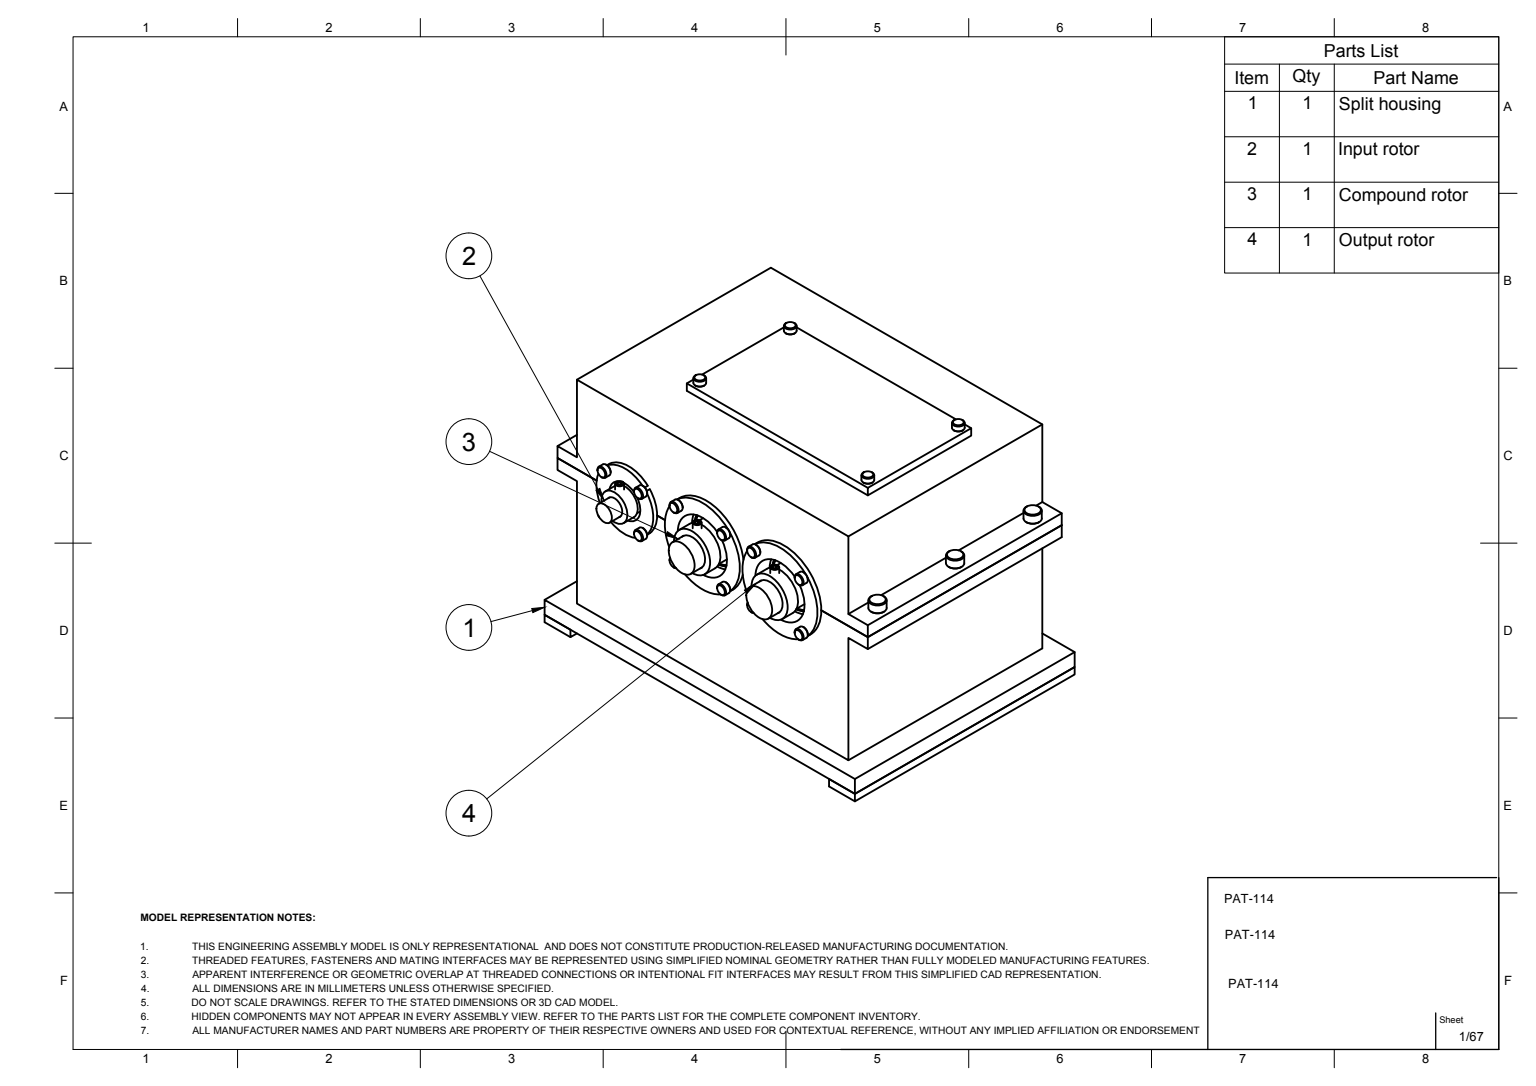
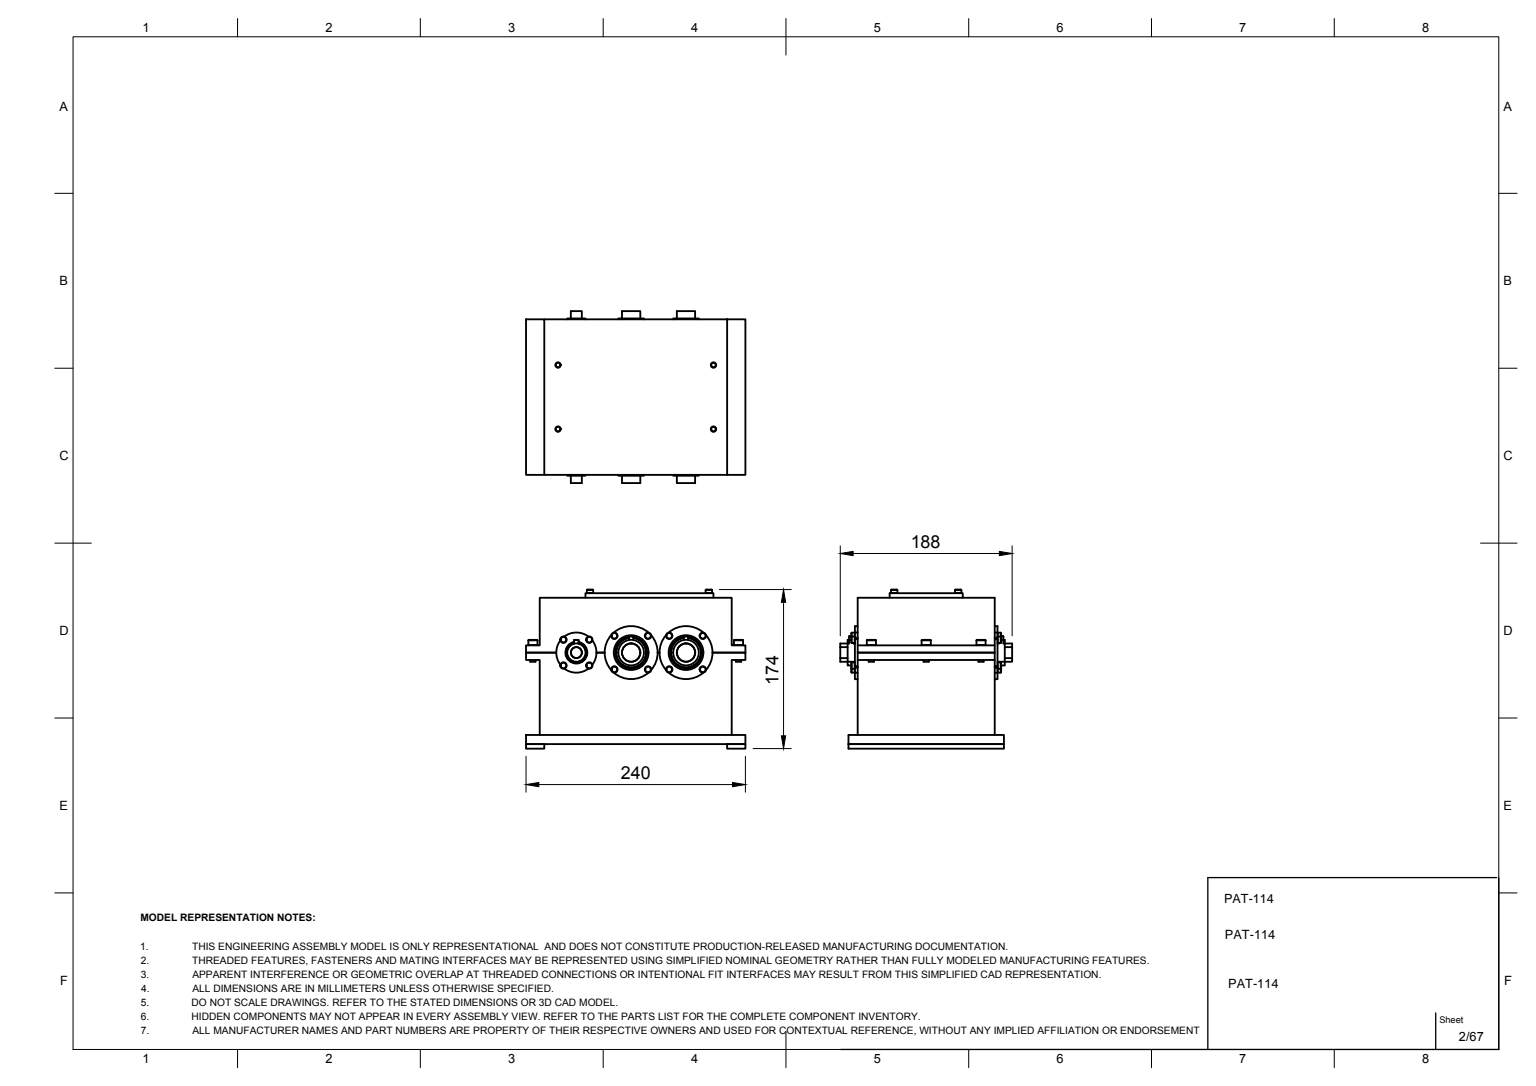
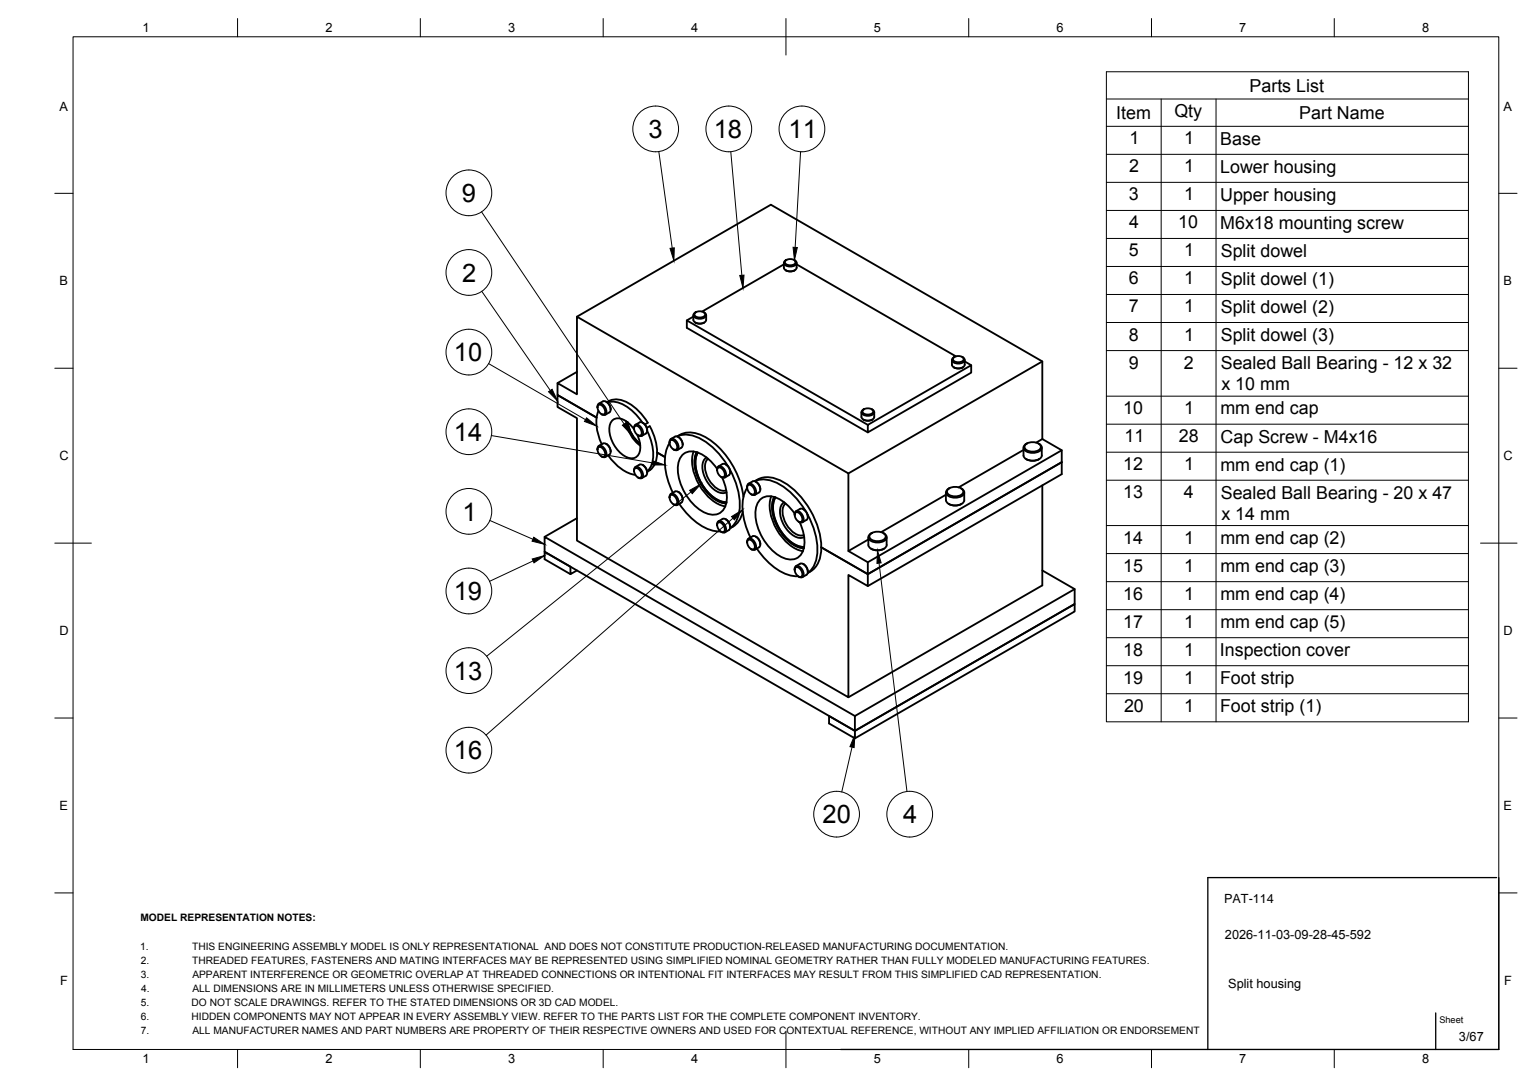
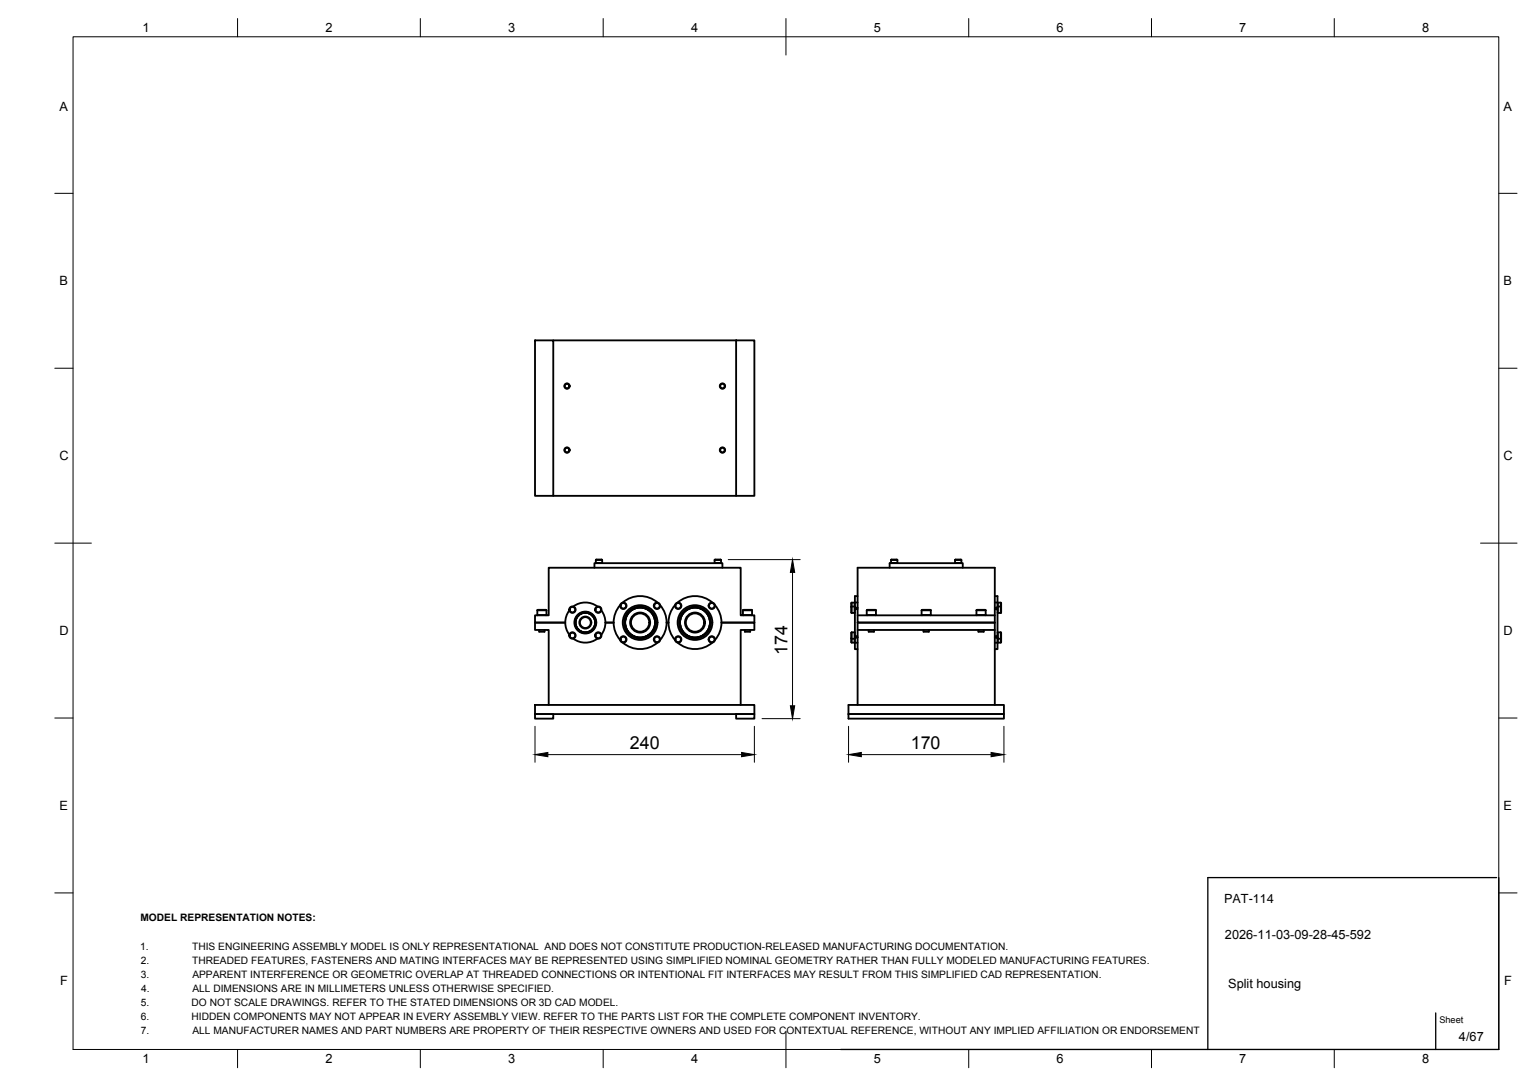
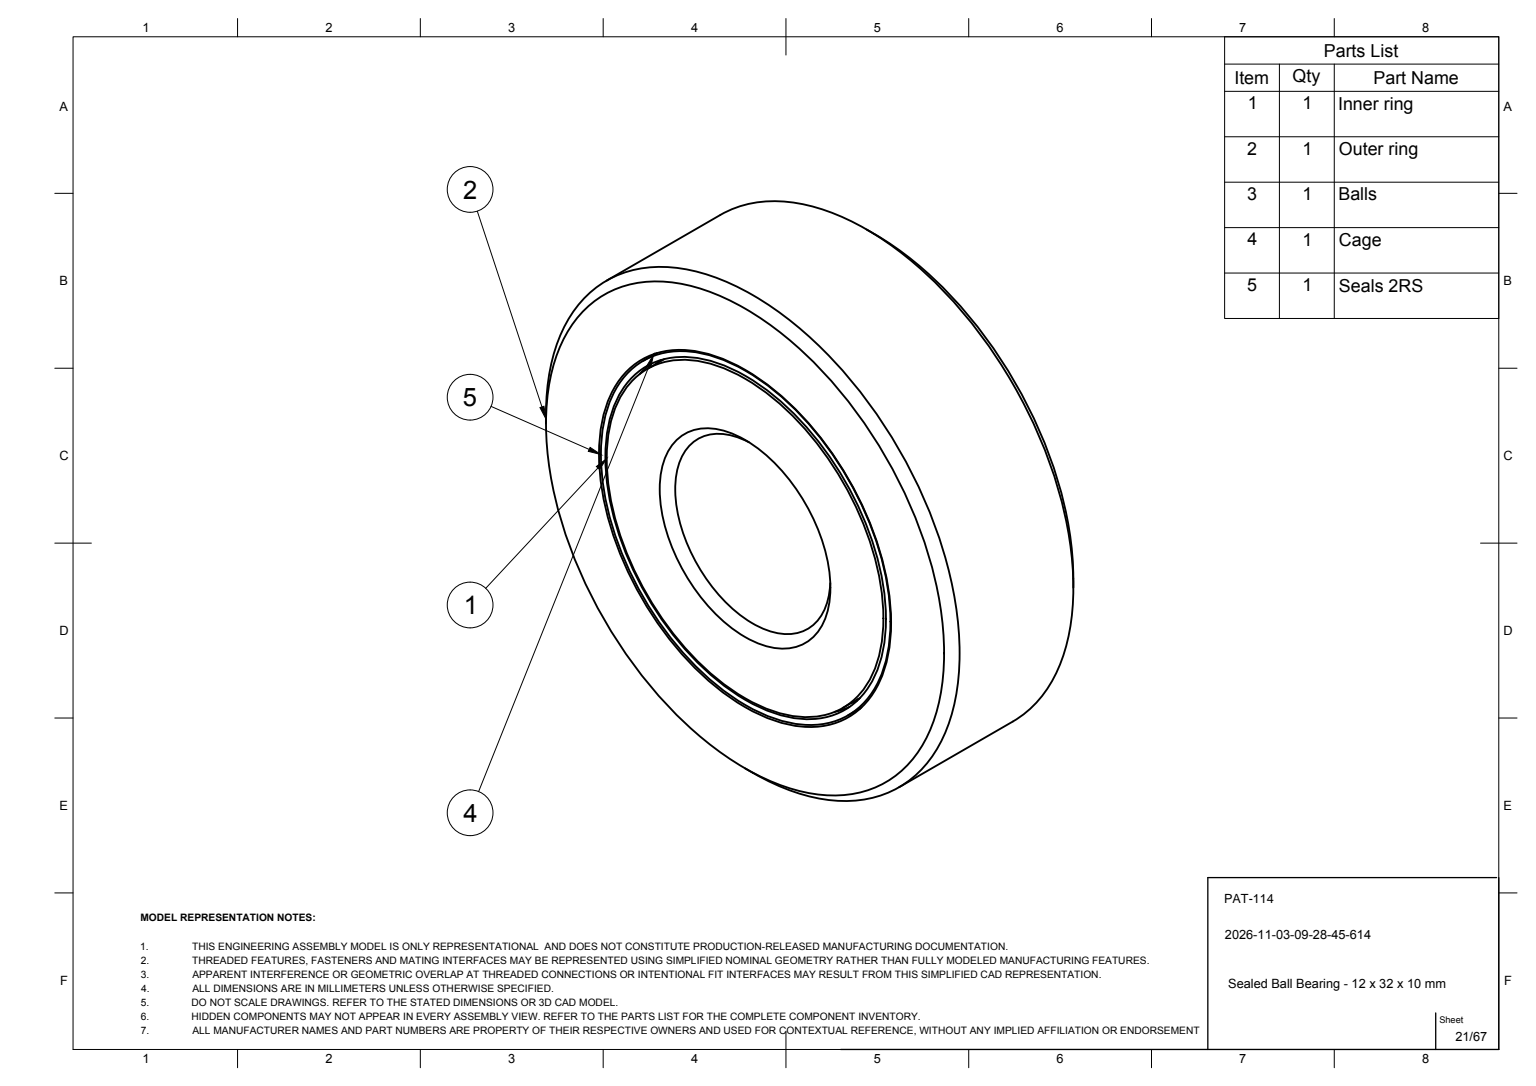
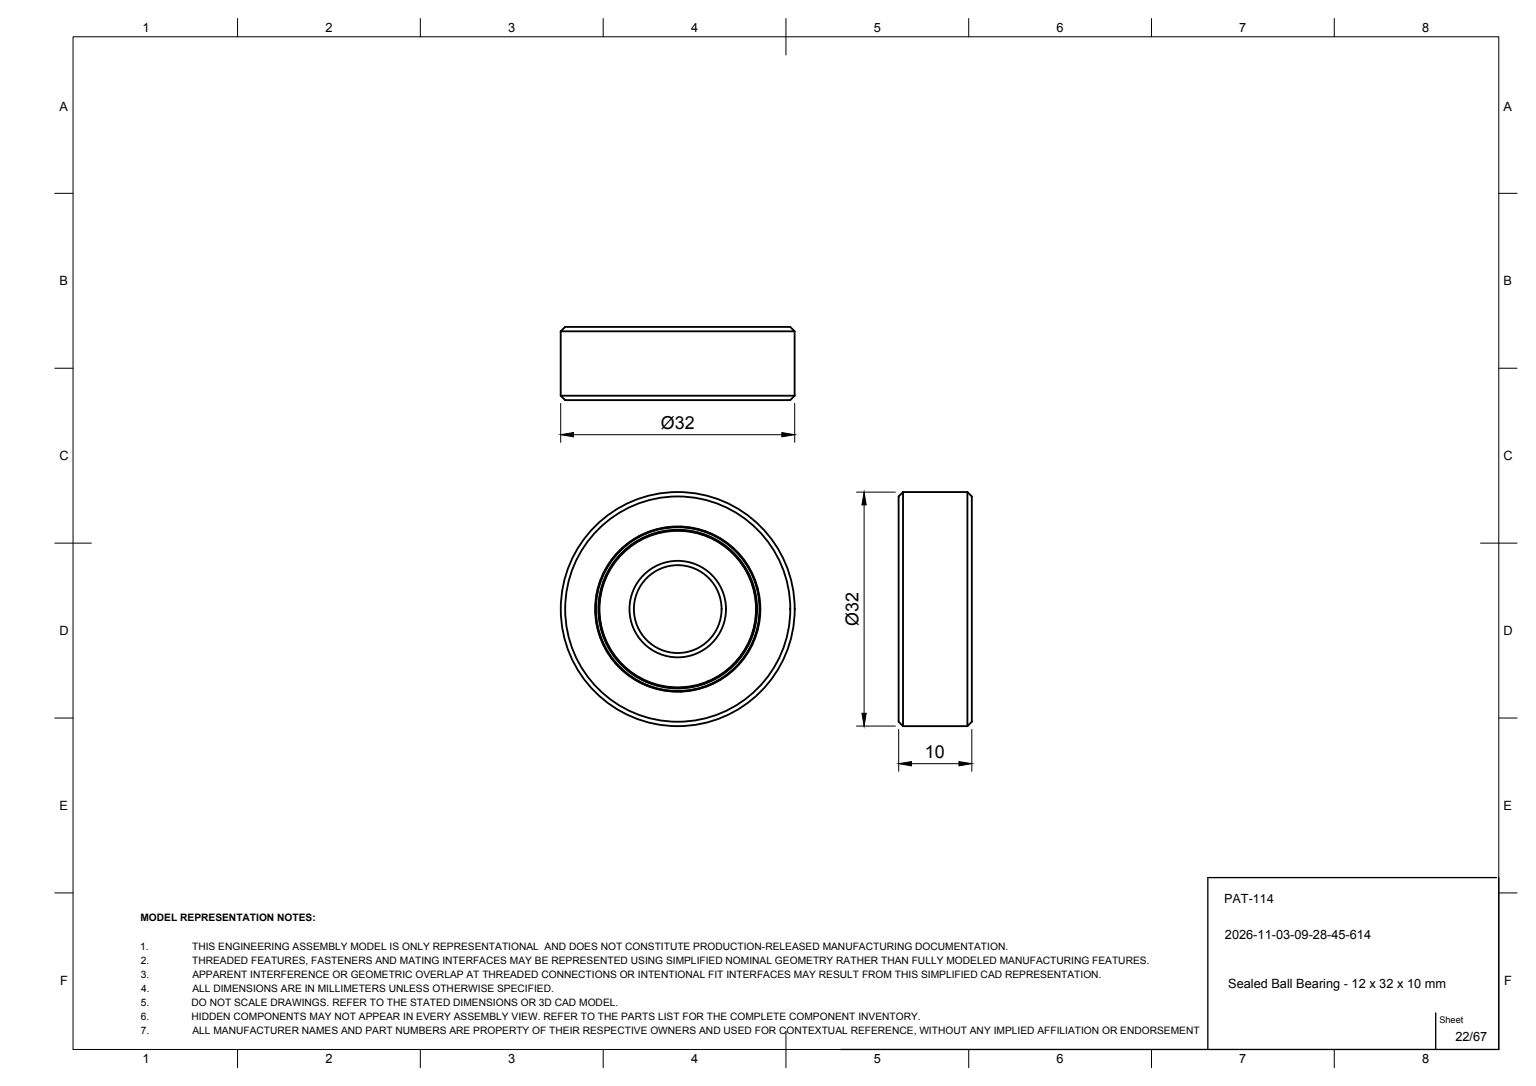
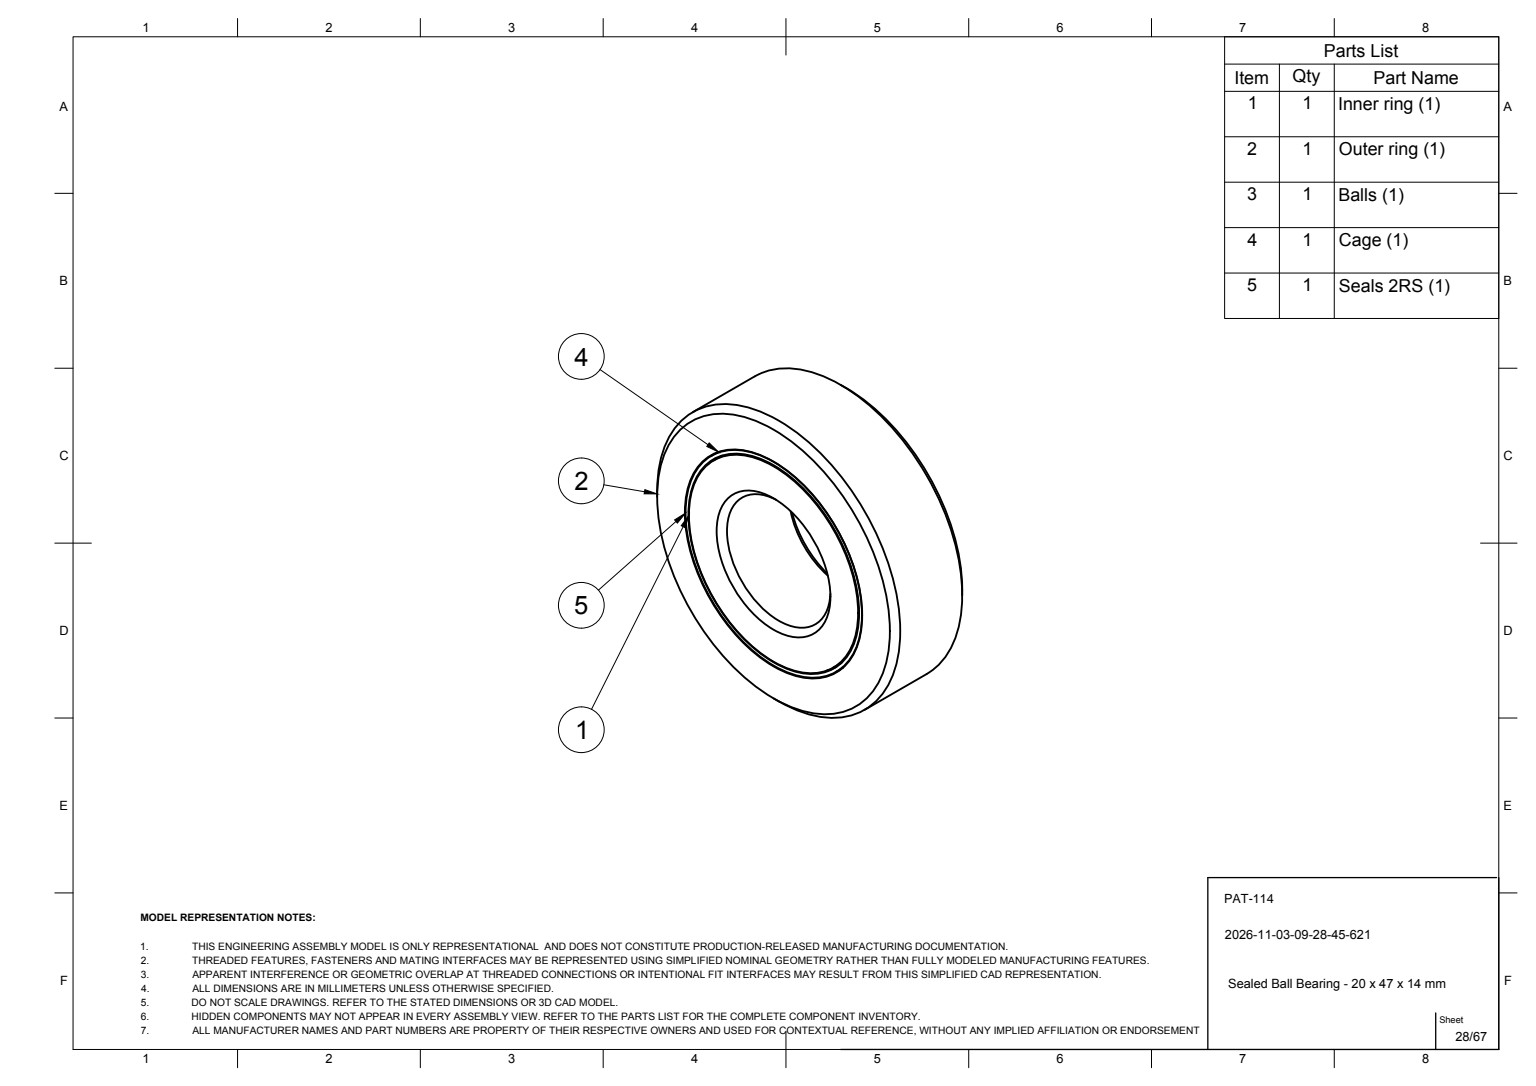
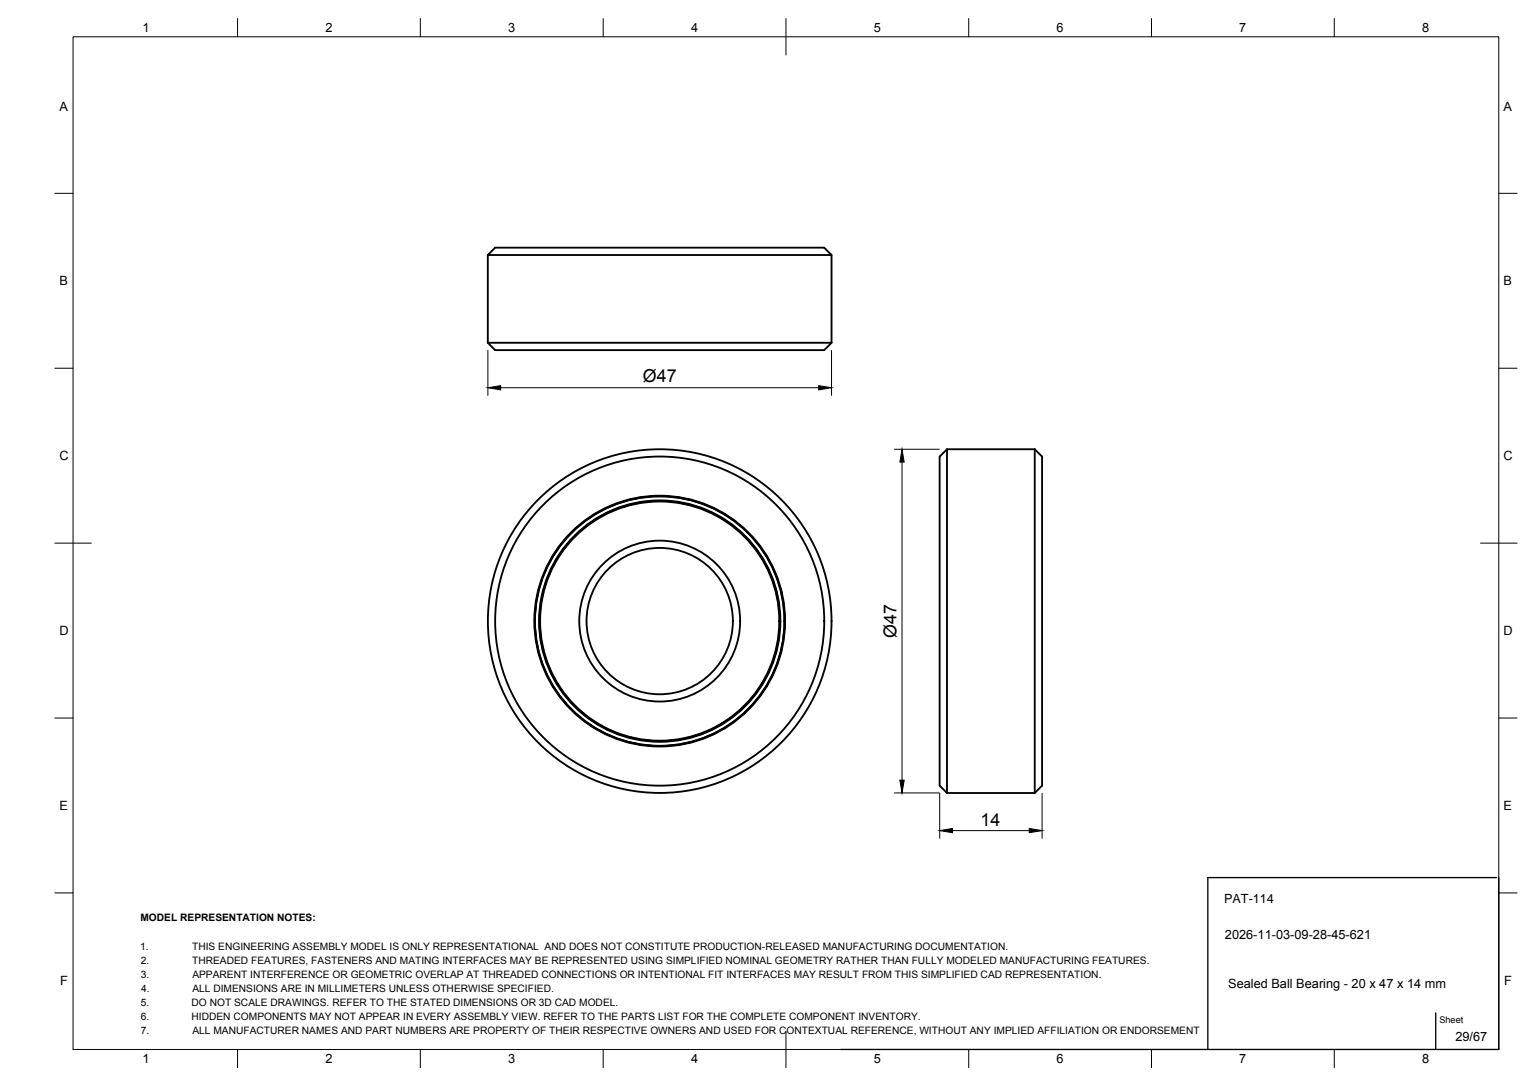
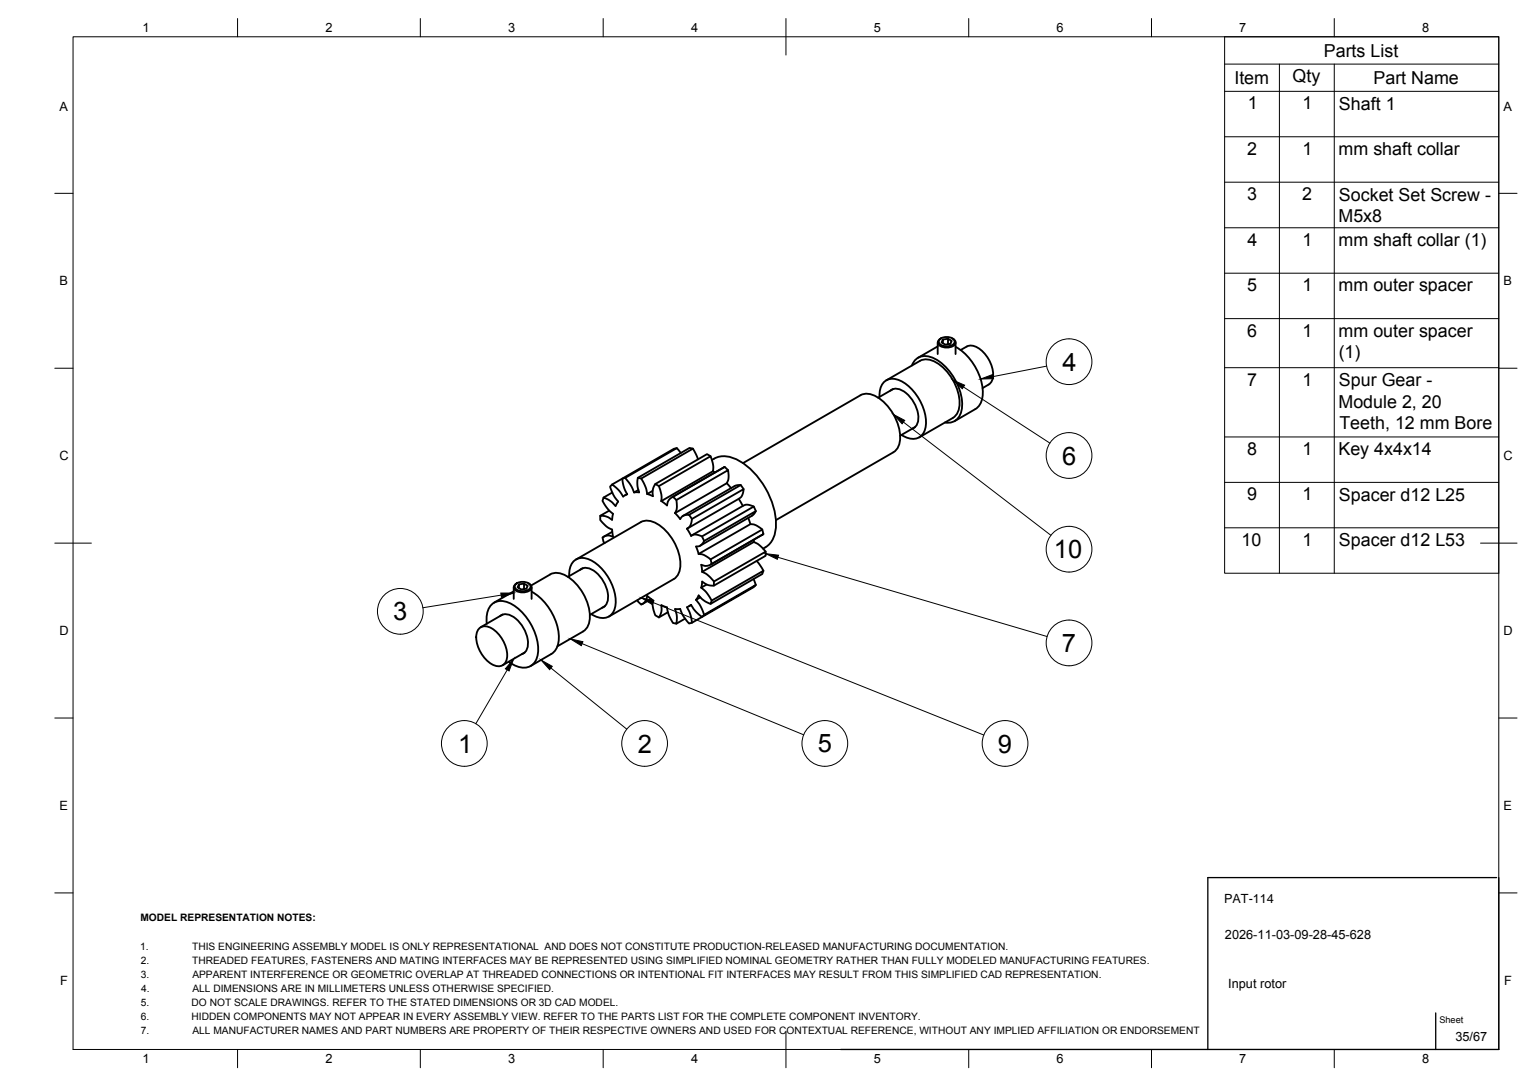
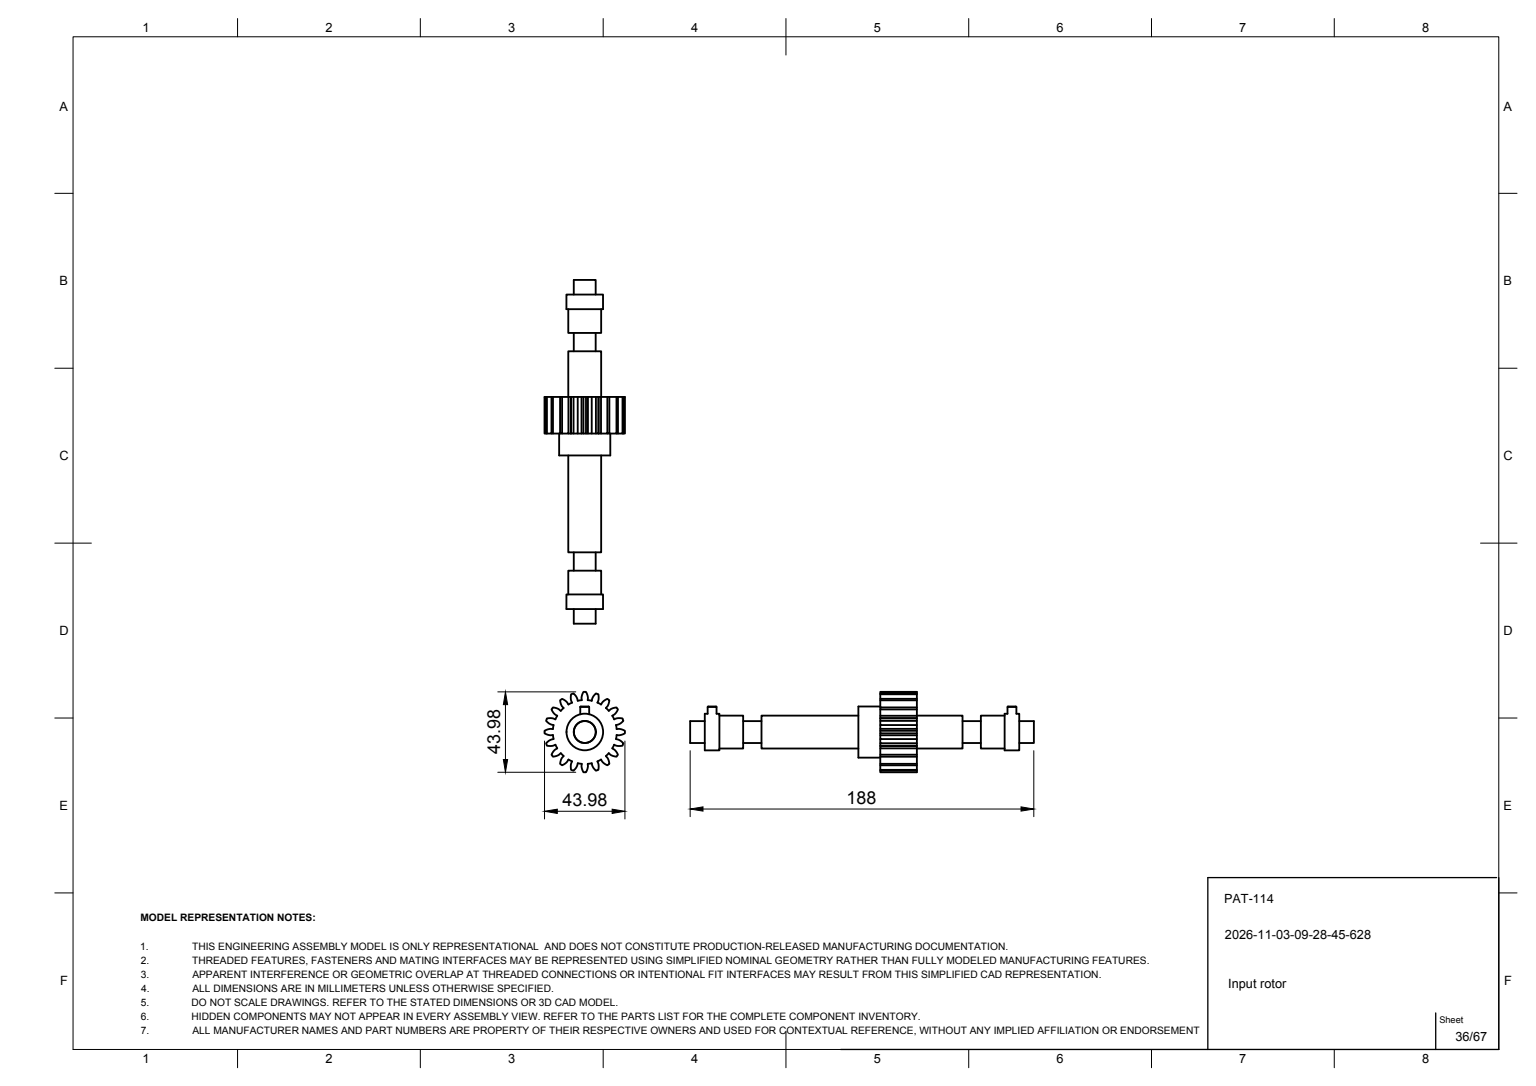
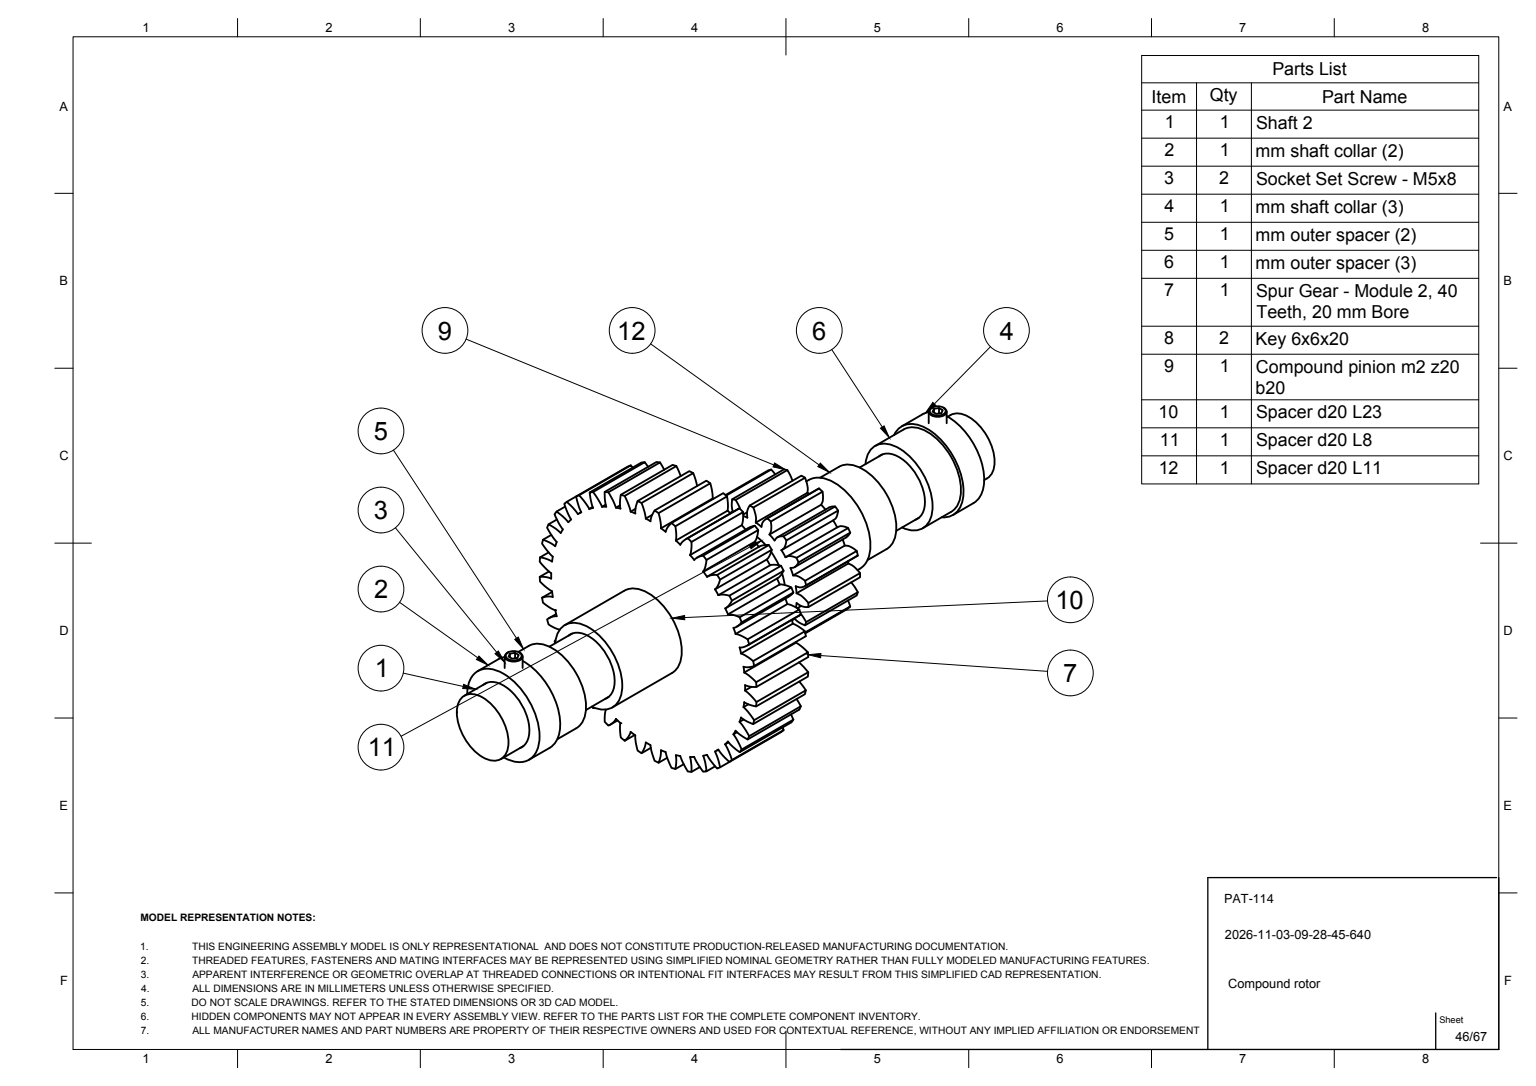
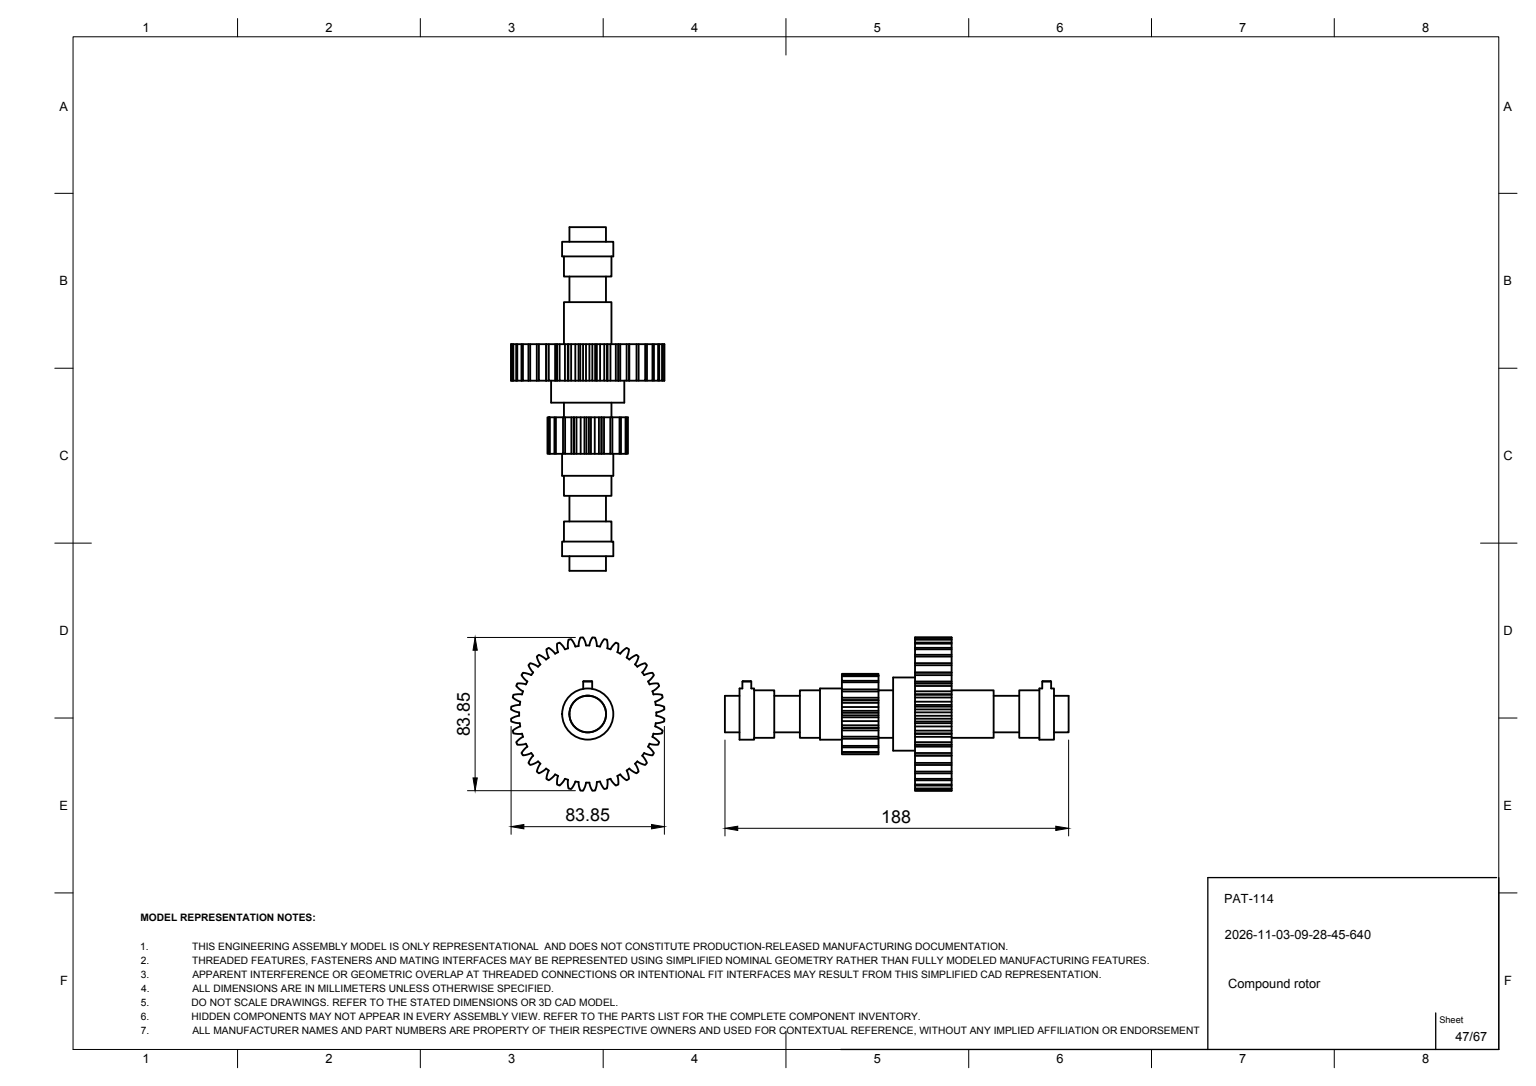
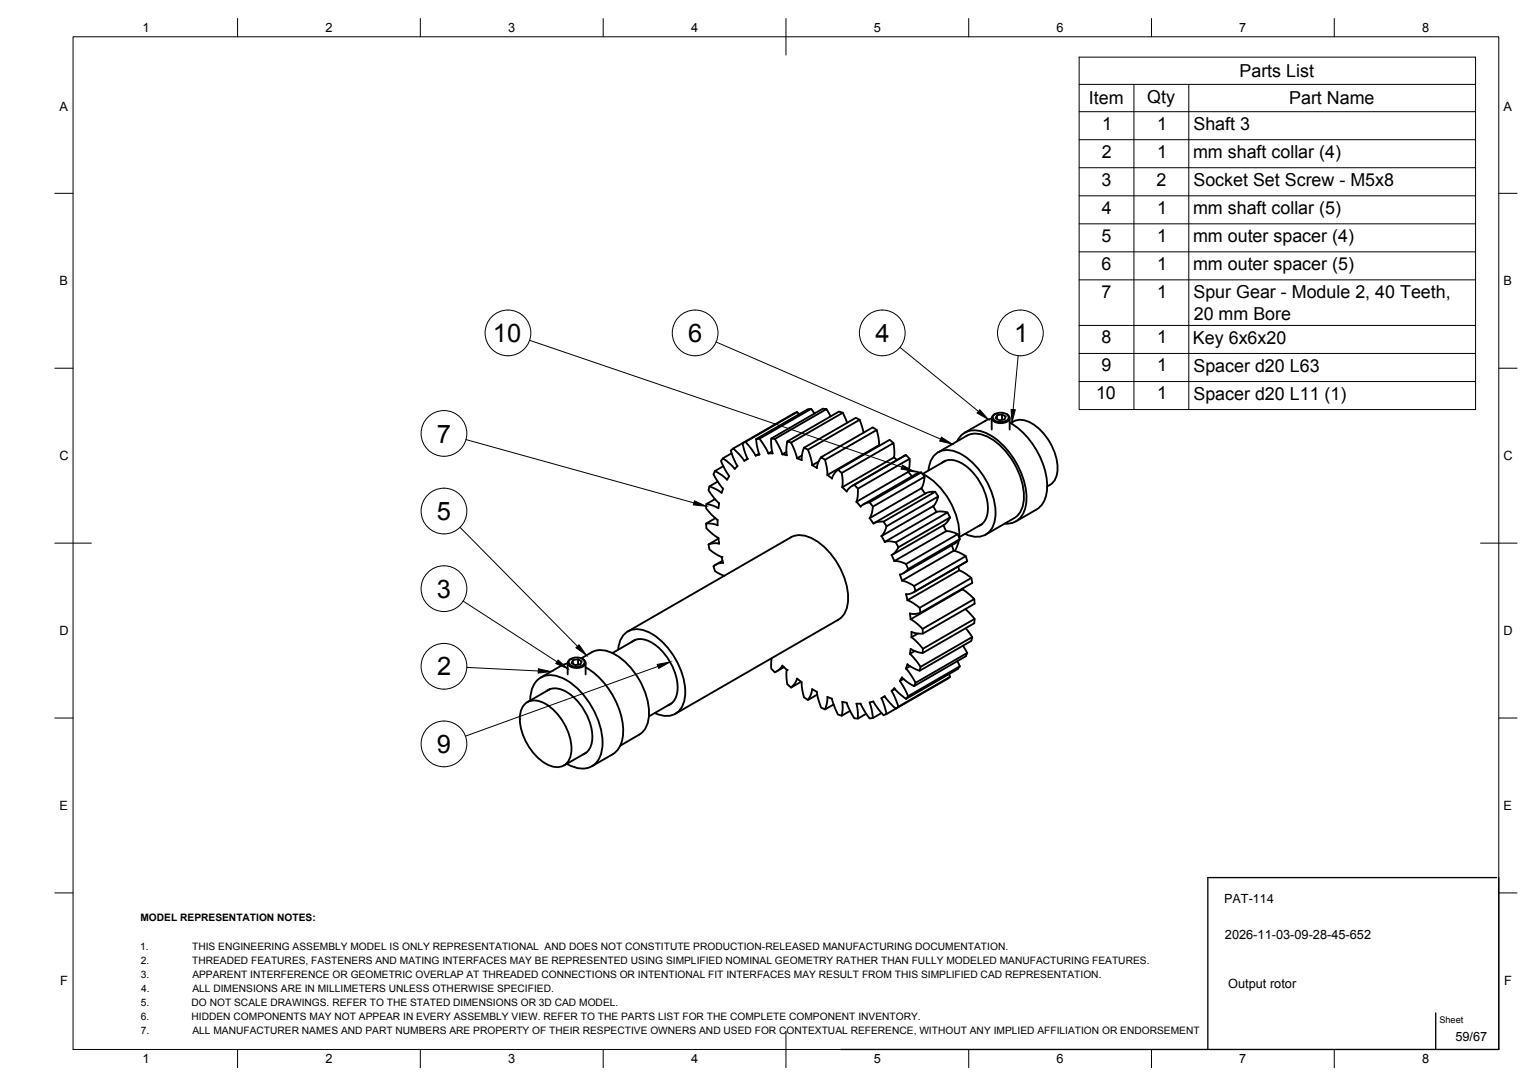
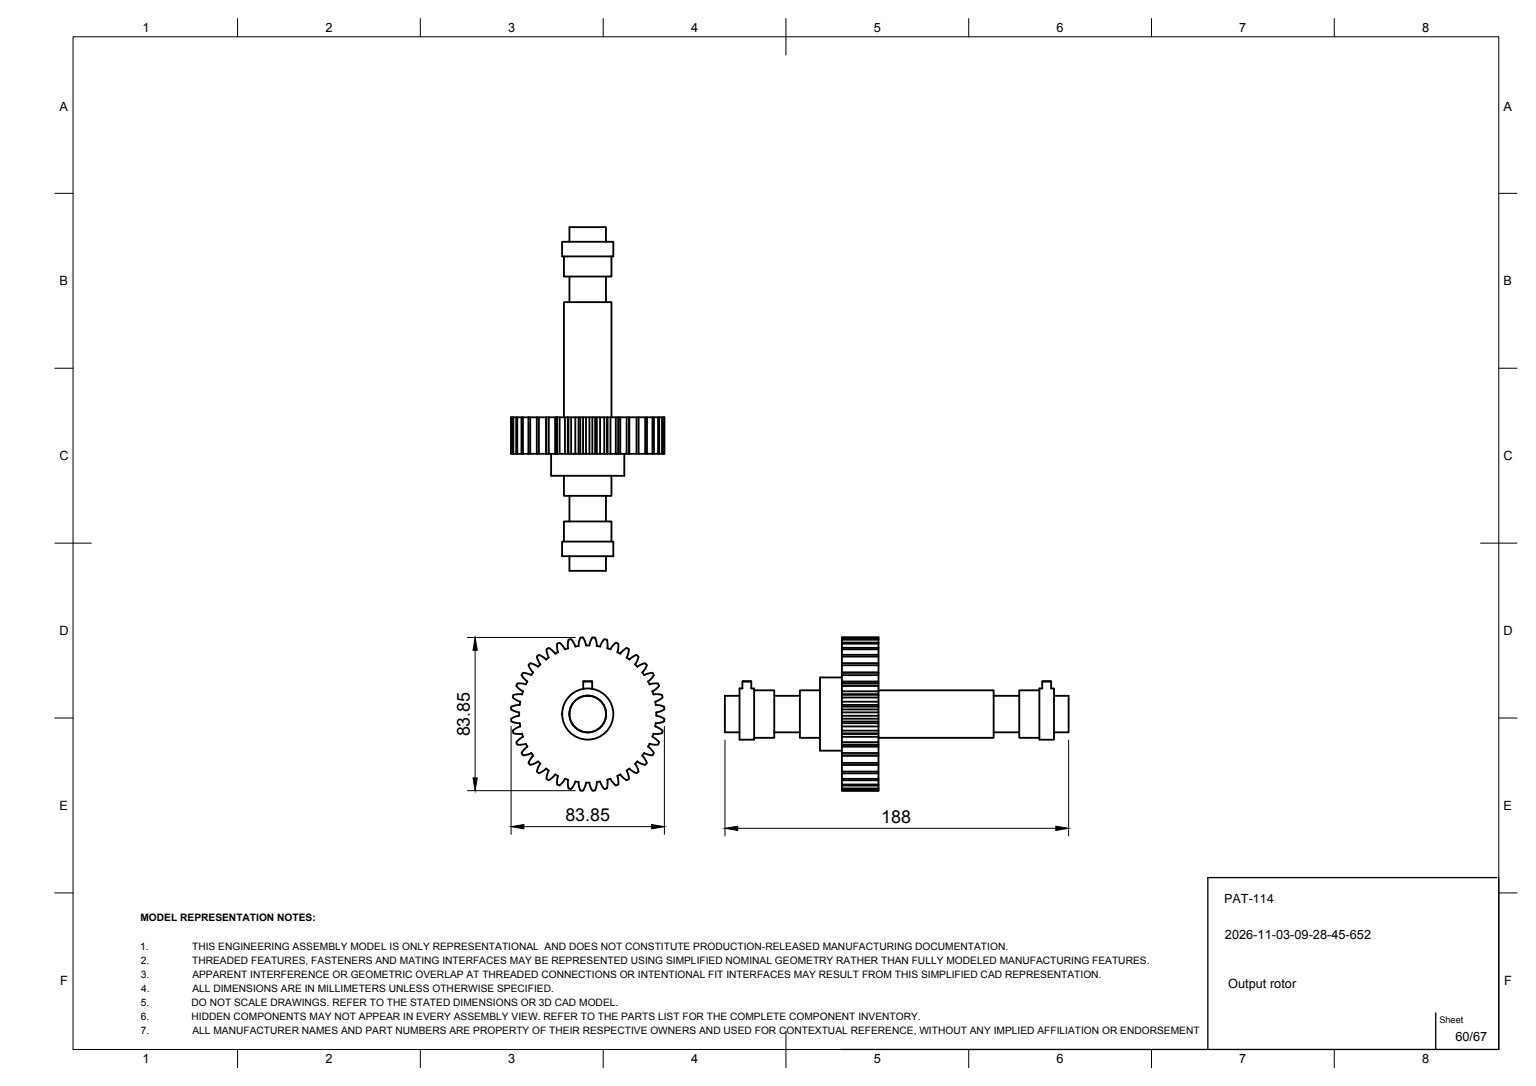
ISO-10303-21;
HEADER;
/* Generated by software containing ST-Developer
 * from STEP Tools, Inc. (www.steptools.com) 
 */

FILE_DESCRIPTION(
/* description */ ('Two-stage gear reducer in split housing'),
/* implementation_level */ '2;1');

FILE_NAME(
/* name */ 'PAT-114',
/* time_stamp */ '2026-10-28T03:22:31-07:00',
/* author */ (''),
/* organization */ (''),
/* preprocessor_version */ 'ST-DEVELOPER v20.2',
/* originating_system */ 'Autodesk Translation Framework v15.17.0.0',
/* authorisation */ '');

FILE_SCHEMA (('AUTOMOTIVE_DESIGN { 1 0 10303 214 3 1 1 }'));
ENDSEC;

DATA;
#10=MECHANICAL_DESIGN_GEOMETRIC_PRESENTATION_REPRESENTATION('',(#1234,#1235,
#1236,#1237,#1238,#1239,#1240,#1241,#1242,#1243,#1244,#1245,#1246,#1247,
#1248,#1249,#1250,#1251,#1252,#1253,#1254,#1255,#1256,#1257,#1258,#1259,
#1260,#1261,#1262,#1263,#1264,#1265,#1266,#1267,#1268,#1269,#1270,#1271,
#1272,#1273,#1274,#1275,#1276,#1277,#1278,#1279,#1280,#1281,#1282,#1283,
#1284,#1285,#1286,#1287,#1288,#1289,#1290,#1291,#1292,#1293,#1294,#1295,
#1296,#1297,#1298,#1299,#1300,#1301,#1302,#1303,#1304),#73366);
#11=(
BOUNDED_SURFACE()
B_SPLINE_SURFACE(5,1,((#28644,#28645),(#28646,#28647),(#28648,#28649),(#28650,
#28651),(#28652,#28653),(#28654,#28655),(#28656,#28657),(#28658,#28659),
(#28660,#28661),(#28662,#28663),(#28664,#28665),(#28666,#28667),(#28668,
#28669),(#28670,#28671),(#28672,#28673),(#28674,#28675),(#28676,#28677),
(#28678,#28679),(#28680,#28681),(#28682,#28683),(#28684,#28685),(#28686,
#28687),(#28688,#28689),(#28690,#28691),(#28692,#28693),(#28694,#28695),
(#28696,#28697),(#28698,#28699),(#28700,#28701),(#28702,#28703),(#28704,
#28705),(#28706,#28707),(#28708,#28709),(#28710,#28711),(#28712,#28713),
(#28714,#28715),(#28716,#28717),(#28718,#28719),(#28720,#28721),(#28722,
#28723),(#28724,#28725),(#28726,#28727),(#28728,#28729),(#28730,#28731),
(#28732,#28733),(#28734,#28735),(#28736,#28737),(#28738,#28739),(#28740,
#28741),(#28742,#28743),(#28744,#28745),(#28746,#28747),(#28748,#28749),
(#28750,#28751),(#28752,#28753),(#28754,#28755),(#28756,#28757),(#28758,
#28759),(#28760,#28761),(#28762,#28763),(#28764,#28765),(#28766,#28767),
(#28768,#28769),(#28770,#28771),(#28772,#28773),(#28774,#28775),(#28776,
#28777),(#28778,#28779),(#28780,#28781),(#28782,#28783)),.UNSPECIFIED.,
 .F.,.F.,.F.)
B_SPLINE_SURFACE_WITH_KNOTS((6,1,1,1,1,1,1,1,1,1,1,1,1,1,1,1,1,1,1,1,1,
1,1,1,1,1,1,1,1,1,1,1,1,1,1,1,1,1,1,1,1,1,1,1,1,1,1,1,1,1,1,1,1,1,1,1,1,
1,1,1,1,1,1,1,1,6),(2,2),(-1.,-0.984615384615383,-0.969230769230768,-0.953846153846152,
-0.938461538461537,-0.923076923076922,-0.907692307692306,-0.892307692307691,
-0.876923076923076,-0.86153846153846,-0.846153846153845,-0.83076923076923,
-0.815384615384614,-0.799999999999999,-0.784615384615384,-0.769230769230768,
-0.753846153846153,-0.738461538461538,-0.723076923076922,-0.707692307692307,
-0.692307692307692,-0.676923076923076,-0.661538461538461,-0.646153846153846,
-0.63076923076923,-0.615384615384615,-0.6,-0.584615384615384,-0.569230769230769,
-0.553846153846154,-0.538461538461538,-0.523076923076923,-0.507692307692308,
-0.492307692307692,-0.476923076923077,-0.461538461538462,-0.446153846153846,
-0.430769230769231,-0.415384615384615,-0.4,-0.384615384615385,-0.369230769230769,
-0.353846153846154,-0.338461538461538,-0.323076923076923,-0.307692307692308,
-0.292307692307692,-0.276923076923077,-0.261538461538462,-0.246153846153846,
-0.230769230769231,-0.215384615384615,-0.2,-0.184615384615385,-0.169230769230769,
-0.153846153846154,-0.138461538461538,-0.123076923076923,-0.107692307692308,
-0.0923076923076923,-0.0769230769230769,-0.0615384615384615,-0.0461538461538462,
-0.0307692307692308,-0.0153846153846154,0.),(-1.,1.),.UNSPECIFIED.)
GEOMETRIC_REPRESENTATION_ITEM()
RATIONAL_B_SPLINE_SURFACE(((1.,1.),(1.,1.),(1.,1.),(1.,1.),(1.,1.),(1.,
1.),(1.,1.),(1.,1.),(1.,1.),(1.,1.),(1.,1.),(1.,1.),(1.,1.),(1.,1.),(1.,
1.),(1.,1.),(1.,1.),(1.,1.),(1.,1.),(1.,1.),(1.,1.),(1.,1.),(1.,1.),(1.,
1.),(1.,1.),(1.,1.),(1.,1.),(1.,1.),(1.,1.),(1.,1.),(1.,1.),(1.,1.),(1.,
1.),(1.,1.),(1.,1.),(1.,1.),(1.,1.),(1.,1.),(1.,1.),(1.,1.),(1.,1.),(1.,
1.),(1.,1.),(1.,1.),(1.,1.),(1.,1.),(1.,1.),(1.,1.),(1.,1.),(1.,1.),(1.,
1.),(1.,1.),(1.,1.),(1.,1.),(1.,1.),(1.,1.),(1.,1.),(1.,1.),(1.,1.),(1.,
1.),(1.,1.),(1.,1.),(1.,1.),(1.,1.),(1.,1.),(1.,1.),(1.,1.),(1.,1.),(1.,
1.),(1.,1.)))
REPRESENTATION_ITEM('')
SURFACE()
);
#12=(
BOUNDED_SURFACE()
B_SPLINE_SURFACE(5,1,((#28862,#28863),(#28864,#28865),(#28866,#28867),(#28868,
#28869),(#28870,#28871),(#28872,#28873),(#28874,#28875),(#28876,#28877),
(#28878,#28879),(#28880,#28881),(#28882,#28883),(#28884,#28885),(#28886,
#28887),(#28888,#28889),(#28890,#28891),(#28892,#28893),(#28894,#28895),
(#28896,#28897),(#28898,#28899),(#28900,#28901),(#28902,#28903),(#28904,
#28905),(#28906,#28907),(#28908,#28909),(#28910,#28911),(#28912,#28913),
(#28914,#28915),(#28916,#28917),(#28918,#28919),(#28920,#28921),(#28922,
#28923),(#28924,#28925),(#28926,#28927),(#28928,#28929),(#28930,#28931),
(#28932,#28933),(#28934,#28935),(#28936,#28937),(#28938,#28939),(#28940,
#28941),(#28942,#28943),(#28944,#28945),(#28946,#28947),(#28948,#28949),
(#28950,#28951),(#28952,#28953),(#28954,#28955),(#28956,#28957),(#28958,
#28959),(#28960,#28961),(#28962,#28963),(#28964,#28965),(#28966,#28967),
(#28968,#28969),(#28970,#28971),(#28972,#28973),(#28974,#28975),(#28976,
#28977),(#28978,#28979),(#28980,#28981),(#28982,#28983),(#28984,#28985),
(#28986,#28987),(#28988,#28989),(#28990,#28991),(#28992,#28993),(#28994,
#28995),(#28996,#28997),(#28998,#28999),(#29000,#29001)),.UNSPECIFIED.,
 .F.,.F.,.F.)
B_SPLINE_SURFACE_WITH_KNOTS((6,1,1,1,1,1,1,1,1,1,1,1,1,1,1,1,1,1,1,1,1,
1,1,1,1,1,1,1,1,1,1,1,1,1,1,1,1,1,1,1,1,1,1,1,1,1,1,1,1,1,1,1,1,1,1,1,1,
1,1,1,1,1,1,1,1,6),(2,2),(-1.,-0.984615384615383,-0.969230769230768,-0.953846153846152,
-0.938461538461537,-0.923076923076922,-0.907692307692306,-0.892307692307691,
-0.876923076923076,-0.86153846153846,-0.846153846153845,-0.83076923076923,
-0.815384615384614,-0.799999999999999,-0.784615384615384,-0.769230769230768,
-0.753846153846153,-0.738461538461538,-0.723076923076922,-0.707692307692307,
-0.692307692307692,-0.676923076923076,-0.661538461538461,-0.646153846153846,
-0.63076923076923,-0.615384615384615,-0.6,-0.584615384615384,-0.569230769230769,
-0.553846153846154,-0.538461538461538,-0.523076923076923,-0.507692307692308,
-0.492307692307692,-0.476923076923077,-0.461538461538462,-0.446153846153846,
-0.430769230769231,-0.415384615384615,-0.4,-0.384615384615385,-0.369230769230769,
-0.353846153846154,-0.338461538461538,-0.323076923076923,-0.307692307692308,
-0.292307692307692,-0.276923076923077,-0.261538461538462,-0.246153846153846,
-0.230769230769231,-0.215384615384615,-0.2,-0.184615384615385,-0.169230769230769,
-0.153846153846154,-0.138461538461538,-0.123076923076923,-0.107692307692308,
-0.0923076923076923,-0.0769230769230769,-0.0615384615384615,-0.0461538461538462,
-0.0307692307692308,-0.0153846153846154,0.),(-1.,1.),.UNSPECIFIED.)
GEOMETRIC_REPRESENTATION_ITEM()
RATIONAL_B_SPLINE_SURFACE(((1.,1.),(1.,1.),(1.,1.),(1.,1.),(1.,1.),(1.,
1.),(1.,1.),(1.,1.),(1.,1.),(1.,1.),(1.,1.),(1.,1.),(1.,1.),(1.,1.),(1.,
1.),(1.,1.),(1.,1.),(1.,1.),(1.,1.),(1.,1.),(1.,1.),(1.,1.),(1.,1.),(1.,
1.),(1.,1.),(1.,1.),(1.,1.),(1.,1.),(1.,1.),(1.,1.),(1.,1.),(1.,1.),(1.,
1.),(1.,1.),(1.,1.),(1.,1.),(1.,1.),(1.,1.),(1.,1.),(1.,1.),(1.,1.),(1.,
1.),(1.,1.),(1.,1.),(1.,1.),(1.,1.),(1.,1.),(1.,1.),(1.,1.),(1.,1.),(1.,
1.),(1.,1.),(1.,1.),(1.,1.),(1.,1.),(1.,1.),(1.,1.),(1.,1.),(1.,1.),(1.,
1.),(1.,1.),(1.,1.),(1.,1.),(1.,1.),(1.,1.),(1.,1.),(1.,1.),(1.,1.),(1.,
1.),(1.,1.)))
REPRESENTATION_ITEM('')
SURFACE()
);
#13=(
BOUNDED_SURFACE()
B_SPLINE_SURFACE(5,1,((#29078,#29079),(#29080,#29081),(#29082,#29083),(#29084,
#29085),(#29086,#29087),(#29088,#29089),(#29090,#29091),(#29092,#29093),
(#29094,#29095),(#29096,#29097),(#29098,#29099),(#29100,#29101),(#29102,
#29103),(#29104,#29105),(#29106,#29107),(#29108,#29109),(#29110,#29111),
(#29112,#29113),(#29114,#29115),(#29116,#29117),(#29118,#29119),(#29120,
#29121),(#29122,#29123),(#29124,#29125),(#29126,#29127),(#29128,#29129),
(#29130,#29131),(#29132,#29133),(#29134,#29135),(#29136,#29137),(#29138,
#29139),(#29140,#29141),(#29142,#29143),(#29144,#29145),(#29146,#29147),
(#29148,#29149),(#29150,#29151),(#29152,#29153),(#29154,#29155),(#29156,
#29157),(#29158,#29159),(#29160,#29161),(#29162,#29163),(#29164,#29165),
(#29166,#29167),(#29168,#29169),(#29170,#29171),(#29172,#29173),(#29174,
#29175),(#29176,#29177),(#29178,#29179),(#29180,#29181),(#29182,#29183),
(#29184,#29185),(#29186,#29187),(#29188,#29189),(#29190,#29191),(#29192,
#29193),(#29194,#29195),(#29196,#29197),(#29198,#29199),(#29200,#29201),
(#29202,#29203),(#29204,#29205),(#29206,#29207),(#29208,#29209),(#29210,
#29211),(#29212,#29213),(#29214,#29215),(#29216,#29217)),.UNSPECIFIED.,
 .F.,.F.,.F.)
B_SPLINE_SURFACE_WITH_KNOTS((6,1,1,1,1,1,1,1,1,1,1,1,1,1,1,1,1,1,1,1,1,
1,1,1,1,1,1,1,1,1,1,1,1,1,1,1,1,1,1,1,1,1,1,1,1,1,1,1,1,1,1,1,1,1,1,1,1,
1,1,1,1,1,1,1,1,6),(2,2),(-1.,-0.984615384615383,-0.969230769230768,-0.953846153846152,
-0.938461538461537,-0.923076923076922,-0.907692307692306,-0.892307692307691,
-0.876923076923076,-0.86153846153846,-0.846153846153845,-0.83076923076923,
-0.815384615384614,-0.799999999999999,-0.784615384615384,-0.769230769230768,
-0.753846153846153,-0.738461538461538,-0.723076923076922,-0.707692307692307,
-0.692307692307692,-0.676923076923076,-0.661538461538461,-0.646153846153846,
-0.63076923076923,-0.615384615384615,-0.6,-0.584615384615384,-0.569230769230769,
-0.553846153846154,-0.538461538461538,-0.523076923076923,-0.507692307692308,
-0.492307692307692,-0.476923076923077,-0.461538461538462,-0.446153846153846,
-0.430769230769231,-0.415384615384615,-0.4,-0.384615384615385,-0.369230769230769,
-0.353846153846154,-0.338461538461538,-0.323076923076923,-0.307692307692308,
-0.292307692307692,-0.276923076923077,-0.261538461538462,-0.246153846153846,
-0.230769230769231,-0.215384615384615,-0.2,-0.184615384615385,-0.169230769230769,
-0.153846153846154,-0.138461538461538,-0.123076923076923,-0.107692307692308,
-0.0923076923076923,-0.0769230769230769,-0.0615384615384615,-0.0461538461538462,
-0.0307692307692308,-0.0153846153846154,0.),(-1.,1.),.UNSPECIFIED.)
GEOMETRIC_REPRESENTATION_ITEM()
RATIONAL_B_SPLINE_SURFACE(((1.,1.),(1.,1.),(1.,1.),(1.,1.),(1.,1.),(1.,
1.),(1.,1.),(1.,1.),(1.,1.),(1.,1.),(1.,1.),(1.,1.),(1.,1.),(1.,1.),(1.,
1.),(1.,1.),(1.,1.),(1.,1.),(1.,1.),(1.,1.),(1.,1.),(1.,1.),(1.,1.),(1.,
1.),(1.,1.),(1.,1.),(1.,1.),(1.,1.),(1.,1.),(1.,1.),(1.,1.),(1.,1.),(1.,
1.),(1.,1.),(1.,1.),(1.,1.),(1.,1.),(1.,1.),(1.,1.),(1.,1.),(1.,1.),(1.,
1.),(1.,1.),(1.,1.),(1.,1.),(1.,1.),(1.,1.),(1.,1.),(1.,1.),(1.,1.),(1.,
1.),(1.,1.),(1.,1.),(1.,1.),(1.,1.),(1.,1.),(1.,1.),(1.,1.),(1.,1.),(1.,
1.),(1.,1.),(1.,1.),(1.,1.),(1.,1.),(1.,1.),(1.,1.),(1.,1.),(1.,1.),(1.,
1.),(1.,1.)))
REPRESENTATION_ITEM('')
SURFACE()
);
#14=(
BOUNDED_SURFACE()
B_SPLINE_SURFACE(5,1,((#29294,#29295),(#29296,#29297),(#29298,#29299),(#29300,
#29301),(#29302,#29303),(#29304,#29305),(#29306,#29307),(#29308,#29309),
(#29310,#29311),(#29312,#29313),(#29314,#29315),(#29316,#29317),(#29318,
#29319),(#29320,#29321),(#29322,#29323),(#29324,#29325),(#29326,#29327),
(#29328,#29329),(#29330,#29331),(#29332,#29333),(#29334,#29335),(#29336,
#29337),(#29338,#29339),(#29340,#29341),(#29342,#29343),(#29344,#29345),
(#29346,#29347),(#29348,#29349),(#29350,#29351),(#29352,#29353),(#29354,
#29355),(#29356,#29357),(#29358,#29359),(#29360,#29361),(#29362,#29363),
(#29364,#29365),(#29366,#29367),(#29368,#29369),(#29370,#29371),(#29372,
#29373),(#29374,#29375),(#29376,#29377),(#29378,#29379),(#29380,#29381),
(#29382,#29383),(#29384,#29385),(#29386,#29387),(#29388,#29389),(#29390,
#29391),(#29392,#29393),(#29394,#29395),(#29396,#29397),(#29398,#29399),
(#29400,#29401),(#29402,#29403),(#29404,#29405),(#29406,#29407),(#29408,
#29409),(#29410,#29411),(#29412,#29413),(#29414,#29415),(#29416,#29417),
(#29418,#29419),(#29420,#29421),(#29422,#29423),(#29424,#29425),(#29426,
#29427),(#29428,#29429),(#29430,#29431),(#29432,#29433)),.UNSPECIFIED.,
 .F.,.F.,.F.)
B_SPLINE_SURFACE_WITH_KNOTS((6,1,1,1,1,1,1,1,1,1,1,1,1,1,1,1,1,1,1,1,1,
1,1,1,1,1,1,1,1,1,1,1,1,1,1,1,1,1,1,1,1,1,1,1,1,1,1,1,1,1,1,1,1,1,1,1,1,
1,1,1,1,1,1,1,1,6),(2,2),(-1.,-0.984615384615383,-0.969230769230768,-0.953846153846152,
-0.938461538461537,-0.923076923076922,-0.907692307692306,-0.892307692307691,
-0.876923076923076,-0.86153846153846,-0.846153846153845,-0.83076923076923,
-0.815384615384614,-0.799999999999999,-0.784615384615384,-0.769230769230768,
-0.753846153846153,-0.738461538461538,-0.723076923076922,-0.707692307692307,
-0.692307692307692,-0.676923076923076,-0.661538461538461,-0.646153846153846,
-0.63076923076923,-0.615384615384615,-0.6,-0.584615384615384,-0.569230769230769,
-0.553846153846154,-0.538461538461538,-0.523076923076923,-0.507692307692308,
-0.492307692307692,-0.476923076923077,-0.461538461538462,-0.446153846153846,
-0.430769230769231,-0.415384615384615,-0.4,-0.384615384615385,-0.369230769230769,
-0.353846153846154,-0.338461538461538,-0.323076923076923,-0.307692307692308,
-0.292307692307692,-0.276923076923077,-0.261538461538462,-0.246153846153846,
-0.230769230769231,-0.215384615384615,-0.2,-0.184615384615385,-0.169230769230769,
-0.153846153846154,-0.138461538461538,-0.123076923076923,-0.107692307692308,
-0.0923076923076923,-0.0769230769230769,-0.0615384615384615,-0.0461538461538462,
-0.0307692307692308,-0.0153846153846154,0.),(-1.,1.),.UNSPECIFIED.)
GEOMETRIC_REPRESENTATION_ITEM()
RATIONAL_B_SPLINE_SURFACE(((1.,1.),(1.,1.),(1.,1.),(1.,1.),(1.,1.),(1.,
1.),(1.,1.),(1.,1.),(1.,1.),(1.,1.),(1.,1.),(1.,1.),(1.,1.),(1.,1.),(1.,
1.),(1.,1.),(1.,1.),(1.,1.),(1.,1.),(1.,1.),(1.,1.),(1.,1.),(1.,1.),(1.,
1.),(1.,1.),(1.,1.),(1.,1.),(1.,1.),(1.,1.),(1.,1.),(1.,1.),(1.,1.),(1.,
1.),(1.,1.),(1.,1.),(1.,1.),(1.,1.),(1.,1.),(1.,1.),(1.,1.),(1.,1.),(1.,
1.),(1.,1.),(1.,1.),(1.,1.),(1.,1.),(1.,1.),(1.,1.),(1.,1.),(1.,1.),(1.,
1.),(1.,1.),(1.,1.),(1.,1.),(1.,1.),(1.,1.),(1.,1.),(1.,1.),(1.,1.),(1.,
1.),(1.,1.),(1.,1.),(1.,1.),(1.,1.),(1.,1.),(1.,1.),(1.,1.),(1.,1.),(1.,
1.),(1.,1.)))
REPRESENTATION_ITEM('')
SURFACE()
);
#15=(
BOUNDED_SURFACE()
B_SPLINE_SURFACE(5,1,((#29510,#29511),(#29512,#29513),(#29514,#29515),(#29516,
#29517),(#29518,#29519),(#29520,#29521),(#29522,#29523),(#29524,#29525),
(#29526,#29527),(#29528,#29529),(#29530,#29531),(#29532,#29533),(#29534,
#29535),(#29536,#29537),(#29538,#29539),(#29540,#29541),(#29542,#29543),
(#29544,#29545),(#29546,#29547),(#29548,#29549),(#29550,#29551),(#29552,
#29553),(#29554,#29555),(#29556,#29557),(#29558,#29559),(#29560,#29561),
(#29562,#29563),(#29564,#29565),(#29566,#29567),(#29568,#29569),(#29570,
#29571),(#29572,#29573),(#29574,#29575),(#29576,#29577),(#29578,#29579),
(#29580,#29581),(#29582,#29583),(#29584,#29585),(#29586,#29587),(#29588,
#29589),(#29590,#29591),(#29592,#29593),(#29594,#29595),(#29596,#29597),
(#29598,#29599),(#29600,#29601),(#29602,#29603),(#29604,#29605),(#29606,
#29607),(#29608,#29609),(#29610,#29611),(#29612,#29613),(#29614,#29615),
(#29616,#29617),(#29618,#29619),(#29620,#29621),(#29622,#29623),(#29624,
#29625),(#29626,#29627),(#29628,#29629),(#29630,#29631),(#29632,#29633),
(#29634,#29635),(#29636,#29637),(#29638,#29639),(#29640,#29641),(#29642,
#29643),(#29644,#29645),(#29646,#29647),(#29648,#29649)),.UNSPECIFIED.,
 .F.,.F.,.F.)
B_SPLINE_SURFACE_WITH_KNOTS((6,1,1,1,1,1,1,1,1,1,1,1,1,1,1,1,1,1,1,1,1,
1,1,1,1,1,1,1,1,1,1,1,1,1,1,1,1,1,1,1,1,1,1,1,1,1,1,1,1,1,1,1,1,1,1,1,1,
1,1,1,1,1,1,1,1,6),(2,2),(-1.,-0.984615384615383,-0.969230769230768,-0.953846153846152,
-0.938461538461537,-0.923076923076922,-0.907692307692306,-0.892307692307691,
-0.876923076923076,-0.86153846153846,-0.846153846153845,-0.83076923076923,
-0.815384615384614,-0.799999999999999,-0.784615384615384,-0.769230769230768,
-0.753846153846153,-0.738461538461538,-0.723076923076922,-0.707692307692307,
-0.692307692307692,-0.676923076923076,-0.661538461538461,-0.646153846153846,
-0.63076923076923,-0.615384615384615,-0.6,-0.584615384615384,-0.569230769230769,
-0.553846153846154,-0.538461538461538,-0.523076923076923,-0.507692307692308,
-0.492307692307692,-0.476923076923077,-0.461538461538462,-0.446153846153846,
-0.430769230769231,-0.415384615384615,-0.4,-0.384615384615385,-0.369230769230769,
-0.353846153846154,-0.338461538461538,-0.323076923076923,-0.307692307692308,
-0.292307692307692,-0.276923076923077,-0.261538461538462,-0.246153846153846,
-0.230769230769231,-0.215384615384615,-0.2,-0.184615384615385,-0.169230769230769,
-0.153846153846154,-0.138461538461538,-0.123076923076923,-0.107692307692308,
-0.0923076923076923,-0.0769230769230769,-0.0615384615384615,-0.0461538461538462,
-0.0307692307692308,-0.0153846153846154,0.),(-1.,1.),.UNSPECIFIED.)
GEOMETRIC_REPRESENTATION_ITEM()
RATIONAL_B_SPLINE_SURFACE(((1.,1.),(1.,1.),(1.,1.),(1.,1.),(1.,1.),(1.,
1.),(1.,1.),(1.,1.),(1.,1.),(1.,1.),(1.,1.),(1.,1.),(1.,1.),(1.,1.),(1.,
1.),(1.,1.),(1.,1.),(1.,1.),(1.,1.),(1.,1.),(1.,1.),(1.,1.),(1.,1.),(1.,
1.),(1.,1.),(1.,1.),(1.,1.),(1.,1.),(1.,1.),(1.,1.),(1.,1.),(1.,1.),(1.,
1.),(1.,1.),(1.,1.),(1.,1.),(1.,1.),(1.,1.),(1.,1.),(1.,1.),(1.,1.),(1.,
1.),(1.,1.),(1.,1.),(1.,1.),(1.,1.),(1.,1.),(1.,1.),(1.,1.),(1.,1.),(1.,
1.),(1.,1.),(1.,1.),(1.,1.),(1.,1.),(1.,1.),(1.,1.),(1.,1.),(1.,1.),(1.,
1.),(1.,1.),(1.,1.),(1.,1.),(1.,1.),(1.,1.),(1.,1.),(1.,1.),(1.,1.),(1.,
1.),(1.,1.)))
REPRESENTATION_ITEM('')
SURFACE()
);
#16=(
BOUNDED_SURFACE()
B_SPLINE_SURFACE(5,1,((#29726,#29727),(#29728,#29729),(#29730,#29731),(#29732,
#29733),(#29734,#29735),(#29736,#29737),(#29738,#29739),(#29740,#29741),
(#29742,#29743),(#29744,#29745),(#29746,#29747),(#29748,#29749),(#29750,
#29751),(#29752,#29753),(#29754,#29755),(#29756,#29757),(#29758,#29759),
(#29760,#29761),(#29762,#29763),(#29764,#29765),(#29766,#29767),(#29768,
#29769),(#29770,#29771),(#29772,#29773),(#29774,#29775),(#29776,#29777),
(#29778,#29779),(#29780,#29781),(#29782,#29783),(#29784,#29785),(#29786,
#29787),(#29788,#29789),(#29790,#29791),(#29792,#29793),(#29794,#29795),
(#29796,#29797),(#29798,#29799),(#29800,#29801),(#29802,#29803),(#29804,
#29805),(#29806,#29807),(#29808,#29809),(#29810,#29811),(#29812,#29813),
(#29814,#29815),(#29816,#29817),(#29818,#29819),(#29820,#29821),(#29822,
#29823),(#29824,#29825),(#29826,#29827),(#29828,#29829),(#29830,#29831),
(#29832,#29833),(#29834,#29835),(#29836,#29837),(#29838,#29839),(#29840,
#29841),(#29842,#29843),(#29844,#29845),(#29846,#29847),(#29848,#29849),
(#29850,#29851),(#29852,#29853),(#29854,#29855),(#29856,#29857),(#29858,
#29859),(#29860,#29861),(#29862,#29863),(#29864,#29865)),.UNSPECIFIED.,
 .F.,.F.,.F.)
B_SPLINE_SURFACE_WITH_KNOTS((6,1,1,1,1,1,1,1,1,1,1,1,1,1,1,1,1,1,1,1,1,
1,1,1,1,1,1,1,1,1,1,1,1,1,1,1,1,1,1,1,1,1,1,1,1,1,1,1,1,1,1,1,1,1,1,1,1,
1,1,1,1,1,1,1,1,6),(2,2),(-1.,-0.984615384615383,-0.969230769230768,-0.953846153846152,
-0.938461538461537,-0.923076923076922,-0.907692307692306,-0.892307692307691,
-0.876923076923076,-0.86153846153846,-0.846153846153845,-0.83076923076923,
-0.815384615384614,-0.799999999999999,-0.784615384615384,-0.769230769230768,
-0.753846153846153,-0.738461538461538,-0.723076923076922,-0.707692307692307,
-0.692307692307692,-0.676923076923076,-0.661538461538461,-0.646153846153846,
-0.63076923076923,-0.615384615384615,-0.6,-0.584615384615384,-0.569230769230769,
-0.553846153846154,-0.538461538461538,-0.523076923076923,-0.507692307692308,
-0.492307692307692,-0.476923076923077,-0.461538461538462,-0.446153846153846,
-0.430769230769231,-0.415384615384615,-0.4,-0.384615384615385,-0.369230769230769,
-0.353846153846154,-0.338461538461538,-0.323076923076923,-0.307692307692308,
-0.292307692307692,-0.276923076923077,-0.261538461538462,-0.246153846153846,
-0.230769230769231,-0.215384615384615,-0.2,-0.184615384615385,-0.169230769230769,
-0.153846153846154,-0.138461538461538,-0.123076923076923,-0.107692307692308,
-0.0923076923076923,-0.0769230769230769,-0.0615384615384615,-0.0461538461538462,
-0.0307692307692308,-0.0153846153846154,0.),(-1.,1.),.UNSPECIFIED.)
GEOMETRIC_REPRESENTATION_ITEM()
RATIONAL_B_SPLINE_SURFACE(((1.,1.),(1.,1.),(1.,1.),(1.,1.),(1.,1.),(1.,
1.),(1.,1.),(1.,1.),(1.,1.),(1.,1.),(1.,1.),(1.,1.),(1.,1.),(1.,1.),(1.,
1.),(1.,1.),(1.,1.),(1.,1.),(1.,1.),(1.,1.),(1.,1.),(1.,1.),(1.,1.),(1.,
1.),(1.,1.),(1.,1.),(1.,1.),(1.,1.),(1.,1.),(1.,1.),(1.,1.),(1.,1.),(1.,
1.),(1.,1.),(1.,1.),(1.,1.),(1.,1.),(1.,1.),(1.,1.),(1.,1.),(1.,1.),(1.,
1.),(1.,1.),(1.,1.),(1.,1.),(1.,1.),(1.,1.),(1.,1.),(1.,1.),(1.,1.),(1.,
1.),(1.,1.),(1.,1.),(1.,1.),(1.,1.),(1.,1.),(1.,1.),(1.,1.),(1.,1.),(1.,
1.),(1.,1.),(1.,1.),(1.,1.),(1.,1.),(1.,1.),(1.,1.),(1.,1.),(1.,1.),(1.,
1.),(1.,1.)))
REPRESENTATION_ITEM('')
SURFACE()
);
#17=(
BOUNDED_SURFACE()
B_SPLINE_SURFACE(5,1,((#29942,#29943),(#29944,#29945),(#29946,#29947),(#29948,
#29949),(#29950,#29951),(#29952,#29953),(#29954,#29955),(#29956,#29957),
(#29958,#29959),(#29960,#29961),(#29962,#29963),(#29964,#29965),(#29966,
#29967),(#29968,#29969),(#29970,#29971),(#29972,#29973),(#29974,#29975),
(#29976,#29977),(#29978,#29979),(#29980,#29981),(#29982,#29983),(#29984,
#29985),(#29986,#29987),(#29988,#29989),(#29990,#29991),(#29992,#29993),
(#29994,#29995),(#29996,#29997),(#29998,#29999),(#30000,#30001),(#30002,
#30003),(#30004,#30005),(#30006,#30007),(#30008,#30009),(#30010,#30011),
(#30012,#30013),(#30014,#30015),(#30016,#30017),(#30018,#30019),(#30020,
#30021),(#30022,#30023),(#30024,#30025),(#30026,#30027),(#30028,#30029),
(#30030,#30031),(#30032,#30033),(#30034,#30035),(#30036,#30037),(#30038,
#30039),(#30040,#30041),(#30042,#30043),(#30044,#30045),(#30046,#30047),
(#30048,#30049),(#30050,#30051),(#30052,#30053),(#30054,#30055),(#30056,
#30057),(#30058,#30059),(#30060,#30061),(#30062,#30063),(#30064,#30065),
(#30066,#30067),(#30068,#30069),(#30070,#30071),(#30072,#30073),(#30074,
#30075),(#30076,#30077),(#30078,#30079),(#30080,#30081)),.UNSPECIFIED.,
 .F.,.F.,.F.)
B_SPLINE_SURFACE_WITH_KNOTS((6,1,1,1,1,1,1,1,1,1,1,1,1,1,1,1,1,1,1,1,1,
1,1,1,1,1,1,1,1,1,1,1,1,1,1,1,1,1,1,1,1,1,1,1,1,1,1,1,1,1,1,1,1,1,1,1,1,
1,1,1,1,1,1,1,1,6),(2,2),(-1.,-0.984615384615383,-0.969230769230768,-0.953846153846152,
-0.938461538461537,-0.923076923076922,-0.907692307692306,-0.892307692307691,
-0.876923076923076,-0.86153846153846,-0.846153846153845,-0.83076923076923,
-0.815384615384614,-0.799999999999999,-0.784615384615384,-0.769230769230768,
-0.753846153846153,-0.738461538461538,-0.723076923076922,-0.707692307692307,
-0.692307692307692,-0.676923076923076,-0.661538461538461,-0.646153846153846,
-0.63076923076923,-0.615384615384615,-0.6,-0.584615384615384,-0.569230769230769,
-0.553846153846154,-0.538461538461538,-0.523076923076923,-0.507692307692308,
-0.492307692307692,-0.476923076923077,-0.461538461538462,-0.446153846153846,
-0.430769230769231,-0.415384615384615,-0.4,-0.384615384615385,-0.369230769230769,
-0.353846153846154,-0.338461538461538,-0.323076923076923,-0.307692307692308,
-0.292307692307692,-0.276923076923077,-0.261538461538462,-0.246153846153846,
-0.230769230769231,-0.215384615384615,-0.2,-0.184615384615385,-0.169230769230769,
-0.153846153846154,-0.138461538461538,-0.123076923076923,-0.107692307692308,
-0.0923076923076923,-0.0769230769230769,-0.0615384615384615,-0.0461538461538462,
-0.0307692307692308,-0.0153846153846154,0.),(-1.,1.),.UNSPECIFIED.)
GEOMETRIC_REPRESENTATION_ITEM()
RATIONAL_B_SPLINE_SURFACE(((1.,1.),(1.,1.),(1.,1.),(1.,1.),(1.,1.),(1.,
1.),(1.,1.),(1.,1.),(1.,1.),(1.,1.),(1.,1.),(1.,1.),(1.,1.),(1.,1.),(1.,
1.),(1.,1.),(1.,1.),(1.,1.),(1.,1.),(1.,1.),(1.,1.),(1.,1.),(1.,1.),(1.,
1.),(1.,1.),(1.,1.),(1.,1.),(1.,1.),(1.,1.),(1.,1.),(1.,1.),(1.,1.),(1.,
1.),(1.,1.),(1.,1.),(1.,1.),(1.,1.),(1.,1.),(1.,1.),(1.,1.),(1.,1.),(1.,
1.),(1.,1.),(1.,1.),(1.,1.),(1.,1.),(1.,1.),(1.,1.),(1.,1.),(1.,1.),(1.,
1.),(1.,1.),(1.,1.),(1.,1.),(1.,1.),(1.,1.),(1.,1.),(1.,1.),(1.,1.),(1.,
1.),(1.,1.),(1.,1.),(1.,1.),(1.,1.),(1.,1.),(1.,1.),(1.,1.),(1.,1.),(1.,
1.),(1.,1.)))
REPRESENTATION_ITEM('')
SURFACE()
);
#18=(
BOUNDED_SURFACE()
B_SPLINE_SURFACE(5,1,((#30158,#30159),(#30160,#30161),(#30162,#30163),(#30164,
#30165),(#30166,#30167),(#30168,#30169),(#30170,#30171),(#30172,#30173),
(#30174,#30175),(#30176,#30177),(#30178,#30179),(#30180,#30181),(#30182,
#30183),(#30184,#30185),(#30186,#30187),(#30188,#30189),(#30190,#30191),
(#30192,#30193),(#30194,#30195),(#30196,#30197),(#30198,#30199),(#30200,
#30201),(#30202,#30203),(#30204,#30205),(#30206,#30207),(#30208,#30209),
(#30210,#30211),(#30212,#30213),(#30214,#30215),(#30216,#30217),(#30218,
#30219),(#30220,#30221),(#30222,#30223),(#30224,#30225),(#30226,#30227),
(#30228,#30229),(#30230,#30231),(#30232,#30233),(#30234,#30235),(#30236,
#30237),(#30238,#30239),(#30240,#30241),(#30242,#30243),(#30244,#30245),
(#30246,#30247),(#30248,#30249),(#30250,#30251),(#30252,#30253),(#30254,
#30255),(#30256,#30257),(#30258,#30259),(#30260,#30261),(#30262,#30263),
(#30264,#30265),(#30266,#30267),(#30268,#30269),(#30270,#30271),(#30272,
#30273),(#30274,#30275),(#30276,#30277),(#30278,#30279),(#30280,#30281),
(#30282,#30283),(#30284,#30285),(#30286,#30287),(#30288,#30289),(#30290,
#30291),(#30292,#30293),(#30294,#30295),(#30296,#30297)),.UNSPECIFIED.,
 .F.,.F.,.F.)
B_SPLINE_SURFACE_WITH_KNOTS((6,1,1,1,1,1,1,1,1,1,1,1,1,1,1,1,1,1,1,1,1,
1,1,1,1,1,1,1,1,1,1,1,1,1,1,1,1,1,1,1,1,1,1,1,1,1,1,1,1,1,1,1,1,1,1,1,1,
1,1,1,1,1,1,1,1,6),(2,2),(-1.,-0.984615384615383,-0.969230769230768,-0.953846153846152,
-0.938461538461537,-0.923076923076922,-0.907692307692306,-0.892307692307691,
-0.876923076923076,-0.86153846153846,-0.846153846153845,-0.83076923076923,
-0.815384615384614,-0.799999999999999,-0.784615384615384,-0.769230769230768,
-0.753846153846153,-0.738461538461538,-0.723076923076922,-0.707692307692307,
-0.692307692307692,-0.676923076923076,-0.661538461538461,-0.646153846153846,
-0.63076923076923,-0.615384615384615,-0.6,-0.584615384615384,-0.569230769230769,
-0.553846153846154,-0.538461538461538,-0.523076923076923,-0.507692307692308,
-0.492307692307692,-0.476923076923077,-0.461538461538462,-0.446153846153846,
-0.430769230769231,-0.415384615384615,-0.4,-0.384615384615385,-0.369230769230769,
-0.353846153846154,-0.338461538461538,-0.323076923076923,-0.307692307692308,
-0.292307692307692,-0.276923076923077,-0.261538461538462,-0.246153846153846,
-0.230769230769231,-0.215384615384615,-0.2,-0.184615384615385,-0.169230769230769,
-0.153846153846154,-0.138461538461538,-0.123076923076923,-0.107692307692308,
-0.0923076923076923,-0.0769230769230769,-0.0615384615384615,-0.0461538461538462,
-0.0307692307692308,-0.0153846153846154,0.),(-1.,1.),.UNSPECIFIED.)
GEOMETRIC_REPRESENTATION_ITEM()
RATIONAL_B_SPLINE_SURFACE(((1.,1.),(1.,1.),(1.,1.),(1.,1.),(1.,1.),(1.,
1.),(1.,1.),(1.,1.),(1.,1.),(1.,1.),(1.,1.),(1.,1.),(1.,1.),(1.,1.),(1.,
1.),(1.,1.),(1.,1.),(1.,1.),(1.,1.),(1.,1.),(1.,1.),(1.,1.),(1.,1.),(1.,
1.),(1.,1.),(1.,1.),(1.,1.),(1.,1.),(1.,1.),(1.,1.),(1.,1.),(1.,1.),(1.,
1.),(1.,1.),(1.,1.),(1.,1.),(1.,1.),(1.,1.),(1.,1.),(1.,1.),(1.,1.),(1.,
1.),(1.,1.),(1.,1.),(1.,1.),(1.,1.),(1.,1.),(1.,1.),(1.,1.),(1.,1.),(1.,
1.),(1.,1.),(1.,1.),(1.,1.),(1.,1.),(1.,1.),(1.,1.),(1.,1.),(1.,1.),(1.,
1.),(1.,1.),(1.,1.),(1.,1.),(1.,1.),(1.,1.),(1.,1.),(1.,1.),(1.,1.),(1.,
1.),(1.,1.)))
REPRESENTATION_ITEM('')
SURFACE()
);
#19=(
BOUNDED_SURFACE()
B_SPLINE_SURFACE(5,1,((#30374,#30375),(#30376,#30377),(#30378,#30379),(#30380,
#30381),(#30382,#30383),(#30384,#30385),(#30386,#30387),(#30388,#30389),
(#30390,#30391),(#30392,#30393),(#30394,#30395),(#30396,#30397),(#30398,
#30399),(#30400,#30401),(#30402,#30403),(#30404,#30405),(#30406,#30407),
(#30408,#30409),(#30410,#30411),(#30412,#30413),(#30414,#30415),(#30416,
#30417),(#30418,#30419),(#30420,#30421),(#30422,#30423),(#30424,#30425),
(#30426,#30427),(#30428,#30429),(#30430,#30431),(#30432,#30433),(#30434,
#30435),(#30436,#30437),(#30438,#30439),(#30440,#30441),(#30442,#30443),
(#30444,#30445),(#30446,#30447),(#30448,#30449),(#30450,#30451),(#30452,
#30453),(#30454,#30455),(#30456,#30457),(#30458,#30459),(#30460,#30461),
(#30462,#30463),(#30464,#30465),(#30466,#30467),(#30468,#30469),(#30470,
#30471),(#30472,#30473),(#30474,#30475),(#30476,#30477),(#30478,#30479),
(#30480,#30481),(#30482,#30483),(#30484,#30485),(#30486,#30487),(#30488,
#30489),(#30490,#30491),(#30492,#30493),(#30494,#30495),(#30496,#30497),
(#30498,#30499),(#30500,#30501),(#30502,#30503),(#30504,#30505),(#30506,
#30507),(#30508,#30509),(#30510,#30511),(#30512,#30513)),.UNSPECIFIED.,
 .F.,.F.,.F.)
B_SPLINE_SURFACE_WITH_KNOTS((6,1,1,1,1,1,1,1,1,1,1,1,1,1,1,1,1,1,1,1,1,
1,1,1,1,1,1,1,1,1,1,1,1,1,1,1,1,1,1,1,1,1,1,1,1,1,1,1,1,1,1,1,1,1,1,1,1,
1,1,1,1,1,1,1,1,6),(2,2),(-1.,-0.984615384615383,-0.969230769230768,-0.953846153846152,
-0.938461538461537,-0.923076923076922,-0.907692307692306,-0.892307692307691,
-0.876923076923076,-0.86153846153846,-0.846153846153845,-0.83076923076923,
-0.815384615384614,-0.799999999999999,-0.784615384615384,-0.769230769230768,
-0.753846153846153,-0.738461538461538,-0.723076923076922,-0.707692307692307,
-0.692307692307692,-0.676923076923076,-0.661538461538461,-0.646153846153846,
-0.63076923076923,-0.615384615384615,-0.6,-0.584615384615384,-0.569230769230769,
-0.553846153846154,-0.538461538461538,-0.523076923076923,-0.507692307692308,
-0.492307692307692,-0.476923076923077,-0.461538461538462,-0.446153846153846,
-0.430769230769231,-0.415384615384615,-0.4,-0.384615384615385,-0.369230769230769,
-0.353846153846154,-0.338461538461538,-0.323076923076923,-0.307692307692308,
-0.292307692307692,-0.276923076923077,-0.261538461538462,-0.246153846153846,
-0.230769230769231,-0.215384615384615,-0.2,-0.184615384615385,-0.169230769230769,
-0.153846153846154,-0.138461538461538,-0.123076923076923,-0.107692307692308,
-0.0923076923076923,-0.0769230769230769,-0.0615384615384615,-0.0461538461538462,
-0.0307692307692308,-0.0153846153846154,0.),(-1.,1.),.UNSPECIFIED.)
GEOMETRIC_REPRESENTATION_ITEM()
RATIONAL_B_SPLINE_SURFACE(((1.,1.),(1.,1.),(1.,1.),(1.,1.),(1.,1.),(1.,
1.),(1.,1.),(1.,1.),(1.,1.),(1.,1.),(1.,1.),(1.,1.),(1.,1.),(1.,1.),(1.,
1.),(1.,1.),(1.,1.),(1.,1.),(1.,1.),(1.,1.),(1.,1.),(1.,1.),(1.,1.),(1.,
1.),(1.,1.),(1.,1.),(1.,1.),(1.,1.),(1.,1.),(1.,1.),(1.,1.),(1.,1.),(1.,
1.),(1.,1.),(1.,1.),(1.,1.),(1.,1.),(1.,1.),(1.,1.),(1.,1.),(1.,1.),(1.,
1.),(1.,1.),(1.,1.),(1.,1.),(1.,1.),(1.,1.),(1.,1.),(1.,1.),(1.,1.),(1.,
1.),(1.,1.),(1.,1.),(1.,1.),(1.,1.),(1.,1.),(1.,1.),(1.,1.),(1.,1.),(1.,
1.),(1.,1.),(1.,1.),(1.,1.),(1.,1.),(1.,1.),(1.,1.),(1.,1.),(1.,1.),(1.,
1.),(1.,1.)))
REPRESENTATION_ITEM('')
SURFACE()
);
#20=(
BOUNDED_SURFACE()
B_SPLINE_SURFACE(5,1,((#30590,#30591),(#30592,#30593),(#30594,#30595),(#30596,
#30597),(#30598,#30599),(#30600,#30601),(#30602,#30603),(#30604,#30605),
(#30606,#30607),(#30608,#30609),(#30610,#30611),(#30612,#30613),(#30614,
#30615),(#30616,#30617),(#30618,#30619),(#30620,#30621),(#30622,#30623),
(#30624,#30625),(#30626,#30627),(#30628,#30629),(#30630,#30631),(#30632,
#30633),(#30634,#30635),(#30636,#30637),(#30638,#30639),(#30640,#30641),
(#30642,#30643),(#30644,#30645),(#30646,#30647),(#30648,#30649),(#30650,
#30651),(#30652,#30653),(#30654,#30655),(#30656,#30657),(#30658,#30659),
(#30660,#30661),(#30662,#30663),(#30664,#30665),(#30666,#30667),(#30668,
#30669),(#30670,#30671),(#30672,#30673),(#30674,#30675),(#30676,#30677),
(#30678,#30679),(#30680,#30681),(#30682,#30683),(#30684,#30685),(#30686,
#30687),(#30688,#30689),(#30690,#30691),(#30692,#30693),(#30694,#30695),
(#30696,#30697),(#30698,#30699),(#30700,#30701),(#30702,#30703),(#30704,
#30705),(#30706,#30707),(#30708,#30709),(#30710,#30711),(#30712,#30713),
(#30714,#30715),(#30716,#30717),(#30718,#30719),(#30720,#30721),(#30722,
#30723),(#30724,#30725),(#30726,#30727),(#30728,#30729)),.UNSPECIFIED.,
 .F.,.F.,.F.)
B_SPLINE_SURFACE_WITH_KNOTS((6,1,1,1,1,1,1,1,1,1,1,1,1,1,1,1,1,1,1,1,1,
1,1,1,1,1,1,1,1,1,1,1,1,1,1,1,1,1,1,1,1,1,1,1,1,1,1,1,1,1,1,1,1,1,1,1,1,
1,1,1,1,1,1,1,1,6),(2,2),(-1.,-0.984615384615383,-0.969230769230768,-0.953846153846152,
-0.938461538461537,-0.923076923076922,-0.907692307692306,-0.892307692307691,
-0.876923076923076,-0.86153846153846,-0.846153846153845,-0.83076923076923,
-0.815384615384614,-0.799999999999999,-0.784615384615384,-0.769230769230768,
-0.753846153846153,-0.738461538461538,-0.723076923076922,-0.707692307692307,
-0.692307692307692,-0.676923076923076,-0.661538461538461,-0.646153846153846,
-0.63076923076923,-0.615384615384615,-0.6,-0.584615384615384,-0.569230769230769,
-0.553846153846154,-0.538461538461538,-0.523076923076923,-0.507692307692308,
-0.492307692307692,-0.476923076923077,-0.461538461538462,-0.446153846153846,
-0.430769230769231,-0.415384615384615,-0.4,-0.384615384615385,-0.369230769230769,
-0.353846153846154,-0.338461538461538,-0.323076923076923,-0.307692307692308,
-0.292307692307692,-0.276923076923077,-0.261538461538462,-0.246153846153846,
-0.230769230769231,-0.215384615384615,-0.2,-0.184615384615385,-0.169230769230769,
-0.153846153846154,-0.138461538461538,-0.123076923076923,-0.107692307692308,
-0.0923076923076923,-0.0769230769230769,-0.0615384615384615,-0.0461538461538462,
-0.0307692307692308,-0.0153846153846154,0.),(-1.,1.),.UNSPECIFIED.)
GEOMETRIC_REPRESENTATION_ITEM()
RATIONAL_B_SPLINE_SURFACE(((1.,1.),(1.,1.),(1.,1.),(1.,1.),(1.,1.),(1.,
1.),(1.,1.),(1.,1.),(1.,1.),(1.,1.),(1.,1.),(1.,1.),(1.,1.),(1.,1.),(1.,
1.),(1.,1.),(1.,1.),(1.,1.),(1.,1.),(1.,1.),(1.,1.),(1.,1.),(1.,1.),(1.,
1.),(1.,1.),(1.,1.),(1.,1.),(1.,1.),(1.,1.),(1.,1.),(1.,1.),(1.,1.),(1.,
1.),(1.,1.),(1.,1.),(1.,1.),(1.,1.),(1.,1.),(1.,1.),(1.,1.),(1.,1.),(1.,
1.),(1.,1.),(1.,1.),(1.,1.),(1.,1.),(1.,1.),(1.,1.),(1.,1.),(1.,1.),(1.,
1.),(1.,1.),(1.,1.),(1.,1.),(1.,1.),(1.,1.),(1.,1.),(1.,1.),(1.,1.),(1.,
1.),(1.,1.),(1.,1.),(1.,1.),(1.,1.),(1.,1.),(1.,1.),(1.,1.),(1.,1.),(1.,
1.),(1.,1.)))
REPRESENTATION_ITEM('')
SURFACE()
);
#21=(
BOUNDED_SURFACE()
B_SPLINE_SURFACE(5,1,((#30806,#30807),(#30808,#30809),(#30810,#30811),(#30812,
#30813),(#30814,#30815),(#30816,#30817),(#30818,#30819),(#30820,#30821),
(#30822,#30823),(#30824,#30825),(#30826,#30827),(#30828,#30829),(#30830,
#30831),(#30832,#30833),(#30834,#30835),(#30836,#30837),(#30838,#30839),
(#30840,#30841),(#30842,#30843),(#30844,#30845),(#30846,#30847),(#30848,
#30849),(#30850,#30851),(#30852,#30853),(#30854,#30855),(#30856,#30857),
(#30858,#30859),(#30860,#30861),(#30862,#30863),(#30864,#30865),(#30866,
#30867),(#30868,#30869),(#30870,#30871),(#30872,#30873),(#30874,#30875),
(#30876,#30877),(#30878,#30879),(#30880,#30881),(#30882,#30883),(#30884,
#30885),(#30886,#30887),(#30888,#30889),(#30890,#30891),(#30892,#30893),
(#30894,#30895),(#30896,#30897),(#30898,#30899),(#30900,#30901),(#30902,
#30903),(#30904,#30905),(#30906,#30907),(#30908,#30909),(#30910,#30911),
(#30912,#30913),(#30914,#30915),(#30916,#30917),(#30918,#30919),(#30920,
#30921),(#30922,#30923),(#30924,#30925),(#30926,#30927),(#30928,#30929),
(#30930,#30931),(#30932,#30933),(#30934,#30935),(#30936,#30937),(#30938,
#30939),(#30940,#30941),(#30942,#30943),(#30944,#30945)),.UNSPECIFIED.,
 .F.,.F.,.F.)
B_SPLINE_SURFACE_WITH_KNOTS((6,1,1,1,1,1,1,1,1,1,1,1,1,1,1,1,1,1,1,1,1,
1,1,1,1,1,1,1,1,1,1,1,1,1,1,1,1,1,1,1,1,1,1,1,1,1,1,1,1,1,1,1,1,1,1,1,1,
1,1,1,1,1,1,1,1,6),(2,2),(-1.,-0.984615384615383,-0.969230769230768,-0.953846153846152,
-0.938461538461537,-0.923076923076922,-0.907692307692306,-0.892307692307691,
-0.876923076923076,-0.86153846153846,-0.846153846153845,-0.83076923076923,
-0.815384615384614,-0.799999999999999,-0.784615384615384,-0.769230769230768,
-0.753846153846153,-0.738461538461538,-0.723076923076922,-0.707692307692307,
-0.692307692307692,-0.676923076923076,-0.661538461538461,-0.646153846153846,
-0.63076923076923,-0.615384615384615,-0.6,-0.584615384615384,-0.569230769230769,
-0.553846153846154,-0.538461538461538,-0.523076923076923,-0.507692307692308,
-0.492307692307692,-0.476923076923077,-0.461538461538462,-0.446153846153846,
-0.430769230769231,-0.415384615384615,-0.4,-0.384615384615385,-0.369230769230769,
-0.353846153846154,-0.338461538461538,-0.323076923076923,-0.307692307692308,
-0.292307692307692,-0.276923076923077,-0.261538461538462,-0.246153846153846,
-0.230769230769231,-0.215384615384615,-0.2,-0.184615384615385,-0.169230769230769,
-0.153846153846154,-0.138461538461538,-0.123076923076923,-0.107692307692308,
-0.0923076923076923,-0.0769230769230769,-0.0615384615384615,-0.0461538461538462,
-0.0307692307692308,-0.0153846153846154,0.),(-1.,1.),.UNSPECIFIED.)
GEOMETRIC_REPRESENTATION_ITEM()
RATIONAL_B_SPLINE_SURFACE(((1.,1.),(1.,1.),(1.,1.),(1.,1.),(1.,1.),(1.,
1.),(1.,1.),(1.,1.),(1.,1.),(1.,1.),(1.,1.),(1.,1.),(1.,1.),(1.,1.),(1.,
1.),(1.,1.),(1.,1.),(1.,1.),(1.,1.),(1.,1.),(1.,1.),(1.,1.),(1.,1.),(1.,
1.),(1.,1.),(1.,1.),(1.,1.),(1.,1.),(1.,1.),(1.,1.),(1.,1.),(1.,1.),(1.,
1.),(1.,1.),(1.,1.),(1.,1.),(1.,1.),(1.,1.),(1.,1.),(1.,1.),(1.,1.),(1.,
1.),(1.,1.),(1.,1.),(1.,1.),(1.,1.),(1.,1.),(1.,1.),(1.,1.),(1.,1.),(1.,
1.),(1.,1.),(1.,1.),(1.,1.),(1.,1.),(1.,1.),(1.,1.),(1.,1.),(1.,1.),(1.,
1.),(1.,1.),(1.,1.),(1.,1.),(1.,1.),(1.,1.),(1.,1.),(1.,1.),(1.,1.),(1.,
1.),(1.,1.)))
REPRESENTATION_ITEM('')
SURFACE()
);
#22=(
BOUNDED_SURFACE()
B_SPLINE_SURFACE(5,1,((#31022,#31023),(#31024,#31025),(#31026,#31027),(#31028,
#31029),(#31030,#31031),(#31032,#31033),(#31034,#31035),(#31036,#31037),
(#31038,#31039),(#31040,#31041),(#31042,#31043),(#31044,#31045),(#31046,
#31047),(#31048,#31049),(#31050,#31051),(#31052,#31053),(#31054,#31055),
(#31056,#31057),(#31058,#31059),(#31060,#31061),(#31062,#31063),(#31064,
#31065),(#31066,#31067),(#31068,#31069),(#31070,#31071),(#31072,#31073),
(#31074,#31075),(#31076,#31077),(#31078,#31079),(#31080,#31081),(#31082,
#31083),(#31084,#31085),(#31086,#31087),(#31088,#31089),(#31090,#31091),
(#31092,#31093),(#31094,#31095),(#31096,#31097),(#31098,#31099),(#31100,
#31101),(#31102,#31103),(#31104,#31105),(#31106,#31107),(#31108,#31109),
(#31110,#31111),(#31112,#31113),(#31114,#31115),(#31116,#31117),(#31118,
#31119),(#31120,#31121),(#31122,#31123),(#31124,#31125),(#31126,#31127),
(#31128,#31129),(#31130,#31131),(#31132,#31133),(#31134,#31135),(#31136,
#31137),(#31138,#31139),(#31140,#31141),(#31142,#31143),(#31144,#31145),
(#31146,#31147),(#31148,#31149),(#31150,#31151),(#31152,#31153),(#31154,
#31155),(#31156,#31157),(#31158,#31159),(#31160,#31161)),.UNSPECIFIED.,
 .F.,.F.,.F.)
B_SPLINE_SURFACE_WITH_KNOTS((6,1,1,1,1,1,1,1,1,1,1,1,1,1,1,1,1,1,1,1,1,
1,1,1,1,1,1,1,1,1,1,1,1,1,1,1,1,1,1,1,1,1,1,1,1,1,1,1,1,1,1,1,1,1,1,1,1,
1,1,1,1,1,1,1,1,6),(2,2),(-1.,-0.984615384615383,-0.969230769230768,-0.953846153846152,
-0.938461538461537,-0.923076923076922,-0.907692307692306,-0.892307692307691,
-0.876923076923076,-0.86153846153846,-0.846153846153845,-0.83076923076923,
-0.815384615384614,-0.799999999999999,-0.784615384615384,-0.769230769230768,
-0.753846153846153,-0.738461538461538,-0.723076923076922,-0.707692307692307,
-0.692307692307692,-0.676923076923076,-0.661538461538461,-0.646153846153846,
-0.63076923076923,-0.615384615384615,-0.6,-0.584615384615384,-0.569230769230769,
-0.553846153846154,-0.538461538461538,-0.523076923076923,-0.507692307692308,
-0.492307692307692,-0.476923076923077,-0.461538461538462,-0.446153846153846,
-0.430769230769231,-0.415384615384615,-0.4,-0.384615384615385,-0.369230769230769,
-0.353846153846154,-0.338461538461538,-0.323076923076923,-0.307692307692308,
-0.292307692307692,-0.276923076923077,-0.261538461538462,-0.246153846153846,
-0.230769230769231,-0.215384615384615,-0.2,-0.184615384615385,-0.169230769230769,
-0.153846153846154,-0.138461538461538,-0.123076923076923,-0.107692307692308,
-0.0923076923076923,-0.0769230769230769,-0.0615384615384615,-0.0461538461538462,
-0.0307692307692308,-0.0153846153846154,0.),(-1.,1.),.UNSPECIFIED.)
GEOMETRIC_REPRESENTATION_ITEM()
RATIONAL_B_SPLINE_SURFACE(((1.,1.),(1.,1.),(1.,1.),(1.,1.),(1.,1.),(1.,
1.),(1.,1.),(1.,1.),(1.,1.),(1.,1.),(1.,1.),(1.,1.),(1.,1.),(1.,1.),(1.,
1.),(1.,1.),(1.,1.),(1.,1.),(1.,1.),(1.,1.),(1.,1.),(1.,1.),(1.,1.),(1.,
1.),(1.,1.),(1.,1.),(1.,1.),(1.,1.),(1.,1.),(1.,1.),(1.,1.),(1.,1.),(1.,
1.),(1.,1.),(1.,1.),(1.,1.),(1.,1.),(1.,1.),(1.,1.),(1.,1.),(1.,1.),(1.,
1.),(1.,1.),(1.,1.),(1.,1.),(1.,1.),(1.,1.),(1.,1.),(1.,1.),(1.,1.),(1.,
1.),(1.,1.),(1.,1.),(1.,1.),(1.,1.),(1.,1.),(1.,1.),(1.,1.),(1.,1.),(1.,
1.),(1.,1.),(1.,1.),(1.,1.),(1.,1.),(1.,1.),(1.,1.),(1.,1.),(1.,1.),(1.,
1.),(1.,1.)))
REPRESENTATION_ITEM('')
SURFACE()
);
#23=(
BOUNDED_SURFACE()
B_SPLINE_SURFACE(5,1,((#31238,#31239),(#31240,#31241),(#31242,#31243),(#31244,
#31245),(#31246,#31247),(#31248,#31249),(#31250,#31251),(#31252,#31253),
(#31254,#31255),(#31256,#31257),(#31258,#31259),(#31260,#31261),(#31262,
#31263),(#31264,#31265),(#31266,#31267),(#31268,#31269),(#31270,#31271),
(#31272,#31273),(#31274,#31275),(#31276,#31277),(#31278,#31279),(#31280,
#31281),(#31282,#31283),(#31284,#31285),(#31286,#31287),(#31288,#31289),
(#31290,#31291),(#31292,#31293),(#31294,#31295),(#31296,#31297),(#31298,
#31299),(#31300,#31301),(#31302,#31303),(#31304,#31305),(#31306,#31307),
(#31308,#31309),(#31310,#31311),(#31312,#31313),(#31314,#31315),(#31316,
#31317),(#31318,#31319),(#31320,#31321),(#31322,#31323),(#31324,#31325),
(#31326,#31327),(#31328,#31329),(#31330,#31331),(#31332,#31333),(#31334,
#31335),(#31336,#31337),(#31338,#31339),(#31340,#31341),(#31342,#31343),
(#31344,#31345),(#31346,#31347),(#31348,#31349),(#31350,#31351),(#31352,
#31353),(#31354,#31355),(#31356,#31357),(#31358,#31359),(#31360,#31361),
(#31362,#31363),(#31364,#31365),(#31366,#31367),(#31368,#31369),(#31370,
#31371),(#31372,#31373),(#31374,#31375),(#31376,#31377)),.UNSPECIFIED.,
 .F.,.F.,.F.)
B_SPLINE_SURFACE_WITH_KNOTS((6,1,1,1,1,1,1,1,1,1,1,1,1,1,1,1,1,1,1,1,1,
1,1,1,1,1,1,1,1,1,1,1,1,1,1,1,1,1,1,1,1,1,1,1,1,1,1,1,1,1,1,1,1,1,1,1,1,
1,1,1,1,1,1,1,1,6),(2,2),(-1.,-0.984615384615383,-0.969230769230768,-0.953846153846152,
-0.938461538461537,-0.923076923076922,-0.907692307692306,-0.892307692307691,
-0.876923076923076,-0.86153846153846,-0.846153846153845,-0.83076923076923,
-0.815384615384614,-0.799999999999999,-0.784615384615384,-0.769230769230768,
-0.753846153846153,-0.738461538461538,-0.723076923076922,-0.707692307692307,
-0.692307692307692,-0.676923076923076,-0.661538461538461,-0.646153846153846,
-0.63076923076923,-0.615384615384615,-0.6,-0.584615384615384,-0.569230769230769,
-0.553846153846154,-0.538461538461538,-0.523076923076923,-0.507692307692308,
-0.492307692307692,-0.476923076923077,-0.461538461538462,-0.446153846153846,
-0.430769230769231,-0.415384615384615,-0.4,-0.384615384615385,-0.369230769230769,
-0.353846153846154,-0.338461538461538,-0.323076923076923,-0.307692307692308,
-0.292307692307692,-0.276923076923077,-0.261538461538462,-0.246153846153846,
-0.230769230769231,-0.215384615384615,-0.2,-0.184615384615385,-0.169230769230769,
-0.153846153846154,-0.138461538461538,-0.123076923076923,-0.107692307692308,
-0.0923076923076923,-0.0769230769230769,-0.0615384615384615,-0.0461538461538462,
-0.0307692307692308,-0.0153846153846154,0.),(-1.,1.),.UNSPECIFIED.)
GEOMETRIC_REPRESENTATION_ITEM()
RATIONAL_B_SPLINE_SURFACE(((1.,1.),(1.,1.),(1.,1.),(1.,1.),(1.,1.),(1.,
1.),(1.,1.),(1.,1.),(1.,1.),(1.,1.),(1.,1.),(1.,1.),(1.,1.),(1.,1.),(1.,
1.),(1.,1.),(1.,1.),(1.,1.),(1.,1.),(1.,1.),(1.,1.),(1.,1.),(1.,1.),(1.,
1.),(1.,1.),(1.,1.),(1.,1.),(1.,1.),(1.,1.),(1.,1.),(1.,1.),(1.,1.),(1.,
1.),(1.,1.),(1.,1.),(1.,1.),(1.,1.),(1.,1.),(1.,1.),(1.,1.),(1.,1.),(1.,
1.),(1.,1.),(1.,1.),(1.,1.),(1.,1.),(1.,1.),(1.,1.),(1.,1.),(1.,1.),(1.,
1.),(1.,1.),(1.,1.),(1.,1.),(1.,1.),(1.,1.),(1.,1.),(1.,1.),(1.,1.),(1.,
1.),(1.,1.),(1.,1.),(1.,1.),(1.,1.),(1.,1.),(1.,1.),(1.,1.),(1.,1.),(1.,
1.),(1.,1.)))
REPRESENTATION_ITEM('')
SURFACE()
);
#24=(
BOUNDED_SURFACE()
B_SPLINE_SURFACE(5,1,((#31454,#31455),(#31456,#31457),(#31458,#31459),(#31460,
#31461),(#31462,#31463),(#31464,#31465),(#31466,#31467),(#31468,#31469),
(#31470,#31471),(#31472,#31473),(#31474,#31475),(#31476,#31477),(#31478,
#31479),(#31480,#31481),(#31482,#31483),(#31484,#31485),(#31486,#31487),
(#31488,#31489),(#31490,#31491),(#31492,#31493),(#31494,#31495),(#31496,
#31497),(#31498,#31499),(#31500,#31501),(#31502,#31503),(#31504,#31505),
(#31506,#31507),(#31508,#31509),(#31510,#31511),(#31512,#31513),(#31514,
#31515),(#31516,#31517),(#31518,#31519),(#31520,#31521),(#31522,#31523),
(#31524,#31525),(#31526,#31527),(#31528,#31529),(#31530,#31531),(#31532,
#31533),(#31534,#31535),(#31536,#31537),(#31538,#31539),(#31540,#31541),
(#31542,#31543),(#31544,#31545),(#31546,#31547),(#31548,#31549),(#31550,
#31551),(#31552,#31553),(#31554,#31555),(#31556,#31557),(#31558,#31559),
(#31560,#31561),(#31562,#31563),(#31564,#31565),(#31566,#31567),(#31568,
#31569),(#31570,#31571),(#31572,#31573),(#31574,#31575),(#31576,#31577),
(#31578,#31579),(#31580,#31581),(#31582,#31583),(#31584,#31585),(#31586,
#31587),(#31588,#31589),(#31590,#31591),(#31592,#31593)),.UNSPECIFIED.,
 .F.,.F.,.F.)
B_SPLINE_SURFACE_WITH_KNOTS((6,1,1,1,1,1,1,1,1,1,1,1,1,1,1,1,1,1,1,1,1,
1,1,1,1,1,1,1,1,1,1,1,1,1,1,1,1,1,1,1,1,1,1,1,1,1,1,1,1,1,1,1,1,1,1,1,1,
1,1,1,1,1,1,1,1,6),(2,2),(-1.,-0.984615384615383,-0.969230769230768,-0.953846153846152,
-0.938461538461537,-0.923076923076922,-0.907692307692306,-0.892307692307691,
-0.876923076923076,-0.86153846153846,-0.846153846153845,-0.83076923076923,
-0.815384615384614,-0.799999999999999,-0.784615384615384,-0.769230769230768,
-0.753846153846153,-0.738461538461538,-0.723076923076922,-0.707692307692307,
-0.692307692307692,-0.676923076923076,-0.661538461538461,-0.646153846153846,
-0.63076923076923,-0.615384615384615,-0.6,-0.584615384615384,-0.569230769230769,
-0.553846153846154,-0.538461538461538,-0.523076923076923,-0.507692307692308,
-0.492307692307692,-0.476923076923077,-0.461538461538462,-0.446153846153846,
-0.430769230769231,-0.415384615384615,-0.4,-0.384615384615385,-0.369230769230769,
-0.353846153846154,-0.338461538461538,-0.323076923076923,-0.307692307692308,
-0.292307692307692,-0.276923076923077,-0.261538461538462,-0.246153846153846,
-0.230769230769231,-0.215384615384615,-0.2,-0.184615384615385,-0.169230769230769,
-0.153846153846154,-0.138461538461538,-0.123076923076923,-0.107692307692308,
-0.0923076923076923,-0.0769230769230769,-0.0615384615384615,-0.0461538461538462,
-0.0307692307692308,-0.0153846153846154,0.),(-1.,1.),.UNSPECIFIED.)
GEOMETRIC_REPRESENTATION_ITEM()
RATIONAL_B_SPLINE_SURFACE(((1.,1.),(1.,1.),(1.,1.),(1.,1.),(1.,1.),(1.,
1.),(1.,1.),(1.,1.),(1.,1.),(1.,1.),(1.,1.),(1.,1.),(1.,1.),(1.,1.),(1.,
1.),(1.,1.),(1.,1.),(1.,1.),(1.,1.),(1.,1.),(1.,1.),(1.,1.),(1.,1.),(1.,
1.),(1.,1.),(1.,1.),(1.,1.),(1.,1.),(1.,1.),(1.,1.),(1.,1.),(1.,1.),(1.,
1.),(1.,1.),(1.,1.),(1.,1.),(1.,1.),(1.,1.),(1.,1.),(1.,1.),(1.,1.),(1.,
1.),(1.,1.),(1.,1.),(1.,1.),(1.,1.),(1.,1.),(1.,1.),(1.,1.),(1.,1.),(1.,
1.),(1.,1.),(1.,1.),(1.,1.),(1.,1.),(1.,1.),(1.,1.),(1.,1.),(1.,1.),(1.,
1.),(1.,1.),(1.,1.),(1.,1.),(1.,1.),(1.,1.),(1.,1.),(1.,1.),(1.,1.),(1.,
1.),(1.,1.)))
REPRESENTATION_ITEM('')
SURFACE()
);
#25=(
BOUNDED_SURFACE()
B_SPLINE_SURFACE(5,1,((#31670,#31671),(#31672,#31673),(#31674,#31675),(#31676,
#31677),(#31678,#31679),(#31680,#31681),(#31682,#31683),(#31684,#31685),
(#31686,#31687),(#31688,#31689),(#31690,#31691),(#31692,#31693),(#31694,
#31695),(#31696,#31697),(#31698,#31699),(#31700,#31701),(#31702,#31703),
(#31704,#31705),(#31706,#31707),(#31708,#31709),(#31710,#31711),(#31712,
#31713),(#31714,#31715),(#31716,#31717),(#31718,#31719),(#31720,#31721),
(#31722,#31723),(#31724,#31725),(#31726,#31727),(#31728,#31729),(#31730,
#31731),(#31732,#31733),(#31734,#31735),(#31736,#31737),(#31738,#31739),
(#31740,#31741),(#31742,#31743),(#31744,#31745),(#31746,#31747),(#31748,
#31749),(#31750,#31751),(#31752,#31753),(#31754,#31755),(#31756,#31757),
(#31758,#31759),(#31760,#31761),(#31762,#31763),(#31764,#31765),(#31766,
#31767),(#31768,#31769),(#31770,#31771),(#31772,#31773),(#31774,#31775),
(#31776,#31777),(#31778,#31779),(#31780,#31781),(#31782,#31783),(#31784,
#31785),(#31786,#31787),(#31788,#31789),(#31790,#31791),(#31792,#31793),
(#31794,#31795),(#31796,#31797),(#31798,#31799),(#31800,#31801),(#31802,
#31803),(#31804,#31805),(#31806,#31807),(#31808,#31809)),.UNSPECIFIED.,
 .F.,.F.,.F.)
B_SPLINE_SURFACE_WITH_KNOTS((6,1,1,1,1,1,1,1,1,1,1,1,1,1,1,1,1,1,1,1,1,
1,1,1,1,1,1,1,1,1,1,1,1,1,1,1,1,1,1,1,1,1,1,1,1,1,1,1,1,1,1,1,1,1,1,1,1,
1,1,1,1,1,1,1,1,6),(2,2),(-1.,-0.984615384615383,-0.969230769230768,-0.953846153846152,
-0.938461538461537,-0.923076923076922,-0.907692307692306,-0.892307692307691,
-0.876923076923076,-0.86153846153846,-0.846153846153845,-0.83076923076923,
-0.815384615384614,-0.799999999999999,-0.784615384615384,-0.769230769230768,
-0.753846153846153,-0.738461538461538,-0.723076923076922,-0.707692307692307,
-0.692307692307692,-0.676923076923076,-0.661538461538461,-0.646153846153846,
-0.63076923076923,-0.615384615384615,-0.6,-0.584615384615384,-0.569230769230769,
-0.553846153846154,-0.538461538461538,-0.523076923076923,-0.507692307692308,
-0.492307692307692,-0.476923076923077,-0.461538461538462,-0.446153846153846,
-0.430769230769231,-0.415384615384615,-0.4,-0.384615384615385,-0.369230769230769,
-0.353846153846154,-0.338461538461538,-0.323076923076923,-0.307692307692308,
-0.292307692307692,-0.276923076923077,-0.261538461538462,-0.246153846153846,
-0.230769230769231,-0.215384615384615,-0.2,-0.184615384615385,-0.169230769230769,
-0.153846153846154,-0.138461538461538,-0.123076923076923,-0.107692307692308,
-0.0923076923076923,-0.0769230769230769,-0.0615384615384615,-0.0461538461538462,
-0.0307692307692308,-0.0153846153846154,0.),(-1.,1.),.UNSPECIFIED.)
GEOMETRIC_REPRESENTATION_ITEM()
RATIONAL_B_SPLINE_SURFACE(((1.,1.),(1.,1.),(1.,1.),(1.,1.),(1.,1.),(1.,
1.),(1.,1.),(1.,1.),(1.,1.),(1.,1.),(1.,1.),(1.,1.),(1.,1.),(1.,1.),(1.,
1.),(1.,1.),(1.,1.),(1.,1.),(1.,1.),(1.,1.),(1.,1.),(1.,1.),(1.,1.),(1.,
1.),(1.,1.),(1.,1.),(1.,1.),(1.,1.),(1.,1.),(1.,1.),(1.,1.),(1.,1.),(1.,
1.),(1.,1.),(1.,1.),(1.,1.),(1.,1.),(1.,1.),(1.,1.),(1.,1.),(1.,1.),(1.,
1.),(1.,1.),(1.,1.),(1.,1.),(1.,1.),(1.,1.),(1.,1.),(1.,1.),(1.,1.),(1.,
1.),(1.,1.),(1.,1.),(1.,1.),(1.,1.),(1.,1.),(1.,1.),(1.,1.),(1.,1.),(1.,
1.),(1.,1.),(1.,1.),(1.,1.),(1.,1.),(1.,1.),(1.,1.),(1.,1.),(1.,1.),(1.,
1.),(1.,1.)))
REPRESENTATION_ITEM('')
SURFACE()
);
#26=(
BOUNDED_SURFACE()
B_SPLINE_SURFACE(5,1,((#31886,#31887),(#31888,#31889),(#31890,#31891),(#31892,
#31893),(#31894,#31895),(#31896,#31897),(#31898,#31899),(#31900,#31901),
(#31902,#31903),(#31904,#31905),(#31906,#31907),(#31908,#31909),(#31910,
#31911),(#31912,#31913),(#31914,#31915),(#31916,#31917),(#31918,#31919),
(#31920,#31921),(#31922,#31923),(#31924,#31925),(#31926,#31927),(#31928,
#31929),(#31930,#31931),(#31932,#31933),(#31934,#31935),(#31936,#31937),
(#31938,#31939),(#31940,#31941),(#31942,#31943),(#31944,#31945),(#31946,
#31947),(#31948,#31949),(#31950,#31951),(#31952,#31953),(#31954,#31955),
(#31956,#31957),(#31958,#31959),(#31960,#31961),(#31962,#31963),(#31964,
#31965),(#31966,#31967),(#31968,#31969),(#31970,#31971),(#31972,#31973),
(#31974,#31975),(#31976,#31977),(#31978,#31979),(#31980,#31981),(#31982,
#31983),(#31984,#31985),(#31986,#31987),(#31988,#31989),(#31990,#31991),
(#31992,#31993),(#31994,#31995),(#31996,#31997),(#31998,#31999),(#32000,
#32001),(#32002,#32003),(#32004,#32005),(#32006,#32007),(#32008,#32009),
(#32010,#32011),(#32012,#32013),(#32014,#32015),(#32016,#32017),(#32018,
#32019),(#32020,#32021),(#32022,#32023),(#32024,#32025)),.UNSPECIFIED.,
 .F.,.F.,.F.)
B_SPLINE_SURFACE_WITH_KNOTS((6,1,1,1,1,1,1,1,1,1,1,1,1,1,1,1,1,1,1,1,1,
1,1,1,1,1,1,1,1,1,1,1,1,1,1,1,1,1,1,1,1,1,1,1,1,1,1,1,1,1,1,1,1,1,1,1,1,
1,1,1,1,1,1,1,1,6),(2,2),(-1.,-0.984615384615383,-0.969230769230768,-0.953846153846152,
-0.938461538461537,-0.923076923076922,-0.907692307692306,-0.892307692307691,
-0.876923076923076,-0.86153846153846,-0.846153846153845,-0.83076923076923,
-0.815384615384614,-0.799999999999999,-0.784615384615384,-0.769230769230768,
-0.753846153846153,-0.738461538461538,-0.723076923076922,-0.707692307692307,
-0.692307692307692,-0.676923076923076,-0.661538461538461,-0.646153846153846,
-0.63076923076923,-0.615384615384615,-0.6,-0.584615384615384,-0.569230769230769,
-0.553846153846154,-0.538461538461538,-0.523076923076923,-0.507692307692308,
-0.492307692307692,-0.476923076923077,-0.461538461538462,-0.446153846153846,
-0.430769230769231,-0.415384615384615,-0.4,-0.384615384615385,-0.369230769230769,
-0.353846153846154,-0.338461538461538,-0.323076923076923,-0.307692307692308,
-0.292307692307692,-0.276923076923077,-0.261538461538462,-0.246153846153846,
-0.230769230769231,-0.215384615384615,-0.2,-0.184615384615385,-0.169230769230769,
-0.153846153846154,-0.138461538461538,-0.123076923076923,-0.107692307692308,
-0.0923076923076923,-0.0769230769230769,-0.0615384615384615,-0.0461538461538462,
-0.0307692307692308,-0.0153846153846154,0.),(-1.,1.),.UNSPECIFIED.)
GEOMETRIC_REPRESENTATION_ITEM()
RATIONAL_B_SPLINE_SURFACE(((1.,1.),(1.,1.),(1.,1.),(1.,1.),(1.,1.),(1.,
1.),(1.,1.),(1.,1.),(1.,1.),(1.,1.),(1.,1.),(1.,1.),(1.,1.),(1.,1.),(1.,
1.),(1.,1.),(1.,1.),(1.,1.),(1.,1.),(1.,1.),(1.,1.),(1.,1.),(1.,1.),(1.,
1.),(1.,1.),(1.,1.),(1.,1.),(1.,1.),(1.,1.),(1.,1.),(1.,1.),(1.,1.),(1.,
1.),(1.,1.),(1.,1.),(1.,1.),(1.,1.),(1.,1.),(1.,1.),(1.,1.),(1.,1.),(1.,
1.),(1.,1.),(1.,1.),(1.,1.),(1.,1.),(1.,1.),(1.,1.),(1.,1.),(1.,1.),(1.,
1.),(1.,1.),(1.,1.),(1.,1.),(1.,1.),(1.,1.),(1.,1.),(1.,1.),(1.,1.),(1.,
1.),(1.,1.),(1.,1.),(1.,1.),(1.,1.),(1.,1.),(1.,1.),(1.,1.),(1.,1.),(1.,
1.),(1.,1.)))
REPRESENTATION_ITEM('')
SURFACE()
);
#27=(
BOUNDED_SURFACE()
B_SPLINE_SURFACE(5,1,((#32102,#32103),(#32104,#32105),(#32106,#32107),(#32108,
#32109),(#32110,#32111),(#32112,#32113),(#32114,#32115),(#32116,#32117),
(#32118,#32119),(#32120,#32121),(#32122,#32123),(#32124,#32125),(#32126,
#32127),(#32128,#32129),(#32130,#32131),(#32132,#32133),(#32134,#32135),
(#32136,#32137),(#32138,#32139),(#32140,#32141),(#32142,#32143),(#32144,
#32145),(#32146,#32147),(#32148,#32149),(#32150,#32151),(#32152,#32153),
(#32154,#32155),(#32156,#32157),(#32158,#32159),(#32160,#32161),(#32162,
#32163),(#32164,#32165),(#32166,#32167),(#32168,#32169),(#32170,#32171),
(#32172,#32173),(#32174,#32175),(#32176,#32177),(#32178,#32179),(#32180,
#32181),(#32182,#32183),(#32184,#32185),(#32186,#32187),(#32188,#32189),
(#32190,#32191),(#32192,#32193),(#32194,#32195),(#32196,#32197),(#32198,
#32199),(#32200,#32201),(#32202,#32203),(#32204,#32205),(#32206,#32207),
(#32208,#32209),(#32210,#32211),(#32212,#32213),(#32214,#32215),(#32216,
#32217),(#32218,#32219),(#32220,#32221),(#32222,#32223),(#32224,#32225),
(#32226,#32227),(#32228,#32229),(#32230,#32231),(#32232,#32233),(#32234,
#32235),(#32236,#32237),(#32238,#32239),(#32240,#32241)),.UNSPECIFIED.,
 .F.,.F.,.F.)
B_SPLINE_SURFACE_WITH_KNOTS((6,1,1,1,1,1,1,1,1,1,1,1,1,1,1,1,1,1,1,1,1,
1,1,1,1,1,1,1,1,1,1,1,1,1,1,1,1,1,1,1,1,1,1,1,1,1,1,1,1,1,1,1,1,1,1,1,1,
1,1,1,1,1,1,1,1,6),(2,2),(-1.,-0.984615384615383,-0.969230769230768,-0.953846153846152,
-0.938461538461537,-0.923076923076922,-0.907692307692306,-0.892307692307691,
-0.876923076923076,-0.86153846153846,-0.846153846153845,-0.83076923076923,
-0.815384615384614,-0.799999999999999,-0.784615384615384,-0.769230769230768,
-0.753846153846153,-0.738461538461538,-0.723076923076922,-0.707692307692307,
-0.692307692307692,-0.676923076923076,-0.661538461538461,-0.646153846153846,
-0.63076923076923,-0.615384615384615,-0.6,-0.584615384615384,-0.569230769230769,
-0.553846153846154,-0.538461538461538,-0.523076923076923,-0.507692307692308,
-0.492307692307692,-0.476923076923077,-0.461538461538462,-0.446153846153846,
-0.430769230769231,-0.415384615384615,-0.4,-0.384615384615385,-0.369230769230769,
-0.353846153846154,-0.338461538461538,-0.323076923076923,-0.307692307692308,
-0.292307692307692,-0.276923076923077,-0.261538461538462,-0.246153846153846,
-0.230769230769231,-0.215384615384615,-0.2,-0.184615384615385,-0.169230769230769,
-0.153846153846154,-0.138461538461538,-0.123076923076923,-0.107692307692308,
-0.0923076923076923,-0.0769230769230769,-0.0615384615384615,-0.0461538461538462,
-0.0307692307692308,-0.0153846153846154,0.),(-1.,1.),.UNSPECIFIED.)
GEOMETRIC_REPRESENTATION_ITEM()
RATIONAL_B_SPLINE_SURFACE(((1.,1.),(1.,1.),(1.,1.),(1.,1.),(1.,1.),(1.,
1.),(1.,1.),(1.,1.),(1.,1.),(1.,1.),(1.,1.),(1.,1.),(1.,1.),(1.,1.),(1.,
1.),(1.,1.),(1.,1.),(1.,1.),(1.,1.),(1.,1.),(1.,1.),(1.,1.),(1.,1.),(1.,
1.),(1.,1.),(1.,1.),(1.,1.),(1.,1.),(1.,1.),(1.,1.),(1.,1.),(1.,1.),(1.,
1.),(1.,1.),(1.,1.),(1.,1.),(1.,1.),(1.,1.),(1.,1.),(1.,1.),(1.,1.),(1.,
1.),(1.,1.),(1.,1.),(1.,1.),(1.,1.),(1.,1.),(1.,1.),(1.,1.),(1.,1.),(1.,
1.),(1.,1.),(1.,1.),(1.,1.),(1.,1.),(1.,1.),(1.,1.),(1.,1.),(1.,1.),(1.,
1.),(1.,1.),(1.,1.),(1.,1.),(1.,1.),(1.,1.),(1.,1.),(1.,1.),(1.,1.),(1.,
1.),(1.,1.)))
REPRESENTATION_ITEM('')
SURFACE()
);
#28=(
BOUNDED_SURFACE()
B_SPLINE_SURFACE(5,1,((#32318,#32319),(#32320,#32321),(#32322,#32323),(#32324,
#32325),(#32326,#32327),(#32328,#32329),(#32330,#32331),(#32332,#32333),
(#32334,#32335),(#32336,#32337),(#32338,#32339),(#32340,#32341),(#32342,
#32343),(#32344,#32345),(#32346,#32347),(#32348,#32349),(#32350,#32351),
(#32352,#32353),(#32354,#32355),(#32356,#32357),(#32358,#32359),(#32360,
#32361),(#32362,#32363),(#32364,#32365),(#32366,#32367),(#32368,#32369),
(#32370,#32371),(#32372,#32373),(#32374,#32375),(#32376,#32377),(#32378,
#32379),(#32380,#32381),(#32382,#32383),(#32384,#32385),(#32386,#32387),
(#32388,#32389),(#32390,#32391),(#32392,#32393),(#32394,#32395),(#32396,
#32397),(#32398,#32399),(#32400,#32401),(#32402,#32403),(#32404,#32405),
(#32406,#32407),(#32408,#32409),(#32410,#32411),(#32412,#32413),(#32414,
#32415),(#32416,#32417),(#32418,#32419),(#32420,#32421),(#32422,#32423),
(#32424,#32425),(#32426,#32427),(#32428,#32429),(#32430,#32431),(#32432,
#32433),(#32434,#32435),(#32436,#32437),(#32438,#32439),(#32440,#32441),
(#32442,#32443),(#32444,#32445),(#32446,#32447),(#32448,#32449),(#32450,
#32451),(#32452,#32453),(#32454,#32455),(#32456,#32457)),.UNSPECIFIED.,
 .F.,.F.,.F.)
B_SPLINE_SURFACE_WITH_KNOTS((6,1,1,1,1,1,1,1,1,1,1,1,1,1,1,1,1,1,1,1,1,
1,1,1,1,1,1,1,1,1,1,1,1,1,1,1,1,1,1,1,1,1,1,1,1,1,1,1,1,1,1,1,1,1,1,1,1,
1,1,1,1,1,1,1,1,6),(2,2),(-1.,-0.984615384615383,-0.969230769230768,-0.953846153846152,
-0.938461538461537,-0.923076923076922,-0.907692307692306,-0.892307692307691,
-0.876923076923076,-0.86153846153846,-0.846153846153845,-0.83076923076923,
-0.815384615384614,-0.799999999999999,-0.784615384615384,-0.769230769230768,
-0.753846153846153,-0.738461538461538,-0.723076923076922,-0.707692307692307,
-0.692307692307692,-0.676923076923076,-0.661538461538461,-0.646153846153846,
-0.63076923076923,-0.615384615384615,-0.6,-0.584615384615384,-0.569230769230769,
-0.553846153846154,-0.538461538461538,-0.523076923076923,-0.507692307692308,
-0.492307692307692,-0.476923076923077,-0.461538461538462,-0.446153846153846,
-0.430769230769231,-0.415384615384615,-0.4,-0.384615384615385,-0.369230769230769,
-0.353846153846154,-0.338461538461538,-0.323076923076923,-0.307692307692308,
-0.292307692307692,-0.276923076923077,-0.261538461538462,-0.246153846153846,
-0.230769230769231,-0.215384615384615,-0.2,-0.184615384615385,-0.169230769230769,
-0.153846153846154,-0.138461538461538,-0.123076923076923,-0.107692307692308,
-0.0923076923076923,-0.0769230769230769,-0.0615384615384615,-0.0461538461538462,
-0.0307692307692308,-0.0153846153846154,0.),(-1.,1.),.UNSPECIFIED.)
GEOMETRIC_REPRESENTATION_ITEM()
RATIONAL_B_SPLINE_SURFACE(((1.,1.),(1.,1.),(1.,1.),(1.,1.),(1.,1.),(1.,
1.),(1.,1.),(1.,1.),(1.,1.),(1.,1.),(1.,1.),(1.,1.),(1.,1.),(1.,1.),(1.,
1.),(1.,1.),(1.,1.),(1.,1.),(1.,1.),(1.,1.),(1.,1.),(1.,1.),(1.,1.),(1.,
1.),(1.,1.),(1.,1.),(1.,1.),(1.,1.),(1.,1.),(1.,1.),(1.,1.),(1.,1.),(1.,
1.),(1.,1.),(1.,1.),(1.,1.),(1.,1.),(1.,1.),(1.,1.),(1.,1.),(1.,1.),(1.,
1.),(1.,1.),(1.,1.),(1.,1.),(1.,1.),(1.,1.),(1.,1.),(1.,1.),(1.,1.),(1.,
1.),(1.,1.),(1.,1.),(1.,1.),(1.,1.),(1.,1.),(1.,1.),(1.,1.),(1.,1.),(1.,
1.),(1.,1.),(1.,1.),(1.,1.),(1.,1.),(1.,1.),(1.,1.),(1.,1.),(1.,1.),(1.,
1.),(1.,1.)))
REPRESENTATION_ITEM('')
SURFACE()
);
#29=(
BOUNDED_SURFACE()
B_SPLINE_SURFACE(5,1,((#32534,#32535),(#32536,#32537),(#32538,#32539),(#32540,
#32541),(#32542,#32543),(#32544,#32545),(#32546,#32547),(#32548,#32549),
(#32550,#32551),(#32552,#32553),(#32554,#32555),(#32556,#32557),(#32558,
#32559),(#32560,#32561),(#32562,#32563),(#32564,#32565),(#32566,#32567),
(#32568,#32569),(#32570,#32571),(#32572,#32573),(#32574,#32575),(#32576,
#32577),(#32578,#32579),(#32580,#32581),(#32582,#32583),(#32584,#32585),
(#32586,#32587),(#32588,#32589),(#32590,#32591),(#32592,#32593),(#32594,
#32595),(#32596,#32597),(#32598,#32599),(#32600,#32601),(#32602,#32603),
(#32604,#32605),(#32606,#32607),(#32608,#32609),(#32610,#32611),(#32612,
#32613),(#32614,#32615),(#32616,#32617),(#32618,#32619),(#32620,#32621),
(#32622,#32623),(#32624,#32625),(#32626,#32627),(#32628,#32629),(#32630,
#32631),(#32632,#32633),(#32634,#32635),(#32636,#32637),(#32638,#32639),
(#32640,#32641),(#32642,#32643),(#32644,#32645),(#32646,#32647),(#32648,
#32649),(#32650,#32651),(#32652,#32653),(#32654,#32655),(#32656,#32657),
(#32658,#32659),(#32660,#32661),(#32662,#32663),(#32664,#32665),(#32666,
#32667),(#32668,#32669),(#32670,#32671),(#32672,#32673)),.UNSPECIFIED.,
 .F.,.F.,.F.)
B_SPLINE_SURFACE_WITH_KNOTS((6,1,1,1,1,1,1,1,1,1,1,1,1,1,1,1,1,1,1,1,1,
1,1,1,1,1,1,1,1,1,1,1,1,1,1,1,1,1,1,1,1,1,1,1,1,1,1,1,1,1,1,1,1,1,1,1,1,
1,1,1,1,1,1,1,1,6),(2,2),(-1.,-0.984615384615383,-0.969230769230768,-0.953846153846152,
-0.938461538461537,-0.923076923076922,-0.907692307692306,-0.892307692307691,
-0.876923076923076,-0.86153846153846,-0.846153846153845,-0.83076923076923,
-0.815384615384614,-0.799999999999999,-0.784615384615384,-0.769230769230768,
-0.753846153846153,-0.738461538461538,-0.723076923076922,-0.707692307692307,
-0.692307692307692,-0.676923076923076,-0.661538461538461,-0.646153846153846,
-0.63076923076923,-0.615384615384615,-0.6,-0.584615384615384,-0.569230769230769,
-0.553846153846154,-0.538461538461538,-0.523076923076923,-0.507692307692308,
-0.492307692307692,-0.476923076923077,-0.461538461538462,-0.446153846153846,
-0.430769230769231,-0.415384615384615,-0.4,-0.384615384615385,-0.369230769230769,
-0.353846153846154,-0.338461538461538,-0.323076923076923,-0.307692307692308,
-0.292307692307692,-0.276923076923077,-0.261538461538462,-0.246153846153846,
-0.230769230769231,-0.215384615384615,-0.2,-0.184615384615385,-0.169230769230769,
-0.153846153846154,-0.138461538461538,-0.123076923076923,-0.107692307692308,
-0.0923076923076923,-0.0769230769230769,-0.0615384615384615,-0.0461538461538462,
-0.0307692307692308,-0.0153846153846154,0.),(-1.,1.),.UNSPECIFIED.)
GEOMETRIC_REPRESENTATION_ITEM()
RATIONAL_B_SPLINE_SURFACE(((1.,1.),(1.,1.),(1.,1.),(1.,1.),(1.,1.),(1.,
1.),(1.,1.),(1.,1.),(1.,1.),(1.,1.),(1.,1.),(1.,1.),(1.,1.),(1.,1.),(1.,
1.),(1.,1.),(1.,1.),(1.,1.),(1.,1.),(1.,1.),(1.,1.),(1.,1.),(1.,1.),(1.,
1.),(1.,1.),(1.,1.),(1.,1.),(1.,1.),(1.,1.),(1.,1.),(1.,1.),(1.,1.),(1.,
1.),(1.,1.),(1.,1.),(1.,1.),(1.,1.),(1.,1.),(1.,1.),(1.,1.),(1.,1.),(1.,
1.),(1.,1.),(1.,1.),(1.,1.),(1.,1.),(1.,1.),(1.,1.),(1.,1.),(1.,1.),(1.,
1.),(1.,1.),(1.,1.),(1.,1.),(1.,1.),(1.,1.),(1.,1.),(1.,1.),(1.,1.),(1.,
1.),(1.,1.),(1.,1.),(1.,1.),(1.,1.),(1.,1.),(1.,1.),(1.,1.),(1.,1.),(1.,
1.),(1.,1.)))
REPRESENTATION_ITEM('')
SURFACE()
);
#30=(
BOUNDED_SURFACE()
B_SPLINE_SURFACE(5,1,((#32750,#32751),(#32752,#32753),(#32754,#32755),(#32756,
#32757),(#32758,#32759),(#32760,#32761),(#32762,#32763),(#32764,#32765),
(#32766,#32767),(#32768,#32769),(#32770,#32771),(#32772,#32773),(#32774,
#32775),(#32776,#32777),(#32778,#32779),(#32780,#32781),(#32782,#32783),
(#32784,#32785),(#32786,#32787),(#32788,#32789),(#32790,#32791),(#32792,
#32793),(#32794,#32795),(#32796,#32797),(#32798,#32799),(#32800,#32801),
(#32802,#32803),(#32804,#32805),(#32806,#32807),(#32808,#32809),(#32810,
#32811),(#32812,#32813),(#32814,#32815),(#32816,#32817),(#32818,#32819),
(#32820,#32821),(#32822,#32823),(#32824,#32825),(#32826,#32827),(#32828,
#32829),(#32830,#32831),(#32832,#32833),(#32834,#32835),(#32836,#32837),
(#32838,#32839),(#32840,#32841),(#32842,#32843),(#32844,#32845),(#32846,
#32847),(#32848,#32849),(#32850,#32851),(#32852,#32853),(#32854,#32855),
(#32856,#32857),(#32858,#32859),(#32860,#32861),(#32862,#32863),(#32864,
#32865),(#32866,#32867),(#32868,#32869),(#32870,#32871),(#32872,#32873),
(#32874,#32875),(#32876,#32877),(#32878,#32879),(#32880,#32881),(#32882,
#32883),(#32884,#32885),(#32886,#32887),(#32888,#32889)),.UNSPECIFIED.,
 .F.,.F.,.F.)
B_SPLINE_SURFACE_WITH_KNOTS((6,1,1,1,1,1,1,1,1,1,1,1,1,1,1,1,1,1,1,1,1,
1,1,1,1,1,1,1,1,1,1,1,1,1,1,1,1,1,1,1,1,1,1,1,1,1,1,1,1,1,1,1,1,1,1,1,1,
1,1,1,1,1,1,1,1,6),(2,2),(-1.,-0.984615384615383,-0.969230769230768,-0.953846153846152,
-0.938461538461537,-0.923076923076922,-0.907692307692306,-0.892307692307691,
-0.876923076923076,-0.86153846153846,-0.846153846153845,-0.83076923076923,
-0.815384615384614,-0.799999999999999,-0.784615384615384,-0.769230769230768,
-0.753846153846153,-0.738461538461538,-0.723076923076922,-0.707692307692307,
-0.692307692307692,-0.676923076923076,-0.661538461538461,-0.646153846153846,
-0.63076923076923,-0.615384615384615,-0.6,-0.584615384615384,-0.569230769230769,
-0.553846153846154,-0.538461538461538,-0.523076923076923,-0.507692307692308,
-0.492307692307692,-0.476923076923077,-0.461538461538462,-0.446153846153846,
-0.430769230769231,-0.415384615384615,-0.4,-0.384615384615385,-0.369230769230769,
-0.353846153846154,-0.338461538461538,-0.323076923076923,-0.307692307692308,
-0.292307692307692,-0.276923076923077,-0.261538461538462,-0.246153846153846,
-0.230769230769231,-0.215384615384615,-0.2,-0.184615384615385,-0.169230769230769,
-0.153846153846154,-0.138461538461538,-0.123076923076923,-0.107692307692308,
-0.0923076923076923,-0.0769230769230769,-0.0615384615384615,-0.0461538461538462,
-0.0307692307692308,-0.0153846153846154,0.),(-1.,1.),.UNSPECIFIED.)
GEOMETRIC_REPRESENTATION_ITEM()
RATIONAL_B_SPLINE_SURFACE(((1.,1.),(1.,1.),(1.,1.),(1.,1.),(1.,1.),(1.,
1.),(1.,1.),(1.,1.),(1.,1.),(1.,1.),(1.,1.),(1.,1.),(1.,1.),(1.,1.),(1.,
1.),(1.,1.),(1.,1.),(1.,1.),(1.,1.),(1.,1.),(1.,1.),(1.,1.),(1.,1.),(1.,
1.),(1.,1.),(1.,1.),(1.,1.),(1.,1.),(1.,1.),(1.,1.),(1.,1.),(1.,1.),(1.,
1.),(1.,1.),(1.,1.),(1.,1.),(1.,1.),(1.,1.),(1.,1.),(1.,1.),(1.,1.),(1.,
1.),(1.,1.),(1.,1.),(1.,1.),(1.,1.),(1.,1.),(1.,1.),(1.,1.),(1.,1.),(1.,
1.),(1.,1.),(1.,1.),(1.,1.),(1.,1.),(1.,1.),(1.,1.),(1.,1.),(1.,1.),(1.,
1.),(1.,1.),(1.,1.),(1.,1.),(1.,1.),(1.,1.),(1.,1.),(1.,1.),(1.,1.),(1.,
1.),(1.,1.)))
REPRESENTATION_ITEM('')
SURFACE()
);
#31=(
BOUNDED_SURFACE()
B_SPLINE_SURFACE(5,1,((#32966,#32967),(#32968,#32969),(#32970,#32971),(#32972,
#32973),(#32974,#32975),(#32976,#32977),(#32978,#32979),(#32980,#32981),
(#32982,#32983),(#32984,#32985),(#32986,#32987),(#32988,#32989),(#32990,
#32991),(#32992,#32993),(#32994,#32995),(#32996,#32997),(#32998,#32999),
(#33000,#33001),(#33002,#33003),(#33004,#33005),(#33006,#33007),(#33008,
#33009),(#33010,#33011),(#33012,#33013),(#33014,#33015),(#33016,#33017),
(#33018,#33019),(#33020,#33021),(#33022,#33023),(#33024,#33025),(#33026,
#33027),(#33028,#33029),(#33030,#33031),(#33032,#33033),(#33034,#33035),
(#33036,#33037),(#33038,#33039),(#33040,#33041),(#33042,#33043),(#33044,
#33045),(#33046,#33047),(#33048,#33049),(#33050,#33051),(#33052,#33053),
(#33054,#33055),(#33056,#33057),(#33058,#33059),(#33060,#33061),(#33062,
#33063),(#33064,#33065),(#33066,#33067),(#33068,#33069),(#33070,#33071),
(#33072,#33073),(#33074,#33075),(#33076,#33077),(#33078,#33079),(#33080,
#33081),(#33082,#33083),(#33084,#33085),(#33086,#33087),(#33088,#33089),
(#33090,#33091),(#33092,#33093),(#33094,#33095),(#33096,#33097),(#33098,
#33099),(#33100,#33101),(#33102,#33103),(#33104,#33105)),.UNSPECIFIED.,
 .F.,.F.,.F.)
B_SPLINE_SURFACE_WITH_KNOTS((6,1,1,1,1,1,1,1,1,1,1,1,1,1,1,1,1,1,1,1,1,
1,1,1,1,1,1,1,1,1,1,1,1,1,1,1,1,1,1,1,1,1,1,1,1,1,1,1,1,1,1,1,1,1,1,1,1,
1,1,1,1,1,1,1,1,6),(2,2),(-1.,-0.984615384615383,-0.969230769230768,-0.953846153846152,
-0.938461538461537,-0.923076923076922,-0.907692307692306,-0.892307692307691,
-0.876923076923076,-0.86153846153846,-0.846153846153845,-0.83076923076923,
-0.815384615384614,-0.799999999999999,-0.784615384615384,-0.769230769230768,
-0.753846153846153,-0.738461538461538,-0.723076923076922,-0.707692307692307,
-0.692307692307692,-0.676923076923076,-0.661538461538461,-0.646153846153846,
-0.63076923076923,-0.615384615384615,-0.6,-0.584615384615384,-0.569230769230769,
-0.553846153846154,-0.538461538461538,-0.523076923076923,-0.507692307692308,
-0.492307692307692,-0.476923076923077,-0.461538461538462,-0.446153846153846,
-0.430769230769231,-0.415384615384615,-0.4,-0.384615384615385,-0.369230769230769,
-0.353846153846154,-0.338461538461538,-0.323076923076923,-0.307692307692308,
-0.292307692307692,-0.276923076923077,-0.261538461538462,-0.246153846153846,
-0.230769230769231,-0.215384615384615,-0.2,-0.184615384615385,-0.169230769230769,
-0.153846153846154,-0.138461538461538,-0.123076923076923,-0.107692307692308,
-0.0923076923076923,-0.0769230769230769,-0.0615384615384615,-0.0461538461538462,
-0.0307692307692308,-0.0153846153846154,0.),(-1.,1.),.UNSPECIFIED.)
GEOMETRIC_REPRESENTATION_ITEM()
RATIONAL_B_SPLINE_SURFACE(((1.,1.),(1.,1.),(1.,1.),(1.,1.),(1.,1.),(1.,
1.),(1.,1.),(1.,1.),(1.,1.),(1.,1.),(1.,1.),(1.,1.),(1.,1.),(1.,1.),(1.,
1.),(1.,1.),(1.,1.),(1.,1.),(1.,1.),(1.,1.),(1.,1.),(1.,1.),(1.,1.),(1.,
1.),(1.,1.),(1.,1.),(1.,1.),(1.,1.),(1.,1.),(1.,1.),(1.,1.),(1.,1.),(1.,
1.),(1.,1.),(1.,1.),(1.,1.),(1.,1.),(1.,1.),(1.,1.),(1.,1.),(1.,1.),(1.,
1.),(1.,1.),(1.,1.),(1.,1.),(1.,1.),(1.,1.),(1.,1.),(1.,1.),(1.,1.),(1.,
1.),(1.,1.),(1.,1.),(1.,1.),(1.,1.),(1.,1.),(1.,1.),(1.,1.),(1.,1.),(1.,
1.),(1.,1.),(1.,1.),(1.,1.),(1.,1.),(1.,1.),(1.,1.),(1.,1.),(1.,1.),(1.,
1.),(1.,1.)))
REPRESENTATION_ITEM('')
SURFACE()
);
#32=(
BOUNDED_SURFACE()
B_SPLINE_SURFACE(5,1,((#33182,#33183),(#33184,#33185),(#33186,#33187),(#33188,
#33189),(#33190,#33191),(#33192,#33193),(#33194,#33195),(#33196,#33197),
(#33198,#33199),(#33200,#33201),(#33202,#33203),(#33204,#33205),(#33206,
#33207),(#33208,#33209),(#33210,#33211),(#33212,#33213),(#33214,#33215),
(#33216,#33217),(#33218,#33219),(#33220,#33221),(#33222,#33223),(#33224,
#33225),(#33226,#33227),(#33228,#33229),(#33230,#33231),(#33232,#33233),
(#33234,#33235),(#33236,#33237),(#33238,#33239),(#33240,#33241),(#33242,
#33243),(#33244,#33245),(#33246,#33247),(#33248,#33249),(#33250,#33251),
(#33252,#33253),(#33254,#33255),(#33256,#33257),(#33258,#33259),(#33260,
#33261),(#33262,#33263),(#33264,#33265),(#33266,#33267),(#33268,#33269),
(#33270,#33271),(#33272,#33273),(#33274,#33275),(#33276,#33277),(#33278,
#33279),(#33280,#33281),(#33282,#33283),(#33284,#33285),(#33286,#33287),
(#33288,#33289),(#33290,#33291),(#33292,#33293),(#33294,#33295),(#33296,
#33297),(#33298,#33299),(#33300,#33301),(#33302,#33303),(#33304,#33305),
(#33306,#33307),(#33308,#33309),(#33310,#33311),(#33312,#33313),(#33314,
#33315),(#33316,#33317),(#33318,#33319),(#33320,#33321)),.UNSPECIFIED.,
 .F.,.F.,.F.)
B_SPLINE_SURFACE_WITH_KNOTS((6,1,1,1,1,1,1,1,1,1,1,1,1,1,1,1,1,1,1,1,1,
1,1,1,1,1,1,1,1,1,1,1,1,1,1,1,1,1,1,1,1,1,1,1,1,1,1,1,1,1,1,1,1,1,1,1,1,
1,1,1,1,1,1,1,1,6),(2,2),(-1.,-0.984615384615383,-0.969230769230768,-0.953846153846152,
-0.938461538461537,-0.923076923076922,-0.907692307692306,-0.892307692307691,
-0.876923076923076,-0.86153846153846,-0.846153846153845,-0.83076923076923,
-0.815384615384614,-0.799999999999999,-0.784615384615384,-0.769230769230768,
-0.753846153846153,-0.738461538461538,-0.723076923076922,-0.707692307692307,
-0.692307692307692,-0.676923076923076,-0.661538461538461,-0.646153846153846,
-0.63076923076923,-0.615384615384615,-0.6,-0.584615384615384,-0.569230769230769,
-0.553846153846154,-0.538461538461538,-0.523076923076923,-0.507692307692308,
-0.492307692307692,-0.476923076923077,-0.461538461538462,-0.446153846153846,
-0.430769230769231,-0.415384615384615,-0.4,-0.384615384615385,-0.369230769230769,
-0.353846153846154,-0.338461538461538,-0.323076923076923,-0.307692307692308,
-0.292307692307692,-0.276923076923077,-0.261538461538462,-0.246153846153846,
-0.230769230769231,-0.215384615384615,-0.2,-0.184615384615385,-0.169230769230769,
-0.153846153846154,-0.138461538461538,-0.123076923076923,-0.107692307692308,
-0.0923076923076923,-0.0769230769230769,-0.0615384615384615,-0.0461538461538462,
-0.0307692307692308,-0.0153846153846154,0.),(-1.,1.),.UNSPECIFIED.)
GEOMETRIC_REPRESENTATION_ITEM()
RATIONAL_B_SPLINE_SURFACE(((1.,1.),(1.,1.),(1.,1.),(1.,1.),(1.,1.),(1.,
1.),(1.,1.),(1.,1.),(1.,1.),(1.,1.),(1.,1.),(1.,1.),(1.,1.),(1.,1.),(1.,
1.),(1.,1.),(1.,1.),(1.,1.),(1.,1.),(1.,1.),(1.,1.),(1.,1.),(1.,1.),(1.,
1.),(1.,1.),(1.,1.),(1.,1.),(1.,1.),(1.,1.),(1.,1.),(1.,1.),(1.,1.),(1.,
1.),(1.,1.),(1.,1.),(1.,1.),(1.,1.),(1.,1.),(1.,1.),(1.,1.),(1.,1.),(1.,
1.),(1.,1.),(1.,1.),(1.,1.),(1.,1.),(1.,1.),(1.,1.),(1.,1.),(1.,1.),(1.,
1.),(1.,1.),(1.,1.),(1.,1.),(1.,1.),(1.,1.),(1.,1.),(1.,1.),(1.,1.),(1.,
1.),(1.,1.),(1.,1.),(1.,1.),(1.,1.),(1.,1.),(1.,1.),(1.,1.),(1.,1.),(1.,
1.),(1.,1.)))
REPRESENTATION_ITEM('')
SURFACE()
);
#33=(
BOUNDED_SURFACE()
B_SPLINE_SURFACE(5,1,((#33398,#33399),(#33400,#33401),(#33402,#33403),(#33404,
#33405),(#33406,#33407),(#33408,#33409),(#33410,#33411),(#33412,#33413),
(#33414,#33415),(#33416,#33417),(#33418,#33419),(#33420,#33421),(#33422,
#33423),(#33424,#33425),(#33426,#33427),(#33428,#33429),(#33430,#33431),
(#33432,#33433),(#33434,#33435),(#33436,#33437),(#33438,#33439),(#33440,
#33441),(#33442,#33443),(#33444,#33445),(#33446,#33447),(#33448,#33449),
(#33450,#33451),(#33452,#33453),(#33454,#33455),(#33456,#33457),(#33458,
#33459),(#33460,#33461),(#33462,#33463),(#33464,#33465),(#33466,#33467),
(#33468,#33469),(#33470,#33471),(#33472,#33473),(#33474,#33475),(#33476,
#33477),(#33478,#33479),(#33480,#33481),(#33482,#33483),(#33484,#33485),
(#33486,#33487),(#33488,#33489),(#33490,#33491),(#33492,#33493),(#33494,
#33495),(#33496,#33497),(#33498,#33499),(#33500,#33501),(#33502,#33503),
(#33504,#33505),(#33506,#33507),(#33508,#33509),(#33510,#33511),(#33512,
#33513),(#33514,#33515),(#33516,#33517),(#33518,#33519),(#33520,#33521),
(#33522,#33523),(#33524,#33525),(#33526,#33527),(#33528,#33529),(#33530,
#33531),(#33532,#33533),(#33534,#33535),(#33536,#33537)),.UNSPECIFIED.,
 .F.,.F.,.F.)
B_SPLINE_SURFACE_WITH_KNOTS((6,1,1,1,1,1,1,1,1,1,1,1,1,1,1,1,1,1,1,1,1,
1,1,1,1,1,1,1,1,1,1,1,1,1,1,1,1,1,1,1,1,1,1,1,1,1,1,1,1,1,1,1,1,1,1,1,1,
1,1,1,1,1,1,1,1,6),(2,2),(-1.,-0.984615384615383,-0.969230769230768,-0.953846153846152,
-0.938461538461537,-0.923076923076922,-0.907692307692306,-0.892307692307691,
-0.876923076923076,-0.86153846153846,-0.846153846153845,-0.83076923076923,
-0.815384615384614,-0.799999999999999,-0.784615384615384,-0.769230769230768,
-0.753846153846153,-0.738461538461538,-0.723076923076922,-0.707692307692307,
-0.692307692307692,-0.676923076923076,-0.661538461538461,-0.646153846153846,
-0.63076923076923,-0.615384615384615,-0.6,-0.584615384615384,-0.569230769230769,
-0.553846153846154,-0.538461538461538,-0.523076923076923,-0.507692307692308,
-0.492307692307692,-0.476923076923077,-0.461538461538462,-0.446153846153846,
-0.430769230769231,-0.415384615384615,-0.4,-0.384615384615385,-0.369230769230769,
-0.353846153846154,-0.338461538461538,-0.323076923076923,-0.307692307692308,
-0.292307692307692,-0.276923076923077,-0.261538461538462,-0.246153846153846,
-0.230769230769231,-0.215384615384615,-0.2,-0.184615384615385,-0.169230769230769,
-0.153846153846154,-0.138461538461538,-0.123076923076923,-0.107692307692308,
-0.0923076923076923,-0.0769230769230769,-0.0615384615384615,-0.0461538461538462,
-0.0307692307692308,-0.0153846153846154,0.),(-1.,1.),.UNSPECIFIED.)
GEOMETRIC_REPRESENTATION_ITEM()
RATIONAL_B_SPLINE_SURFACE(((1.,1.),(1.,1.),(1.,1.),(1.,1.),(1.,1.),(1.,
1.),(1.,1.),(1.,1.),(1.,1.),(1.,1.),(1.,1.),(1.,1.),(1.,1.),(1.,1.),(1.,
1.),(1.,1.),(1.,1.),(1.,1.),(1.,1.),(1.,1.),(1.,1.),(1.,1.),(1.,1.),(1.,
1.),(1.,1.),(1.,1.),(1.,1.),(1.,1.),(1.,1.),(1.,1.),(1.,1.),(1.,1.),(1.,
1.),(1.,1.),(1.,1.),(1.,1.),(1.,1.),(1.,1.),(1.,1.),(1.,1.),(1.,1.),(1.,
1.),(1.,1.),(1.,1.),(1.,1.),(1.,1.),(1.,1.),(1.,1.),(1.,1.),(1.,1.),(1.,
1.),(1.,1.),(1.,1.),(1.,1.),(1.,1.),(1.,1.),(1.,1.),(1.,1.),(1.,1.),(1.,
1.),(1.,1.),(1.,1.),(1.,1.),(1.,1.),(1.,1.),(1.,1.),(1.,1.),(1.,1.),(1.,
1.),(1.,1.)))
REPRESENTATION_ITEM('')
SURFACE()
);
#34=(
BOUNDED_SURFACE()
B_SPLINE_SURFACE(5,1,((#33614,#33615),(#33616,#33617),(#33618,#33619),(#33620,
#33621),(#33622,#33623),(#33624,#33625),(#33626,#33627),(#33628,#33629),
(#33630,#33631),(#33632,#33633),(#33634,#33635),(#33636,#33637),(#33638,
#33639),(#33640,#33641),(#33642,#33643),(#33644,#33645),(#33646,#33647),
(#33648,#33649),(#33650,#33651),(#33652,#33653),(#33654,#33655),(#33656,
#33657),(#33658,#33659),(#33660,#33661),(#33662,#33663),(#33664,#33665),
(#33666,#33667),(#33668,#33669),(#33670,#33671),(#33672,#33673),(#33674,
#33675),(#33676,#33677),(#33678,#33679),(#33680,#33681),(#33682,#33683),
(#33684,#33685),(#33686,#33687),(#33688,#33689),(#33690,#33691),(#33692,
#33693),(#33694,#33695),(#33696,#33697),(#33698,#33699),(#33700,#33701),
(#33702,#33703),(#33704,#33705),(#33706,#33707),(#33708,#33709),(#33710,
#33711),(#33712,#33713),(#33714,#33715),(#33716,#33717),(#33718,#33719),
(#33720,#33721),(#33722,#33723),(#33724,#33725),(#33726,#33727),(#33728,
#33729),(#33730,#33731),(#33732,#33733),(#33734,#33735),(#33736,#33737),
(#33738,#33739),(#33740,#33741),(#33742,#33743),(#33744,#33745),(#33746,
#33747),(#33748,#33749),(#33750,#33751),(#33752,#33753)),.UNSPECIFIED.,
 .F.,.F.,.F.)
B_SPLINE_SURFACE_WITH_KNOTS((6,1,1,1,1,1,1,1,1,1,1,1,1,1,1,1,1,1,1,1,1,
1,1,1,1,1,1,1,1,1,1,1,1,1,1,1,1,1,1,1,1,1,1,1,1,1,1,1,1,1,1,1,1,1,1,1,1,
1,1,1,1,1,1,1,1,6),(2,2),(-1.,-0.984615384615383,-0.969230769230768,-0.953846153846152,
-0.938461538461537,-0.923076923076922,-0.907692307692306,-0.892307692307691,
-0.876923076923076,-0.86153846153846,-0.846153846153845,-0.83076923076923,
-0.815384615384614,-0.799999999999999,-0.784615384615384,-0.769230769230768,
-0.753846153846153,-0.738461538461538,-0.723076923076922,-0.707692307692307,
-0.692307692307692,-0.676923076923076,-0.661538461538461,-0.646153846153846,
-0.63076923076923,-0.615384615384615,-0.6,-0.584615384615384,-0.569230769230769,
-0.553846153846154,-0.538461538461538,-0.523076923076923,-0.507692307692308,
-0.492307692307692,-0.476923076923077,-0.461538461538462,-0.446153846153846,
-0.430769230769231,-0.415384615384615,-0.4,-0.384615384615385,-0.369230769230769,
-0.353846153846154,-0.338461538461538,-0.323076923076923,-0.307692307692308,
-0.292307692307692,-0.276923076923077,-0.261538461538462,-0.246153846153846,
-0.230769230769231,-0.215384615384615,-0.2,-0.184615384615385,-0.169230769230769,
-0.153846153846154,-0.138461538461538,-0.123076923076923,-0.107692307692308,
-0.0923076923076923,-0.0769230769230769,-0.0615384615384615,-0.0461538461538462,
-0.0307692307692308,-0.0153846153846154,0.),(-1.,1.),.UNSPECIFIED.)
GEOMETRIC_REPRESENTATION_ITEM()
RATIONAL_B_SPLINE_SURFACE(((1.,1.),(1.,1.),(1.,1.),(1.,1.),(1.,1.),(1.,
1.),(1.,1.),(1.,1.),(1.,1.),(1.,1.),(1.,1.),(1.,1.),(1.,1.),(1.,1.),(1.,
1.),(1.,1.),(1.,1.),(1.,1.),(1.,1.),(1.,1.),(1.,1.),(1.,1.),(1.,1.),(1.,
1.),(1.,1.),(1.,1.),(1.,1.),(1.,1.),(1.,1.),(1.,1.),(1.,1.),(1.,1.),(1.,
1.),(1.,1.),(1.,1.),(1.,1.),(1.,1.),(1.,1.),(1.,1.),(1.,1.),(1.,1.),(1.,
1.),(1.,1.),(1.,1.),(1.,1.),(1.,1.),(1.,1.),(1.,1.),(1.,1.),(1.,1.),(1.,
1.),(1.,1.),(1.,1.),(1.,1.),(1.,1.),(1.,1.),(1.,1.),(1.,1.),(1.,1.),(1.,
1.),(1.,1.),(1.,1.),(1.,1.),(1.,1.),(1.,1.),(1.,1.),(1.,1.),(1.,1.),(1.,
1.),(1.,1.)))
REPRESENTATION_ITEM('')
SURFACE()
);
#35=(
BOUNDED_SURFACE()
B_SPLINE_SURFACE(5,1,((#33830,#33831),(#33832,#33833),(#33834,#33835),(#33836,
#33837),(#33838,#33839),(#33840,#33841),(#33842,#33843),(#33844,#33845),
(#33846,#33847),(#33848,#33849),(#33850,#33851),(#33852,#33853),(#33854,
#33855),(#33856,#33857),(#33858,#33859),(#33860,#33861),(#33862,#33863),
(#33864,#33865),(#33866,#33867),(#33868,#33869),(#33870,#33871),(#33872,
#33873),(#33874,#33875),(#33876,#33877),(#33878,#33879),(#33880,#33881),
(#33882,#33883),(#33884,#33885),(#33886,#33887),(#33888,#33889),(#33890,
#33891),(#33892,#33893),(#33894,#33895),(#33896,#33897),(#33898,#33899),
(#33900,#33901),(#33902,#33903),(#33904,#33905),(#33906,#33907),(#33908,
#33909),(#33910,#33911),(#33912,#33913),(#33914,#33915),(#33916,#33917),
(#33918,#33919),(#33920,#33921),(#33922,#33923),(#33924,#33925),(#33926,
#33927),(#33928,#33929),(#33930,#33931),(#33932,#33933),(#33934,#33935),
(#33936,#33937),(#33938,#33939),(#33940,#33941),(#33942,#33943),(#33944,
#33945),(#33946,#33947),(#33948,#33949),(#33950,#33951),(#33952,#33953),
(#33954,#33955),(#33956,#33957),(#33958,#33959),(#33960,#33961),(#33962,
#33963),(#33964,#33965),(#33966,#33967),(#33968,#33969)),.UNSPECIFIED.,
 .F.,.F.,.F.)
B_SPLINE_SURFACE_WITH_KNOTS((6,1,1,1,1,1,1,1,1,1,1,1,1,1,1,1,1,1,1,1,1,
1,1,1,1,1,1,1,1,1,1,1,1,1,1,1,1,1,1,1,1,1,1,1,1,1,1,1,1,1,1,1,1,1,1,1,1,
1,1,1,1,1,1,1,1,6),(2,2),(-1.,-0.984615384615383,-0.969230769230768,-0.953846153846152,
-0.938461538461537,-0.923076923076922,-0.907692307692306,-0.892307692307691,
-0.876923076923076,-0.86153846153846,-0.846153846153845,-0.83076923076923,
-0.815384615384614,-0.799999999999999,-0.784615384615384,-0.769230769230768,
-0.753846153846153,-0.738461538461538,-0.723076923076922,-0.707692307692307,
-0.692307692307692,-0.676923076923076,-0.661538461538461,-0.646153846153846,
-0.63076923076923,-0.615384615384615,-0.6,-0.584615384615384,-0.569230769230769,
-0.553846153846154,-0.538461538461538,-0.523076923076923,-0.507692307692308,
-0.492307692307692,-0.476923076923077,-0.461538461538462,-0.446153846153846,
-0.430769230769231,-0.415384615384615,-0.4,-0.384615384615385,-0.369230769230769,
-0.353846153846154,-0.338461538461538,-0.323076923076923,-0.307692307692308,
-0.292307692307692,-0.276923076923077,-0.261538461538462,-0.246153846153846,
-0.230769230769231,-0.215384615384615,-0.2,-0.184615384615385,-0.169230769230769,
-0.153846153846154,-0.138461538461538,-0.123076923076923,-0.107692307692308,
-0.0923076923076923,-0.0769230769230769,-0.0615384615384615,-0.0461538461538462,
-0.0307692307692308,-0.0153846153846154,0.),(-1.,1.),.UNSPECIFIED.)
GEOMETRIC_REPRESENTATION_ITEM()
RATIONAL_B_SPLINE_SURFACE(((1.,1.),(1.,1.),(1.,1.),(1.,1.),(1.,1.),(1.,
1.),(1.,1.),(1.,1.),(1.,1.),(1.,1.),(1.,1.),(1.,1.),(1.,1.),(1.,1.),(1.,
1.),(1.,1.),(1.,1.),(1.,1.),(1.,1.),(1.,1.),(1.,1.),(1.,1.),(1.,1.),(1.,
1.),(1.,1.),(1.,1.),(1.,1.),(1.,1.),(1.,1.),(1.,1.),(1.,1.),(1.,1.),(1.,
1.),(1.,1.),(1.,1.),(1.,1.),(1.,1.),(1.,1.),(1.,1.),(1.,1.),(1.,1.),(1.,
1.),(1.,1.),(1.,1.),(1.,1.),(1.,1.),(1.,1.),(1.,1.),(1.,1.),(1.,1.),(1.,
1.),(1.,1.),(1.,1.),(1.,1.),(1.,1.),(1.,1.),(1.,1.),(1.,1.),(1.,1.),(1.,
1.),(1.,1.),(1.,1.),(1.,1.),(1.,1.),(1.,1.),(1.,1.),(1.,1.),(1.,1.),(1.,
1.),(1.,1.)))
REPRESENTATION_ITEM('')
SURFACE()
);
#36=(
BOUNDED_SURFACE()
B_SPLINE_SURFACE(5,1,((#34046,#34047),(#34048,#34049),(#34050,#34051),(#34052,
#34053),(#34054,#34055),(#34056,#34057),(#34058,#34059),(#34060,#34061),
(#34062,#34063),(#34064,#34065),(#34066,#34067),(#34068,#34069),(#34070,
#34071),(#34072,#34073),(#34074,#34075),(#34076,#34077),(#34078,#34079),
(#34080,#34081),(#34082,#34083),(#34084,#34085),(#34086,#34087),(#34088,
#34089),(#34090,#34091),(#34092,#34093),(#34094,#34095),(#34096,#34097),
(#34098,#34099),(#34100,#34101),(#34102,#34103),(#34104,#34105),(#34106,
#34107),(#34108,#34109),(#34110,#34111),(#34112,#34113),(#34114,#34115),
(#34116,#34117),(#34118,#34119),(#34120,#34121),(#34122,#34123),(#34124,
#34125),(#34126,#34127),(#34128,#34129),(#34130,#34131),(#34132,#34133),
(#34134,#34135),(#34136,#34137),(#34138,#34139),(#34140,#34141),(#34142,
#34143),(#34144,#34145),(#34146,#34147),(#34148,#34149),(#34150,#34151),
(#34152,#34153),(#34154,#34155),(#34156,#34157),(#34158,#34159),(#34160,
#34161),(#34162,#34163),(#34164,#34165),(#34166,#34167),(#34168,#34169),
(#34170,#34171),(#34172,#34173),(#34174,#34175),(#34176,#34177),(#34178,
#34179),(#34180,#34181),(#34182,#34183),(#34184,#34185)),.UNSPECIFIED.,
 .F.,.F.,.F.)
B_SPLINE_SURFACE_WITH_KNOTS((6,1,1,1,1,1,1,1,1,1,1,1,1,1,1,1,1,1,1,1,1,
1,1,1,1,1,1,1,1,1,1,1,1,1,1,1,1,1,1,1,1,1,1,1,1,1,1,1,1,1,1,1,1,1,1,1,1,
1,1,1,1,1,1,1,1,6),(2,2),(-1.,-0.984615384615383,-0.969230769230768,-0.953846153846152,
-0.938461538461537,-0.923076923076922,-0.907692307692306,-0.892307692307691,
-0.876923076923076,-0.86153846153846,-0.846153846153845,-0.83076923076923,
-0.815384615384614,-0.799999999999999,-0.784615384615384,-0.769230769230768,
-0.753846153846153,-0.738461538461538,-0.723076923076922,-0.707692307692307,
-0.692307692307692,-0.676923076923076,-0.661538461538461,-0.646153846153846,
-0.63076923076923,-0.615384615384615,-0.6,-0.584615384615384,-0.569230769230769,
-0.553846153846154,-0.538461538461538,-0.523076923076923,-0.507692307692308,
-0.492307692307692,-0.476923076923077,-0.461538461538462,-0.446153846153846,
-0.430769230769231,-0.415384615384615,-0.4,-0.384615384615385,-0.369230769230769,
-0.353846153846154,-0.338461538461538,-0.323076923076923,-0.307692307692308,
-0.292307692307692,-0.276923076923077,-0.261538461538462,-0.246153846153846,
-0.230769230769231,-0.215384615384615,-0.2,-0.184615384615385,-0.169230769230769,
-0.153846153846154,-0.138461538461538,-0.123076923076923,-0.107692307692308,
-0.0923076923076923,-0.0769230769230769,-0.0615384615384615,-0.0461538461538462,
-0.0307692307692308,-0.0153846153846154,0.),(-1.,1.),.UNSPECIFIED.)
GEOMETRIC_REPRESENTATION_ITEM()
RATIONAL_B_SPLINE_SURFACE(((1.,1.),(1.,1.),(1.,1.),(1.,1.),(1.,1.),(1.,
1.),(1.,1.),(1.,1.),(1.,1.),(1.,1.),(1.,1.),(1.,1.),(1.,1.),(1.,1.),(1.,
1.),(1.,1.),(1.,1.),(1.,1.),(1.,1.),(1.,1.),(1.,1.),(1.,1.),(1.,1.),(1.,
1.),(1.,1.),(1.,1.),(1.,1.),(1.,1.),(1.,1.),(1.,1.),(1.,1.),(1.,1.),(1.,
1.),(1.,1.),(1.,1.),(1.,1.),(1.,1.),(1.,1.),(1.,1.),(1.,1.),(1.,1.),(1.,
1.),(1.,1.),(1.,1.),(1.,1.),(1.,1.),(1.,1.),(1.,1.),(1.,1.),(1.,1.),(1.,
1.),(1.,1.),(1.,1.),(1.,1.),(1.,1.),(1.,1.),(1.,1.),(1.,1.),(1.,1.),(1.,
1.),(1.,1.),(1.,1.),(1.,1.),(1.,1.),(1.,1.),(1.,1.),(1.,1.),(1.,1.),(1.,
1.),(1.,1.)))
REPRESENTATION_ITEM('')
SURFACE()
);
#37=(
BOUNDED_SURFACE()
B_SPLINE_SURFACE(5,1,((#34262,#34263),(#34264,#34265),(#34266,#34267),(#34268,
#34269),(#34270,#34271),(#34272,#34273),(#34274,#34275),(#34276,#34277),
(#34278,#34279),(#34280,#34281),(#34282,#34283),(#34284,#34285),(#34286,
#34287),(#34288,#34289),(#34290,#34291),(#34292,#34293),(#34294,#34295),
(#34296,#34297),(#34298,#34299),(#34300,#34301),(#34302,#34303),(#34304,
#34305),(#34306,#34307),(#34308,#34309),(#34310,#34311),(#34312,#34313),
(#34314,#34315),(#34316,#34317),(#34318,#34319),(#34320,#34321),(#34322,
#34323),(#34324,#34325),(#34326,#34327),(#34328,#34329),(#34330,#34331),
(#34332,#34333),(#34334,#34335),(#34336,#34337),(#34338,#34339),(#34340,
#34341),(#34342,#34343),(#34344,#34345),(#34346,#34347),(#34348,#34349),
(#34350,#34351),(#34352,#34353),(#34354,#34355),(#34356,#34357),(#34358,
#34359),(#34360,#34361),(#34362,#34363),(#34364,#34365),(#34366,#34367),
(#34368,#34369),(#34370,#34371),(#34372,#34373),(#34374,#34375),(#34376,
#34377),(#34378,#34379),(#34380,#34381),(#34382,#34383),(#34384,#34385),
(#34386,#34387),(#34388,#34389),(#34390,#34391),(#34392,#34393),(#34394,
#34395),(#34396,#34397),(#34398,#34399),(#34400,#34401)),.UNSPECIFIED.,
 .F.,.F.,.F.)
B_SPLINE_SURFACE_WITH_KNOTS((6,1,1,1,1,1,1,1,1,1,1,1,1,1,1,1,1,1,1,1,1,
1,1,1,1,1,1,1,1,1,1,1,1,1,1,1,1,1,1,1,1,1,1,1,1,1,1,1,1,1,1,1,1,1,1,1,1,
1,1,1,1,1,1,1,1,6),(2,2),(-1.,-0.984615384615383,-0.969230769230768,-0.953846153846152,
-0.938461538461537,-0.923076923076922,-0.907692307692306,-0.892307692307691,
-0.876923076923076,-0.86153846153846,-0.846153846153845,-0.83076923076923,
-0.815384615384614,-0.799999999999999,-0.784615384615384,-0.769230769230768,
-0.753846153846153,-0.738461538461538,-0.723076923076922,-0.707692307692307,
-0.692307692307692,-0.676923076923076,-0.661538461538461,-0.646153846153846,
-0.63076923076923,-0.615384615384615,-0.6,-0.584615384615384,-0.569230769230769,
-0.553846153846154,-0.538461538461538,-0.523076923076923,-0.507692307692308,
-0.492307692307692,-0.476923076923077,-0.461538461538462,-0.446153846153846,
-0.430769230769231,-0.415384615384615,-0.4,-0.384615384615385,-0.369230769230769,
-0.353846153846154,-0.338461538461538,-0.323076923076923,-0.307692307692308,
-0.292307692307692,-0.276923076923077,-0.261538461538462,-0.246153846153846,
-0.230769230769231,-0.215384615384615,-0.2,-0.184615384615385,-0.169230769230769,
-0.153846153846154,-0.138461538461538,-0.123076923076923,-0.107692307692308,
-0.0923076923076923,-0.0769230769230769,-0.0615384615384615,-0.0461538461538462,
-0.0307692307692308,-0.0153846153846154,0.),(-1.,1.),.UNSPECIFIED.)
GEOMETRIC_REPRESENTATION_ITEM()
RATIONAL_B_SPLINE_SURFACE(((1.,1.),(1.,1.),(1.,1.),(1.,1.),(1.,1.),(1.,
1.),(1.,1.),(1.,1.),(1.,1.),(1.,1.),(1.,1.),(1.,1.),(1.,1.),(1.,1.),(1.,
1.),(1.,1.),(1.,1.),(1.,1.),(1.,1.),(1.,1.),(1.,1.),(1.,1.),(1.,1.),(1.,
1.),(1.,1.),(1.,1.),(1.,1.),(1.,1.),(1.,1.),(1.,1.),(1.,1.),(1.,1.),(1.,
1.),(1.,1.),(1.,1.),(1.,1.),(1.,1.),(1.,1.),(1.,1.),(1.,1.),(1.,1.),(1.,
1.),(1.,1.),(1.,1.),(1.,1.),(1.,1.),(1.,1.),(1.,1.),(1.,1.),(1.,1.),(1.,
1.),(1.,1.),(1.,1.),(1.,1.),(1.,1.),(1.,1.),(1.,1.),(1.,1.),(1.,1.),(1.,
1.),(1.,1.),(1.,1.),(1.,1.),(1.,1.),(1.,1.),(1.,1.),(1.,1.),(1.,1.),(1.,
1.),(1.,1.)))
REPRESENTATION_ITEM('')
SURFACE()
);
#38=(
BOUNDED_SURFACE()
B_SPLINE_SURFACE(5,1,((#34478,#34479),(#34480,#34481),(#34482,#34483),(#34484,
#34485),(#34486,#34487),(#34488,#34489),(#34490,#34491),(#34492,#34493),
(#34494,#34495),(#34496,#34497),(#34498,#34499),(#34500,#34501),(#34502,
#34503),(#34504,#34505),(#34506,#34507),(#34508,#34509),(#34510,#34511),
(#34512,#34513),(#34514,#34515),(#34516,#34517),(#34518,#34519),(#34520,
#34521),(#34522,#34523),(#34524,#34525),(#34526,#34527),(#34528,#34529),
(#34530,#34531),(#34532,#34533),(#34534,#34535),(#34536,#34537),(#34538,
#34539),(#34540,#34541),(#34542,#34543),(#34544,#34545),(#34546,#34547),
(#34548,#34549),(#34550,#34551),(#34552,#34553),(#34554,#34555),(#34556,
#34557),(#34558,#34559),(#34560,#34561),(#34562,#34563),(#34564,#34565),
(#34566,#34567),(#34568,#34569),(#34570,#34571),(#34572,#34573),(#34574,
#34575),(#34576,#34577),(#34578,#34579),(#34580,#34581),(#34582,#34583),
(#34584,#34585),(#34586,#34587),(#34588,#34589),(#34590,#34591),(#34592,
#34593),(#34594,#34595),(#34596,#34597),(#34598,#34599),(#34600,#34601),
(#34602,#34603),(#34604,#34605),(#34606,#34607),(#34608,#34609),(#34610,
#34611),(#34612,#34613),(#34614,#34615),(#34616,#34617)),.UNSPECIFIED.,
 .F.,.F.,.F.)
B_SPLINE_SURFACE_WITH_KNOTS((6,1,1,1,1,1,1,1,1,1,1,1,1,1,1,1,1,1,1,1,1,
1,1,1,1,1,1,1,1,1,1,1,1,1,1,1,1,1,1,1,1,1,1,1,1,1,1,1,1,1,1,1,1,1,1,1,1,
1,1,1,1,1,1,1,1,6),(2,2),(-1.,-0.984615384615383,-0.969230769230768,-0.953846153846152,
-0.938461538461537,-0.923076923076922,-0.907692307692306,-0.892307692307691,
-0.876923076923076,-0.86153846153846,-0.846153846153845,-0.83076923076923,
-0.815384615384614,-0.799999999999999,-0.784615384615384,-0.769230769230768,
-0.753846153846153,-0.738461538461538,-0.723076923076922,-0.707692307692307,
-0.692307692307692,-0.676923076923076,-0.661538461538461,-0.646153846153846,
-0.63076923076923,-0.615384615384615,-0.6,-0.584615384615384,-0.569230769230769,
-0.553846153846154,-0.538461538461538,-0.523076923076923,-0.507692307692308,
-0.492307692307692,-0.476923076923077,-0.461538461538462,-0.446153846153846,
-0.430769230769231,-0.415384615384615,-0.4,-0.384615384615385,-0.369230769230769,
-0.353846153846154,-0.338461538461538,-0.323076923076923,-0.307692307692308,
-0.292307692307692,-0.276923076923077,-0.261538461538462,-0.246153846153846,
-0.230769230769231,-0.215384615384615,-0.2,-0.184615384615385,-0.169230769230769,
-0.153846153846154,-0.138461538461538,-0.123076923076923,-0.107692307692308,
-0.0923076923076923,-0.0769230769230769,-0.0615384615384615,-0.0461538461538462,
-0.0307692307692308,-0.0153846153846154,0.),(-1.,1.),.UNSPECIFIED.)
GEOMETRIC_REPRESENTATION_ITEM()
RATIONAL_B_SPLINE_SURFACE(((1.,1.),(1.,1.),(1.,1.),(1.,1.),(1.,1.),(1.,
1.),(1.,1.),(1.,1.),(1.,1.),(1.,1.),(1.,1.),(1.,1.),(1.,1.),(1.,1.),(1.,
1.),(1.,1.),(1.,1.),(1.,1.),(1.,1.),(1.,1.),(1.,1.),(1.,1.),(1.,1.),(1.,
1.),(1.,1.),(1.,1.),(1.,1.),(1.,1.),(1.,1.),(1.,1.),(1.,1.),(1.,1.),(1.,
1.),(1.,1.),(1.,1.),(1.,1.),(1.,1.),(1.,1.),(1.,1.),(1.,1.),(1.,1.),(1.,
1.),(1.,1.),(1.,1.),(1.,1.),(1.,1.),(1.,1.),(1.,1.),(1.,1.),(1.,1.),(1.,
1.),(1.,1.),(1.,1.),(1.,1.),(1.,1.),(1.,1.),(1.,1.),(1.,1.),(1.,1.),(1.,
1.),(1.,1.),(1.,1.),(1.,1.),(1.,1.),(1.,1.),(1.,1.),(1.,1.),(1.,1.),(1.,
1.),(1.,1.)))
REPRESENTATION_ITEM('')
SURFACE()
);
#39=(
BOUNDED_SURFACE()
B_SPLINE_SURFACE(5,1,((#34694,#34695),(#34696,#34697),(#34698,#34699),(#34700,
#34701),(#34702,#34703),(#34704,#34705),(#34706,#34707),(#34708,#34709),
(#34710,#34711),(#34712,#34713),(#34714,#34715),(#34716,#34717),(#34718,
#34719),(#34720,#34721),(#34722,#34723),(#34724,#34725),(#34726,#34727),
(#34728,#34729),(#34730,#34731),(#34732,#34733),(#34734,#34735),(#34736,
#34737),(#34738,#34739),(#34740,#34741),(#34742,#34743),(#34744,#34745),
(#34746,#34747),(#34748,#34749),(#34750,#34751),(#34752,#34753),(#34754,
#34755),(#34756,#34757),(#34758,#34759),(#34760,#34761),(#34762,#34763),
(#34764,#34765),(#34766,#34767),(#34768,#34769),(#34770,#34771),(#34772,
#34773),(#34774,#34775),(#34776,#34777),(#34778,#34779),(#34780,#34781),
(#34782,#34783),(#34784,#34785),(#34786,#34787),(#34788,#34789),(#34790,
#34791),(#34792,#34793),(#34794,#34795),(#34796,#34797),(#34798,#34799),
(#34800,#34801),(#34802,#34803),(#34804,#34805),(#34806,#34807),(#34808,
#34809),(#34810,#34811),(#34812,#34813),(#34814,#34815),(#34816,#34817),
(#34818,#34819),(#34820,#34821),(#34822,#34823),(#34824,#34825),(#34826,
#34827),(#34828,#34829),(#34830,#34831),(#34832,#34833)),.UNSPECIFIED.,
 .F.,.F.,.F.)
B_SPLINE_SURFACE_WITH_KNOTS((6,1,1,1,1,1,1,1,1,1,1,1,1,1,1,1,1,1,1,1,1,
1,1,1,1,1,1,1,1,1,1,1,1,1,1,1,1,1,1,1,1,1,1,1,1,1,1,1,1,1,1,1,1,1,1,1,1,
1,1,1,1,1,1,1,1,6),(2,2),(-1.,-0.984615384615383,-0.969230769230768,-0.953846153846152,
-0.938461538461537,-0.923076923076922,-0.907692307692306,-0.892307692307691,
-0.876923076923076,-0.86153846153846,-0.846153846153845,-0.83076923076923,
-0.815384615384614,-0.799999999999999,-0.784615384615384,-0.769230769230768,
-0.753846153846153,-0.738461538461538,-0.723076923076922,-0.707692307692307,
-0.692307692307692,-0.676923076923076,-0.661538461538461,-0.646153846153846,
-0.63076923076923,-0.615384615384615,-0.6,-0.584615384615384,-0.569230769230769,
-0.553846153846154,-0.538461538461538,-0.523076923076923,-0.507692307692308,
-0.492307692307692,-0.476923076923077,-0.461538461538462,-0.446153846153846,
-0.430769230769231,-0.415384615384615,-0.4,-0.384615384615385,-0.369230769230769,
-0.353846153846154,-0.338461538461538,-0.323076923076923,-0.307692307692308,
-0.292307692307692,-0.276923076923077,-0.261538461538462,-0.246153846153846,
-0.230769230769231,-0.215384615384615,-0.2,-0.184615384615385,-0.169230769230769,
-0.153846153846154,-0.138461538461538,-0.123076923076923,-0.107692307692308,
-0.0923076923076923,-0.0769230769230769,-0.0615384615384615,-0.0461538461538462,
-0.0307692307692308,-0.0153846153846154,0.),(-1.,1.),.UNSPECIFIED.)
GEOMETRIC_REPRESENTATION_ITEM()
RATIONAL_B_SPLINE_SURFACE(((1.,1.),(1.,1.),(1.,1.),(1.,1.),(1.,1.),(1.,
1.),(1.,1.),(1.,1.),(1.,1.),(1.,1.),(1.,1.),(1.,1.),(1.,1.),(1.,1.),(1.,
1.),(1.,1.),(1.,1.),(1.,1.),(1.,1.),(1.,1.),(1.,1.),(1.,1.),(1.,1.),(1.,
1.),(1.,1.),(1.,1.),(1.,1.),(1.,1.),(1.,1.),(1.,1.),(1.,1.),(1.,1.),(1.,
1.),(1.,1.),(1.,1.),(1.,1.),(1.,1.),(1.,1.),(1.,1.),(1.,1.),(1.,1.),(1.,
1.),(1.,1.),(1.,1.),(1.,1.),(1.,1.),(1.,1.),(1.,1.),(1.,1.),(1.,1.),(1.,
1.),(1.,1.),(1.,1.),(1.,1.),(1.,1.),(1.,1.),(1.,1.),(1.,1.),(1.,1.),(1.,
1.),(1.,1.),(1.,1.),(1.,1.),(1.,1.),(1.,1.),(1.,1.),(1.,1.),(1.,1.),(1.,
1.),(1.,1.)))
REPRESENTATION_ITEM('')
SURFACE()
);
#40=(
BOUNDED_SURFACE()
B_SPLINE_SURFACE(5,1,((#34910,#34911),(#34912,#34913),(#34914,#34915),(#34916,
#34917),(#34918,#34919),(#34920,#34921),(#34922,#34923),(#34924,#34925),
(#34926,#34927),(#34928,#34929),(#34930,#34931),(#34932,#34933),(#34934,
#34935),(#34936,#34937),(#34938,#34939),(#34940,#34941),(#34942,#34943),
(#34944,#34945),(#34946,#34947),(#34948,#34949),(#34950,#34951),(#34952,
#34953),(#34954,#34955),(#34956,#34957),(#34958,#34959),(#34960,#34961),
(#34962,#34963),(#34964,#34965),(#34966,#34967),(#34968,#34969),(#34970,
#34971),(#34972,#34973),(#34974,#34975),(#34976,#34977),(#34978,#34979),
(#34980,#34981),(#34982,#34983),(#34984,#34985),(#34986,#34987),(#34988,
#34989),(#34990,#34991),(#34992,#34993),(#34994,#34995),(#34996,#34997),
(#34998,#34999),(#35000,#35001),(#35002,#35003),(#35004,#35005),(#35006,
#35007),(#35008,#35009),(#35010,#35011),(#35012,#35013),(#35014,#35015),
(#35016,#35017),(#35018,#35019),(#35020,#35021),(#35022,#35023),(#35024,
#35025),(#35026,#35027),(#35028,#35029),(#35030,#35031),(#35032,#35033),
(#35034,#35035),(#35036,#35037),(#35038,#35039),(#35040,#35041),(#35042,
#35043),(#35044,#35045),(#35046,#35047),(#35048,#35049)),.UNSPECIFIED.,
 .F.,.F.,.F.)
B_SPLINE_SURFACE_WITH_KNOTS((6,1,1,1,1,1,1,1,1,1,1,1,1,1,1,1,1,1,1,1,1,
1,1,1,1,1,1,1,1,1,1,1,1,1,1,1,1,1,1,1,1,1,1,1,1,1,1,1,1,1,1,1,1,1,1,1,1,
1,1,1,1,1,1,1,1,6),(2,2),(-1.,-0.984615384615383,-0.969230769230768,-0.953846153846152,
-0.938461538461537,-0.923076923076922,-0.907692307692306,-0.892307692307691,
-0.876923076923076,-0.86153846153846,-0.846153846153845,-0.83076923076923,
-0.815384615384614,-0.799999999999999,-0.784615384615384,-0.769230769230768,
-0.753846153846153,-0.738461538461538,-0.723076923076922,-0.707692307692307,
-0.692307692307692,-0.676923076923076,-0.661538461538461,-0.646153846153846,
-0.63076923076923,-0.615384615384615,-0.6,-0.584615384615384,-0.569230769230769,
-0.553846153846154,-0.538461538461538,-0.523076923076923,-0.507692307692308,
-0.492307692307692,-0.476923076923077,-0.461538461538462,-0.446153846153846,
-0.430769230769231,-0.415384615384615,-0.4,-0.384615384615385,-0.369230769230769,
-0.353846153846154,-0.338461538461538,-0.323076923076923,-0.307692307692308,
-0.292307692307692,-0.276923076923077,-0.261538461538462,-0.246153846153846,
-0.230769230769231,-0.215384615384615,-0.2,-0.184615384615385,-0.169230769230769,
-0.153846153846154,-0.138461538461538,-0.123076923076923,-0.107692307692308,
-0.0923076923076923,-0.0769230769230769,-0.0615384615384615,-0.0461538461538462,
-0.0307692307692308,-0.0153846153846154,0.),(-1.,1.),.UNSPECIFIED.)
GEOMETRIC_REPRESENTATION_ITEM()
RATIONAL_B_SPLINE_SURFACE(((1.,1.),(1.,1.),(1.,1.),(1.,1.),(1.,1.),(1.,
1.),(1.,1.),(1.,1.),(1.,1.),(1.,1.),(1.,1.),(1.,1.),(1.,1.),(1.,1.),(1.,
1.),(1.,1.),(1.,1.),(1.,1.),(1.,1.),(1.,1.),(1.,1.),(1.,1.),(1.,1.),(1.,
1.),(1.,1.),(1.,1.),(1.,1.),(1.,1.),(1.,1.),(1.,1.),(1.,1.),(1.,1.),(1.,
1.),(1.,1.),(1.,1.),(1.,1.),(1.,1.),(1.,1.),(1.,1.),(1.,1.),(1.,1.),(1.,
1.),(1.,1.),(1.,1.),(1.,1.),(1.,1.),(1.,1.),(1.,1.),(1.,1.),(1.,1.),(1.,
1.),(1.,1.),(1.,1.),(1.,1.),(1.,1.),(1.,1.),(1.,1.),(1.,1.),(1.,1.),(1.,
1.),(1.,1.),(1.,1.),(1.,1.),(1.,1.),(1.,1.),(1.,1.),(1.,1.),(1.,1.),(1.,
1.),(1.,1.)))
REPRESENTATION_ITEM('')
SURFACE()
);
#41=(
BOUNDED_SURFACE()
B_SPLINE_SURFACE(5,1,((#35126,#35127),(#35128,#35129),(#35130,#35131),(#35132,
#35133),(#35134,#35135),(#35136,#35137),(#35138,#35139),(#35140,#35141),
(#35142,#35143),(#35144,#35145),(#35146,#35147),(#35148,#35149),(#35150,
#35151),(#35152,#35153),(#35154,#35155),(#35156,#35157),(#35158,#35159),
(#35160,#35161),(#35162,#35163),(#35164,#35165),(#35166,#35167),(#35168,
#35169),(#35170,#35171),(#35172,#35173),(#35174,#35175),(#35176,#35177),
(#35178,#35179),(#35180,#35181),(#35182,#35183),(#35184,#35185),(#35186,
#35187),(#35188,#35189),(#35190,#35191),(#35192,#35193),(#35194,#35195),
(#35196,#35197),(#35198,#35199),(#35200,#35201),(#35202,#35203),(#35204,
#35205),(#35206,#35207),(#35208,#35209),(#35210,#35211),(#35212,#35213),
(#35214,#35215),(#35216,#35217),(#35218,#35219),(#35220,#35221),(#35222,
#35223),(#35224,#35225),(#35226,#35227),(#35228,#35229),(#35230,#35231),
(#35232,#35233),(#35234,#35235),(#35236,#35237),(#35238,#35239),(#35240,
#35241),(#35242,#35243),(#35244,#35245),(#35246,#35247),(#35248,#35249),
(#35250,#35251),(#35252,#35253),(#35254,#35255),(#35256,#35257),(#35258,
#35259),(#35260,#35261),(#35262,#35263),(#35264,#35265)),.UNSPECIFIED.,
 .F.,.F.,.F.)
B_SPLINE_SURFACE_WITH_KNOTS((6,1,1,1,1,1,1,1,1,1,1,1,1,1,1,1,1,1,1,1,1,
1,1,1,1,1,1,1,1,1,1,1,1,1,1,1,1,1,1,1,1,1,1,1,1,1,1,1,1,1,1,1,1,1,1,1,1,
1,1,1,1,1,1,1,1,6),(2,2),(-1.,-0.984615384615383,-0.969230769230768,-0.953846153846152,
-0.938461538461537,-0.923076923076922,-0.907692307692306,-0.892307692307691,
-0.876923076923076,-0.86153846153846,-0.846153846153845,-0.83076923076923,
-0.815384615384614,-0.799999999999999,-0.784615384615384,-0.769230769230768,
-0.753846153846153,-0.738461538461538,-0.723076923076922,-0.707692307692307,
-0.692307692307692,-0.676923076923076,-0.661538461538461,-0.646153846153846,
-0.63076923076923,-0.615384615384615,-0.6,-0.584615384615384,-0.569230769230769,
-0.553846153846154,-0.538461538461538,-0.523076923076923,-0.507692307692308,
-0.492307692307692,-0.476923076923077,-0.461538461538462,-0.446153846153846,
-0.430769230769231,-0.415384615384615,-0.4,-0.384615384615385,-0.369230769230769,
-0.353846153846154,-0.338461538461538,-0.323076923076923,-0.307692307692308,
-0.292307692307692,-0.276923076923077,-0.261538461538462,-0.246153846153846,
-0.230769230769231,-0.215384615384615,-0.2,-0.184615384615385,-0.169230769230769,
-0.153846153846154,-0.138461538461538,-0.123076923076923,-0.107692307692308,
-0.0923076923076923,-0.0769230769230769,-0.0615384615384615,-0.0461538461538462,
-0.0307692307692308,-0.0153846153846154,0.),(-1.,1.),.UNSPECIFIED.)
GEOMETRIC_REPRESENTATION_ITEM()
RATIONAL_B_SPLINE_SURFACE(((1.,1.),(1.,1.),(1.,1.),(1.,1.),(1.,1.),(1.,
1.),(1.,1.),(1.,1.),(1.,1.),(1.,1.),(1.,1.),(1.,1.),(1.,1.),(1.,1.),(1.,
1.),(1.,1.),(1.,1.),(1.,1.),(1.,1.),(1.,1.),(1.,1.),(1.,1.),(1.,1.),(1.,
1.),(1.,1.),(1.,1.),(1.,1.),(1.,1.),(1.,1.),(1.,1.),(1.,1.),(1.,1.),(1.,
1.),(1.,1.),(1.,1.),(1.,1.),(1.,1.),(1.,1.),(1.,1.),(1.,1.),(1.,1.),(1.,
1.),(1.,1.),(1.,1.),(1.,1.),(1.,1.),(1.,1.),(1.,1.),(1.,1.),(1.,1.),(1.,
1.),(1.,1.),(1.,1.),(1.,1.),(1.,1.),(1.,1.),(1.,1.),(1.,1.),(1.,1.),(1.,
1.),(1.,1.),(1.,1.),(1.,1.),(1.,1.),(1.,1.),(1.,1.),(1.,1.),(1.,1.),(1.,
1.),(1.,1.)))
REPRESENTATION_ITEM('')
SURFACE()
);
#42=(
BOUNDED_SURFACE()
B_SPLINE_SURFACE(5,1,((#35342,#35343),(#35344,#35345),(#35346,#35347),(#35348,
#35349),(#35350,#35351),(#35352,#35353),(#35354,#35355),(#35356,#35357),
(#35358,#35359),(#35360,#35361),(#35362,#35363),(#35364,#35365),(#35366,
#35367),(#35368,#35369),(#35370,#35371),(#35372,#35373),(#35374,#35375),
(#35376,#35377),(#35378,#35379),(#35380,#35381),(#35382,#35383),(#35384,
#35385),(#35386,#35387),(#35388,#35389),(#35390,#35391),(#35392,#35393),
(#35394,#35395),(#35396,#35397),(#35398,#35399),(#35400,#35401),(#35402,
#35403),(#35404,#35405),(#35406,#35407),(#35408,#35409),(#35410,#35411),
(#35412,#35413),(#35414,#35415),(#35416,#35417),(#35418,#35419),(#35420,
#35421),(#35422,#35423),(#35424,#35425),(#35426,#35427),(#35428,#35429),
(#35430,#35431),(#35432,#35433),(#35434,#35435),(#35436,#35437),(#35438,
#35439),(#35440,#35441),(#35442,#35443),(#35444,#35445),(#35446,#35447),
(#35448,#35449),(#35450,#35451),(#35452,#35453),(#35454,#35455),(#35456,
#35457),(#35458,#35459),(#35460,#35461),(#35462,#35463),(#35464,#35465),
(#35466,#35467),(#35468,#35469),(#35470,#35471),(#35472,#35473),(#35474,
#35475),(#35476,#35477),(#35478,#35479),(#35480,#35481)),.UNSPECIFIED.,
 .F.,.F.,.F.)
B_SPLINE_SURFACE_WITH_KNOTS((6,1,1,1,1,1,1,1,1,1,1,1,1,1,1,1,1,1,1,1,1,
1,1,1,1,1,1,1,1,1,1,1,1,1,1,1,1,1,1,1,1,1,1,1,1,1,1,1,1,1,1,1,1,1,1,1,1,
1,1,1,1,1,1,1,1,6),(2,2),(-1.,-0.984615384615383,-0.969230769230768,-0.953846153846152,
-0.938461538461537,-0.923076923076922,-0.907692307692306,-0.892307692307691,
-0.876923076923076,-0.86153846153846,-0.846153846153845,-0.83076923076923,
-0.815384615384614,-0.799999999999999,-0.784615384615384,-0.769230769230768,
-0.753846153846153,-0.738461538461538,-0.723076923076922,-0.707692307692307,
-0.692307692307692,-0.676923076923076,-0.661538461538461,-0.646153846153846,
-0.63076923076923,-0.615384615384615,-0.6,-0.584615384615384,-0.569230769230769,
-0.553846153846154,-0.538461538461538,-0.523076923076923,-0.507692307692308,
-0.492307692307692,-0.476923076923077,-0.461538461538462,-0.446153846153846,
-0.430769230769231,-0.415384615384615,-0.4,-0.384615384615385,-0.369230769230769,
-0.353846153846154,-0.338461538461538,-0.323076923076923,-0.307692307692308,
-0.292307692307692,-0.276923076923077,-0.261538461538462,-0.246153846153846,
-0.230769230769231,-0.215384615384615,-0.2,-0.184615384615385,-0.169230769230769,
-0.153846153846154,-0.138461538461538,-0.123076923076923,-0.107692307692308,
-0.0923076923076923,-0.0769230769230769,-0.0615384615384615,-0.0461538461538462,
-0.0307692307692308,-0.0153846153846154,0.),(-1.,1.),.UNSPECIFIED.)
GEOMETRIC_REPRESENTATION_ITEM()
RATIONAL_B_SPLINE_SURFACE(((1.,1.),(1.,1.),(1.,1.),(1.,1.),(1.,1.),(1.,
1.),(1.,1.),(1.,1.),(1.,1.),(1.,1.),(1.,1.),(1.,1.),(1.,1.),(1.,1.),(1.,
1.),(1.,1.),(1.,1.),(1.,1.),(1.,1.),(1.,1.),(1.,1.),(1.,1.),(1.,1.),(1.,
1.),(1.,1.),(1.,1.),(1.,1.),(1.,1.),(1.,1.),(1.,1.),(1.,1.),(1.,1.),(1.,
1.),(1.,1.),(1.,1.),(1.,1.),(1.,1.),(1.,1.),(1.,1.),(1.,1.),(1.,1.),(1.,
1.),(1.,1.),(1.,1.),(1.,1.),(1.,1.),(1.,1.),(1.,1.),(1.,1.),(1.,1.),(1.,
1.),(1.,1.),(1.,1.),(1.,1.),(1.,1.),(1.,1.),(1.,1.),(1.,1.),(1.,1.),(1.,
1.),(1.,1.),(1.,1.),(1.,1.),(1.,1.),(1.,1.),(1.,1.),(1.,1.),(1.,1.),(1.,
1.),(1.,1.)))
REPRESENTATION_ITEM('')
SURFACE()
);
#43=(
BOUNDED_SURFACE()
B_SPLINE_SURFACE(5,1,((#35558,#35559),(#35560,#35561),(#35562,#35563),(#35564,
#35565),(#35566,#35567),(#35568,#35569),(#35570,#35571),(#35572,#35573),
(#35574,#35575),(#35576,#35577),(#35578,#35579),(#35580,#35581),(#35582,
#35583),(#35584,#35585),(#35586,#35587),(#35588,#35589),(#35590,#35591),
(#35592,#35593),(#35594,#35595),(#35596,#35597),(#35598,#35599),(#35600,
#35601),(#35602,#35603),(#35604,#35605),(#35606,#35607),(#35608,#35609),
(#35610,#35611),(#35612,#35613),(#35614,#35615),(#35616,#35617),(#35618,
#35619),(#35620,#35621),(#35622,#35623),(#35624,#35625),(#35626,#35627),
(#35628,#35629),(#35630,#35631),(#35632,#35633),(#35634,#35635),(#35636,
#35637),(#35638,#35639),(#35640,#35641),(#35642,#35643),(#35644,#35645),
(#35646,#35647),(#35648,#35649),(#35650,#35651),(#35652,#35653),(#35654,
#35655),(#35656,#35657),(#35658,#35659),(#35660,#35661),(#35662,#35663),
(#35664,#35665),(#35666,#35667),(#35668,#35669),(#35670,#35671),(#35672,
#35673),(#35674,#35675),(#35676,#35677),(#35678,#35679),(#35680,#35681),
(#35682,#35683),(#35684,#35685),(#35686,#35687),(#35688,#35689),(#35690,
#35691),(#35692,#35693),(#35694,#35695),(#35696,#35697)),.UNSPECIFIED.,
 .F.,.F.,.F.)
B_SPLINE_SURFACE_WITH_KNOTS((6,1,1,1,1,1,1,1,1,1,1,1,1,1,1,1,1,1,1,1,1,
1,1,1,1,1,1,1,1,1,1,1,1,1,1,1,1,1,1,1,1,1,1,1,1,1,1,1,1,1,1,1,1,1,1,1,1,
1,1,1,1,1,1,1,1,6),(2,2),(-1.,-0.984615384615383,-0.969230769230768,-0.953846153846152,
-0.938461538461537,-0.923076923076922,-0.907692307692306,-0.892307692307691,
-0.876923076923076,-0.86153846153846,-0.846153846153845,-0.83076923076923,
-0.815384615384614,-0.799999999999999,-0.784615384615384,-0.769230769230768,
-0.753846153846153,-0.738461538461538,-0.723076923076922,-0.707692307692307,
-0.692307692307692,-0.676923076923076,-0.661538461538461,-0.646153846153846,
-0.63076923076923,-0.615384615384615,-0.6,-0.584615384615384,-0.569230769230769,
-0.553846153846154,-0.538461538461538,-0.523076923076923,-0.507692307692308,
-0.492307692307692,-0.476923076923077,-0.461538461538462,-0.446153846153846,
-0.430769230769231,-0.415384615384615,-0.4,-0.384615384615385,-0.369230769230769,
-0.353846153846154,-0.338461538461538,-0.323076923076923,-0.307692307692308,
-0.292307692307692,-0.276923076923077,-0.261538461538462,-0.246153846153846,
-0.230769230769231,-0.215384615384615,-0.2,-0.184615384615385,-0.169230769230769,
-0.153846153846154,-0.138461538461538,-0.123076923076923,-0.107692307692308,
-0.0923076923076923,-0.0769230769230769,-0.0615384615384615,-0.0461538461538462,
-0.0307692307692308,-0.0153846153846154,0.),(-1.,1.),.UNSPECIFIED.)
GEOMETRIC_REPRESENTATION_ITEM()
RATIONAL_B_SPLINE_SURFACE(((1.,1.),(1.,1.),(1.,1.),(1.,1.),(1.,1.),(1.,
1.),(1.,1.),(1.,1.),(1.,1.),(1.,1.),(1.,1.),(1.,1.),(1.,1.),(1.,1.),(1.,
1.),(1.,1.),(1.,1.),(1.,1.),(1.,1.),(1.,1.),(1.,1.),(1.,1.),(1.,1.),(1.,
1.),(1.,1.),(1.,1.),(1.,1.),(1.,1.),(1.,1.),(1.,1.),(1.,1.),(1.,1.),(1.,
1.),(1.,1.),(1.,1.),(1.,1.),(1.,1.),(1.,1.),(1.,1.),(1.,1.),(1.,1.),(1.,
1.),(1.,1.),(1.,1.),(1.,1.),(1.,1.),(1.,1.),(1.,1.),(1.,1.),(1.,1.),(1.,
1.),(1.,1.),(1.,1.),(1.,1.),(1.,1.),(1.,1.),(1.,1.),(1.,1.),(1.,1.),(1.,
1.),(1.,1.),(1.,1.),(1.,1.),(1.,1.),(1.,1.),(1.,1.),(1.,1.),(1.,1.),(1.,
1.),(1.,1.)))
REPRESENTATION_ITEM('')
SURFACE()
);
#44=(
BOUNDED_SURFACE()
B_SPLINE_SURFACE(5,1,((#35774,#35775),(#35776,#35777),(#35778,#35779),(#35780,
#35781),(#35782,#35783),(#35784,#35785),(#35786,#35787),(#35788,#35789),
(#35790,#35791),(#35792,#35793),(#35794,#35795),(#35796,#35797),(#35798,
#35799),(#35800,#35801),(#35802,#35803),(#35804,#35805),(#35806,#35807),
(#35808,#35809),(#35810,#35811),(#35812,#35813),(#35814,#35815),(#35816,
#35817),(#35818,#35819),(#35820,#35821),(#35822,#35823),(#35824,#35825),
(#35826,#35827),(#35828,#35829),(#35830,#35831),(#35832,#35833),(#35834,
#35835),(#35836,#35837),(#35838,#35839),(#35840,#35841),(#35842,#35843),
(#35844,#35845),(#35846,#35847),(#35848,#35849),(#35850,#35851),(#35852,
#35853),(#35854,#35855),(#35856,#35857),(#35858,#35859),(#35860,#35861),
(#35862,#35863),(#35864,#35865),(#35866,#35867),(#35868,#35869),(#35870,
#35871),(#35872,#35873),(#35874,#35875),(#35876,#35877),(#35878,#35879),
(#35880,#35881),(#35882,#35883),(#35884,#35885),(#35886,#35887),(#35888,
#35889),(#35890,#35891),(#35892,#35893),(#35894,#35895),(#35896,#35897),
(#35898,#35899),(#35900,#35901),(#35902,#35903),(#35904,#35905),(#35906,
#35907),(#35908,#35909),(#35910,#35911),(#35912,#35913)),.UNSPECIFIED.,
 .F.,.F.,.F.)
B_SPLINE_SURFACE_WITH_KNOTS((6,1,1,1,1,1,1,1,1,1,1,1,1,1,1,1,1,1,1,1,1,
1,1,1,1,1,1,1,1,1,1,1,1,1,1,1,1,1,1,1,1,1,1,1,1,1,1,1,1,1,1,1,1,1,1,1,1,
1,1,1,1,1,1,1,1,6),(2,2),(-1.,-0.984615384615383,-0.969230769230768,-0.953846153846152,
-0.938461538461537,-0.923076923076922,-0.907692307692306,-0.892307692307691,
-0.876923076923076,-0.86153846153846,-0.846153846153845,-0.83076923076923,
-0.815384615384614,-0.799999999999999,-0.784615384615384,-0.769230769230768,
-0.753846153846153,-0.738461538461538,-0.723076923076922,-0.707692307692307,
-0.692307692307692,-0.676923076923076,-0.661538461538461,-0.646153846153846,
-0.63076923076923,-0.615384615384615,-0.6,-0.584615384615384,-0.569230769230769,
-0.553846153846154,-0.538461538461538,-0.523076923076923,-0.507692307692308,
-0.492307692307692,-0.476923076923077,-0.461538461538462,-0.446153846153846,
-0.430769230769231,-0.415384615384615,-0.4,-0.384615384615385,-0.369230769230769,
-0.353846153846154,-0.338461538461538,-0.323076923076923,-0.307692307692308,
-0.292307692307692,-0.276923076923077,-0.261538461538462,-0.246153846153846,
-0.230769230769231,-0.215384615384615,-0.2,-0.184615384615385,-0.169230769230769,
-0.153846153846154,-0.138461538461538,-0.123076923076923,-0.107692307692308,
-0.0923076923076923,-0.0769230769230769,-0.0615384615384615,-0.0461538461538462,
-0.0307692307692308,-0.0153846153846154,0.),(-1.,1.),.UNSPECIFIED.)
GEOMETRIC_REPRESENTATION_ITEM()
RATIONAL_B_SPLINE_SURFACE(((1.,1.),(1.,1.),(1.,1.),(1.,1.),(1.,1.),(1.,
1.),(1.,1.),(1.,1.),(1.,1.),(1.,1.),(1.,1.),(1.,1.),(1.,1.),(1.,1.),(1.,
1.),(1.,1.),(1.,1.),(1.,1.),(1.,1.),(1.,1.),(1.,1.),(1.,1.),(1.,1.),(1.,
1.),(1.,1.),(1.,1.),(1.,1.),(1.,1.),(1.,1.),(1.,1.),(1.,1.),(1.,1.),(1.,
1.),(1.,1.),(1.,1.),(1.,1.),(1.,1.),(1.,1.),(1.,1.),(1.,1.),(1.,1.),(1.,
1.),(1.,1.),(1.,1.),(1.,1.),(1.,1.),(1.,1.),(1.,1.),(1.,1.),(1.,1.),(1.,
1.),(1.,1.),(1.,1.),(1.,1.),(1.,1.),(1.,1.),(1.,1.),(1.,1.),(1.,1.),(1.,
1.),(1.,1.),(1.,1.),(1.,1.),(1.,1.),(1.,1.),(1.,1.),(1.,1.),(1.,1.),(1.,
1.),(1.,1.)))
REPRESENTATION_ITEM('')
SURFACE()
);
#45=(
BOUNDED_SURFACE()
B_SPLINE_SURFACE(5,1,((#35990,#35991),(#35992,#35993),(#35994,#35995),(#35996,
#35997),(#35998,#35999),(#36000,#36001),(#36002,#36003),(#36004,#36005),
(#36006,#36007),(#36008,#36009),(#36010,#36011),(#36012,#36013),(#36014,
#36015),(#36016,#36017),(#36018,#36019),(#36020,#36021),(#36022,#36023),
(#36024,#36025),(#36026,#36027),(#36028,#36029),(#36030,#36031),(#36032,
#36033),(#36034,#36035),(#36036,#36037),(#36038,#36039),(#36040,#36041),
(#36042,#36043),(#36044,#36045),(#36046,#36047),(#36048,#36049),(#36050,
#36051),(#36052,#36053),(#36054,#36055),(#36056,#36057),(#36058,#36059),
(#36060,#36061),(#36062,#36063),(#36064,#36065),(#36066,#36067),(#36068,
#36069),(#36070,#36071),(#36072,#36073),(#36074,#36075),(#36076,#36077),
(#36078,#36079),(#36080,#36081),(#36082,#36083),(#36084,#36085),(#36086,
#36087),(#36088,#36089),(#36090,#36091),(#36092,#36093),(#36094,#36095),
(#36096,#36097),(#36098,#36099),(#36100,#36101),(#36102,#36103),(#36104,
#36105),(#36106,#36107),(#36108,#36109),(#36110,#36111),(#36112,#36113),
(#36114,#36115),(#36116,#36117),(#36118,#36119),(#36120,#36121),(#36122,
#36123),(#36124,#36125),(#36126,#36127),(#36128,#36129)),.UNSPECIFIED.,
 .F.,.F.,.F.)
B_SPLINE_SURFACE_WITH_KNOTS((6,1,1,1,1,1,1,1,1,1,1,1,1,1,1,1,1,1,1,1,1,
1,1,1,1,1,1,1,1,1,1,1,1,1,1,1,1,1,1,1,1,1,1,1,1,1,1,1,1,1,1,1,1,1,1,1,1,
1,1,1,1,1,1,1,1,6),(2,2),(-1.,-0.984615384615383,-0.969230769230768,-0.953846153846152,
-0.938461538461537,-0.923076923076922,-0.907692307692306,-0.892307692307691,
-0.876923076923076,-0.86153846153846,-0.846153846153845,-0.83076923076923,
-0.815384615384614,-0.799999999999999,-0.784615384615384,-0.769230769230768,
-0.753846153846153,-0.738461538461538,-0.723076923076922,-0.707692307692307,
-0.692307692307692,-0.676923076923076,-0.661538461538461,-0.646153846153846,
-0.63076923076923,-0.615384615384615,-0.6,-0.584615384615384,-0.569230769230769,
-0.553846153846154,-0.538461538461538,-0.523076923076923,-0.507692307692308,
-0.492307692307692,-0.476923076923077,-0.461538461538462,-0.446153846153846,
-0.430769230769231,-0.415384615384615,-0.4,-0.384615384615385,-0.369230769230769,
-0.353846153846154,-0.338461538461538,-0.323076923076923,-0.307692307692308,
-0.292307692307692,-0.276923076923077,-0.261538461538462,-0.246153846153846,
-0.230769230769231,-0.215384615384615,-0.2,-0.184615384615385,-0.169230769230769,
-0.153846153846154,-0.138461538461538,-0.123076923076923,-0.107692307692308,
-0.0923076923076923,-0.0769230769230769,-0.0615384615384615,-0.0461538461538462,
-0.0307692307692308,-0.0153846153846154,0.),(-1.,1.),.UNSPECIFIED.)
GEOMETRIC_REPRESENTATION_ITEM()
RATIONAL_B_SPLINE_SURFACE(((1.,1.),(1.,1.),(1.,1.),(1.,1.),(1.,1.),(1.,
1.),(1.,1.),(1.,1.),(1.,1.),(1.,1.),(1.,1.),(1.,1.),(1.,1.),(1.,1.),(1.,
1.),(1.,1.),(1.,1.),(1.,1.),(1.,1.),(1.,1.),(1.,1.),(1.,1.),(1.,1.),(1.,
1.),(1.,1.),(1.,1.),(1.,1.),(1.,1.),(1.,1.),(1.,1.),(1.,1.),(1.,1.),(1.,
1.),(1.,1.),(1.,1.),(1.,1.),(1.,1.),(1.,1.),(1.,1.),(1.,1.),(1.,1.),(1.,
1.),(1.,1.),(1.,1.),(1.,1.),(1.,1.),(1.,1.),(1.,1.),(1.,1.),(1.,1.),(1.,
1.),(1.,1.),(1.,1.),(1.,1.),(1.,1.),(1.,1.),(1.,1.),(1.,1.),(1.,1.),(1.,
1.),(1.,1.),(1.,1.),(1.,1.),(1.,1.),(1.,1.),(1.,1.),(1.,1.),(1.,1.),(1.,
1.),(1.,1.)))
REPRESENTATION_ITEM('')
SURFACE()
);
#46=(
BOUNDED_SURFACE()
B_SPLINE_SURFACE(5,1,((#36206,#36207),(#36208,#36209),(#36210,#36211),(#36212,
#36213),(#36214,#36215),(#36216,#36217),(#36218,#36219),(#36220,#36221),
(#36222,#36223),(#36224,#36225),(#36226,#36227),(#36228,#36229),(#36230,
#36231),(#36232,#36233),(#36234,#36235),(#36236,#36237),(#36238,#36239),
(#36240,#36241),(#36242,#36243),(#36244,#36245),(#36246,#36247),(#36248,
#36249),(#36250,#36251),(#36252,#36253),(#36254,#36255),(#36256,#36257),
(#36258,#36259),(#36260,#36261),(#36262,#36263),(#36264,#36265),(#36266,
#36267),(#36268,#36269),(#36270,#36271),(#36272,#36273),(#36274,#36275),
(#36276,#36277),(#36278,#36279),(#36280,#36281),(#36282,#36283),(#36284,
#36285),(#36286,#36287),(#36288,#36289),(#36290,#36291),(#36292,#36293),
(#36294,#36295),(#36296,#36297),(#36298,#36299),(#36300,#36301),(#36302,
#36303),(#36304,#36305),(#36306,#36307),(#36308,#36309),(#36310,#36311),
(#36312,#36313),(#36314,#36315),(#36316,#36317),(#36318,#36319),(#36320,
#36321),(#36322,#36323),(#36324,#36325),(#36326,#36327),(#36328,#36329),
(#36330,#36331),(#36332,#36333),(#36334,#36335),(#36336,#36337),(#36338,
#36339),(#36340,#36341),(#36342,#36343),(#36344,#36345)),.UNSPECIFIED.,
 .F.,.F.,.F.)
B_SPLINE_SURFACE_WITH_KNOTS((6,1,1,1,1,1,1,1,1,1,1,1,1,1,1,1,1,1,1,1,1,
1,1,1,1,1,1,1,1,1,1,1,1,1,1,1,1,1,1,1,1,1,1,1,1,1,1,1,1,1,1,1,1,1,1,1,1,
1,1,1,1,1,1,1,1,6),(2,2),(-1.,-0.984615384615383,-0.969230769230768,-0.953846153846152,
-0.938461538461537,-0.923076923076922,-0.907692307692306,-0.892307692307691,
-0.876923076923076,-0.86153846153846,-0.846153846153845,-0.83076923076923,
-0.815384615384614,-0.799999999999999,-0.784615384615384,-0.769230769230768,
-0.753846153846153,-0.738461538461538,-0.723076923076922,-0.707692307692307,
-0.692307692307692,-0.676923076923076,-0.661538461538461,-0.646153846153846,
-0.63076923076923,-0.615384615384615,-0.6,-0.584615384615384,-0.569230769230769,
-0.553846153846154,-0.538461538461538,-0.523076923076923,-0.507692307692308,
-0.492307692307692,-0.476923076923077,-0.461538461538462,-0.446153846153846,
-0.430769230769231,-0.415384615384615,-0.4,-0.384615384615385,-0.369230769230769,
-0.353846153846154,-0.338461538461538,-0.323076923076923,-0.307692307692308,
-0.292307692307692,-0.276923076923077,-0.261538461538462,-0.246153846153846,
-0.230769230769231,-0.215384615384615,-0.2,-0.184615384615385,-0.169230769230769,
-0.153846153846154,-0.138461538461538,-0.123076923076923,-0.107692307692308,
-0.0923076923076923,-0.0769230769230769,-0.0615384615384615,-0.0461538461538462,
-0.0307692307692308,-0.0153846153846154,0.),(-1.,1.),.UNSPECIFIED.)
GEOMETRIC_REPRESENTATION_ITEM()
RATIONAL_B_SPLINE_SURFACE(((1.,1.),(1.,1.),(1.,1.),(1.,1.),(1.,1.),(1.,
1.),(1.,1.),(1.,1.),(1.,1.),(1.,1.),(1.,1.),(1.,1.),(1.,1.),(1.,1.),(1.,
1.),(1.,1.),(1.,1.),(1.,1.),(1.,1.),(1.,1.),(1.,1.),(1.,1.),(1.,1.),(1.,
1.),(1.,1.),(1.,1.),(1.,1.),(1.,1.),(1.,1.),(1.,1.),(1.,1.),(1.,1.),(1.,
1.),(1.,1.),(1.,1.),(1.,1.),(1.,1.),(1.,1.),(1.,1.),(1.,1.),(1.,1.),(1.,
1.),(1.,1.),(1.,1.),(1.,1.),(1.,1.),(1.,1.),(1.,1.),(1.,1.),(1.,1.),(1.,
1.),(1.,1.),(1.,1.),(1.,1.),(1.,1.),(1.,1.),(1.,1.),(1.,1.),(1.,1.),(1.,
1.),(1.,1.),(1.,1.),(1.,1.),(1.,1.),(1.,1.),(1.,1.),(1.,1.),(1.,1.),(1.,
1.),(1.,1.)))
REPRESENTATION_ITEM('')
SURFACE()
);
#47=(
BOUNDED_SURFACE()
B_SPLINE_SURFACE(5,1,((#36422,#36423),(#36424,#36425),(#36426,#36427),(#36428,
#36429),(#36430,#36431),(#36432,#36433),(#36434,#36435),(#36436,#36437),
(#36438,#36439),(#36440,#36441),(#36442,#36443),(#36444,#36445),(#36446,
#36447),(#36448,#36449),(#36450,#36451),(#36452,#36453),(#36454,#36455),
(#36456,#36457),(#36458,#36459),(#36460,#36461),(#36462,#36463),(#36464,
#36465),(#36466,#36467),(#36468,#36469),(#36470,#36471),(#36472,#36473),
(#36474,#36475),(#36476,#36477),(#36478,#36479),(#36480,#36481),(#36482,
#36483),(#36484,#36485),(#36486,#36487),(#36488,#36489),(#36490,#36491),
(#36492,#36493),(#36494,#36495),(#36496,#36497),(#36498,#36499),(#36500,
#36501),(#36502,#36503),(#36504,#36505),(#36506,#36507),(#36508,#36509),
(#36510,#36511),(#36512,#36513),(#36514,#36515),(#36516,#36517),(#36518,
#36519),(#36520,#36521),(#36522,#36523),(#36524,#36525),(#36526,#36527),
(#36528,#36529),(#36530,#36531),(#36532,#36533),(#36534,#36535),(#36536,
#36537),(#36538,#36539),(#36540,#36541),(#36542,#36543),(#36544,#36545),
(#36546,#36547),(#36548,#36549),(#36550,#36551),(#36552,#36553),(#36554,
#36555),(#36556,#36557),(#36558,#36559),(#36560,#36561)),.UNSPECIFIED.,
 .F.,.F.,.F.)
B_SPLINE_SURFACE_WITH_KNOTS((6,1,1,1,1,1,1,1,1,1,1,1,1,1,1,1,1,1,1,1,1,
1,1,1,1,1,1,1,1,1,1,1,1,1,1,1,1,1,1,1,1,1,1,1,1,1,1,1,1,1,1,1,1,1,1,1,1,
1,1,1,1,1,1,1,1,6),(2,2),(-1.,-0.984615384615383,-0.969230769230768,-0.953846153846152,
-0.938461538461537,-0.923076923076922,-0.907692307692306,-0.892307692307691,
-0.876923076923076,-0.86153846153846,-0.846153846153845,-0.83076923076923,
-0.815384615384614,-0.799999999999999,-0.784615384615384,-0.769230769230768,
-0.753846153846153,-0.738461538461538,-0.723076923076922,-0.707692307692307,
-0.692307692307692,-0.676923076923076,-0.661538461538461,-0.646153846153846,
-0.63076923076923,-0.615384615384615,-0.6,-0.584615384615384,-0.569230769230769,
-0.553846153846154,-0.538461538461538,-0.523076923076923,-0.507692307692308,
-0.492307692307692,-0.476923076923077,-0.461538461538462,-0.446153846153846,
-0.430769230769231,-0.415384615384615,-0.4,-0.384615384615385,-0.369230769230769,
-0.353846153846154,-0.338461538461538,-0.323076923076923,-0.307692307692308,
-0.292307692307692,-0.276923076923077,-0.261538461538462,-0.246153846153846,
-0.230769230769231,-0.215384615384615,-0.2,-0.184615384615385,-0.169230769230769,
-0.153846153846154,-0.138461538461538,-0.123076923076923,-0.107692307692308,
-0.0923076923076923,-0.0769230769230769,-0.0615384615384615,-0.0461538461538462,
-0.0307692307692308,-0.0153846153846154,0.),(-1.,1.),.UNSPECIFIED.)
GEOMETRIC_REPRESENTATION_ITEM()
RATIONAL_B_SPLINE_SURFACE(((1.,1.),(1.,1.),(1.,1.),(1.,1.),(1.,1.),(1.,
1.),(1.,1.),(1.,1.),(1.,1.),(1.,1.),(1.,1.),(1.,1.),(1.,1.),(1.,1.),(1.,
1.),(1.,1.),(1.,1.),(1.,1.),(1.,1.),(1.,1.),(1.,1.),(1.,1.),(1.,1.),(1.,
1.),(1.,1.),(1.,1.),(1.,1.),(1.,1.),(1.,1.),(1.,1.),(1.,1.),(1.,1.),(1.,
1.),(1.,1.),(1.,1.),(1.,1.),(1.,1.),(1.,1.),(1.,1.),(1.,1.),(1.,1.),(1.,
1.),(1.,1.),(1.,1.),(1.,1.),(1.,1.),(1.,1.),(1.,1.),(1.,1.),(1.,1.),(1.,
1.),(1.,1.),(1.,1.),(1.,1.),(1.,1.),(1.,1.),(1.,1.),(1.,1.),(1.,1.),(1.,
1.),(1.,1.),(1.,1.),(1.,1.),(1.,1.),(1.,1.),(1.,1.),(1.,1.),(1.,1.),(1.,
1.),(1.,1.)))
REPRESENTATION_ITEM('')
SURFACE()
);
#48=(
BOUNDED_SURFACE()
B_SPLINE_SURFACE(5,1,((#36638,#36639),(#36640,#36641),(#36642,#36643),(#36644,
#36645),(#36646,#36647),(#36648,#36649),(#36650,#36651),(#36652,#36653),
(#36654,#36655),(#36656,#36657),(#36658,#36659),(#36660,#36661),(#36662,
#36663),(#36664,#36665),(#36666,#36667),(#36668,#36669),(#36670,#36671),
(#36672,#36673),(#36674,#36675),(#36676,#36677),(#36678,#36679),(#36680,
#36681),(#36682,#36683),(#36684,#36685),(#36686,#36687),(#36688,#36689),
(#36690,#36691),(#36692,#36693),(#36694,#36695),(#36696,#36697),(#36698,
#36699),(#36700,#36701),(#36702,#36703),(#36704,#36705),(#36706,#36707),
(#36708,#36709),(#36710,#36711),(#36712,#36713),(#36714,#36715),(#36716,
#36717),(#36718,#36719),(#36720,#36721),(#36722,#36723),(#36724,#36725),
(#36726,#36727),(#36728,#36729),(#36730,#36731),(#36732,#36733),(#36734,
#36735),(#36736,#36737),(#36738,#36739),(#36740,#36741),(#36742,#36743),
(#36744,#36745),(#36746,#36747),(#36748,#36749),(#36750,#36751),(#36752,
#36753),(#36754,#36755),(#36756,#36757),(#36758,#36759),(#36760,#36761),
(#36762,#36763),(#36764,#36765),(#36766,#36767),(#36768,#36769),(#36770,
#36771),(#36772,#36773),(#36774,#36775),(#36776,#36777)),.UNSPECIFIED.,
 .F.,.F.,.F.)
B_SPLINE_SURFACE_WITH_KNOTS((6,1,1,1,1,1,1,1,1,1,1,1,1,1,1,1,1,1,1,1,1,
1,1,1,1,1,1,1,1,1,1,1,1,1,1,1,1,1,1,1,1,1,1,1,1,1,1,1,1,1,1,1,1,1,1,1,1,
1,1,1,1,1,1,1,1,6),(2,2),(-1.,-0.984615384615383,-0.969230769230768,-0.953846153846152,
-0.938461538461537,-0.923076923076922,-0.907692307692306,-0.892307692307691,
-0.876923076923076,-0.86153846153846,-0.846153846153845,-0.83076923076923,
-0.815384615384614,-0.799999999999999,-0.784615384615384,-0.769230769230768,
-0.753846153846153,-0.738461538461538,-0.723076923076922,-0.707692307692307,
-0.692307692307692,-0.676923076923076,-0.661538461538461,-0.646153846153846,
-0.63076923076923,-0.615384615384615,-0.6,-0.584615384615384,-0.569230769230769,
-0.553846153846154,-0.538461538461538,-0.523076923076923,-0.507692307692308,
-0.492307692307692,-0.476923076923077,-0.461538461538462,-0.446153846153846,
-0.430769230769231,-0.415384615384615,-0.4,-0.384615384615385,-0.369230769230769,
-0.353846153846154,-0.338461538461538,-0.323076923076923,-0.307692307692308,
-0.292307692307692,-0.276923076923077,-0.261538461538462,-0.246153846153846,
-0.230769230769231,-0.215384615384615,-0.2,-0.184615384615385,-0.169230769230769,
-0.153846153846154,-0.138461538461538,-0.123076923076923,-0.107692307692308,
-0.0923076923076923,-0.0769230769230769,-0.0615384615384615,-0.0461538461538462,
-0.0307692307692308,-0.0153846153846154,0.),(-1.,1.),.UNSPECIFIED.)
GEOMETRIC_REPRESENTATION_ITEM()
RATIONAL_B_SPLINE_SURFACE(((1.,1.),(1.,1.),(1.,1.),(1.,1.),(1.,1.),(1.,
1.),(1.,1.),(1.,1.),(1.,1.),(1.,1.),(1.,1.),(1.,1.),(1.,1.),(1.,1.),(1.,
1.),(1.,1.),(1.,1.),(1.,1.),(1.,1.),(1.,1.),(1.,1.),(1.,1.),(1.,1.),(1.,
1.),(1.,1.),(1.,1.),(1.,1.),(1.,1.),(1.,1.),(1.,1.),(1.,1.),(1.,1.),(1.,
1.),(1.,1.),(1.,1.),(1.,1.),(1.,1.),(1.,1.),(1.,1.),(1.,1.),(1.,1.),(1.,
1.),(1.,1.),(1.,1.),(1.,1.),(1.,1.),(1.,1.),(1.,1.),(1.,1.),(1.,1.),(1.,
1.),(1.,1.),(1.,1.),(1.,1.),(1.,1.),(1.,1.),(1.,1.),(1.,1.),(1.,1.),(1.,
1.),(1.,1.),(1.,1.),(1.,1.),(1.,1.),(1.,1.),(1.,1.),(1.,1.),(1.,1.),(1.,
1.),(1.,1.)))
REPRESENTATION_ITEM('')
SURFACE()
);
#49=(
BOUNDED_SURFACE()
B_SPLINE_SURFACE(5,1,((#36854,#36855),(#36856,#36857),(#36858,#36859),(#36860,
#36861),(#36862,#36863),(#36864,#36865),(#36866,#36867),(#36868,#36869),
(#36870,#36871),(#36872,#36873),(#36874,#36875),(#36876,#36877),(#36878,
#36879),(#36880,#36881),(#36882,#36883),(#36884,#36885),(#36886,#36887),
(#36888,#36889),(#36890,#36891),(#36892,#36893),(#36894,#36895),(#36896,
#36897),(#36898,#36899),(#36900,#36901),(#36902,#36903),(#36904,#36905),
(#36906,#36907),(#36908,#36909),(#36910,#36911),(#36912,#36913),(#36914,
#36915),(#36916,#36917),(#36918,#36919),(#36920,#36921),(#36922,#36923),
(#36924,#36925),(#36926,#36927),(#36928,#36929),(#36930,#36931),(#36932,
#36933),(#36934,#36935),(#36936,#36937),(#36938,#36939),(#36940,#36941),
(#36942,#36943),(#36944,#36945),(#36946,#36947),(#36948,#36949),(#36950,
#36951),(#36952,#36953),(#36954,#36955),(#36956,#36957),(#36958,#36959),
(#36960,#36961),(#36962,#36963),(#36964,#36965),(#36966,#36967),(#36968,
#36969),(#36970,#36971),(#36972,#36973),(#36974,#36975),(#36976,#36977),
(#36978,#36979),(#36980,#36981),(#36982,#36983),(#36984,#36985),(#36986,
#36987),(#36988,#36989),(#36990,#36991),(#36992,#36993)),.UNSPECIFIED.,
 .F.,.F.,.F.)
B_SPLINE_SURFACE_WITH_KNOTS((6,1,1,1,1,1,1,1,1,1,1,1,1,1,1,1,1,1,1,1,1,
1,1,1,1,1,1,1,1,1,1,1,1,1,1,1,1,1,1,1,1,1,1,1,1,1,1,1,1,1,1,1,1,1,1,1,1,
1,1,1,1,1,1,1,1,6),(2,2),(-1.,-0.984615384615383,-0.969230769230768,-0.953846153846152,
-0.938461538461537,-0.923076923076922,-0.907692307692306,-0.892307692307691,
-0.876923076923076,-0.86153846153846,-0.846153846153845,-0.83076923076923,
-0.815384615384614,-0.799999999999999,-0.784615384615384,-0.769230769230768,
-0.753846153846153,-0.738461538461538,-0.723076923076922,-0.707692307692307,
-0.692307692307692,-0.676923076923076,-0.661538461538461,-0.646153846153846,
-0.63076923076923,-0.615384615384615,-0.6,-0.584615384615384,-0.569230769230769,
-0.553846153846154,-0.538461538461538,-0.523076923076923,-0.507692307692308,
-0.492307692307692,-0.476923076923077,-0.461538461538462,-0.446153846153846,
-0.430769230769231,-0.415384615384615,-0.4,-0.384615384615385,-0.369230769230769,
-0.353846153846154,-0.338461538461538,-0.323076923076923,-0.307692307692308,
-0.292307692307692,-0.276923076923077,-0.261538461538462,-0.246153846153846,
-0.230769230769231,-0.215384615384615,-0.2,-0.184615384615385,-0.169230769230769,
-0.153846153846154,-0.138461538461538,-0.123076923076923,-0.107692307692308,
-0.0923076923076923,-0.0769230769230769,-0.0615384615384615,-0.0461538461538462,
-0.0307692307692308,-0.0153846153846154,0.),(-1.,1.),.UNSPECIFIED.)
GEOMETRIC_REPRESENTATION_ITEM()
RATIONAL_B_SPLINE_SURFACE(((1.,1.),(1.,1.),(1.,1.),(1.,1.),(1.,1.),(1.,
1.),(1.,1.),(1.,1.),(1.,1.),(1.,1.),(1.,1.),(1.,1.),(1.,1.),(1.,1.),(1.,
1.),(1.,1.),(1.,1.),(1.,1.),(1.,1.),(1.,1.),(1.,1.),(1.,1.),(1.,1.),(1.,
1.),(1.,1.),(1.,1.),(1.,1.),(1.,1.),(1.,1.),(1.,1.),(1.,1.),(1.,1.),(1.,
1.),(1.,1.),(1.,1.),(1.,1.),(1.,1.),(1.,1.),(1.,1.),(1.,1.),(1.,1.),(1.,
1.),(1.,1.),(1.,1.),(1.,1.),(1.,1.),(1.,1.),(1.,1.),(1.,1.),(1.,1.),(1.,
1.),(1.,1.),(1.,1.),(1.,1.),(1.,1.),(1.,1.),(1.,1.),(1.,1.),(1.,1.),(1.,
1.),(1.,1.),(1.,1.),(1.,1.),(1.,1.),(1.,1.),(1.,1.),(1.,1.),(1.,1.),(1.,
1.),(1.,1.)))
REPRESENTATION_ITEM('')
SURFACE()
);
#50=(
BOUNDED_SURFACE()
B_SPLINE_SURFACE(5,1,((#37070,#37071),(#37072,#37073),(#37074,#37075),(#37076,
#37077),(#37078,#37079),(#37080,#37081),(#37082,#37083),(#37084,#37085),
(#37086,#37087),(#37088,#37089),(#37090,#37091),(#37092,#37093),(#37094,
#37095),(#37096,#37097),(#37098,#37099),(#37100,#37101),(#37102,#37103),
(#37104,#37105),(#37106,#37107),(#37108,#37109),(#37110,#37111),(#37112,
#37113),(#37114,#37115),(#37116,#37117),(#37118,#37119),(#37120,#37121),
(#37122,#37123),(#37124,#37125),(#37126,#37127),(#37128,#37129),(#37130,
#37131),(#37132,#37133),(#37134,#37135),(#37136,#37137),(#37138,#37139),
(#37140,#37141),(#37142,#37143),(#37144,#37145),(#37146,#37147),(#37148,
#37149),(#37150,#37151),(#37152,#37153),(#37154,#37155),(#37156,#37157),
(#37158,#37159),(#37160,#37161),(#37162,#37163),(#37164,#37165),(#37166,
#37167),(#37168,#37169),(#37170,#37171),(#37172,#37173),(#37174,#37175),
(#37176,#37177),(#37178,#37179),(#37180,#37181),(#37182,#37183),(#37184,
#37185),(#37186,#37187),(#37188,#37189),(#37190,#37191),(#37192,#37193),
(#37194,#37195),(#37196,#37197),(#37198,#37199),(#37200,#37201),(#37202,
#37203),(#37204,#37205),(#37206,#37207),(#37208,#37209)),.UNSPECIFIED.,
 .F.,.F.,.F.)
B_SPLINE_SURFACE_WITH_KNOTS((6,1,1,1,1,1,1,1,1,1,1,1,1,1,1,1,1,1,1,1,1,
1,1,1,1,1,1,1,1,1,1,1,1,1,1,1,1,1,1,1,1,1,1,1,1,1,1,1,1,1,1,1,1,1,1,1,1,
1,1,1,1,1,1,1,1,6),(2,2),(-1.,-0.984615384615383,-0.969230769230768,-0.953846153846152,
-0.938461538461537,-0.923076923076922,-0.907692307692306,-0.892307692307691,
-0.876923076923076,-0.86153846153846,-0.846153846153845,-0.83076923076923,
-0.815384615384614,-0.799999999999999,-0.784615384615384,-0.769230769230768,
-0.753846153846153,-0.738461538461538,-0.723076923076922,-0.707692307692307,
-0.692307692307692,-0.676923076923076,-0.661538461538461,-0.646153846153846,
-0.63076923076923,-0.615384615384615,-0.6,-0.584615384615384,-0.569230769230769,
-0.553846153846154,-0.538461538461538,-0.523076923076923,-0.507692307692308,
-0.492307692307692,-0.476923076923077,-0.461538461538462,-0.446153846153846,
-0.430769230769231,-0.415384615384615,-0.4,-0.384615384615385,-0.369230769230769,
-0.353846153846154,-0.338461538461538,-0.323076923076923,-0.307692307692308,
-0.292307692307692,-0.276923076923077,-0.261538461538462,-0.246153846153846,
-0.230769230769231,-0.215384615384615,-0.2,-0.184615384615385,-0.169230769230769,
-0.153846153846154,-0.138461538461538,-0.123076923076923,-0.107692307692308,
-0.0923076923076923,-0.0769230769230769,-0.0615384615384615,-0.0461538461538462,
-0.0307692307692308,-0.0153846153846154,0.),(-1.,1.),.UNSPECIFIED.)
GEOMETRIC_REPRESENTATION_ITEM()
RATIONAL_B_SPLINE_SURFACE(((1.,1.),(1.,1.),(1.,1.),(1.,1.),(1.,1.),(1.,
1.),(1.,1.),(1.,1.),(1.,1.),(1.,1.),(1.,1.),(1.,1.),(1.,1.),(1.,1.),(1.,
1.),(1.,1.),(1.,1.),(1.,1.),(1.,1.),(1.,1.),(1.,1.),(1.,1.),(1.,1.),(1.,
1.),(1.,1.),(1.,1.),(1.,1.),(1.,1.),(1.,1.),(1.,1.),(1.,1.),(1.,1.),(1.,
1.),(1.,1.),(1.,1.),(1.,1.),(1.,1.),(1.,1.),(1.,1.),(1.,1.),(1.,1.),(1.,
1.),(1.,1.),(1.,1.),(1.,1.),(1.,1.),(1.,1.),(1.,1.),(1.,1.),(1.,1.),(1.,
1.),(1.,1.),(1.,1.),(1.,1.),(1.,1.),(1.,1.),(1.,1.),(1.,1.),(1.,1.),(1.,
1.),(1.,1.),(1.,1.),(1.,1.),(1.,1.),(1.,1.),(1.,1.),(1.,1.),(1.,1.),(1.,
1.),(1.,1.)))
REPRESENTATION_ITEM('')
SURFACE()
);
#51=(
BOUNDED_SURFACE()
B_SPLINE_SURFACE(5,1,((#40614,#40615),(#40616,#40617),(#40618,#40619),(#40620,
#40621),(#40622,#40623),(#40624,#40625),(#40626,#40627),(#40628,#40629),
(#40630,#40631),(#40632,#40633),(#40634,#40635),(#40636,#40637),(#40638,
#40639),(#40640,#40641),(#40642,#40643),(#40644,#40645),(#40646,#40647),
(#40648,#40649),(#40650,#40651),(#40652,#40653),(#40654,#40655),(#40656,
#40657),(#40658,#40659),(#40660,#40661),(#40662,#40663),(#40664,#40665),
(#40666,#40667),(#40668,#40669),(#40670,#40671),(#40672,#40673),(#40674,
#40675),(#40676,#40677),(#40678,#40679),(#40680,#40681),(#40682,#40683),
(#40684,#40685),(#40686,#40687),(#40688,#40689),(#40690,#40691),(#40692,
#40693),(#40694,#40695),(#40696,#40697),(#40698,#40699),(#40700,#40701),
(#40702,#40703),(#40704,#40705),(#40706,#40707),(#40708,#40709),(#40710,
#40711),(#40712,#40713),(#40714,#40715),(#40716,#40717),(#40718,#40719),
(#40720,#40721),(#40722,#40723),(#40724,#40725),(#40726,#40727),(#40728,
#40729),(#40730,#40731),(#40732,#40733),(#40734,#40735),(#40736,#40737),
(#40738,#40739),(#40740,#40741),(#40742,#40743),(#40744,#40745),(#40746,
#40747),(#40748,#40749),(#40750,#40751),(#40752,#40753)),.UNSPECIFIED.,
 .F.,.F.,.F.)
B_SPLINE_SURFACE_WITH_KNOTS((6,1,1,1,1,1,1,1,1,1,1,1,1,1,1,1,1,1,1,1,1,
1,1,1,1,1,1,1,1,1,1,1,1,1,1,1,1,1,1,1,1,1,1,1,1,1,1,1,1,1,1,1,1,1,1,1,1,
1,1,1,1,1,1,1,1,6),(2,2),(-1.,-0.984615384615383,-0.969230769230768,-0.953846153846152,
-0.938461538461537,-0.923076923076922,-0.907692307692306,-0.892307692307691,
-0.876923076923076,-0.86153846153846,-0.846153846153845,-0.83076923076923,
-0.815384615384614,-0.799999999999999,-0.784615384615384,-0.769230769230768,
-0.753846153846153,-0.738461538461538,-0.723076923076922,-0.707692307692307,
-0.692307692307692,-0.676923076923076,-0.661538461538461,-0.646153846153846,
-0.63076923076923,-0.615384615384615,-0.6,-0.584615384615384,-0.569230769230769,
-0.553846153846154,-0.538461538461538,-0.523076923076923,-0.507692307692308,
-0.492307692307692,-0.476923076923077,-0.461538461538462,-0.446153846153846,
-0.430769230769231,-0.415384615384615,-0.4,-0.384615384615385,-0.369230769230769,
-0.353846153846154,-0.338461538461538,-0.323076923076923,-0.307692307692308,
-0.292307692307692,-0.276923076923077,-0.261538461538462,-0.246153846153846,
-0.230769230769231,-0.215384615384615,-0.2,-0.184615384615385,-0.169230769230769,
-0.153846153846154,-0.138461538461538,-0.123076923076923,-0.107692307692308,
-0.0923076923076923,-0.0769230769230769,-0.0615384615384615,-0.0461538461538462,
-0.0307692307692308,-0.0153846153846154,0.),(-1.,1.),.UNSPECIFIED.)
GEOMETRIC_REPRESENTATION_ITEM()
RATIONAL_B_SPLINE_SURFACE(((1.,1.),(1.,1.),(1.,1.),(1.,1.),(1.,1.),(1.,
1.),(1.,1.),(1.,1.),(1.,1.),(1.,1.),(1.,1.),(1.,1.),(1.,1.),(1.,1.),(1.,
1.),(1.,1.),(1.,1.),(1.,1.),(1.,1.),(1.,1.),(1.,1.),(1.,1.),(1.,1.),(1.,
1.),(1.,1.),(1.,1.),(1.,1.),(1.,1.),(1.,1.),(1.,1.),(1.,1.),(1.,1.),(1.,
1.),(1.,1.),(1.,1.),(1.,1.),(1.,1.),(1.,1.),(1.,1.),(1.,1.),(1.,1.),(1.,
1.),(1.,1.),(1.,1.),(1.,1.),(1.,1.),(1.,1.),(1.,1.),(1.,1.),(1.,1.),(1.,
1.),(1.,1.),(1.,1.),(1.,1.),(1.,1.),(1.,1.),(1.,1.),(1.,1.),(1.,1.),(1.,
1.),(1.,1.),(1.,1.),(1.,1.),(1.,1.),(1.,1.),(1.,1.),(1.,1.),(1.,1.),(1.,
1.),(1.,1.)))
REPRESENTATION_ITEM('')
SURFACE()
);
#52=(
BOUNDED_SURFACE()
B_SPLINE_SURFACE(5,1,((#40832,#40833),(#40834,#40835),(#40836,#40837),(#40838,
#40839),(#40840,#40841),(#40842,#40843),(#40844,#40845),(#40846,#40847),
(#40848,#40849),(#40850,#40851),(#40852,#40853),(#40854,#40855),(#40856,
#40857),(#40858,#40859),(#40860,#40861),(#40862,#40863),(#40864,#40865),
(#40866,#40867),(#40868,#40869),(#40870,#40871),(#40872,#40873),(#40874,
#40875),(#40876,#40877),(#40878,#40879),(#40880,#40881),(#40882,#40883),
(#40884,#40885),(#40886,#40887),(#40888,#40889),(#40890,#40891),(#40892,
#40893),(#40894,#40895),(#40896,#40897),(#40898,#40899),(#40900,#40901),
(#40902,#40903),(#40904,#40905),(#40906,#40907),(#40908,#40909),(#40910,
#40911),(#40912,#40913),(#40914,#40915),(#40916,#40917),(#40918,#40919),
(#40920,#40921),(#40922,#40923),(#40924,#40925),(#40926,#40927),(#40928,
#40929),(#40930,#40931),(#40932,#40933),(#40934,#40935),(#40936,#40937),
(#40938,#40939),(#40940,#40941),(#40942,#40943),(#40944,#40945),(#40946,
#40947),(#40948,#40949),(#40950,#40951),(#40952,#40953),(#40954,#40955),
(#40956,#40957),(#40958,#40959),(#40960,#40961),(#40962,#40963),(#40964,
#40965),(#40966,#40967),(#40968,#40969),(#40970,#40971)),.UNSPECIFIED.,
 .F.,.F.,.F.)
B_SPLINE_SURFACE_WITH_KNOTS((6,1,1,1,1,1,1,1,1,1,1,1,1,1,1,1,1,1,1,1,1,
1,1,1,1,1,1,1,1,1,1,1,1,1,1,1,1,1,1,1,1,1,1,1,1,1,1,1,1,1,1,1,1,1,1,1,1,
1,1,1,1,1,1,1,1,6),(2,2),(-1.,-0.984615384615383,-0.969230769230768,-0.953846153846152,
-0.938461538461537,-0.923076923076922,-0.907692307692306,-0.892307692307691,
-0.876923076923076,-0.86153846153846,-0.846153846153845,-0.83076923076923,
-0.815384615384614,-0.799999999999999,-0.784615384615384,-0.769230769230768,
-0.753846153846153,-0.738461538461538,-0.723076923076922,-0.707692307692307,
-0.692307692307692,-0.676923076923076,-0.661538461538461,-0.646153846153846,
-0.63076923076923,-0.615384615384615,-0.6,-0.584615384615384,-0.569230769230769,
-0.553846153846154,-0.538461538461538,-0.523076923076923,-0.507692307692308,
-0.492307692307692,-0.476923076923077,-0.461538461538462,-0.446153846153846,
-0.430769230769231,-0.415384615384615,-0.4,-0.384615384615385,-0.369230769230769,
-0.353846153846154,-0.338461538461538,-0.323076923076923,-0.307692307692308,
-0.292307692307692,-0.276923076923077,-0.261538461538462,-0.246153846153846,
-0.230769230769231,-0.215384615384615,-0.2,-0.184615384615385,-0.169230769230769,
-0.153846153846154,-0.138461538461538,-0.123076923076923,-0.107692307692308,
-0.0923076923076923,-0.0769230769230769,-0.0615384615384615,-0.0461538461538462,
-0.0307692307692308,-0.0153846153846154,0.),(-1.,1.),.UNSPECIFIED.)
GEOMETRIC_REPRESENTATION_ITEM()
RATIONAL_B_SPLINE_SURFACE(((1.,1.),(1.,1.),(1.,1.),(1.,1.),(1.,1.),(1.,
1.),(1.,1.),(1.,1.),(1.,1.),(1.,1.),(1.,1.),(1.,1.),(1.,1.),(1.,1.),(1.,
1.),(1.,1.),(1.,1.),(1.,1.),(1.,1.),(1.,1.),(1.,1.),(1.,1.),(1.,1.),(1.,
1.),(1.,1.),(1.,1.),(1.,1.),(1.,1.),(1.,1.),(1.,1.),(1.,1.),(1.,1.),(1.,
1.),(1.,1.),(1.,1.),(1.,1.),(1.,1.),(1.,1.),(1.,1.),(1.,1.),(1.,1.),(1.,
1.),(1.,1.),(1.,1.),(1.,1.),(1.,1.),(1.,1.),(1.,1.),(1.,1.),(1.,1.),(1.,
1.),(1.,1.),(1.,1.),(1.,1.),(1.,1.),(1.,1.),(1.,1.),(1.,1.),(1.,1.),(1.,
1.),(1.,1.),(1.,1.),(1.,1.),(1.,1.),(1.,1.),(1.,1.),(1.,1.),(1.,1.),(1.,
1.),(1.,1.)))
REPRESENTATION_ITEM('')
SURFACE()
);
#53=(
BOUNDED_SURFACE()
B_SPLINE_SURFACE(5,1,((#41048,#41049),(#41050,#41051),(#41052,#41053),(#41054,
#41055),(#41056,#41057),(#41058,#41059),(#41060,#41061),(#41062,#41063),
(#41064,#41065),(#41066,#41067),(#41068,#41069),(#41070,#41071),(#41072,
#41073),(#41074,#41075),(#41076,#41077),(#41078,#41079),(#41080,#41081),
(#41082,#41083),(#41084,#41085),(#41086,#41087),(#41088,#41089),(#41090,
#41091),(#41092,#41093),(#41094,#41095),(#41096,#41097),(#41098,#41099),
(#41100,#41101),(#41102,#41103),(#41104,#41105),(#41106,#41107),(#41108,
#41109),(#41110,#41111),(#41112,#41113),(#41114,#41115),(#41116,#41117),
(#41118,#41119),(#41120,#41121),(#41122,#41123),(#41124,#41125),(#41126,
#41127),(#41128,#41129),(#41130,#41131),(#41132,#41133),(#41134,#41135),
(#41136,#41137),(#41138,#41139),(#41140,#41141),(#41142,#41143),(#41144,
#41145),(#41146,#41147),(#41148,#41149),(#41150,#41151),(#41152,#41153),
(#41154,#41155),(#41156,#41157),(#41158,#41159),(#41160,#41161),(#41162,
#41163),(#41164,#41165),(#41166,#41167),(#41168,#41169),(#41170,#41171),
(#41172,#41173),(#41174,#41175),(#41176,#41177),(#41178,#41179),(#41180,
#41181),(#41182,#41183),(#41184,#41185),(#41186,#41187)),.UNSPECIFIED.,
 .F.,.F.,.F.)
B_SPLINE_SURFACE_WITH_KNOTS((6,1,1,1,1,1,1,1,1,1,1,1,1,1,1,1,1,1,1,1,1,
1,1,1,1,1,1,1,1,1,1,1,1,1,1,1,1,1,1,1,1,1,1,1,1,1,1,1,1,1,1,1,1,1,1,1,1,
1,1,1,1,1,1,1,1,6),(2,2),(-1.,-0.984615384615383,-0.969230769230768,-0.953846153846152,
-0.938461538461537,-0.923076923076922,-0.907692307692306,-0.892307692307691,
-0.876923076923076,-0.86153846153846,-0.846153846153845,-0.83076923076923,
-0.815384615384614,-0.799999999999999,-0.784615384615384,-0.769230769230768,
-0.753846153846153,-0.738461538461538,-0.723076923076922,-0.707692307692307,
-0.692307692307692,-0.676923076923076,-0.661538461538461,-0.646153846153846,
-0.63076923076923,-0.615384615384615,-0.6,-0.584615384615384,-0.569230769230769,
-0.553846153846154,-0.538461538461538,-0.523076923076923,-0.507692307692308,
-0.492307692307692,-0.476923076923077,-0.461538461538462,-0.446153846153846,
-0.430769230769231,-0.415384615384615,-0.4,-0.384615384615385,-0.369230769230769,
-0.353846153846154,-0.338461538461538,-0.323076923076923,-0.307692307692308,
-0.292307692307692,-0.276923076923077,-0.261538461538462,-0.246153846153846,
-0.230769230769231,-0.215384615384615,-0.2,-0.184615384615385,-0.169230769230769,
-0.153846153846154,-0.138461538461538,-0.123076923076923,-0.107692307692308,
-0.0923076923076923,-0.0769230769230769,-0.0615384615384615,-0.0461538461538462,
-0.0307692307692308,-0.0153846153846154,0.),(-1.,1.),.UNSPECIFIED.)
GEOMETRIC_REPRESENTATION_ITEM()
RATIONAL_B_SPLINE_SURFACE(((1.,1.),(1.,1.),(1.,1.),(1.,1.),(1.,1.),(1.,
1.),(1.,1.),(1.,1.),(1.,1.),(1.,1.),(1.,1.),(1.,1.),(1.,1.),(1.,1.),(1.,
1.),(1.,1.),(1.,1.),(1.,1.),(1.,1.),(1.,1.),(1.,1.),(1.,1.),(1.,1.),(1.,
1.),(1.,1.),(1.,1.),(1.,1.),(1.,1.),(1.,1.),(1.,1.),(1.,1.),(1.,1.),(1.,
1.),(1.,1.),(1.,1.),(1.,1.),(1.,1.),(1.,1.),(1.,1.),(1.,1.),(1.,1.),(1.,
1.),(1.,1.),(1.,1.),(1.,1.),(1.,1.),(1.,1.),(1.,1.),(1.,1.),(1.,1.),(1.,
1.),(1.,1.),(1.,1.),(1.,1.),(1.,1.),(1.,1.),(1.,1.),(1.,1.),(1.,1.),(1.,
1.),(1.,1.),(1.,1.),(1.,1.),(1.,1.),(1.,1.),(1.,1.),(1.,1.),(1.,1.),(1.,
1.),(1.,1.)))
REPRESENTATION_ITEM('')
SURFACE()
);
#54=(
BOUNDED_SURFACE()
B_SPLINE_SURFACE(5,1,((#41264,#41265),(#41266,#41267),(#41268,#41269),(#41270,
#41271),(#41272,#41273),(#41274,#41275),(#41276,#41277),(#41278,#41279),
(#41280,#41281),(#41282,#41283),(#41284,#41285),(#41286,#41287),(#41288,
#41289),(#41290,#41291),(#41292,#41293),(#41294,#41295),(#41296,#41297),
(#41298,#41299),(#41300,#41301),(#41302,#41303),(#41304,#41305),(#41306,
#41307),(#41308,#41309),(#41310,#41311),(#41312,#41313),(#41314,#41315),
(#41316,#41317),(#41318,#41319),(#41320,#41321),(#41322,#41323),(#41324,
#41325),(#41326,#41327),(#41328,#41329),(#41330,#41331),(#41332,#41333),
(#41334,#41335),(#41336,#41337),(#41338,#41339),(#41340,#41341),(#41342,
#41343),(#41344,#41345),(#41346,#41347),(#41348,#41349),(#41350,#41351),
(#41352,#41353),(#41354,#41355),(#41356,#41357),(#41358,#41359),(#41360,
#41361),(#41362,#41363),(#41364,#41365),(#41366,#41367),(#41368,#41369),
(#41370,#41371),(#41372,#41373),(#41374,#41375),(#41376,#41377),(#41378,
#41379),(#41380,#41381),(#41382,#41383),(#41384,#41385),(#41386,#41387),
(#41388,#41389),(#41390,#41391),(#41392,#41393),(#41394,#41395),(#41396,
#41397),(#41398,#41399),(#41400,#41401),(#41402,#41403)),.UNSPECIFIED.,
 .F.,.F.,.F.)
B_SPLINE_SURFACE_WITH_KNOTS((6,1,1,1,1,1,1,1,1,1,1,1,1,1,1,1,1,1,1,1,1,
1,1,1,1,1,1,1,1,1,1,1,1,1,1,1,1,1,1,1,1,1,1,1,1,1,1,1,1,1,1,1,1,1,1,1,1,
1,1,1,1,1,1,1,1,6),(2,2),(-1.,-0.984615384615383,-0.969230769230768,-0.953846153846152,
-0.938461538461537,-0.923076923076922,-0.907692307692306,-0.892307692307691,
-0.876923076923076,-0.86153846153846,-0.846153846153845,-0.83076923076923,
-0.815384615384614,-0.799999999999999,-0.784615384615384,-0.769230769230768,
-0.753846153846153,-0.738461538461538,-0.723076923076922,-0.707692307692307,
-0.692307692307692,-0.676923076923076,-0.661538461538461,-0.646153846153846,
-0.63076923076923,-0.615384615384615,-0.6,-0.584615384615384,-0.569230769230769,
-0.553846153846154,-0.538461538461538,-0.523076923076923,-0.507692307692308,
-0.492307692307692,-0.476923076923077,-0.461538461538462,-0.446153846153846,
-0.430769230769231,-0.415384615384615,-0.4,-0.384615384615385,-0.369230769230769,
-0.353846153846154,-0.338461538461538,-0.323076923076923,-0.307692307692308,
-0.292307692307692,-0.276923076923077,-0.261538461538462,-0.246153846153846,
-0.230769230769231,-0.215384615384615,-0.2,-0.184615384615385,-0.169230769230769,
-0.153846153846154,-0.138461538461538,-0.123076923076923,-0.107692307692308,
-0.0923076923076923,-0.0769230769230769,-0.0615384615384615,-0.0461538461538462,
-0.0307692307692308,-0.0153846153846154,0.),(-1.,1.),.UNSPECIFIED.)
GEOMETRIC_REPRESENTATION_ITEM()
RATIONAL_B_SPLINE_SURFACE(((1.,1.),(1.,1.),(1.,1.),(1.,1.),(1.,1.),(1.,
1.),(1.,1.),(1.,1.),(1.,1.),(1.,1.),(1.,1.),(1.,1.),(1.,1.),(1.,1.),(1.,
1.),(1.,1.),(1.,1.),(1.,1.),(1.,1.),(1.,1.),(1.,1.),(1.,1.),(1.,1.),(1.,
1.),(1.,1.),(1.,1.),(1.,1.),(1.,1.),(1.,1.),(1.,1.),(1.,1.),(1.,1.),(1.,
1.),(1.,1.),(1.,1.),(1.,1.),(1.,1.),(1.,1.),(1.,1.),(1.,1.),(1.,1.),(1.,
1.),(1.,1.),(1.,1.),(1.,1.),(1.,1.),(1.,1.),(1.,1.),(1.,1.),(1.,1.),(1.,
1.),(1.,1.),(1.,1.),(1.,1.),(1.,1.),(1.,1.),(1.,1.),(1.,1.),(1.,1.),(1.,
1.),(1.,1.),(1.,1.),(1.,1.),(1.,1.),(1.,1.),(1.,1.),(1.,1.),(1.,1.),(1.,
1.),(1.,1.)))
REPRESENTATION_ITEM('')
SURFACE()
);
#55=(
BOUNDED_SURFACE()
B_SPLINE_SURFACE(5,1,((#41480,#41481),(#41482,#41483),(#41484,#41485),(#41486,
#41487),(#41488,#41489),(#41490,#41491),(#41492,#41493),(#41494,#41495),
(#41496,#41497),(#41498,#41499),(#41500,#41501),(#41502,#41503),(#41504,
#41505),(#41506,#41507),(#41508,#41509),(#41510,#41511),(#41512,#41513),
(#41514,#41515),(#41516,#41517),(#41518,#41519),(#41520,#41521),(#41522,
#41523),(#41524,#41525),(#41526,#41527),(#41528,#41529),(#41530,#41531),
(#41532,#41533),(#41534,#41535),(#41536,#41537),(#41538,#41539),(#41540,
#41541),(#41542,#41543),(#41544,#41545),(#41546,#41547),(#41548,#41549),
(#41550,#41551),(#41552,#41553),(#41554,#41555),(#41556,#41557),(#41558,
#41559),(#41560,#41561),(#41562,#41563),(#41564,#41565),(#41566,#41567),
(#41568,#41569),(#41570,#41571),(#41572,#41573),(#41574,#41575),(#41576,
#41577),(#41578,#41579),(#41580,#41581),(#41582,#41583),(#41584,#41585),
(#41586,#41587),(#41588,#41589),(#41590,#41591),(#41592,#41593),(#41594,
#41595),(#41596,#41597),(#41598,#41599),(#41600,#41601),(#41602,#41603),
(#41604,#41605),(#41606,#41607),(#41608,#41609),(#41610,#41611),(#41612,
#41613),(#41614,#41615),(#41616,#41617),(#41618,#41619)),.UNSPECIFIED.,
 .F.,.F.,.F.)
B_SPLINE_SURFACE_WITH_KNOTS((6,1,1,1,1,1,1,1,1,1,1,1,1,1,1,1,1,1,1,1,1,
1,1,1,1,1,1,1,1,1,1,1,1,1,1,1,1,1,1,1,1,1,1,1,1,1,1,1,1,1,1,1,1,1,1,1,1,
1,1,1,1,1,1,1,1,6),(2,2),(-1.,-0.984615384615383,-0.969230769230768,-0.953846153846152,
-0.938461538461537,-0.923076923076922,-0.907692307692306,-0.892307692307691,
-0.876923076923076,-0.86153846153846,-0.846153846153845,-0.83076923076923,
-0.815384615384614,-0.799999999999999,-0.784615384615384,-0.769230769230768,
-0.753846153846153,-0.738461538461538,-0.723076923076922,-0.707692307692307,
-0.692307692307692,-0.676923076923076,-0.661538461538461,-0.646153846153846,
-0.63076923076923,-0.615384615384615,-0.6,-0.584615384615384,-0.569230769230769,
-0.553846153846154,-0.538461538461538,-0.523076923076923,-0.507692307692308,
-0.492307692307692,-0.476923076923077,-0.461538461538462,-0.446153846153846,
-0.430769230769231,-0.415384615384615,-0.4,-0.384615384615385,-0.369230769230769,
-0.353846153846154,-0.338461538461538,-0.323076923076923,-0.307692307692308,
-0.292307692307692,-0.276923076923077,-0.261538461538462,-0.246153846153846,
-0.230769230769231,-0.215384615384615,-0.2,-0.184615384615385,-0.169230769230769,
-0.153846153846154,-0.138461538461538,-0.123076923076923,-0.107692307692308,
-0.0923076923076923,-0.0769230769230769,-0.0615384615384615,-0.0461538461538462,
-0.0307692307692308,-0.0153846153846154,0.),(-1.,1.),.UNSPECIFIED.)
GEOMETRIC_REPRESENTATION_ITEM()
RATIONAL_B_SPLINE_SURFACE(((1.,1.),(1.,1.),(1.,1.),(1.,1.),(1.,1.),(1.,
1.),(1.,1.),(1.,1.),(1.,1.),(1.,1.),(1.,1.),(1.,1.),(1.,1.),(1.,1.),(1.,
1.),(1.,1.),(1.,1.),(1.,1.),(1.,1.),(1.,1.),(1.,1.),(1.,1.),(1.,1.),(1.,
1.),(1.,1.),(1.,1.),(1.,1.),(1.,1.),(1.,1.),(1.,1.),(1.,1.),(1.,1.),(1.,
1.),(1.,1.),(1.,1.),(1.,1.),(1.,1.),(1.,1.),(1.,1.),(1.,1.),(1.,1.),(1.,
1.),(1.,1.),(1.,1.),(1.,1.),(1.,1.),(1.,1.),(1.,1.),(1.,1.),(1.,1.),(1.,
1.),(1.,1.),(1.,1.),(1.,1.),(1.,1.),(1.,1.),(1.,1.),(1.,1.),(1.,1.),(1.,
1.),(1.,1.),(1.,1.),(1.,1.),(1.,1.),(1.,1.),(1.,1.),(1.,1.),(1.,1.),(1.,
1.),(1.,1.)))
REPRESENTATION_ITEM('')
SURFACE()
);
#56=(
BOUNDED_SURFACE()
B_SPLINE_SURFACE(5,1,((#41696,#41697),(#41698,#41699),(#41700,#41701),(#41702,
#41703),(#41704,#41705),(#41706,#41707),(#41708,#41709),(#41710,#41711),
(#41712,#41713),(#41714,#41715),(#41716,#41717),(#41718,#41719),(#41720,
#41721),(#41722,#41723),(#41724,#41725),(#41726,#41727),(#41728,#41729),
(#41730,#41731),(#41732,#41733),(#41734,#41735),(#41736,#41737),(#41738,
#41739),(#41740,#41741),(#41742,#41743),(#41744,#41745),(#41746,#41747),
(#41748,#41749),(#41750,#41751),(#41752,#41753),(#41754,#41755),(#41756,
#41757),(#41758,#41759),(#41760,#41761),(#41762,#41763),(#41764,#41765),
(#41766,#41767),(#41768,#41769),(#41770,#41771),(#41772,#41773),(#41774,
#41775),(#41776,#41777),(#41778,#41779),(#41780,#41781),(#41782,#41783),
(#41784,#41785),(#41786,#41787),(#41788,#41789),(#41790,#41791),(#41792,
#41793),(#41794,#41795),(#41796,#41797),(#41798,#41799),(#41800,#41801),
(#41802,#41803),(#41804,#41805),(#41806,#41807),(#41808,#41809),(#41810,
#41811),(#41812,#41813),(#41814,#41815),(#41816,#41817),(#41818,#41819),
(#41820,#41821),(#41822,#41823),(#41824,#41825),(#41826,#41827),(#41828,
#41829),(#41830,#41831),(#41832,#41833),(#41834,#41835)),.UNSPECIFIED.,
 .F.,.F.,.F.)
B_SPLINE_SURFACE_WITH_KNOTS((6,1,1,1,1,1,1,1,1,1,1,1,1,1,1,1,1,1,1,1,1,
1,1,1,1,1,1,1,1,1,1,1,1,1,1,1,1,1,1,1,1,1,1,1,1,1,1,1,1,1,1,1,1,1,1,1,1,
1,1,1,1,1,1,1,1,6),(2,2),(-1.,-0.984615384615383,-0.969230769230768,-0.953846153846152,
-0.938461538461537,-0.923076923076922,-0.907692307692306,-0.892307692307691,
-0.876923076923076,-0.86153846153846,-0.846153846153845,-0.83076923076923,
-0.815384615384614,-0.799999999999999,-0.784615384615384,-0.769230769230768,
-0.753846153846153,-0.738461538461538,-0.723076923076922,-0.707692307692307,
-0.692307692307692,-0.676923076923076,-0.661538461538461,-0.646153846153846,
-0.63076923076923,-0.615384615384615,-0.6,-0.584615384615384,-0.569230769230769,
-0.553846153846154,-0.538461538461538,-0.523076923076923,-0.507692307692308,
-0.492307692307692,-0.476923076923077,-0.461538461538462,-0.446153846153846,
-0.430769230769231,-0.415384615384615,-0.4,-0.384615384615385,-0.369230769230769,
-0.353846153846154,-0.338461538461538,-0.323076923076923,-0.307692307692308,
-0.292307692307692,-0.276923076923077,-0.261538461538462,-0.246153846153846,
-0.230769230769231,-0.215384615384615,-0.2,-0.184615384615385,-0.169230769230769,
-0.153846153846154,-0.138461538461538,-0.123076923076923,-0.107692307692308,
-0.0923076923076923,-0.0769230769230769,-0.0615384615384615,-0.0461538461538462,
-0.0307692307692308,-0.0153846153846154,0.),(-1.,1.),.UNSPECIFIED.)
GEOMETRIC_REPRESENTATION_ITEM()
RATIONAL_B_SPLINE_SURFACE(((1.,1.),(1.,1.),(1.,1.),(1.,1.),(1.,1.),(1.,
1.),(1.,1.),(1.,1.),(1.,1.),(1.,1.),(1.,1.),(1.,1.),(1.,1.),(1.,1.),(1.,
1.),(1.,1.),(1.,1.),(1.,1.),(1.,1.),(1.,1.),(1.,1.),(1.,1.),(1.,1.),(1.,
1.),(1.,1.),(1.,1.),(1.,1.),(1.,1.),(1.,1.),(1.,1.),(1.,1.),(1.,1.),(1.,
1.),(1.,1.),(1.,1.),(1.,1.),(1.,1.),(1.,1.),(1.,1.),(1.,1.),(1.,1.),(1.,
1.),(1.,1.),(1.,1.),(1.,1.),(1.,1.),(1.,1.),(1.,1.),(1.,1.),(1.,1.),(1.,
1.),(1.,1.),(1.,1.),(1.,1.),(1.,1.),(1.,1.),(1.,1.),(1.,1.),(1.,1.),(1.,
1.),(1.,1.),(1.,1.),(1.,1.),(1.,1.),(1.,1.),(1.,1.),(1.,1.),(1.,1.),(1.,
1.),(1.,1.)))
REPRESENTATION_ITEM('')
SURFACE()
);
#57=(
BOUNDED_SURFACE()
B_SPLINE_SURFACE(5,1,((#41912,#41913),(#41914,#41915),(#41916,#41917),(#41918,
#41919),(#41920,#41921),(#41922,#41923),(#41924,#41925),(#41926,#41927),
(#41928,#41929),(#41930,#41931),(#41932,#41933),(#41934,#41935),(#41936,
#41937),(#41938,#41939),(#41940,#41941),(#41942,#41943),(#41944,#41945),
(#41946,#41947),(#41948,#41949),(#41950,#41951),(#41952,#41953),(#41954,
#41955),(#41956,#41957),(#41958,#41959),(#41960,#41961),(#41962,#41963),
(#41964,#41965),(#41966,#41967),(#41968,#41969),(#41970,#41971),(#41972,
#41973),(#41974,#41975),(#41976,#41977),(#41978,#41979),(#41980,#41981),
(#41982,#41983),(#41984,#41985),(#41986,#41987),(#41988,#41989),(#41990,
#41991),(#41992,#41993),(#41994,#41995),(#41996,#41997),(#41998,#41999),
(#42000,#42001),(#42002,#42003),(#42004,#42005),(#42006,#42007),(#42008,
#42009),(#42010,#42011),(#42012,#42013),(#42014,#42015),(#42016,#42017),
(#42018,#42019),(#42020,#42021),(#42022,#42023),(#42024,#42025),(#42026,
#42027),(#42028,#42029),(#42030,#42031),(#42032,#42033),(#42034,#42035),
(#42036,#42037),(#42038,#42039),(#42040,#42041),(#42042,#42043),(#42044,
#42045),(#42046,#42047),(#42048,#42049),(#42050,#42051)),.UNSPECIFIED.,
 .F.,.F.,.F.)
B_SPLINE_SURFACE_WITH_KNOTS((6,1,1,1,1,1,1,1,1,1,1,1,1,1,1,1,1,1,1,1,1,
1,1,1,1,1,1,1,1,1,1,1,1,1,1,1,1,1,1,1,1,1,1,1,1,1,1,1,1,1,1,1,1,1,1,1,1,
1,1,1,1,1,1,1,1,6),(2,2),(-1.,-0.984615384615383,-0.969230769230768,-0.953846153846152,
-0.938461538461537,-0.923076923076922,-0.907692307692306,-0.892307692307691,
-0.876923076923076,-0.86153846153846,-0.846153846153845,-0.83076923076923,
-0.815384615384614,-0.799999999999999,-0.784615384615384,-0.769230769230768,
-0.753846153846153,-0.738461538461538,-0.723076923076922,-0.707692307692307,
-0.692307692307692,-0.676923076923076,-0.661538461538461,-0.646153846153846,
-0.63076923076923,-0.615384615384615,-0.6,-0.584615384615384,-0.569230769230769,
-0.553846153846154,-0.538461538461538,-0.523076923076923,-0.507692307692308,
-0.492307692307692,-0.476923076923077,-0.461538461538462,-0.446153846153846,
-0.430769230769231,-0.415384615384615,-0.4,-0.384615384615385,-0.369230769230769,
-0.353846153846154,-0.338461538461538,-0.323076923076923,-0.307692307692308,
-0.292307692307692,-0.276923076923077,-0.261538461538462,-0.246153846153846,
-0.230769230769231,-0.215384615384615,-0.2,-0.184615384615385,-0.169230769230769,
-0.153846153846154,-0.138461538461538,-0.123076923076923,-0.107692307692308,
-0.0923076923076923,-0.0769230769230769,-0.0615384615384615,-0.0461538461538462,
-0.0307692307692308,-0.0153846153846154,0.),(-1.,1.),.UNSPECIFIED.)
GEOMETRIC_REPRESENTATION_ITEM()
RATIONAL_B_SPLINE_SURFACE(((1.,1.),(1.,1.),(1.,1.),(1.,1.),(1.,1.),(1.,
1.),(1.,1.),(1.,1.),(1.,1.),(1.,1.),(1.,1.),(1.,1.),(1.,1.),(1.,1.),(1.,
1.),(1.,1.),(1.,1.),(1.,1.),(1.,1.),(1.,1.),(1.,1.),(1.,1.),(1.,1.),(1.,
1.),(1.,1.),(1.,1.),(1.,1.),(1.,1.),(1.,1.),(1.,1.),(1.,1.),(1.,1.),(1.,
1.),(1.,1.),(1.,1.),(1.,1.),(1.,1.),(1.,1.),(1.,1.),(1.,1.),(1.,1.),(1.,
1.),(1.,1.),(1.,1.),(1.,1.),(1.,1.),(1.,1.),(1.,1.),(1.,1.),(1.,1.),(1.,
1.),(1.,1.),(1.,1.),(1.,1.),(1.,1.),(1.,1.),(1.,1.),(1.,1.),(1.,1.),(1.,
1.),(1.,1.),(1.,1.),(1.,1.),(1.,1.),(1.,1.),(1.,1.),(1.,1.),(1.,1.),(1.,
1.),(1.,1.)))
REPRESENTATION_ITEM('')
SURFACE()
);
#58=(
BOUNDED_SURFACE()
B_SPLINE_SURFACE(5,1,((#42128,#42129),(#42130,#42131),(#42132,#42133),(#42134,
#42135),(#42136,#42137),(#42138,#42139),(#42140,#42141),(#42142,#42143),
(#42144,#42145),(#42146,#42147),(#42148,#42149),(#42150,#42151),(#42152,
#42153),(#42154,#42155),(#42156,#42157),(#42158,#42159),(#42160,#42161),
(#42162,#42163),(#42164,#42165),(#42166,#42167),(#42168,#42169),(#42170,
#42171),(#42172,#42173),(#42174,#42175),(#42176,#42177),(#42178,#42179),
(#42180,#42181),(#42182,#42183),(#42184,#42185),(#42186,#42187),(#42188,
#42189),(#42190,#42191),(#42192,#42193),(#42194,#42195),(#42196,#42197),
(#42198,#42199),(#42200,#42201),(#42202,#42203),(#42204,#42205),(#42206,
#42207),(#42208,#42209),(#42210,#42211),(#42212,#42213),(#42214,#42215),
(#42216,#42217),(#42218,#42219),(#42220,#42221),(#42222,#42223),(#42224,
#42225),(#42226,#42227),(#42228,#42229),(#42230,#42231),(#42232,#42233),
(#42234,#42235),(#42236,#42237),(#42238,#42239),(#42240,#42241),(#42242,
#42243),(#42244,#42245),(#42246,#42247),(#42248,#42249),(#42250,#42251),
(#42252,#42253),(#42254,#42255),(#42256,#42257),(#42258,#42259),(#42260,
#42261),(#42262,#42263),(#42264,#42265),(#42266,#42267)),.UNSPECIFIED.,
 .F.,.F.,.F.)
B_SPLINE_SURFACE_WITH_KNOTS((6,1,1,1,1,1,1,1,1,1,1,1,1,1,1,1,1,1,1,1,1,
1,1,1,1,1,1,1,1,1,1,1,1,1,1,1,1,1,1,1,1,1,1,1,1,1,1,1,1,1,1,1,1,1,1,1,1,
1,1,1,1,1,1,1,1,6),(2,2),(-1.,-0.984615384615383,-0.969230769230768,-0.953846153846152,
-0.938461538461537,-0.923076923076922,-0.907692307692306,-0.892307692307691,
-0.876923076923076,-0.86153846153846,-0.846153846153845,-0.83076923076923,
-0.815384615384614,-0.799999999999999,-0.784615384615384,-0.769230769230768,
-0.753846153846153,-0.738461538461538,-0.723076923076922,-0.707692307692307,
-0.692307692307692,-0.676923076923076,-0.661538461538461,-0.646153846153846,
-0.63076923076923,-0.615384615384615,-0.6,-0.584615384615384,-0.569230769230769,
-0.553846153846154,-0.538461538461538,-0.523076923076923,-0.507692307692308,
-0.492307692307692,-0.476923076923077,-0.461538461538462,-0.446153846153846,
-0.430769230769231,-0.415384615384615,-0.4,-0.384615384615385,-0.369230769230769,
-0.353846153846154,-0.338461538461538,-0.323076923076923,-0.307692307692308,
-0.292307692307692,-0.276923076923077,-0.261538461538462,-0.246153846153846,
-0.230769230769231,-0.215384615384615,-0.2,-0.184615384615385,-0.169230769230769,
-0.153846153846154,-0.138461538461538,-0.123076923076923,-0.107692307692308,
-0.0923076923076923,-0.0769230769230769,-0.0615384615384615,-0.0461538461538462,
-0.0307692307692308,-0.0153846153846154,0.),(-1.,1.),.UNSPECIFIED.)
GEOMETRIC_REPRESENTATION_ITEM()
RATIONAL_B_SPLINE_SURFACE(((1.,1.),(1.,1.),(1.,1.),(1.,1.),(1.,1.),(1.,
1.),(1.,1.),(1.,1.),(1.,1.),(1.,1.),(1.,1.),(1.,1.),(1.,1.),(1.,1.),(1.,
1.),(1.,1.),(1.,1.),(1.,1.),(1.,1.),(1.,1.),(1.,1.),(1.,1.),(1.,1.),(1.,
1.),(1.,1.),(1.,1.),(1.,1.),(1.,1.),(1.,1.),(1.,1.),(1.,1.),(1.,1.),(1.,
1.),(1.,1.),(1.,1.),(1.,1.),(1.,1.),(1.,1.),(1.,1.),(1.,1.),(1.,1.),(1.,
1.),(1.,1.),(1.,1.),(1.,1.),(1.,1.),(1.,1.),(1.,1.),(1.,1.),(1.,1.),(1.,
1.),(1.,1.),(1.,1.),(1.,1.),(1.,1.),(1.,1.),(1.,1.),(1.,1.),(1.,1.),(1.,
1.),(1.,1.),(1.,1.),(1.,1.),(1.,1.),(1.,1.),(1.,1.),(1.,1.),(1.,1.),(1.,
1.),(1.,1.)))
REPRESENTATION_ITEM('')
SURFACE()
);
#59=(
BOUNDED_SURFACE()
B_SPLINE_SURFACE(5,1,((#42344,#42345),(#42346,#42347),(#42348,#42349),(#42350,
#42351),(#42352,#42353),(#42354,#42355),(#42356,#42357),(#42358,#42359),
(#42360,#42361),(#42362,#42363),(#42364,#42365),(#42366,#42367),(#42368,
#42369),(#42370,#42371),(#42372,#42373),(#42374,#42375),(#42376,#42377),
(#42378,#42379),(#42380,#42381),(#42382,#42383),(#42384,#42385),(#42386,
#42387),(#42388,#42389),(#42390,#42391),(#42392,#42393),(#42394,#42395),
(#42396,#42397),(#42398,#42399),(#42400,#42401),(#42402,#42403),(#42404,
#42405),(#42406,#42407),(#42408,#42409),(#42410,#42411),(#42412,#42413),
(#42414,#42415),(#42416,#42417),(#42418,#42419),(#42420,#42421),(#42422,
#42423),(#42424,#42425),(#42426,#42427),(#42428,#42429),(#42430,#42431),
(#42432,#42433),(#42434,#42435),(#42436,#42437),(#42438,#42439),(#42440,
#42441),(#42442,#42443),(#42444,#42445),(#42446,#42447),(#42448,#42449),
(#42450,#42451),(#42452,#42453),(#42454,#42455),(#42456,#42457),(#42458,
#42459),(#42460,#42461),(#42462,#42463),(#42464,#42465),(#42466,#42467),
(#42468,#42469),(#42470,#42471),(#42472,#42473),(#42474,#42475),(#42476,
#42477),(#42478,#42479),(#42480,#42481),(#42482,#42483)),.UNSPECIFIED.,
 .F.,.F.,.F.)
B_SPLINE_SURFACE_WITH_KNOTS((6,1,1,1,1,1,1,1,1,1,1,1,1,1,1,1,1,1,1,1,1,
1,1,1,1,1,1,1,1,1,1,1,1,1,1,1,1,1,1,1,1,1,1,1,1,1,1,1,1,1,1,1,1,1,1,1,1,
1,1,1,1,1,1,1,1,6),(2,2),(-1.,-0.984615384615383,-0.969230769230768,-0.953846153846152,
-0.938461538461537,-0.923076923076922,-0.907692307692306,-0.892307692307691,
-0.876923076923076,-0.86153846153846,-0.846153846153845,-0.83076923076923,
-0.815384615384614,-0.799999999999999,-0.784615384615384,-0.769230769230768,
-0.753846153846153,-0.738461538461538,-0.723076923076922,-0.707692307692307,
-0.692307692307692,-0.676923076923076,-0.661538461538461,-0.646153846153846,
-0.63076923076923,-0.615384615384615,-0.6,-0.584615384615384,-0.569230769230769,
-0.553846153846154,-0.538461538461538,-0.523076923076923,-0.507692307692308,
-0.492307692307692,-0.476923076923077,-0.461538461538462,-0.446153846153846,
-0.430769230769231,-0.415384615384615,-0.4,-0.384615384615385,-0.369230769230769,
-0.353846153846154,-0.338461538461538,-0.323076923076923,-0.307692307692308,
-0.292307692307692,-0.276923076923077,-0.261538461538462,-0.246153846153846,
-0.230769230769231,-0.215384615384615,-0.2,-0.184615384615385,-0.169230769230769,
-0.153846153846154,-0.138461538461538,-0.123076923076923,-0.107692307692308,
-0.0923076923076923,-0.0769230769230769,-0.0615384615384615,-0.0461538461538462,
-0.0307692307692308,-0.0153846153846154,0.),(-1.,1.),.UNSPECIFIED.)
GEOMETRIC_REPRESENTATION_ITEM()
RATIONAL_B_SPLINE_SURFACE(((1.,1.),(1.,1.),(1.,1.),(1.,1.),(1.,1.),(1.,
1.),(1.,1.),(1.,1.),(1.,1.),(1.,1.),(1.,1.),(1.,1.),(1.,1.),(1.,1.),(1.,
1.),(1.,1.),(1.,1.),(1.,1.),(1.,1.),(1.,1.),(1.,1.),(1.,1.),(1.,1.),(1.,
1.),(1.,1.),(1.,1.),(1.,1.),(1.,1.),(1.,1.),(1.,1.),(1.,1.),(1.,1.),(1.,
1.),(1.,1.),(1.,1.),(1.,1.),(1.,1.),(1.,1.),(1.,1.),(1.,1.),(1.,1.),(1.,
1.),(1.,1.),(1.,1.),(1.,1.),(1.,1.),(1.,1.),(1.,1.),(1.,1.),(1.,1.),(1.,
1.),(1.,1.),(1.,1.),(1.,1.),(1.,1.),(1.,1.),(1.,1.),(1.,1.),(1.,1.),(1.,
1.),(1.,1.),(1.,1.),(1.,1.),(1.,1.),(1.,1.),(1.,1.),(1.,1.),(1.,1.),(1.,
1.),(1.,1.)))
REPRESENTATION_ITEM('')
SURFACE()
);
#60=(
BOUNDED_SURFACE()
B_SPLINE_SURFACE(5,1,((#42560,#42561),(#42562,#42563),(#42564,#42565),(#42566,
#42567),(#42568,#42569),(#42570,#42571),(#42572,#42573),(#42574,#42575),
(#42576,#42577),(#42578,#42579),(#42580,#42581),(#42582,#42583),(#42584,
#42585),(#42586,#42587),(#42588,#42589),(#42590,#42591),(#42592,#42593),
(#42594,#42595),(#42596,#42597),(#42598,#42599),(#42600,#42601),(#42602,
#42603),(#42604,#42605),(#42606,#42607),(#42608,#42609),(#42610,#42611),
(#42612,#42613),(#42614,#42615),(#42616,#42617),(#42618,#42619),(#42620,
#42621),(#42622,#42623),(#42624,#42625),(#42626,#42627),(#42628,#42629),
(#42630,#42631),(#42632,#42633),(#42634,#42635),(#42636,#42637),(#42638,
#42639),(#42640,#42641),(#42642,#42643),(#42644,#42645),(#42646,#42647),
(#42648,#42649),(#42650,#42651),(#42652,#42653),(#42654,#42655),(#42656,
#42657),(#42658,#42659),(#42660,#42661),(#42662,#42663),(#42664,#42665),
(#42666,#42667),(#42668,#42669),(#42670,#42671),(#42672,#42673),(#42674,
#42675),(#42676,#42677),(#42678,#42679),(#42680,#42681),(#42682,#42683),
(#42684,#42685),(#42686,#42687),(#42688,#42689),(#42690,#42691),(#42692,
#42693),(#42694,#42695),(#42696,#42697),(#42698,#42699)),.UNSPECIFIED.,
 .F.,.F.,.F.)
B_SPLINE_SURFACE_WITH_KNOTS((6,1,1,1,1,1,1,1,1,1,1,1,1,1,1,1,1,1,1,1,1,
1,1,1,1,1,1,1,1,1,1,1,1,1,1,1,1,1,1,1,1,1,1,1,1,1,1,1,1,1,1,1,1,1,1,1,1,
1,1,1,1,1,1,1,1,6),(2,2),(-1.,-0.984615384615383,-0.969230769230768,-0.953846153846152,
-0.938461538461537,-0.923076923076922,-0.907692307692306,-0.892307692307691,
-0.876923076923076,-0.86153846153846,-0.846153846153845,-0.83076923076923,
-0.815384615384614,-0.799999999999999,-0.784615384615384,-0.769230769230768,
-0.753846153846153,-0.738461538461538,-0.723076923076922,-0.707692307692307,
-0.692307692307692,-0.676923076923076,-0.661538461538461,-0.646153846153846,
-0.63076923076923,-0.615384615384615,-0.6,-0.584615384615384,-0.569230769230769,
-0.553846153846154,-0.538461538461538,-0.523076923076923,-0.507692307692308,
-0.492307692307692,-0.476923076923077,-0.461538461538462,-0.446153846153846,
-0.430769230769231,-0.415384615384615,-0.4,-0.384615384615385,-0.369230769230769,
-0.353846153846154,-0.338461538461538,-0.323076923076923,-0.307692307692308,
-0.292307692307692,-0.276923076923077,-0.261538461538462,-0.246153846153846,
-0.230769230769231,-0.215384615384615,-0.2,-0.184615384615385,-0.169230769230769,
-0.153846153846154,-0.138461538461538,-0.123076923076923,-0.107692307692308,
-0.0923076923076923,-0.0769230769230769,-0.0615384615384615,-0.0461538461538462,
-0.0307692307692308,-0.0153846153846154,0.),(-1.,1.),.UNSPECIFIED.)
GEOMETRIC_REPRESENTATION_ITEM()
RATIONAL_B_SPLINE_SURFACE(((1.,1.),(1.,1.),(1.,1.),(1.,1.),(1.,1.),(1.,
1.),(1.,1.),(1.,1.),(1.,1.),(1.,1.),(1.,1.),(1.,1.),(1.,1.),(1.,1.),(1.,
1.),(1.,1.),(1.,1.),(1.,1.),(1.,1.),(1.,1.),(1.,1.),(1.,1.),(1.,1.),(1.,
1.),(1.,1.),(1.,1.),(1.,1.),(1.,1.),(1.,1.),(1.,1.),(1.,1.),(1.,1.),(1.,
1.),(1.,1.),(1.,1.),(1.,1.),(1.,1.),(1.,1.),(1.,1.),(1.,1.),(1.,1.),(1.,
1.),(1.,1.),(1.,1.),(1.,1.),(1.,1.),(1.,1.),(1.,1.),(1.,1.),(1.,1.),(1.,
1.),(1.,1.),(1.,1.),(1.,1.),(1.,1.),(1.,1.),(1.,1.),(1.,1.),(1.,1.),(1.,
1.),(1.,1.),(1.,1.),(1.,1.),(1.,1.),(1.,1.),(1.,1.),(1.,1.),(1.,1.),(1.,
1.),(1.,1.)))
REPRESENTATION_ITEM('')
SURFACE()
);
#61=(
BOUNDED_SURFACE()
B_SPLINE_SURFACE(5,1,((#42776,#42777),(#42778,#42779),(#42780,#42781),(#42782,
#42783),(#42784,#42785),(#42786,#42787),(#42788,#42789),(#42790,#42791),
(#42792,#42793),(#42794,#42795),(#42796,#42797),(#42798,#42799),(#42800,
#42801),(#42802,#42803),(#42804,#42805),(#42806,#42807),(#42808,#42809),
(#42810,#42811),(#42812,#42813),(#42814,#42815),(#42816,#42817),(#42818,
#42819),(#42820,#42821),(#42822,#42823),(#42824,#42825),(#42826,#42827),
(#42828,#42829),(#42830,#42831),(#42832,#42833),(#42834,#42835),(#42836,
#42837),(#42838,#42839),(#42840,#42841),(#42842,#42843),(#42844,#42845),
(#42846,#42847),(#42848,#42849),(#42850,#42851),(#42852,#42853),(#42854,
#42855),(#42856,#42857),(#42858,#42859),(#42860,#42861),(#42862,#42863),
(#42864,#42865),(#42866,#42867),(#42868,#42869),(#42870,#42871),(#42872,
#42873),(#42874,#42875),(#42876,#42877),(#42878,#42879),(#42880,#42881),
(#42882,#42883),(#42884,#42885),(#42886,#42887),(#42888,#42889),(#42890,
#42891),(#42892,#42893),(#42894,#42895),(#42896,#42897),(#42898,#42899),
(#42900,#42901),(#42902,#42903),(#42904,#42905),(#42906,#42907),(#42908,
#42909),(#42910,#42911),(#42912,#42913),(#42914,#42915)),.UNSPECIFIED.,
 .F.,.F.,.F.)
B_SPLINE_SURFACE_WITH_KNOTS((6,1,1,1,1,1,1,1,1,1,1,1,1,1,1,1,1,1,1,1,1,
1,1,1,1,1,1,1,1,1,1,1,1,1,1,1,1,1,1,1,1,1,1,1,1,1,1,1,1,1,1,1,1,1,1,1,1,
1,1,1,1,1,1,1,1,6),(2,2),(-1.,-0.984615384615383,-0.969230769230768,-0.953846153846152,
-0.938461538461537,-0.923076923076922,-0.907692307692306,-0.892307692307691,
-0.876923076923076,-0.86153846153846,-0.846153846153845,-0.83076923076923,
-0.815384615384614,-0.799999999999999,-0.784615384615384,-0.769230769230768,
-0.753846153846153,-0.738461538461538,-0.723076923076922,-0.707692307692307,
-0.692307692307692,-0.676923076923076,-0.661538461538461,-0.646153846153846,
-0.63076923076923,-0.615384615384615,-0.6,-0.584615384615384,-0.569230769230769,
-0.553846153846154,-0.538461538461538,-0.523076923076923,-0.507692307692308,
-0.492307692307692,-0.476923076923077,-0.461538461538462,-0.446153846153846,
-0.430769230769231,-0.415384615384615,-0.4,-0.384615384615385,-0.369230769230769,
-0.353846153846154,-0.338461538461538,-0.323076923076923,-0.307692307692308,
-0.292307692307692,-0.276923076923077,-0.261538461538462,-0.246153846153846,
-0.230769230769231,-0.215384615384615,-0.2,-0.184615384615385,-0.169230769230769,
-0.153846153846154,-0.138461538461538,-0.123076923076923,-0.107692307692308,
-0.0923076923076923,-0.0769230769230769,-0.0615384615384615,-0.0461538461538462,
-0.0307692307692308,-0.0153846153846154,0.),(-1.,1.),.UNSPECIFIED.)
GEOMETRIC_REPRESENTATION_ITEM()
RATIONAL_B_SPLINE_SURFACE(((1.,1.),(1.,1.),(1.,1.),(1.,1.),(1.,1.),(1.,
1.),(1.,1.),(1.,1.),(1.,1.),(1.,1.),(1.,1.),(1.,1.),(1.,1.),(1.,1.),(1.,
1.),(1.,1.),(1.,1.),(1.,1.),(1.,1.),(1.,1.),(1.,1.),(1.,1.),(1.,1.),(1.,
1.),(1.,1.),(1.,1.),(1.,1.),(1.,1.),(1.,1.),(1.,1.),(1.,1.),(1.,1.),(1.,
1.),(1.,1.),(1.,1.),(1.,1.),(1.,1.),(1.,1.),(1.,1.),(1.,1.),(1.,1.),(1.,
1.),(1.,1.),(1.,1.),(1.,1.),(1.,1.),(1.,1.),(1.,1.),(1.,1.),(1.,1.),(1.,
1.),(1.,1.),(1.,1.),(1.,1.),(1.,1.),(1.,1.),(1.,1.),(1.,1.),(1.,1.),(1.,
1.),(1.,1.),(1.,1.),(1.,1.),(1.,1.),(1.,1.),(1.,1.),(1.,1.),(1.,1.),(1.,
1.),(1.,1.)))
REPRESENTATION_ITEM('')
SURFACE()
);
#62=(
BOUNDED_SURFACE()
B_SPLINE_SURFACE(5,1,((#42992,#42993),(#42994,#42995),(#42996,#42997),(#42998,
#42999),(#43000,#43001),(#43002,#43003),(#43004,#43005),(#43006,#43007),
(#43008,#43009),(#43010,#43011),(#43012,#43013),(#43014,#43015),(#43016,
#43017),(#43018,#43019),(#43020,#43021),(#43022,#43023),(#43024,#43025),
(#43026,#43027),(#43028,#43029),(#43030,#43031),(#43032,#43033),(#43034,
#43035),(#43036,#43037),(#43038,#43039),(#43040,#43041),(#43042,#43043),
(#43044,#43045),(#43046,#43047),(#43048,#43049),(#43050,#43051),(#43052,
#43053),(#43054,#43055),(#43056,#43057),(#43058,#43059),(#43060,#43061),
(#43062,#43063),(#43064,#43065),(#43066,#43067),(#43068,#43069),(#43070,
#43071),(#43072,#43073),(#43074,#43075),(#43076,#43077),(#43078,#43079),
(#43080,#43081),(#43082,#43083),(#43084,#43085),(#43086,#43087),(#43088,
#43089),(#43090,#43091),(#43092,#43093),(#43094,#43095),(#43096,#43097),
(#43098,#43099),(#43100,#43101),(#43102,#43103),(#43104,#43105),(#43106,
#43107),(#43108,#43109),(#43110,#43111),(#43112,#43113),(#43114,#43115),
(#43116,#43117),(#43118,#43119),(#43120,#43121),(#43122,#43123),(#43124,
#43125),(#43126,#43127),(#43128,#43129),(#43130,#43131)),.UNSPECIFIED.,
 .F.,.F.,.F.)
B_SPLINE_SURFACE_WITH_KNOTS((6,1,1,1,1,1,1,1,1,1,1,1,1,1,1,1,1,1,1,1,1,
1,1,1,1,1,1,1,1,1,1,1,1,1,1,1,1,1,1,1,1,1,1,1,1,1,1,1,1,1,1,1,1,1,1,1,1,
1,1,1,1,1,1,1,1,6),(2,2),(-1.,-0.984615384615383,-0.969230769230768,-0.953846153846152,
-0.938461538461537,-0.923076923076922,-0.907692307692306,-0.892307692307691,
-0.876923076923076,-0.86153846153846,-0.846153846153845,-0.83076923076923,
-0.815384615384614,-0.799999999999999,-0.784615384615384,-0.769230769230768,
-0.753846153846153,-0.738461538461538,-0.723076923076922,-0.707692307692307,
-0.692307692307692,-0.676923076923076,-0.661538461538461,-0.646153846153846,
-0.63076923076923,-0.615384615384615,-0.6,-0.584615384615384,-0.569230769230769,
-0.553846153846154,-0.538461538461538,-0.523076923076923,-0.507692307692308,
-0.492307692307692,-0.476923076923077,-0.461538461538462,-0.446153846153846,
-0.430769230769231,-0.415384615384615,-0.4,-0.384615384615385,-0.369230769230769,
-0.353846153846154,-0.338461538461538,-0.323076923076923,-0.307692307692308,
-0.292307692307692,-0.276923076923077,-0.261538461538462,-0.246153846153846,
-0.230769230769231,-0.215384615384615,-0.2,-0.184615384615385,-0.169230769230769,
-0.153846153846154,-0.138461538461538,-0.123076923076923,-0.107692307692308,
-0.0923076923076923,-0.0769230769230769,-0.0615384615384615,-0.0461538461538462,
-0.0307692307692308,-0.0153846153846154,0.),(-1.,1.),.UNSPECIFIED.)
GEOMETRIC_REPRESENTATION_ITEM()
RATIONAL_B_SPLINE_SURFACE(((1.,1.),(1.,1.),(1.,1.),(1.,1.),(1.,1.),(1.,
1.),(1.,1.),(1.,1.),(1.,1.),(1.,1.),(1.,1.),(1.,1.),(1.,1.),(1.,1.),(1.,
1.),(1.,1.),(1.,1.),(1.,1.),(1.,1.),(1.,1.),(1.,1.),(1.,1.),(1.,1.),(1.,
1.),(1.,1.),(1.,1.),(1.,1.),(1.,1.),(1.,1.),(1.,1.),(1.,1.),(1.,1.),(1.,
1.),(1.,1.),(1.,1.),(1.,1.),(1.,1.),(1.,1.),(1.,1.),(1.,1.),(1.,1.),(1.,
1.),(1.,1.),(1.,1.),(1.,1.),(1.,1.),(1.,1.),(1.,1.),(1.,1.),(1.,1.),(1.,
1.),(1.,1.),(1.,1.),(1.,1.),(1.,1.),(1.,1.),(1.,1.),(1.,1.),(1.,1.),(1.,
1.),(1.,1.),(1.,1.),(1.,1.),(1.,1.),(1.,1.),(1.,1.),(1.,1.),(1.,1.),(1.,
1.),(1.,1.)))
REPRESENTATION_ITEM('')
SURFACE()
);
#63=(
BOUNDED_SURFACE()
B_SPLINE_SURFACE(5,1,((#43208,#43209),(#43210,#43211),(#43212,#43213),(#43214,
#43215),(#43216,#43217),(#43218,#43219),(#43220,#43221),(#43222,#43223),
(#43224,#43225),(#43226,#43227),(#43228,#43229),(#43230,#43231),(#43232,
#43233),(#43234,#43235),(#43236,#43237),(#43238,#43239),(#43240,#43241),
(#43242,#43243),(#43244,#43245),(#43246,#43247),(#43248,#43249),(#43250,
#43251),(#43252,#43253),(#43254,#43255),(#43256,#43257),(#43258,#43259),
(#43260,#43261),(#43262,#43263),(#43264,#43265),(#43266,#43267),(#43268,
#43269),(#43270,#43271),(#43272,#43273),(#43274,#43275),(#43276,#43277),
(#43278,#43279),(#43280,#43281),(#43282,#43283),(#43284,#43285),(#43286,
#43287),(#43288,#43289),(#43290,#43291),(#43292,#43293),(#43294,#43295),
(#43296,#43297),(#43298,#43299),(#43300,#43301),(#43302,#43303),(#43304,
#43305),(#43306,#43307),(#43308,#43309),(#43310,#43311),(#43312,#43313),
(#43314,#43315),(#43316,#43317),(#43318,#43319),(#43320,#43321),(#43322,
#43323),(#43324,#43325),(#43326,#43327),(#43328,#43329),(#43330,#43331),
(#43332,#43333),(#43334,#43335),(#43336,#43337),(#43338,#43339),(#43340,
#43341),(#43342,#43343),(#43344,#43345),(#43346,#43347)),.UNSPECIFIED.,
 .F.,.F.,.F.)
B_SPLINE_SURFACE_WITH_KNOTS((6,1,1,1,1,1,1,1,1,1,1,1,1,1,1,1,1,1,1,1,1,
1,1,1,1,1,1,1,1,1,1,1,1,1,1,1,1,1,1,1,1,1,1,1,1,1,1,1,1,1,1,1,1,1,1,1,1,
1,1,1,1,1,1,1,1,6),(2,2),(-1.,-0.984615384615383,-0.969230769230768,-0.953846153846152,
-0.938461538461537,-0.923076923076922,-0.907692307692306,-0.892307692307691,
-0.876923076923076,-0.86153846153846,-0.846153846153845,-0.83076923076923,
-0.815384615384614,-0.799999999999999,-0.784615384615384,-0.769230769230768,
-0.753846153846153,-0.738461538461538,-0.723076923076922,-0.707692307692307,
-0.692307692307692,-0.676923076923076,-0.661538461538461,-0.646153846153846,
-0.63076923076923,-0.615384615384615,-0.6,-0.584615384615384,-0.569230769230769,
-0.553846153846154,-0.538461538461538,-0.523076923076923,-0.507692307692308,
-0.492307692307692,-0.476923076923077,-0.461538461538462,-0.446153846153846,
-0.430769230769231,-0.415384615384615,-0.4,-0.384615384615385,-0.369230769230769,
-0.353846153846154,-0.338461538461538,-0.323076923076923,-0.307692307692308,
-0.292307692307692,-0.276923076923077,-0.261538461538462,-0.246153846153846,
-0.230769230769231,-0.215384615384615,-0.2,-0.184615384615385,-0.169230769230769,
-0.153846153846154,-0.138461538461538,-0.123076923076923,-0.107692307692308,
-0.0923076923076923,-0.0769230769230769,-0.0615384615384615,-0.0461538461538462,
-0.0307692307692308,-0.0153846153846154,0.),(-1.,1.),.UNSPECIFIED.)
GEOMETRIC_REPRESENTATION_ITEM()
RATIONAL_B_SPLINE_SURFACE(((1.,1.),(1.,1.),(1.,1.),(1.,1.),(1.,1.),(1.,
1.),(1.,1.),(1.,1.),(1.,1.),(1.,1.),(1.,1.),(1.,1.),(1.,1.),(1.,1.),(1.,
1.),(1.,1.),(1.,1.),(1.,1.),(1.,1.),(1.,1.),(1.,1.),(1.,1.),(1.,1.),(1.,
1.),(1.,1.),(1.,1.),(1.,1.),(1.,1.),(1.,1.),(1.,1.),(1.,1.),(1.,1.),(1.,
1.),(1.,1.),(1.,1.),(1.,1.),(1.,1.),(1.,1.),(1.,1.),(1.,1.),(1.,1.),(1.,
1.),(1.,1.),(1.,1.),(1.,1.),(1.,1.),(1.,1.),(1.,1.),(1.,1.),(1.,1.),(1.,
1.),(1.,1.),(1.,1.),(1.,1.),(1.,1.),(1.,1.),(1.,1.),(1.,1.),(1.,1.),(1.,
1.),(1.,1.),(1.,1.),(1.,1.),(1.,1.),(1.,1.),(1.,1.),(1.,1.),(1.,1.),(1.,
1.),(1.,1.)))
REPRESENTATION_ITEM('')
SURFACE()
);
#64=(
BOUNDED_SURFACE()
B_SPLINE_SURFACE(5,1,((#43424,#43425),(#43426,#43427),(#43428,#43429),(#43430,
#43431),(#43432,#43433),(#43434,#43435),(#43436,#43437),(#43438,#43439),
(#43440,#43441),(#43442,#43443),(#43444,#43445),(#43446,#43447),(#43448,
#43449),(#43450,#43451),(#43452,#43453),(#43454,#43455),(#43456,#43457),
(#43458,#43459),(#43460,#43461),(#43462,#43463),(#43464,#43465),(#43466,
#43467),(#43468,#43469),(#43470,#43471),(#43472,#43473),(#43474,#43475),
(#43476,#43477),(#43478,#43479),(#43480,#43481),(#43482,#43483),(#43484,
#43485),(#43486,#43487),(#43488,#43489),(#43490,#43491),(#43492,#43493),
(#43494,#43495),(#43496,#43497),(#43498,#43499),(#43500,#43501),(#43502,
#43503),(#43504,#43505),(#43506,#43507),(#43508,#43509),(#43510,#43511),
(#43512,#43513),(#43514,#43515),(#43516,#43517),(#43518,#43519),(#43520,
#43521),(#43522,#43523),(#43524,#43525),(#43526,#43527),(#43528,#43529),
(#43530,#43531),(#43532,#43533),(#43534,#43535),(#43536,#43537),(#43538,
#43539),(#43540,#43541),(#43542,#43543),(#43544,#43545),(#43546,#43547),
(#43548,#43549),(#43550,#43551),(#43552,#43553),(#43554,#43555),(#43556,
#43557),(#43558,#43559),(#43560,#43561),(#43562,#43563)),.UNSPECIFIED.,
 .F.,.F.,.F.)
B_SPLINE_SURFACE_WITH_KNOTS((6,1,1,1,1,1,1,1,1,1,1,1,1,1,1,1,1,1,1,1,1,
1,1,1,1,1,1,1,1,1,1,1,1,1,1,1,1,1,1,1,1,1,1,1,1,1,1,1,1,1,1,1,1,1,1,1,1,
1,1,1,1,1,1,1,1,6),(2,2),(-1.,-0.984615384615383,-0.969230769230768,-0.953846153846152,
-0.938461538461537,-0.923076923076922,-0.907692307692306,-0.892307692307691,
-0.876923076923076,-0.86153846153846,-0.846153846153845,-0.83076923076923,
-0.815384615384614,-0.799999999999999,-0.784615384615384,-0.769230769230768,
-0.753846153846153,-0.738461538461538,-0.723076923076922,-0.707692307692307,
-0.692307692307692,-0.676923076923076,-0.661538461538461,-0.646153846153846,
-0.63076923076923,-0.615384615384615,-0.6,-0.584615384615384,-0.569230769230769,
-0.553846153846154,-0.538461538461538,-0.523076923076923,-0.507692307692308,
-0.492307692307692,-0.476923076923077,-0.461538461538462,-0.446153846153846,
-0.430769230769231,-0.415384615384615,-0.4,-0.384615384615385,-0.369230769230769,
-0.353846153846154,-0.338461538461538,-0.323076923076923,-0.307692307692308,
-0.292307692307692,-0.276923076923077,-0.261538461538462,-0.246153846153846,
-0.230769230769231,-0.215384615384615,-0.2,-0.184615384615385,-0.169230769230769,
-0.153846153846154,-0.138461538461538,-0.123076923076923,-0.107692307692308,
-0.0923076923076923,-0.0769230769230769,-0.0615384615384615,-0.0461538461538462,
-0.0307692307692308,-0.0153846153846154,0.),(-1.,1.),.UNSPECIFIED.)
GEOMETRIC_REPRESENTATION_ITEM()
RATIONAL_B_SPLINE_SURFACE(((1.,1.),(1.,1.),(1.,1.),(1.,1.),(1.,1.),(1.,
1.),(1.,1.),(1.,1.),(1.,1.),(1.,1.),(1.,1.),(1.,1.),(1.,1.),(1.,1.),(1.,
1.),(1.,1.),(1.,1.),(1.,1.),(1.,1.),(1.,1.),(1.,1.),(1.,1.),(1.,1.),(1.,
1.),(1.,1.),(1.,1.),(1.,1.),(1.,1.),(1.,1.),(1.,1.),(1.,1.),(1.,1.),(1.,
1.),(1.,1.),(1.,1.),(1.,1.),(1.,1.),(1.,1.),(1.,1.),(1.,1.),(1.,1.),(1.,
1.),(1.,1.),(1.,1.),(1.,1.),(1.,1.),(1.,1.),(1.,1.),(1.,1.),(1.,1.),(1.,
1.),(1.,1.),(1.,1.),(1.,1.),(1.,1.),(1.,1.),(1.,1.),(1.,1.),(1.,1.),(1.,
1.),(1.,1.),(1.,1.),(1.,1.),(1.,1.),(1.,1.),(1.,1.),(1.,1.),(1.,1.),(1.,
1.),(1.,1.)))
REPRESENTATION_ITEM('')
SURFACE()
);
#65=(
BOUNDED_SURFACE()
B_SPLINE_SURFACE(5,1,((#43640,#43641),(#43642,#43643),(#43644,#43645),(#43646,
#43647),(#43648,#43649),(#43650,#43651),(#43652,#43653),(#43654,#43655),
(#43656,#43657),(#43658,#43659),(#43660,#43661),(#43662,#43663),(#43664,
#43665),(#43666,#43667),(#43668,#43669),(#43670,#43671),(#43672,#43673),
(#43674,#43675),(#43676,#43677),(#43678,#43679),(#43680,#43681),(#43682,
#43683),(#43684,#43685),(#43686,#43687),(#43688,#43689),(#43690,#43691),
(#43692,#43693),(#43694,#43695),(#43696,#43697),(#43698,#43699),(#43700,
#43701),(#43702,#43703),(#43704,#43705),(#43706,#43707),(#43708,#43709),
(#43710,#43711),(#43712,#43713),(#43714,#43715),(#43716,#43717),(#43718,
#43719),(#43720,#43721),(#43722,#43723),(#43724,#43725),(#43726,#43727),
(#43728,#43729),(#43730,#43731),(#43732,#43733),(#43734,#43735),(#43736,
#43737),(#43738,#43739),(#43740,#43741),(#43742,#43743),(#43744,#43745),
(#43746,#43747),(#43748,#43749),(#43750,#43751),(#43752,#43753),(#43754,
#43755),(#43756,#43757),(#43758,#43759),(#43760,#43761),(#43762,#43763),
(#43764,#43765),(#43766,#43767),(#43768,#43769),(#43770,#43771),(#43772,
#43773),(#43774,#43775),(#43776,#43777),(#43778,#43779)),.UNSPECIFIED.,
 .F.,.F.,.F.)
B_SPLINE_SURFACE_WITH_KNOTS((6,1,1,1,1,1,1,1,1,1,1,1,1,1,1,1,1,1,1,1,1,
1,1,1,1,1,1,1,1,1,1,1,1,1,1,1,1,1,1,1,1,1,1,1,1,1,1,1,1,1,1,1,1,1,1,1,1,
1,1,1,1,1,1,1,1,6),(2,2),(-1.,-0.984615384615383,-0.969230769230768,-0.953846153846152,
-0.938461538461537,-0.923076923076922,-0.907692307692306,-0.892307692307691,
-0.876923076923076,-0.86153846153846,-0.846153846153845,-0.83076923076923,
-0.815384615384614,-0.799999999999999,-0.784615384615384,-0.769230769230768,
-0.753846153846153,-0.738461538461538,-0.723076923076922,-0.707692307692307,
-0.692307692307692,-0.676923076923076,-0.661538461538461,-0.646153846153846,
-0.63076923076923,-0.615384615384615,-0.6,-0.584615384615384,-0.569230769230769,
-0.553846153846154,-0.538461538461538,-0.523076923076923,-0.507692307692308,
-0.492307692307692,-0.476923076923077,-0.461538461538462,-0.446153846153846,
-0.430769230769231,-0.415384615384615,-0.4,-0.384615384615385,-0.369230769230769,
-0.353846153846154,-0.338461538461538,-0.323076923076923,-0.307692307692308,
-0.292307692307692,-0.276923076923077,-0.261538461538462,-0.246153846153846,
-0.230769230769231,-0.215384615384615,-0.2,-0.184615384615385,-0.169230769230769,
-0.153846153846154,-0.138461538461538,-0.123076923076923,-0.107692307692308,
-0.0923076923076923,-0.0769230769230769,-0.0615384615384615,-0.0461538461538462,
-0.0307692307692308,-0.0153846153846154,0.),(-1.,1.),.UNSPECIFIED.)
GEOMETRIC_REPRESENTATION_ITEM()
RATIONAL_B_SPLINE_SURFACE(((1.,1.),(1.,1.),(1.,1.),(1.,1.),(1.,1.),(1.,
1.),(1.,1.),(1.,1.),(1.,1.),(1.,1.),(1.,1.),(1.,1.),(1.,1.),(1.,1.),(1.,
1.),(1.,1.),(1.,1.),(1.,1.),(1.,1.),(1.,1.),(1.,1.),(1.,1.),(1.,1.),(1.,
1.),(1.,1.),(1.,1.),(1.,1.),(1.,1.),(1.,1.),(1.,1.),(1.,1.),(1.,1.),(1.,
1.),(1.,1.),(1.,1.),(1.,1.),(1.,1.),(1.,1.),(1.,1.),(1.,1.),(1.,1.),(1.,
1.),(1.,1.),(1.,1.),(1.,1.),(1.,1.),(1.,1.),(1.,1.),(1.,1.),(1.,1.),(1.,
1.),(1.,1.),(1.,1.),(1.,1.),(1.,1.),(1.,1.),(1.,1.),(1.,1.),(1.,1.),(1.,
1.),(1.,1.),(1.,1.),(1.,1.),(1.,1.),(1.,1.),(1.,1.),(1.,1.),(1.,1.),(1.,
1.),(1.,1.)))
REPRESENTATION_ITEM('')
SURFACE()
);
#66=(
BOUNDED_SURFACE()
B_SPLINE_SURFACE(5,1,((#43856,#43857),(#43858,#43859),(#43860,#43861),(#43862,
#43863),(#43864,#43865),(#43866,#43867),(#43868,#43869),(#43870,#43871),
(#43872,#43873),(#43874,#43875),(#43876,#43877),(#43878,#43879),(#43880,
#43881),(#43882,#43883),(#43884,#43885),(#43886,#43887),(#43888,#43889),
(#43890,#43891),(#43892,#43893),(#43894,#43895),(#43896,#43897),(#43898,
#43899),(#43900,#43901),(#43902,#43903),(#43904,#43905),(#43906,#43907),
(#43908,#43909),(#43910,#43911),(#43912,#43913),(#43914,#43915),(#43916,
#43917),(#43918,#43919),(#43920,#43921),(#43922,#43923),(#43924,#43925),
(#43926,#43927),(#43928,#43929),(#43930,#43931),(#43932,#43933),(#43934,
#43935),(#43936,#43937),(#43938,#43939),(#43940,#43941),(#43942,#43943),
(#43944,#43945),(#43946,#43947),(#43948,#43949),(#43950,#43951),(#43952,
#43953),(#43954,#43955),(#43956,#43957),(#43958,#43959),(#43960,#43961),
(#43962,#43963),(#43964,#43965),(#43966,#43967),(#43968,#43969),(#43970,
#43971),(#43972,#43973),(#43974,#43975),(#43976,#43977),(#43978,#43979),
(#43980,#43981),(#43982,#43983),(#43984,#43985),(#43986,#43987),(#43988,
#43989),(#43990,#43991),(#43992,#43993),(#43994,#43995)),.UNSPECIFIED.,
 .F.,.F.,.F.)
B_SPLINE_SURFACE_WITH_KNOTS((6,1,1,1,1,1,1,1,1,1,1,1,1,1,1,1,1,1,1,1,1,
1,1,1,1,1,1,1,1,1,1,1,1,1,1,1,1,1,1,1,1,1,1,1,1,1,1,1,1,1,1,1,1,1,1,1,1,
1,1,1,1,1,1,1,1,6),(2,2),(-1.,-0.984615384615383,-0.969230769230768,-0.953846153846152,
-0.938461538461537,-0.923076923076922,-0.907692307692306,-0.892307692307691,
-0.876923076923076,-0.86153846153846,-0.846153846153845,-0.83076923076923,
-0.815384615384614,-0.799999999999999,-0.784615384615384,-0.769230769230768,
-0.753846153846153,-0.738461538461538,-0.723076923076922,-0.707692307692307,
-0.692307692307692,-0.676923076923076,-0.661538461538461,-0.646153846153846,
-0.63076923076923,-0.615384615384615,-0.6,-0.584615384615384,-0.569230769230769,
-0.553846153846154,-0.538461538461538,-0.523076923076923,-0.507692307692308,
-0.492307692307692,-0.476923076923077,-0.461538461538462,-0.446153846153846,
-0.430769230769231,-0.415384615384615,-0.4,-0.384615384615385,-0.369230769230769,
-0.353846153846154,-0.338461538461538,-0.323076923076923,-0.307692307692308,
-0.292307692307692,-0.276923076923077,-0.261538461538462,-0.246153846153846,
-0.230769230769231,-0.215384615384615,-0.2,-0.184615384615385,-0.169230769230769,
-0.153846153846154,-0.138461538461538,-0.123076923076923,-0.107692307692308,
-0.0923076923076923,-0.0769230769230769,-0.0615384615384615,-0.0461538461538462,
-0.0307692307692308,-0.0153846153846154,0.),(-1.,1.),.UNSPECIFIED.)
GEOMETRIC_REPRESENTATION_ITEM()
RATIONAL_B_SPLINE_SURFACE(((1.,1.),(1.,1.),(1.,1.),(1.,1.),(1.,1.),(1.,
1.),(1.,1.),(1.,1.),(1.,1.),(1.,1.),(1.,1.),(1.,1.),(1.,1.),(1.,1.),(1.,
1.),(1.,1.),(1.,1.),(1.,1.),(1.,1.),(1.,1.),(1.,1.),(1.,1.),(1.,1.),(1.,
1.),(1.,1.),(1.,1.),(1.,1.),(1.,1.),(1.,1.),(1.,1.),(1.,1.),(1.,1.),(1.,
1.),(1.,1.),(1.,1.),(1.,1.),(1.,1.),(1.,1.),(1.,1.),(1.,1.),(1.,1.),(1.,
1.),(1.,1.),(1.,1.),(1.,1.),(1.,1.),(1.,1.),(1.,1.),(1.,1.),(1.,1.),(1.,
1.),(1.,1.),(1.,1.),(1.,1.),(1.,1.),(1.,1.),(1.,1.),(1.,1.),(1.,1.),(1.,
1.),(1.,1.),(1.,1.),(1.,1.),(1.,1.),(1.,1.),(1.,1.),(1.,1.),(1.,1.),(1.,
1.),(1.,1.)))
REPRESENTATION_ITEM('')
SURFACE()
);
#67=(
BOUNDED_SURFACE()
B_SPLINE_SURFACE(5,1,((#44072,#44073),(#44074,#44075),(#44076,#44077),(#44078,
#44079),(#44080,#44081),(#44082,#44083),(#44084,#44085),(#44086,#44087),
(#44088,#44089),(#44090,#44091),(#44092,#44093),(#44094,#44095),(#44096,
#44097),(#44098,#44099),(#44100,#44101),(#44102,#44103),(#44104,#44105),
(#44106,#44107),(#44108,#44109),(#44110,#44111),(#44112,#44113),(#44114,
#44115),(#44116,#44117),(#44118,#44119),(#44120,#44121),(#44122,#44123),
(#44124,#44125),(#44126,#44127),(#44128,#44129),(#44130,#44131),(#44132,
#44133),(#44134,#44135),(#44136,#44137),(#44138,#44139),(#44140,#44141),
(#44142,#44143),(#44144,#44145),(#44146,#44147),(#44148,#44149),(#44150,
#44151),(#44152,#44153),(#44154,#44155),(#44156,#44157),(#44158,#44159),
(#44160,#44161),(#44162,#44163),(#44164,#44165),(#44166,#44167),(#44168,
#44169),(#44170,#44171),(#44172,#44173),(#44174,#44175),(#44176,#44177),
(#44178,#44179),(#44180,#44181),(#44182,#44183),(#44184,#44185),(#44186,
#44187),(#44188,#44189),(#44190,#44191),(#44192,#44193),(#44194,#44195),
(#44196,#44197),(#44198,#44199),(#44200,#44201),(#44202,#44203),(#44204,
#44205),(#44206,#44207),(#44208,#44209),(#44210,#44211)),.UNSPECIFIED.,
 .F.,.F.,.F.)
B_SPLINE_SURFACE_WITH_KNOTS((6,1,1,1,1,1,1,1,1,1,1,1,1,1,1,1,1,1,1,1,1,
1,1,1,1,1,1,1,1,1,1,1,1,1,1,1,1,1,1,1,1,1,1,1,1,1,1,1,1,1,1,1,1,1,1,1,1,
1,1,1,1,1,1,1,1,6),(2,2),(-1.,-0.984615384615383,-0.969230769230768,-0.953846153846152,
-0.938461538461537,-0.923076923076922,-0.907692307692306,-0.892307692307691,
-0.876923076923076,-0.86153846153846,-0.846153846153845,-0.83076923076923,
-0.815384615384614,-0.799999999999999,-0.784615384615384,-0.769230769230768,
-0.753846153846153,-0.738461538461538,-0.723076923076922,-0.707692307692307,
-0.692307692307692,-0.676923076923076,-0.661538461538461,-0.646153846153846,
-0.63076923076923,-0.615384615384615,-0.6,-0.584615384615384,-0.569230769230769,
-0.553846153846154,-0.538461538461538,-0.523076923076923,-0.507692307692308,
-0.492307692307692,-0.476923076923077,-0.461538461538462,-0.446153846153846,
-0.430769230769231,-0.415384615384615,-0.4,-0.384615384615385,-0.369230769230769,
-0.353846153846154,-0.338461538461538,-0.323076923076923,-0.307692307692308,
-0.292307692307692,-0.276923076923077,-0.261538461538462,-0.246153846153846,
-0.230769230769231,-0.215384615384615,-0.2,-0.184615384615385,-0.169230769230769,
-0.153846153846154,-0.138461538461538,-0.123076923076923,-0.107692307692308,
-0.0923076923076923,-0.0769230769230769,-0.0615384615384615,-0.0461538461538462,
-0.0307692307692308,-0.0153846153846154,0.),(-1.,1.),.UNSPECIFIED.)
GEOMETRIC_REPRESENTATION_ITEM()
RATIONAL_B_SPLINE_SURFACE(((1.,1.),(1.,1.),(1.,1.),(1.,1.),(1.,1.),(1.,
1.),(1.,1.),(1.,1.),(1.,1.),(1.,1.),(1.,1.),(1.,1.),(1.,1.),(1.,1.),(1.,
1.),(1.,1.),(1.,1.),(1.,1.),(1.,1.),(1.,1.),(1.,1.),(1.,1.),(1.,1.),(1.,
1.),(1.,1.),(1.,1.),(1.,1.),(1.,1.),(1.,1.),(1.,1.),(1.,1.),(1.,1.),(1.,
1.),(1.,1.),(1.,1.),(1.,1.),(1.,1.),(1.,1.),(1.,1.),(1.,1.),(1.,1.),(1.,
1.),(1.,1.),(1.,1.),(1.,1.),(1.,1.),(1.,1.),(1.,1.),(1.,1.),(1.,1.),(1.,
1.),(1.,1.),(1.,1.),(1.,1.),(1.,1.),(1.,1.),(1.,1.),(1.,1.),(1.,1.),(1.,
1.),(1.,1.),(1.,1.),(1.,1.),(1.,1.),(1.,1.),(1.,1.),(1.,1.),(1.,1.),(1.,
1.),(1.,1.)))
REPRESENTATION_ITEM('')
SURFACE()
);
#68=(
BOUNDED_SURFACE()
B_SPLINE_SURFACE(5,1,((#44288,#44289),(#44290,#44291),(#44292,#44293),(#44294,
#44295),(#44296,#44297),(#44298,#44299),(#44300,#44301),(#44302,#44303),
(#44304,#44305),(#44306,#44307),(#44308,#44309),(#44310,#44311),(#44312,
#44313),(#44314,#44315),(#44316,#44317),(#44318,#44319),(#44320,#44321),
(#44322,#44323),(#44324,#44325),(#44326,#44327),(#44328,#44329),(#44330,
#44331),(#44332,#44333),(#44334,#44335),(#44336,#44337),(#44338,#44339),
(#44340,#44341),(#44342,#44343),(#44344,#44345),(#44346,#44347),(#44348,
#44349),(#44350,#44351),(#44352,#44353),(#44354,#44355),(#44356,#44357),
(#44358,#44359),(#44360,#44361),(#44362,#44363),(#44364,#44365),(#44366,
#44367),(#44368,#44369),(#44370,#44371),(#44372,#44373),(#44374,#44375),
(#44376,#44377),(#44378,#44379),(#44380,#44381),(#44382,#44383),(#44384,
#44385),(#44386,#44387),(#44388,#44389),(#44390,#44391),(#44392,#44393),
(#44394,#44395),(#44396,#44397),(#44398,#44399),(#44400,#44401),(#44402,
#44403),(#44404,#44405),(#44406,#44407),(#44408,#44409),(#44410,#44411),
(#44412,#44413),(#44414,#44415),(#44416,#44417),(#44418,#44419),(#44420,
#44421),(#44422,#44423),(#44424,#44425),(#44426,#44427)),.UNSPECIFIED.,
 .F.,.F.,.F.)
B_SPLINE_SURFACE_WITH_KNOTS((6,1,1,1,1,1,1,1,1,1,1,1,1,1,1,1,1,1,1,1,1,
1,1,1,1,1,1,1,1,1,1,1,1,1,1,1,1,1,1,1,1,1,1,1,1,1,1,1,1,1,1,1,1,1,1,1,1,
1,1,1,1,1,1,1,1,6),(2,2),(-1.,-0.984615384615383,-0.969230769230768,-0.953846153846152,
-0.938461538461537,-0.923076923076922,-0.907692307692306,-0.892307692307691,
-0.876923076923076,-0.86153846153846,-0.846153846153845,-0.83076923076923,
-0.815384615384614,-0.799999999999999,-0.784615384615384,-0.769230769230768,
-0.753846153846153,-0.738461538461538,-0.723076923076922,-0.707692307692307,
-0.692307692307692,-0.676923076923076,-0.661538461538461,-0.646153846153846,
-0.63076923076923,-0.615384615384615,-0.6,-0.584615384615384,-0.569230769230769,
-0.553846153846154,-0.538461538461538,-0.523076923076923,-0.507692307692308,
-0.492307692307692,-0.476923076923077,-0.461538461538462,-0.446153846153846,
-0.430769230769231,-0.415384615384615,-0.4,-0.384615384615385,-0.369230769230769,
-0.353846153846154,-0.338461538461538,-0.323076923076923,-0.307692307692308,
-0.292307692307692,-0.276923076923077,-0.261538461538462,-0.246153846153846,
-0.230769230769231,-0.215384615384615,-0.2,-0.184615384615385,-0.169230769230769,
-0.153846153846154,-0.138461538461538,-0.123076923076923,-0.107692307692308,
-0.0923076923076923,-0.0769230769230769,-0.0615384615384615,-0.0461538461538462,
-0.0307692307692308,-0.0153846153846154,0.),(-1.,1.),.UNSPECIFIED.)
GEOMETRIC_REPRESENTATION_ITEM()
RATIONAL_B_SPLINE_SURFACE(((1.,1.),(1.,1.),(1.,1.),(1.,1.),(1.,1.),(1.,
1.),(1.,1.),(1.,1.),(1.,1.),(1.,1.),(1.,1.),(1.,1.),(1.,1.),(1.,1.),(1.,
1.),(1.,1.),(1.,1.),(1.,1.),(1.,1.),(1.,1.),(1.,1.),(1.,1.),(1.,1.),(1.,
1.),(1.,1.),(1.,1.),(1.,1.),(1.,1.),(1.,1.),(1.,1.),(1.,1.),(1.,1.),(1.,
1.),(1.,1.),(1.,1.),(1.,1.),(1.,1.),(1.,1.),(1.,1.),(1.,1.),(1.,1.),(1.,
1.),(1.,1.),(1.,1.),(1.,1.),(1.,1.),(1.,1.),(1.,1.),(1.,1.),(1.,1.),(1.,
1.),(1.,1.),(1.,1.),(1.,1.),(1.,1.),(1.,1.),(1.,1.),(1.,1.),(1.,1.),(1.,
1.),(1.,1.),(1.,1.),(1.,1.),(1.,1.),(1.,1.),(1.,1.),(1.,1.),(1.,1.),(1.,
1.),(1.,1.)))
REPRESENTATION_ITEM('')
SURFACE()
);
#69=(
BOUNDED_SURFACE()
B_SPLINE_SURFACE(5,1,((#44504,#44505),(#44506,#44507),(#44508,#44509),(#44510,
#44511),(#44512,#44513),(#44514,#44515),(#44516,#44517),(#44518,#44519),
(#44520,#44521),(#44522,#44523),(#44524,#44525),(#44526,#44527),(#44528,
#44529),(#44530,#44531),(#44532,#44533),(#44534,#44535),(#44536,#44537),
(#44538,#44539),(#44540,#44541),(#44542,#44543),(#44544,#44545),(#44546,
#44547),(#44548,#44549),(#44550,#44551),(#44552,#44553),(#44554,#44555),
(#44556,#44557),(#44558,#44559),(#44560,#44561),(#44562,#44563),(#44564,
#44565),(#44566,#44567),(#44568,#44569),(#44570,#44571),(#44572,#44573),
(#44574,#44575),(#44576,#44577),(#44578,#44579),(#44580,#44581),(#44582,
#44583),(#44584,#44585),(#44586,#44587),(#44588,#44589),(#44590,#44591),
(#44592,#44593),(#44594,#44595),(#44596,#44597),(#44598,#44599),(#44600,
#44601),(#44602,#44603),(#44604,#44605),(#44606,#44607),(#44608,#44609),
(#44610,#44611),(#44612,#44613),(#44614,#44615),(#44616,#44617),(#44618,
#44619),(#44620,#44621),(#44622,#44623),(#44624,#44625),(#44626,#44627),
(#44628,#44629),(#44630,#44631),(#44632,#44633),(#44634,#44635),(#44636,
#44637),(#44638,#44639),(#44640,#44641),(#44642,#44643)),.UNSPECIFIED.,
 .F.,.F.,.F.)
B_SPLINE_SURFACE_WITH_KNOTS((6,1,1,1,1,1,1,1,1,1,1,1,1,1,1,1,1,1,1,1,1,
1,1,1,1,1,1,1,1,1,1,1,1,1,1,1,1,1,1,1,1,1,1,1,1,1,1,1,1,1,1,1,1,1,1,1,1,
1,1,1,1,1,1,1,1,6),(2,2),(-1.,-0.984615384615383,-0.969230769230768,-0.953846153846152,
-0.938461538461537,-0.923076923076922,-0.907692307692306,-0.892307692307691,
-0.876923076923076,-0.86153846153846,-0.846153846153845,-0.83076923076923,
-0.815384615384614,-0.799999999999999,-0.784615384615384,-0.769230769230768,
-0.753846153846153,-0.738461538461538,-0.723076923076922,-0.707692307692307,
-0.692307692307692,-0.676923076923076,-0.661538461538461,-0.646153846153846,
-0.63076923076923,-0.615384615384615,-0.6,-0.584615384615384,-0.569230769230769,
-0.553846153846154,-0.538461538461538,-0.523076923076923,-0.507692307692308,
-0.492307692307692,-0.476923076923077,-0.461538461538462,-0.446153846153846,
-0.430769230769231,-0.415384615384615,-0.4,-0.384615384615385,-0.369230769230769,
-0.353846153846154,-0.338461538461538,-0.323076923076923,-0.307692307692308,
-0.292307692307692,-0.276923076923077,-0.261538461538462,-0.246153846153846,
-0.230769230769231,-0.215384615384615,-0.2,-0.184615384615385,-0.169230769230769,
-0.153846153846154,-0.138461538461538,-0.123076923076923,-0.107692307692308,
-0.0923076923076923,-0.0769230769230769,-0.0615384615384615,-0.0461538461538462,
-0.0307692307692308,-0.0153846153846154,0.),(-1.,1.),.UNSPECIFIED.)
GEOMETRIC_REPRESENTATION_ITEM()
RATIONAL_B_SPLINE_SURFACE(((1.,1.),(1.,1.),(1.,1.),(1.,1.),(1.,1.),(1.,
1.),(1.,1.),(1.,1.),(1.,1.),(1.,1.),(1.,1.),(1.,1.),(1.,1.),(1.,1.),(1.,
1.),(1.,1.),(1.,1.),(1.,1.),(1.,1.),(1.,1.),(1.,1.),(1.,1.),(1.,1.),(1.,
1.),(1.,1.),(1.,1.),(1.,1.),(1.,1.),(1.,1.),(1.,1.),(1.,1.),(1.,1.),(1.,
1.),(1.,1.),(1.,1.),(1.,1.),(1.,1.),(1.,1.),(1.,1.),(1.,1.),(1.,1.),(1.,
1.),(1.,1.),(1.,1.),(1.,1.),(1.,1.),(1.,1.),(1.,1.),(1.,1.),(1.,1.),(1.,
1.),(1.,1.),(1.,1.),(1.,1.),(1.,1.),(1.,1.),(1.,1.),(1.,1.),(1.,1.),(1.,
1.),(1.,1.),(1.,1.),(1.,1.),(1.,1.),(1.,1.),(1.,1.),(1.,1.),(1.,1.),(1.,
1.),(1.,1.)))
REPRESENTATION_ITEM('')
SURFACE()
);
#70=(
BOUNDED_SURFACE()
B_SPLINE_SURFACE(5,1,((#44720,#44721),(#44722,#44723),(#44724,#44725),(#44726,
#44727),(#44728,#44729),(#44730,#44731),(#44732,#44733),(#44734,#44735),
(#44736,#44737),(#44738,#44739),(#44740,#44741),(#44742,#44743),(#44744,
#44745),(#44746,#44747),(#44748,#44749),(#44750,#44751),(#44752,#44753),
(#44754,#44755),(#44756,#44757),(#44758,#44759),(#44760,#44761),(#44762,
#44763),(#44764,#44765),(#44766,#44767),(#44768,#44769),(#44770,#44771),
(#44772,#44773),(#44774,#44775),(#44776,#44777),(#44778,#44779),(#44780,
#44781),(#44782,#44783),(#44784,#44785),(#44786,#44787),(#44788,#44789),
(#44790,#44791),(#44792,#44793),(#44794,#44795),(#44796,#44797),(#44798,
#44799),(#44800,#44801),(#44802,#44803),(#44804,#44805),(#44806,#44807),
(#44808,#44809),(#44810,#44811),(#44812,#44813),(#44814,#44815),(#44816,
#44817),(#44818,#44819),(#44820,#44821),(#44822,#44823),(#44824,#44825),
(#44826,#44827),(#44828,#44829),(#44830,#44831),(#44832,#44833),(#44834,
#44835),(#44836,#44837),(#44838,#44839),(#44840,#44841),(#44842,#44843),
(#44844,#44845),(#44846,#44847),(#44848,#44849),(#44850,#44851),(#44852,
#44853),(#44854,#44855),(#44856,#44857),(#44858,#44859)),.UNSPECIFIED.,
 .F.,.F.,.F.)
B_SPLINE_SURFACE_WITH_KNOTS((6,1,1,1,1,1,1,1,1,1,1,1,1,1,1,1,1,1,1,1,1,
1,1,1,1,1,1,1,1,1,1,1,1,1,1,1,1,1,1,1,1,1,1,1,1,1,1,1,1,1,1,1,1,1,1,1,1,
1,1,1,1,1,1,1,1,6),(2,2),(-1.,-0.984615384615383,-0.969230769230768,-0.953846153846152,
-0.938461538461537,-0.923076923076922,-0.907692307692306,-0.892307692307691,
-0.876923076923076,-0.86153846153846,-0.846153846153845,-0.83076923076923,
-0.815384615384614,-0.799999999999999,-0.784615384615384,-0.769230769230768,
-0.753846153846153,-0.738461538461538,-0.723076923076922,-0.707692307692307,
-0.692307692307692,-0.676923076923076,-0.661538461538461,-0.646153846153846,
-0.63076923076923,-0.615384615384615,-0.6,-0.584615384615384,-0.569230769230769,
-0.553846153846154,-0.538461538461538,-0.523076923076923,-0.507692307692308,
-0.492307692307692,-0.476923076923077,-0.461538461538462,-0.446153846153846,
-0.430769230769231,-0.415384615384615,-0.4,-0.384615384615385,-0.369230769230769,
-0.353846153846154,-0.338461538461538,-0.323076923076923,-0.307692307692308,
-0.292307692307692,-0.276923076923077,-0.261538461538462,-0.246153846153846,
-0.230769230769231,-0.215384615384615,-0.2,-0.184615384615385,-0.169230769230769,
-0.153846153846154,-0.138461538461538,-0.123076923076923,-0.107692307692308,
-0.0923076923076923,-0.0769230769230769,-0.0615384615384615,-0.0461538461538462,
-0.0307692307692308,-0.0153846153846154,0.),(-1.,1.),.UNSPECIFIED.)
GEOMETRIC_REPRESENTATION_ITEM()
RATIONAL_B_SPLINE_SURFACE(((1.,1.),(1.,1.),(1.,1.),(1.,1.),(1.,1.),(1.,
1.),(1.,1.),(1.,1.),(1.,1.),(1.,1.),(1.,1.),(1.,1.),(1.,1.),(1.,1.),(1.,
1.),(1.,1.),(1.,1.),(1.,1.),(1.,1.),(1.,1.),(1.,1.),(1.,1.),(1.,1.),(1.,
1.),(1.,1.),(1.,1.),(1.,1.),(1.,1.),(1.,1.),(1.,1.),(1.,1.),(1.,1.),(1.,
1.),(1.,1.),(1.,1.),(1.,1.),(1.,1.),(1.,1.),(1.,1.),(1.,1.),(1.,1.),(1.,
1.),(1.,1.),(1.,1.),(1.,1.),(1.,1.),(1.,1.),(1.,1.),(1.,1.),(1.,1.),(1.,
1.),(1.,1.),(1.,1.),(1.,1.),(1.,1.),(1.,1.),(1.,1.),(1.,1.),(1.,1.),(1.,
1.),(1.,1.),(1.,1.),(1.,1.),(1.,1.),(1.,1.),(1.,1.),(1.,1.),(1.,1.),(1.,
1.),(1.,1.)))
REPRESENTATION_ITEM('')
SURFACE()
);
#71=(
BOUNDED_SURFACE()
B_SPLINE_SURFACE(5,1,((#44936,#44937),(#44938,#44939),(#44940,#44941),(#44942,
#44943),(#44944,#44945),(#44946,#44947),(#44948,#44949),(#44950,#44951),
(#44952,#44953),(#44954,#44955),(#44956,#44957),(#44958,#44959),(#44960,
#44961),(#44962,#44963),(#44964,#44965),(#44966,#44967),(#44968,#44969),
(#44970,#44971),(#44972,#44973),(#44974,#44975),(#44976,#44977),(#44978,
#44979),(#44980,#44981),(#44982,#44983),(#44984,#44985),(#44986,#44987),
(#44988,#44989),(#44990,#44991),(#44992,#44993),(#44994,#44995),(#44996,
#44997),(#44998,#44999),(#45000,#45001),(#45002,#45003),(#45004,#45005),
(#45006,#45007),(#45008,#45009),(#45010,#45011),(#45012,#45013),(#45014,
#45015),(#45016,#45017),(#45018,#45019),(#45020,#45021),(#45022,#45023),
(#45024,#45025),(#45026,#45027),(#45028,#45029),(#45030,#45031),(#45032,
#45033),(#45034,#45035),(#45036,#45037),(#45038,#45039),(#45040,#45041),
(#45042,#45043),(#45044,#45045),(#45046,#45047),(#45048,#45049),(#45050,
#45051),(#45052,#45053),(#45054,#45055),(#45056,#45057),(#45058,#45059),
(#45060,#45061),(#45062,#45063),(#45064,#45065),(#45066,#45067),(#45068,
#45069),(#45070,#45071),(#45072,#45073),(#45074,#45075)),.UNSPECIFIED.,
 .F.,.F.,.F.)
B_SPLINE_SURFACE_WITH_KNOTS((6,1,1,1,1,1,1,1,1,1,1,1,1,1,1,1,1,1,1,1,1,
1,1,1,1,1,1,1,1,1,1,1,1,1,1,1,1,1,1,1,1,1,1,1,1,1,1,1,1,1,1,1,1,1,1,1,1,
1,1,1,1,1,1,1,1,6),(2,2),(-1.,-0.984615384615383,-0.969230769230768,-0.953846153846152,
-0.938461538461537,-0.923076923076922,-0.907692307692306,-0.892307692307691,
-0.876923076923076,-0.86153846153846,-0.846153846153845,-0.83076923076923,
-0.815384615384614,-0.799999999999999,-0.784615384615384,-0.769230769230768,
-0.753846153846153,-0.738461538461538,-0.723076923076922,-0.707692307692307,
-0.692307692307692,-0.676923076923076,-0.661538461538461,-0.646153846153846,
-0.63076923076923,-0.615384615384615,-0.6,-0.584615384615384,-0.569230769230769,
-0.553846153846154,-0.538461538461538,-0.523076923076923,-0.507692307692308,
-0.492307692307692,-0.476923076923077,-0.461538461538462,-0.446153846153846,
-0.430769230769231,-0.415384615384615,-0.4,-0.384615384615385,-0.369230769230769,
-0.353846153846154,-0.338461538461538,-0.323076923076923,-0.307692307692308,
-0.292307692307692,-0.276923076923077,-0.261538461538462,-0.246153846153846,
-0.230769230769231,-0.215384615384615,-0.2,-0.184615384615385,-0.169230769230769,
-0.153846153846154,-0.138461538461538,-0.123076923076923,-0.107692307692308,
-0.0923076923076923,-0.0769230769230769,-0.0615384615384615,-0.0461538461538462,
-0.0307692307692308,-0.0153846153846154,0.),(-1.,1.),.UNSPECIFIED.)
GEOMETRIC_REPRESENTATION_ITEM()
RATIONAL_B_SPLINE_SURFACE(((1.,1.),(1.,1.),(1.,1.),(1.,1.),(1.,1.),(1.,
1.),(1.,1.),(1.,1.),(1.,1.),(1.,1.),(1.,1.),(1.,1.),(1.,1.),(1.,1.),(1.,
1.),(1.,1.),(1.,1.),(1.,1.),(1.,1.),(1.,1.),(1.,1.),(1.,1.),(1.,1.),(1.,
1.),(1.,1.),(1.,1.),(1.,1.),(1.,1.),(1.,1.),(1.,1.),(1.,1.),(1.,1.),(1.,
1.),(1.,1.),(1.,1.),(1.,1.),(1.,1.),(1.,1.),(1.,1.),(1.,1.),(1.,1.),(1.,
1.),(1.,1.),(1.,1.),(1.,1.),(1.,1.),(1.,1.),(1.,1.),(1.,1.),(1.,1.),(1.,
1.),(1.,1.),(1.,1.),(1.,1.),(1.,1.),(1.,1.),(1.,1.),(1.,1.),(1.,1.),(1.,
1.),(1.,1.),(1.,1.),(1.,1.),(1.,1.),(1.,1.),(1.,1.),(1.,1.),(1.,1.),(1.,
1.),(1.,1.)))
REPRESENTATION_ITEM('')
SURFACE()
);
#72=(
BOUNDED_SURFACE()
B_SPLINE_SURFACE(5,1,((#45152,#45153),(#45154,#45155),(#45156,#45157),(#45158,
#45159),(#45160,#45161),(#45162,#45163),(#45164,#45165),(#45166,#45167),
(#45168,#45169),(#45170,#45171),(#45172,#45173),(#45174,#45175),(#45176,
#45177),(#45178,#45179),(#45180,#45181),(#45182,#45183),(#45184,#45185),
(#45186,#45187),(#45188,#45189),(#45190,#45191),(#45192,#45193),(#45194,
#45195),(#45196,#45197),(#45198,#45199),(#45200,#45201),(#45202,#45203),
(#45204,#45205),(#45206,#45207),(#45208,#45209),(#45210,#45211),(#45212,
#45213),(#45214,#45215),(#45216,#45217),(#45218,#45219),(#45220,#45221),
(#45222,#45223),(#45224,#45225),(#45226,#45227),(#45228,#45229),(#45230,
#45231),(#45232,#45233),(#45234,#45235),(#45236,#45237),(#45238,#45239),
(#45240,#45241),(#45242,#45243),(#45244,#45245),(#45246,#45247),(#45248,
#45249),(#45250,#45251),(#45252,#45253),(#45254,#45255),(#45256,#45257),
(#45258,#45259),(#45260,#45261),(#45262,#45263),(#45264,#45265),(#45266,
#45267),(#45268,#45269),(#45270,#45271),(#45272,#45273),(#45274,#45275),
(#45276,#45277),(#45278,#45279),(#45280,#45281),(#45282,#45283),(#45284,
#45285),(#45286,#45287),(#45288,#45289),(#45290,#45291)),.UNSPECIFIED.,
 .F.,.F.,.F.)
B_SPLINE_SURFACE_WITH_KNOTS((6,1,1,1,1,1,1,1,1,1,1,1,1,1,1,1,1,1,1,1,1,
1,1,1,1,1,1,1,1,1,1,1,1,1,1,1,1,1,1,1,1,1,1,1,1,1,1,1,1,1,1,1,1,1,1,1,1,
1,1,1,1,1,1,1,1,6),(2,2),(-1.,-0.984615384615383,-0.969230769230768,-0.953846153846152,
-0.938461538461537,-0.923076923076922,-0.907692307692306,-0.892307692307691,
-0.876923076923076,-0.86153846153846,-0.846153846153845,-0.83076923076923,
-0.815384615384614,-0.799999999999999,-0.784615384615384,-0.769230769230768,
-0.753846153846153,-0.738461538461538,-0.723076923076922,-0.707692307692307,
-0.692307692307692,-0.676923076923076,-0.661538461538461,-0.646153846153846,
-0.63076923076923,-0.615384615384615,-0.6,-0.584615384615384,-0.569230769230769,
-0.553846153846154,-0.538461538461538,-0.523076923076923,-0.507692307692308,
-0.492307692307692,-0.476923076923077,-0.461538461538462,-0.446153846153846,
-0.430769230769231,-0.415384615384615,-0.4,-0.384615384615385,-0.369230769230769,
-0.353846153846154,-0.338461538461538,-0.323076923076923,-0.307692307692308,
-0.292307692307692,-0.276923076923077,-0.261538461538462,-0.246153846153846,
-0.230769230769231,-0.215384615384615,-0.2,-0.184615384615385,-0.169230769230769,
-0.153846153846154,-0.138461538461538,-0.123076923076923,-0.107692307692308,
-0.0923076923076923,-0.0769230769230769,-0.0615384615384615,-0.0461538461538462,
-0.0307692307692308,-0.0153846153846154,0.),(-1.,1.),.UNSPECIFIED.)
GEOMETRIC_REPRESENTATION_ITEM()
RATIONAL_B_SPLINE_SURFACE(((1.,1.),(1.,1.),(1.,1.),(1.,1.),(1.,1.),(1.,
1.),(1.,1.),(1.,1.),(1.,1.),(1.,1.),(1.,1.),(1.,1.),(1.,1.),(1.,1.),(1.,
1.),(1.,1.),(1.,1.),(1.,1.),(1.,1.),(1.,1.),(1.,1.),(1.,1.),(1.,1.),(1.,
1.),(1.,1.),(1.,1.),(1.,1.),(1.,1.),(1.,1.),(1.,1.),(1.,1.),(1.,1.),(1.,
1.),(1.,1.),(1.,1.),(1.,1.),(1.,1.),(1.,1.),(1.,1.),(1.,1.),(1.,1.),(1.,
1.),(1.,1.),(1.,1.),(1.,1.),(1.,1.),(1.,1.),(1.,1.),(1.,1.),(1.,1.),(1.,
1.),(1.,1.),(1.,1.),(1.,1.),(1.,1.),(1.,1.),(1.,1.),(1.,1.),(1.,1.),(1.,
1.),(1.,1.),(1.,1.),(1.,1.),(1.,1.),(1.,1.),(1.,1.),(1.,1.),(1.,1.),(1.,
1.),(1.,1.)))
REPRESENTATION_ITEM('')
SURFACE()
);
#73=(
BOUNDED_SURFACE()
B_SPLINE_SURFACE(5,1,((#45368,#45369),(#45370,#45371),(#45372,#45373),(#45374,
#45375),(#45376,#45377),(#45378,#45379),(#45380,#45381),(#45382,#45383),
(#45384,#45385),(#45386,#45387),(#45388,#45389),(#45390,#45391),(#45392,
#45393),(#45394,#45395),(#45396,#45397),(#45398,#45399),(#45400,#45401),
(#45402,#45403),(#45404,#45405),(#45406,#45407),(#45408,#45409),(#45410,
#45411),(#45412,#45413),(#45414,#45415),(#45416,#45417),(#45418,#45419),
(#45420,#45421),(#45422,#45423),(#45424,#45425),(#45426,#45427),(#45428,
#45429),(#45430,#45431),(#45432,#45433),(#45434,#45435),(#45436,#45437),
(#45438,#45439),(#45440,#45441),(#45442,#45443),(#45444,#45445),(#45446,
#45447),(#45448,#45449),(#45450,#45451),(#45452,#45453),(#45454,#45455),
(#45456,#45457),(#45458,#45459),(#45460,#45461),(#45462,#45463),(#45464,
#45465),(#45466,#45467),(#45468,#45469),(#45470,#45471),(#45472,#45473),
(#45474,#45475),(#45476,#45477),(#45478,#45479),(#45480,#45481),(#45482,
#45483),(#45484,#45485),(#45486,#45487),(#45488,#45489),(#45490,#45491),
(#45492,#45493),(#45494,#45495),(#45496,#45497),(#45498,#45499),(#45500,
#45501),(#45502,#45503),(#45504,#45505),(#45506,#45507)),.UNSPECIFIED.,
 .F.,.F.,.F.)
B_SPLINE_SURFACE_WITH_KNOTS((6,1,1,1,1,1,1,1,1,1,1,1,1,1,1,1,1,1,1,1,1,
1,1,1,1,1,1,1,1,1,1,1,1,1,1,1,1,1,1,1,1,1,1,1,1,1,1,1,1,1,1,1,1,1,1,1,1,
1,1,1,1,1,1,1,1,6),(2,2),(-1.,-0.984615384615383,-0.969230769230768,-0.953846153846152,
-0.938461538461537,-0.923076923076922,-0.907692307692306,-0.892307692307691,
-0.876923076923076,-0.86153846153846,-0.846153846153845,-0.83076923076923,
-0.815384615384614,-0.799999999999999,-0.784615384615384,-0.769230769230768,
-0.753846153846153,-0.738461538461538,-0.723076923076922,-0.707692307692307,
-0.692307692307692,-0.676923076923076,-0.661538461538461,-0.646153846153846,
-0.63076923076923,-0.615384615384615,-0.6,-0.584615384615384,-0.569230769230769,
-0.553846153846154,-0.538461538461538,-0.523076923076923,-0.507692307692308,
-0.492307692307692,-0.476923076923077,-0.461538461538462,-0.446153846153846,
-0.430769230769231,-0.415384615384615,-0.4,-0.384615384615385,-0.369230769230769,
-0.353846153846154,-0.338461538461538,-0.323076923076923,-0.307692307692308,
-0.292307692307692,-0.276923076923077,-0.261538461538462,-0.246153846153846,
-0.230769230769231,-0.215384615384615,-0.2,-0.184615384615385,-0.169230769230769,
-0.153846153846154,-0.138461538461538,-0.123076923076923,-0.107692307692308,
-0.0923076923076923,-0.0769230769230769,-0.0615384615384615,-0.0461538461538462,
-0.0307692307692308,-0.0153846153846154,0.),(-1.,1.),.UNSPECIFIED.)
GEOMETRIC_REPRESENTATION_ITEM()
RATIONAL_B_SPLINE_SURFACE(((1.,1.),(1.,1.),(1.,1.),(1.,1.),(1.,1.),(1.,
1.),(1.,1.),(1.,1.),(1.,1.),(1.,1.),(1.,1.),(1.,1.),(1.,1.),(1.,1.),(1.,
1.),(1.,1.),(1.,1.),(1.,1.),(1.,1.),(1.,1.),(1.,1.),(1.,1.),(1.,1.),(1.,
1.),(1.,1.),(1.,1.),(1.,1.),(1.,1.),(1.,1.),(1.,1.),(1.,1.),(1.,1.),(1.,
1.),(1.,1.),(1.,1.),(1.,1.),(1.,1.),(1.,1.),(1.,1.),(1.,1.),(1.,1.),(1.,
1.),(1.,1.),(1.,1.),(1.,1.),(1.,1.),(1.,1.),(1.,1.),(1.,1.),(1.,1.),(1.,
1.),(1.,1.),(1.,1.),(1.,1.),(1.,1.),(1.,1.),(1.,1.),(1.,1.),(1.,1.),(1.,
1.),(1.,1.),(1.,1.),(1.,1.),(1.,1.),(1.,1.),(1.,1.),(1.,1.),(1.,1.),(1.,
1.),(1.,1.)))
REPRESENTATION_ITEM('')
SURFACE()
);
#74=(
BOUNDED_SURFACE()
B_SPLINE_SURFACE(5,1,((#45584,#45585),(#45586,#45587),(#45588,#45589),(#45590,
#45591),(#45592,#45593),(#45594,#45595),(#45596,#45597),(#45598,#45599),
(#45600,#45601),(#45602,#45603),(#45604,#45605),(#45606,#45607),(#45608,
#45609),(#45610,#45611),(#45612,#45613),(#45614,#45615),(#45616,#45617),
(#45618,#45619),(#45620,#45621),(#45622,#45623),(#45624,#45625),(#45626,
#45627),(#45628,#45629),(#45630,#45631),(#45632,#45633),(#45634,#45635),
(#45636,#45637),(#45638,#45639),(#45640,#45641),(#45642,#45643),(#45644,
#45645),(#45646,#45647),(#45648,#45649),(#45650,#45651),(#45652,#45653),
(#45654,#45655),(#45656,#45657),(#45658,#45659),(#45660,#45661),(#45662,
#45663),(#45664,#45665),(#45666,#45667),(#45668,#45669),(#45670,#45671),
(#45672,#45673),(#45674,#45675),(#45676,#45677),(#45678,#45679),(#45680,
#45681),(#45682,#45683),(#45684,#45685),(#45686,#45687),(#45688,#45689),
(#45690,#45691),(#45692,#45693),(#45694,#45695),(#45696,#45697),(#45698,
#45699),(#45700,#45701),(#45702,#45703),(#45704,#45705),(#45706,#45707),
(#45708,#45709),(#45710,#45711),(#45712,#45713),(#45714,#45715),(#45716,
#45717),(#45718,#45719),(#45720,#45721),(#45722,#45723)),.UNSPECIFIED.,
 .F.,.F.,.F.)
B_SPLINE_SURFACE_WITH_KNOTS((6,1,1,1,1,1,1,1,1,1,1,1,1,1,1,1,1,1,1,1,1,
1,1,1,1,1,1,1,1,1,1,1,1,1,1,1,1,1,1,1,1,1,1,1,1,1,1,1,1,1,1,1,1,1,1,1,1,
1,1,1,1,1,1,1,1,6),(2,2),(-1.,-0.984615384615383,-0.969230769230768,-0.953846153846152,
-0.938461538461537,-0.923076923076922,-0.907692307692306,-0.892307692307691,
-0.876923076923076,-0.86153846153846,-0.846153846153845,-0.83076923076923,
-0.815384615384614,-0.799999999999999,-0.784615384615384,-0.769230769230768,
-0.753846153846153,-0.738461538461538,-0.723076923076922,-0.707692307692307,
-0.692307692307692,-0.676923076923076,-0.661538461538461,-0.646153846153846,
-0.63076923076923,-0.615384615384615,-0.6,-0.584615384615384,-0.569230769230769,
-0.553846153846154,-0.538461538461538,-0.523076923076923,-0.507692307692308,
-0.492307692307692,-0.476923076923077,-0.461538461538462,-0.446153846153846,
-0.430769230769231,-0.415384615384615,-0.4,-0.384615384615385,-0.369230769230769,
-0.353846153846154,-0.338461538461538,-0.323076923076923,-0.307692307692308,
-0.292307692307692,-0.276923076923077,-0.261538461538462,-0.246153846153846,
-0.230769230769231,-0.215384615384615,-0.2,-0.184615384615385,-0.169230769230769,
-0.153846153846154,-0.138461538461538,-0.123076923076923,-0.107692307692308,
-0.0923076923076923,-0.0769230769230769,-0.0615384615384615,-0.0461538461538462,
-0.0307692307692308,-0.0153846153846154,0.),(-1.,1.),.UNSPECIFIED.)
GEOMETRIC_REPRESENTATION_ITEM()
RATIONAL_B_SPLINE_SURFACE(((1.,1.),(1.,1.),(1.,1.),(1.,1.),(1.,1.),(1.,
1.),(1.,1.),(1.,1.),(1.,1.),(1.,1.),(1.,1.),(1.,1.),(1.,1.),(1.,1.),(1.,
1.),(1.,1.),(1.,1.),(1.,1.),(1.,1.),(1.,1.),(1.,1.),(1.,1.),(1.,1.),(1.,
1.),(1.,1.),(1.,1.),(1.,1.),(1.,1.),(1.,1.),(1.,1.),(1.,1.),(1.,1.),(1.,
1.),(1.,1.),(1.,1.),(1.,1.),(1.,1.),(1.,1.),(1.,1.),(1.,1.),(1.,1.),(1.,
1.),(1.,1.),(1.,1.),(1.,1.),(1.,1.),(1.,1.),(1.,1.),(1.,1.),(1.,1.),(1.,
1.),(1.,1.),(1.,1.),(1.,1.),(1.,1.),(1.,1.),(1.,1.),(1.,1.),(1.,1.),(1.,
1.),(1.,1.),(1.,1.),(1.,1.),(1.,1.),(1.,1.),(1.,1.),(1.,1.),(1.,1.),(1.,
1.),(1.,1.)))
REPRESENTATION_ITEM('')
SURFACE()
);
#75=(
BOUNDED_SURFACE()
B_SPLINE_SURFACE(5,1,((#45800,#45801),(#45802,#45803),(#45804,#45805),(#45806,
#45807),(#45808,#45809),(#45810,#45811),(#45812,#45813),(#45814,#45815),
(#45816,#45817),(#45818,#45819),(#45820,#45821),(#45822,#45823),(#45824,
#45825),(#45826,#45827),(#45828,#45829),(#45830,#45831),(#45832,#45833),
(#45834,#45835),(#45836,#45837),(#45838,#45839),(#45840,#45841),(#45842,
#45843),(#45844,#45845),(#45846,#45847),(#45848,#45849),(#45850,#45851),
(#45852,#45853),(#45854,#45855),(#45856,#45857),(#45858,#45859),(#45860,
#45861),(#45862,#45863),(#45864,#45865),(#45866,#45867),(#45868,#45869),
(#45870,#45871),(#45872,#45873),(#45874,#45875),(#45876,#45877),(#45878,
#45879),(#45880,#45881),(#45882,#45883),(#45884,#45885),(#45886,#45887),
(#45888,#45889),(#45890,#45891),(#45892,#45893),(#45894,#45895),(#45896,
#45897),(#45898,#45899),(#45900,#45901),(#45902,#45903),(#45904,#45905),
(#45906,#45907),(#45908,#45909),(#45910,#45911),(#45912,#45913),(#45914,
#45915),(#45916,#45917),(#45918,#45919),(#45920,#45921),(#45922,#45923),
(#45924,#45925),(#45926,#45927),(#45928,#45929),(#45930,#45931),(#45932,
#45933),(#45934,#45935),(#45936,#45937),(#45938,#45939)),.UNSPECIFIED.,
 .F.,.F.,.F.)
B_SPLINE_SURFACE_WITH_KNOTS((6,1,1,1,1,1,1,1,1,1,1,1,1,1,1,1,1,1,1,1,1,
1,1,1,1,1,1,1,1,1,1,1,1,1,1,1,1,1,1,1,1,1,1,1,1,1,1,1,1,1,1,1,1,1,1,1,1,
1,1,1,1,1,1,1,1,6),(2,2),(-1.,-0.984615384615383,-0.969230769230768,-0.953846153846152,
-0.938461538461537,-0.923076923076922,-0.907692307692306,-0.892307692307691,
-0.876923076923076,-0.86153846153846,-0.846153846153845,-0.83076923076923,
-0.815384615384614,-0.799999999999999,-0.784615384615384,-0.769230769230768,
-0.753846153846153,-0.738461538461538,-0.723076923076922,-0.707692307692307,
-0.692307692307692,-0.676923076923076,-0.661538461538461,-0.646153846153846,
-0.63076923076923,-0.615384615384615,-0.6,-0.584615384615384,-0.569230769230769,
-0.553846153846154,-0.538461538461538,-0.523076923076923,-0.507692307692308,
-0.492307692307692,-0.476923076923077,-0.461538461538462,-0.446153846153846,
-0.430769230769231,-0.415384615384615,-0.4,-0.384615384615385,-0.369230769230769,
-0.353846153846154,-0.338461538461538,-0.323076923076923,-0.307692307692308,
-0.292307692307692,-0.276923076923077,-0.261538461538462,-0.246153846153846,
-0.230769230769231,-0.215384615384615,-0.2,-0.184615384615385,-0.169230769230769,
-0.153846153846154,-0.138461538461538,-0.123076923076923,-0.107692307692308,
-0.0923076923076923,-0.0769230769230769,-0.0615384615384615,-0.0461538461538462,
-0.0307692307692308,-0.0153846153846154,0.),(-1.,1.),.UNSPECIFIED.)
GEOMETRIC_REPRESENTATION_ITEM()
RATIONAL_B_SPLINE_SURFACE(((1.,1.),(1.,1.),(1.,1.),(1.,1.),(1.,1.),(1.,
1.),(1.,1.),(1.,1.),(1.,1.),(1.,1.),(1.,1.),(1.,1.),(1.,1.),(1.,1.),(1.,
1.),(1.,1.),(1.,1.),(1.,1.),(1.,1.),(1.,1.),(1.,1.),(1.,1.),(1.,1.),(1.,
1.),(1.,1.),(1.,1.),(1.,1.),(1.,1.),(1.,1.),(1.,1.),(1.,1.),(1.,1.),(1.,
1.),(1.,1.),(1.,1.),(1.,1.),(1.,1.),(1.,1.),(1.,1.),(1.,1.),(1.,1.),(1.,
1.),(1.,1.),(1.,1.),(1.,1.),(1.,1.),(1.,1.),(1.,1.),(1.,1.),(1.,1.),(1.,
1.),(1.,1.),(1.,1.),(1.,1.),(1.,1.),(1.,1.),(1.,1.),(1.,1.),(1.,1.),(1.,
1.),(1.,1.),(1.,1.),(1.,1.),(1.,1.),(1.,1.),(1.,1.),(1.,1.),(1.,1.),(1.,
1.),(1.,1.)))
REPRESENTATION_ITEM('')
SURFACE()
);
#76=(
BOUNDED_SURFACE()
B_SPLINE_SURFACE(5,1,((#46016,#46017),(#46018,#46019),(#46020,#46021),(#46022,
#46023),(#46024,#46025),(#46026,#46027),(#46028,#46029),(#46030,#46031),
(#46032,#46033),(#46034,#46035),(#46036,#46037),(#46038,#46039),(#46040,
#46041),(#46042,#46043),(#46044,#46045),(#46046,#46047),(#46048,#46049),
(#46050,#46051),(#46052,#46053),(#46054,#46055),(#46056,#46057),(#46058,
#46059),(#46060,#46061),(#46062,#46063),(#46064,#46065),(#46066,#46067),
(#46068,#46069),(#46070,#46071),(#46072,#46073),(#46074,#46075),(#46076,
#46077),(#46078,#46079),(#46080,#46081),(#46082,#46083),(#46084,#46085),
(#46086,#46087),(#46088,#46089),(#46090,#46091),(#46092,#46093),(#46094,
#46095),(#46096,#46097),(#46098,#46099),(#46100,#46101),(#46102,#46103),
(#46104,#46105),(#46106,#46107),(#46108,#46109),(#46110,#46111),(#46112,
#46113),(#46114,#46115),(#46116,#46117),(#46118,#46119),(#46120,#46121),
(#46122,#46123),(#46124,#46125),(#46126,#46127),(#46128,#46129),(#46130,
#46131),(#46132,#46133),(#46134,#46135),(#46136,#46137),(#46138,#46139),
(#46140,#46141),(#46142,#46143),(#46144,#46145),(#46146,#46147),(#46148,
#46149),(#46150,#46151),(#46152,#46153),(#46154,#46155)),.UNSPECIFIED.,
 .F.,.F.,.F.)
B_SPLINE_SURFACE_WITH_KNOTS((6,1,1,1,1,1,1,1,1,1,1,1,1,1,1,1,1,1,1,1,1,
1,1,1,1,1,1,1,1,1,1,1,1,1,1,1,1,1,1,1,1,1,1,1,1,1,1,1,1,1,1,1,1,1,1,1,1,
1,1,1,1,1,1,1,1,6),(2,2),(-1.,-0.984615384615383,-0.969230769230768,-0.953846153846152,
-0.938461538461537,-0.923076923076922,-0.907692307692306,-0.892307692307691,
-0.876923076923076,-0.86153846153846,-0.846153846153845,-0.83076923076923,
-0.815384615384614,-0.799999999999999,-0.784615384615384,-0.769230769230768,
-0.753846153846153,-0.738461538461538,-0.723076923076922,-0.707692307692307,
-0.692307692307692,-0.676923076923076,-0.661538461538461,-0.646153846153846,
-0.63076923076923,-0.615384615384615,-0.6,-0.584615384615384,-0.569230769230769,
-0.553846153846154,-0.538461538461538,-0.523076923076923,-0.507692307692308,
-0.492307692307692,-0.476923076923077,-0.461538461538462,-0.446153846153846,
-0.430769230769231,-0.415384615384615,-0.4,-0.384615384615385,-0.369230769230769,
-0.353846153846154,-0.338461538461538,-0.323076923076923,-0.307692307692308,
-0.292307692307692,-0.276923076923077,-0.261538461538462,-0.246153846153846,
-0.230769230769231,-0.215384615384615,-0.2,-0.184615384615385,-0.169230769230769,
-0.153846153846154,-0.138461538461538,-0.123076923076923,-0.107692307692308,
-0.0923076923076923,-0.0769230769230769,-0.0615384615384615,-0.0461538461538462,
-0.0307692307692308,-0.0153846153846154,0.),(-1.,1.),.UNSPECIFIED.)
GEOMETRIC_REPRESENTATION_ITEM()
RATIONAL_B_SPLINE_SURFACE(((1.,1.),(1.,1.),(1.,1.),(1.,1.),(1.,1.),(1.,
1.),(1.,1.),(1.,1.),(1.,1.),(1.,1.),(1.,1.),(1.,1.),(1.,1.),(1.,1.),(1.,
1.),(1.,1.),(1.,1.),(1.,1.),(1.,1.),(1.,1.),(1.,1.),(1.,1.),(1.,1.),(1.,
1.),(1.,1.),(1.,1.),(1.,1.),(1.,1.),(1.,1.),(1.,1.),(1.,1.),(1.,1.),(1.,
1.),(1.,1.),(1.,1.),(1.,1.),(1.,1.),(1.,1.),(1.,1.),(1.,1.),(1.,1.),(1.,
1.),(1.,1.),(1.,1.),(1.,1.),(1.,1.),(1.,1.),(1.,1.),(1.,1.),(1.,1.),(1.,
1.),(1.,1.),(1.,1.),(1.,1.),(1.,1.),(1.,1.),(1.,1.),(1.,1.),(1.,1.),(1.,
1.),(1.,1.),(1.,1.),(1.,1.),(1.,1.),(1.,1.),(1.,1.),(1.,1.),(1.,1.),(1.,
1.),(1.,1.)))
REPRESENTATION_ITEM('')
SURFACE()
);
#77=(
BOUNDED_SURFACE()
B_SPLINE_SURFACE(5,1,((#46232,#46233),(#46234,#46235),(#46236,#46237),(#46238,
#46239),(#46240,#46241),(#46242,#46243),(#46244,#46245),(#46246,#46247),
(#46248,#46249),(#46250,#46251),(#46252,#46253),(#46254,#46255),(#46256,
#46257),(#46258,#46259),(#46260,#46261),(#46262,#46263),(#46264,#46265),
(#46266,#46267),(#46268,#46269),(#46270,#46271),(#46272,#46273),(#46274,
#46275),(#46276,#46277),(#46278,#46279),(#46280,#46281),(#46282,#46283),
(#46284,#46285),(#46286,#46287),(#46288,#46289),(#46290,#46291),(#46292,
#46293),(#46294,#46295),(#46296,#46297),(#46298,#46299),(#46300,#46301),
(#46302,#46303),(#46304,#46305),(#46306,#46307),(#46308,#46309),(#46310,
#46311),(#46312,#46313),(#46314,#46315),(#46316,#46317),(#46318,#46319),
(#46320,#46321),(#46322,#46323),(#46324,#46325),(#46326,#46327),(#46328,
#46329),(#46330,#46331),(#46332,#46333),(#46334,#46335),(#46336,#46337),
(#46338,#46339),(#46340,#46341),(#46342,#46343),(#46344,#46345),(#46346,
#46347),(#46348,#46349),(#46350,#46351),(#46352,#46353),(#46354,#46355),
(#46356,#46357),(#46358,#46359),(#46360,#46361),(#46362,#46363),(#46364,
#46365),(#46366,#46367),(#46368,#46369),(#46370,#46371)),.UNSPECIFIED.,
 .F.,.F.,.F.)
B_SPLINE_SURFACE_WITH_KNOTS((6,1,1,1,1,1,1,1,1,1,1,1,1,1,1,1,1,1,1,1,1,
1,1,1,1,1,1,1,1,1,1,1,1,1,1,1,1,1,1,1,1,1,1,1,1,1,1,1,1,1,1,1,1,1,1,1,1,
1,1,1,1,1,1,1,1,6),(2,2),(-1.,-0.984615384615383,-0.969230769230768,-0.953846153846152,
-0.938461538461537,-0.923076923076922,-0.907692307692306,-0.892307692307691,
-0.876923076923076,-0.86153846153846,-0.846153846153845,-0.83076923076923,
-0.815384615384614,-0.799999999999999,-0.784615384615384,-0.769230769230768,
-0.753846153846153,-0.738461538461538,-0.723076923076922,-0.707692307692307,
-0.692307692307692,-0.676923076923076,-0.661538461538461,-0.646153846153846,
-0.63076923076923,-0.615384615384615,-0.6,-0.584615384615384,-0.569230769230769,
-0.553846153846154,-0.538461538461538,-0.523076923076923,-0.507692307692308,
-0.492307692307692,-0.476923076923077,-0.461538461538462,-0.446153846153846,
-0.430769230769231,-0.415384615384615,-0.4,-0.384615384615385,-0.369230769230769,
-0.353846153846154,-0.338461538461538,-0.323076923076923,-0.307692307692308,
-0.292307692307692,-0.276923076923077,-0.261538461538462,-0.246153846153846,
-0.230769230769231,-0.215384615384615,-0.2,-0.184615384615385,-0.169230769230769,
-0.153846153846154,-0.138461538461538,-0.123076923076923,-0.107692307692308,
-0.0923076923076923,-0.0769230769230769,-0.0615384615384615,-0.0461538461538462,
-0.0307692307692308,-0.0153846153846154,0.),(-1.,1.),.UNSPECIFIED.)
GEOMETRIC_REPRESENTATION_ITEM()
RATIONAL_B_SPLINE_SURFACE(((1.,1.),(1.,1.),(1.,1.),(1.,1.),(1.,1.),(1.,
1.),(1.,1.),(1.,1.),(1.,1.),(1.,1.),(1.,1.),(1.,1.),(1.,1.),(1.,1.),(1.,
1.),(1.,1.),(1.,1.),(1.,1.),(1.,1.),(1.,1.),(1.,1.),(1.,1.),(1.,1.),(1.,
1.),(1.,1.),(1.,1.),(1.,1.),(1.,1.),(1.,1.),(1.,1.),(1.,1.),(1.,1.),(1.,
1.),(1.,1.),(1.,1.),(1.,1.),(1.,1.),(1.,1.),(1.,1.),(1.,1.),(1.,1.),(1.,
1.),(1.,1.),(1.,1.),(1.,1.),(1.,1.),(1.,1.),(1.,1.),(1.,1.),(1.,1.),(1.,
1.),(1.,1.),(1.,1.),(1.,1.),(1.,1.),(1.,1.),(1.,1.),(1.,1.),(1.,1.),(1.,
1.),(1.,1.),(1.,1.),(1.,1.),(1.,1.),(1.,1.),(1.,1.),(1.,1.),(1.,1.),(1.,
1.),(1.,1.)))
REPRESENTATION_ITEM('')
SURFACE()
);
#78=(
BOUNDED_SURFACE()
B_SPLINE_SURFACE(5,1,((#46448,#46449),(#46450,#46451),(#46452,#46453),(#46454,
#46455),(#46456,#46457),(#46458,#46459),(#46460,#46461),(#46462,#46463),
(#46464,#46465),(#46466,#46467),(#46468,#46469),(#46470,#46471),(#46472,
#46473),(#46474,#46475),(#46476,#46477),(#46478,#46479),(#46480,#46481),
(#46482,#46483),(#46484,#46485),(#46486,#46487),(#46488,#46489),(#46490,
#46491),(#46492,#46493),(#46494,#46495),(#46496,#46497),(#46498,#46499),
(#46500,#46501),(#46502,#46503),(#46504,#46505),(#46506,#46507),(#46508,
#46509),(#46510,#46511),(#46512,#46513),(#46514,#46515),(#46516,#46517),
(#46518,#46519),(#46520,#46521),(#46522,#46523),(#46524,#46525),(#46526,
#46527),(#46528,#46529),(#46530,#46531),(#46532,#46533),(#46534,#46535),
(#46536,#46537),(#46538,#46539),(#46540,#46541),(#46542,#46543),(#46544,
#46545),(#46546,#46547),(#46548,#46549),(#46550,#46551),(#46552,#46553),
(#46554,#46555),(#46556,#46557),(#46558,#46559),(#46560,#46561),(#46562,
#46563),(#46564,#46565),(#46566,#46567),(#46568,#46569),(#46570,#46571),
(#46572,#46573),(#46574,#46575),(#46576,#46577),(#46578,#46579),(#46580,
#46581),(#46582,#46583),(#46584,#46585),(#46586,#46587)),.UNSPECIFIED.,
 .F.,.F.,.F.)
B_SPLINE_SURFACE_WITH_KNOTS((6,1,1,1,1,1,1,1,1,1,1,1,1,1,1,1,1,1,1,1,1,
1,1,1,1,1,1,1,1,1,1,1,1,1,1,1,1,1,1,1,1,1,1,1,1,1,1,1,1,1,1,1,1,1,1,1,1,
1,1,1,1,1,1,1,1,6),(2,2),(-1.,-0.984615384615383,-0.969230769230768,-0.953846153846152,
-0.938461538461537,-0.923076923076922,-0.907692307692306,-0.892307692307691,
-0.876923076923076,-0.86153846153846,-0.846153846153845,-0.83076923076923,
-0.815384615384614,-0.799999999999999,-0.784615384615384,-0.769230769230768,
-0.753846153846153,-0.738461538461538,-0.723076923076922,-0.707692307692307,
-0.692307692307692,-0.676923076923076,-0.661538461538461,-0.646153846153846,
-0.63076923076923,-0.615384615384615,-0.6,-0.584615384615384,-0.569230769230769,
-0.553846153846154,-0.538461538461538,-0.523076923076923,-0.507692307692308,
-0.492307692307692,-0.476923076923077,-0.461538461538462,-0.446153846153846,
-0.430769230769231,-0.415384615384615,-0.4,-0.384615384615385,-0.369230769230769,
-0.353846153846154,-0.338461538461538,-0.323076923076923,-0.307692307692308,
-0.292307692307692,-0.276923076923077,-0.261538461538462,-0.246153846153846,
-0.230769230769231,-0.215384615384615,-0.2,-0.184615384615385,-0.169230769230769,
-0.153846153846154,-0.138461538461538,-0.123076923076923,-0.107692307692308,
-0.0923076923076923,-0.0769230769230769,-0.0615384615384615,-0.0461538461538462,
-0.0307692307692308,-0.0153846153846154,0.),(-1.,1.),.UNSPECIFIED.)
GEOMETRIC_REPRESENTATION_ITEM()
RATIONAL_B_SPLINE_SURFACE(((1.,1.),(1.,1.),(1.,1.),(1.,1.),(1.,1.),(1.,
1.),(1.,1.),(1.,1.),(1.,1.),(1.,1.),(1.,1.),(1.,1.),(1.,1.),(1.,1.),(1.,
1.),(1.,1.),(1.,1.),(1.,1.),(1.,1.),(1.,1.),(1.,1.),(1.,1.),(1.,1.),(1.,
1.),(1.,1.),(1.,1.),(1.,1.),(1.,1.),(1.,1.),(1.,1.),(1.,1.),(1.,1.),(1.,
1.),(1.,1.),(1.,1.),(1.,1.),(1.,1.),(1.,1.),(1.,1.),(1.,1.),(1.,1.),(1.,
1.),(1.,1.),(1.,1.),(1.,1.),(1.,1.),(1.,1.),(1.,1.),(1.,1.),(1.,1.),(1.,
1.),(1.,1.),(1.,1.),(1.,1.),(1.,1.),(1.,1.),(1.,1.),(1.,1.),(1.,1.),(1.,
1.),(1.,1.),(1.,1.),(1.,1.),(1.,1.),(1.,1.),(1.,1.),(1.,1.),(1.,1.),(1.,
1.),(1.,1.)))
REPRESENTATION_ITEM('')
SURFACE()
);
#79=(
BOUNDED_SURFACE()
B_SPLINE_SURFACE(5,1,((#46664,#46665),(#46666,#46667),(#46668,#46669),(#46670,
#46671),(#46672,#46673),(#46674,#46675),(#46676,#46677),(#46678,#46679),
(#46680,#46681),(#46682,#46683),(#46684,#46685),(#46686,#46687),(#46688,
#46689),(#46690,#46691),(#46692,#46693),(#46694,#46695),(#46696,#46697),
(#46698,#46699),(#46700,#46701),(#46702,#46703),(#46704,#46705),(#46706,
#46707),(#46708,#46709),(#46710,#46711),(#46712,#46713),(#46714,#46715),
(#46716,#46717),(#46718,#46719),(#46720,#46721),(#46722,#46723),(#46724,
#46725),(#46726,#46727),(#46728,#46729),(#46730,#46731),(#46732,#46733),
(#46734,#46735),(#46736,#46737),(#46738,#46739),(#46740,#46741),(#46742,
#46743),(#46744,#46745),(#46746,#46747),(#46748,#46749),(#46750,#46751),
(#46752,#46753),(#46754,#46755),(#46756,#46757),(#46758,#46759),(#46760,
#46761),(#46762,#46763),(#46764,#46765),(#46766,#46767),(#46768,#46769),
(#46770,#46771),(#46772,#46773),(#46774,#46775),(#46776,#46777),(#46778,
#46779),(#46780,#46781),(#46782,#46783),(#46784,#46785),(#46786,#46787),
(#46788,#46789),(#46790,#46791),(#46792,#46793),(#46794,#46795),(#46796,
#46797),(#46798,#46799),(#46800,#46801),(#46802,#46803)),.UNSPECIFIED.,
 .F.,.F.,.F.)
B_SPLINE_SURFACE_WITH_KNOTS((6,1,1,1,1,1,1,1,1,1,1,1,1,1,1,1,1,1,1,1,1,
1,1,1,1,1,1,1,1,1,1,1,1,1,1,1,1,1,1,1,1,1,1,1,1,1,1,1,1,1,1,1,1,1,1,1,1,
1,1,1,1,1,1,1,1,6),(2,2),(-1.,-0.984615384615383,-0.969230769230768,-0.953846153846152,
-0.938461538461537,-0.923076923076922,-0.907692307692306,-0.892307692307691,
-0.876923076923076,-0.86153846153846,-0.846153846153845,-0.83076923076923,
-0.815384615384614,-0.799999999999999,-0.784615384615384,-0.769230769230768,
-0.753846153846153,-0.738461538461538,-0.723076923076922,-0.707692307692307,
-0.692307692307692,-0.676923076923076,-0.661538461538461,-0.646153846153846,
-0.63076923076923,-0.615384615384615,-0.6,-0.584615384615384,-0.569230769230769,
-0.553846153846154,-0.538461538461538,-0.523076923076923,-0.507692307692308,
-0.492307692307692,-0.476923076923077,-0.461538461538462,-0.446153846153846,
-0.430769230769231,-0.415384615384615,-0.4,-0.384615384615385,-0.369230769230769,
-0.353846153846154,-0.338461538461538,-0.323076923076923,-0.307692307692308,
-0.292307692307692,-0.276923076923077,-0.261538461538462,-0.246153846153846,
-0.230769230769231,-0.215384615384615,-0.2,-0.184615384615385,-0.169230769230769,
-0.153846153846154,-0.138461538461538,-0.123076923076923,-0.107692307692308,
-0.0923076923076923,-0.0769230769230769,-0.0615384615384615,-0.0461538461538462,
-0.0307692307692308,-0.0153846153846154,0.),(-1.,1.),.UNSPECIFIED.)
GEOMETRIC_REPRESENTATION_ITEM()
RATIONAL_B_SPLINE_SURFACE(((1.,1.),(1.,1.),(1.,1.),(1.,1.),(1.,1.),(1.,
1.),(1.,1.),(1.,1.),(1.,1.),(1.,1.),(1.,1.),(1.,1.),(1.,1.),(1.,1.),(1.,
1.),(1.,1.),(1.,1.),(1.,1.),(1.,1.),(1.,1.),(1.,1.),(1.,1.),(1.,1.),(1.,
1.),(1.,1.),(1.,1.),(1.,1.),(1.,1.),(1.,1.),(1.,1.),(1.,1.),(1.,1.),(1.,
1.),(1.,1.),(1.,1.),(1.,1.),(1.,1.),(1.,1.),(1.,1.),(1.,1.),(1.,1.),(1.,
1.),(1.,1.),(1.,1.),(1.,1.),(1.,1.),(1.,1.),(1.,1.),(1.,1.),(1.,1.),(1.,
1.),(1.,1.),(1.,1.),(1.,1.),(1.,1.),(1.,1.),(1.,1.),(1.,1.),(1.,1.),(1.,
1.),(1.,1.),(1.,1.),(1.,1.),(1.,1.),(1.,1.),(1.,1.),(1.,1.),(1.,1.),(1.,
1.),(1.,1.)))
REPRESENTATION_ITEM('')
SURFACE()
);
#80=(
BOUNDED_SURFACE()
B_SPLINE_SURFACE(5,1,((#46880,#46881),(#46882,#46883),(#46884,#46885),(#46886,
#46887),(#46888,#46889),(#46890,#46891),(#46892,#46893),(#46894,#46895),
(#46896,#46897),(#46898,#46899),(#46900,#46901),(#46902,#46903),(#46904,
#46905),(#46906,#46907),(#46908,#46909),(#46910,#46911),(#46912,#46913),
(#46914,#46915),(#46916,#46917),(#46918,#46919),(#46920,#46921),(#46922,
#46923),(#46924,#46925),(#46926,#46927),(#46928,#46929),(#46930,#46931),
(#46932,#46933),(#46934,#46935),(#46936,#46937),(#46938,#46939),(#46940,
#46941),(#46942,#46943),(#46944,#46945),(#46946,#46947),(#46948,#46949),
(#46950,#46951),(#46952,#46953),(#46954,#46955),(#46956,#46957),(#46958,
#46959),(#46960,#46961),(#46962,#46963),(#46964,#46965),(#46966,#46967),
(#46968,#46969),(#46970,#46971),(#46972,#46973),(#46974,#46975),(#46976,
#46977),(#46978,#46979),(#46980,#46981),(#46982,#46983),(#46984,#46985),
(#46986,#46987),(#46988,#46989),(#46990,#46991),(#46992,#46993),(#46994,
#46995),(#46996,#46997),(#46998,#46999),(#47000,#47001),(#47002,#47003),
(#47004,#47005),(#47006,#47007),(#47008,#47009),(#47010,#47011),(#47012,
#47013),(#47014,#47015),(#47016,#47017),(#47018,#47019)),.UNSPECIFIED.,
 .F.,.F.,.F.)
B_SPLINE_SURFACE_WITH_KNOTS((6,1,1,1,1,1,1,1,1,1,1,1,1,1,1,1,1,1,1,1,1,
1,1,1,1,1,1,1,1,1,1,1,1,1,1,1,1,1,1,1,1,1,1,1,1,1,1,1,1,1,1,1,1,1,1,1,1,
1,1,1,1,1,1,1,1,6),(2,2),(-1.,-0.984615384615383,-0.969230769230768,-0.953846153846152,
-0.938461538461537,-0.923076923076922,-0.907692307692306,-0.892307692307691,
-0.876923076923076,-0.86153846153846,-0.846153846153845,-0.83076923076923,
-0.815384615384614,-0.799999999999999,-0.784615384615384,-0.769230769230768,
-0.753846153846153,-0.738461538461538,-0.723076923076922,-0.707692307692307,
-0.692307692307692,-0.676923076923076,-0.661538461538461,-0.646153846153846,
-0.63076923076923,-0.615384615384615,-0.6,-0.584615384615384,-0.569230769230769,
-0.553846153846154,-0.538461538461538,-0.523076923076923,-0.507692307692308,
-0.492307692307692,-0.476923076923077,-0.461538461538462,-0.446153846153846,
-0.430769230769231,-0.415384615384615,-0.4,-0.384615384615385,-0.369230769230769,
-0.353846153846154,-0.338461538461538,-0.323076923076923,-0.307692307692308,
-0.292307692307692,-0.276923076923077,-0.261538461538462,-0.246153846153846,
-0.230769230769231,-0.215384615384615,-0.2,-0.184615384615385,-0.169230769230769,
-0.153846153846154,-0.138461538461538,-0.123076923076923,-0.107692307692308,
-0.0923076923076923,-0.0769230769230769,-0.0615384615384615,-0.0461538461538462,
-0.0307692307692308,-0.0153846153846154,0.),(-1.,1.),.UNSPECIFIED.)
GEOMETRIC_REPRESENTATION_ITEM()
RATIONAL_B_SPLINE_SURFACE(((1.,1.),(1.,1.),(1.,1.),(1.,1.),(1.,1.),(1.,
1.),(1.,1.),(1.,1.),(1.,1.),(1.,1.),(1.,1.),(1.,1.),(1.,1.),(1.,1.),(1.,
1.),(1.,1.),(1.,1.),(1.,1.),(1.,1.),(1.,1.),(1.,1.),(1.,1.),(1.,1.),(1.,
1.),(1.,1.),(1.,1.),(1.,1.),(1.,1.),(1.,1.),(1.,1.),(1.,1.),(1.,1.),(1.,
1.),(1.,1.),(1.,1.),(1.,1.),(1.,1.),(1.,1.),(1.,1.),(1.,1.),(1.,1.),(1.,
1.),(1.,1.),(1.,1.),(1.,1.),(1.,1.),(1.,1.),(1.,1.),(1.,1.),(1.,1.),(1.,
1.),(1.,1.),(1.,1.),(1.,1.),(1.,1.),(1.,1.),(1.,1.),(1.,1.),(1.,1.),(1.,
1.),(1.,1.),(1.,1.),(1.,1.),(1.,1.),(1.,1.),(1.,1.),(1.,1.),(1.,1.),(1.,
1.),(1.,1.)))
REPRESENTATION_ITEM('')
SURFACE()
);
#81=(
BOUNDED_SURFACE()
B_SPLINE_SURFACE(5,1,((#47096,#47097),(#47098,#47099),(#47100,#47101),(#47102,
#47103),(#47104,#47105),(#47106,#47107),(#47108,#47109),(#47110,#47111),
(#47112,#47113),(#47114,#47115),(#47116,#47117),(#47118,#47119),(#47120,
#47121),(#47122,#47123),(#47124,#47125),(#47126,#47127),(#47128,#47129),
(#47130,#47131),(#47132,#47133),(#47134,#47135),(#47136,#47137),(#47138,
#47139),(#47140,#47141),(#47142,#47143),(#47144,#47145),(#47146,#47147),
(#47148,#47149),(#47150,#47151),(#47152,#47153),(#47154,#47155),(#47156,
#47157),(#47158,#47159),(#47160,#47161),(#47162,#47163),(#47164,#47165),
(#47166,#47167),(#47168,#47169),(#47170,#47171),(#47172,#47173),(#47174,
#47175),(#47176,#47177),(#47178,#47179),(#47180,#47181),(#47182,#47183),
(#47184,#47185),(#47186,#47187),(#47188,#47189),(#47190,#47191),(#47192,
#47193),(#47194,#47195),(#47196,#47197),(#47198,#47199),(#47200,#47201),
(#47202,#47203),(#47204,#47205),(#47206,#47207),(#47208,#47209),(#47210,
#47211),(#47212,#47213),(#47214,#47215),(#47216,#47217),(#47218,#47219),
(#47220,#47221),(#47222,#47223),(#47224,#47225),(#47226,#47227),(#47228,
#47229),(#47230,#47231),(#47232,#47233),(#47234,#47235)),.UNSPECIFIED.,
 .F.,.F.,.F.)
B_SPLINE_SURFACE_WITH_KNOTS((6,1,1,1,1,1,1,1,1,1,1,1,1,1,1,1,1,1,1,1,1,
1,1,1,1,1,1,1,1,1,1,1,1,1,1,1,1,1,1,1,1,1,1,1,1,1,1,1,1,1,1,1,1,1,1,1,1,
1,1,1,1,1,1,1,1,6),(2,2),(-1.,-0.984615384615383,-0.969230769230768,-0.953846153846152,
-0.938461538461537,-0.923076923076922,-0.907692307692306,-0.892307692307691,
-0.876923076923076,-0.86153846153846,-0.846153846153845,-0.83076923076923,
-0.815384615384614,-0.799999999999999,-0.784615384615384,-0.769230769230768,
-0.753846153846153,-0.738461538461538,-0.723076923076922,-0.707692307692307,
-0.692307692307692,-0.676923076923076,-0.661538461538461,-0.646153846153846,
-0.63076923076923,-0.615384615384615,-0.6,-0.584615384615384,-0.569230769230769,
-0.553846153846154,-0.538461538461538,-0.523076923076923,-0.507692307692308,
-0.492307692307692,-0.476923076923077,-0.461538461538462,-0.446153846153846,
-0.430769230769231,-0.415384615384615,-0.4,-0.384615384615385,-0.369230769230769,
-0.353846153846154,-0.338461538461538,-0.323076923076923,-0.307692307692308,
-0.292307692307692,-0.276923076923077,-0.261538461538462,-0.246153846153846,
-0.230769230769231,-0.215384615384615,-0.2,-0.184615384615385,-0.169230769230769,
-0.153846153846154,-0.138461538461538,-0.123076923076923,-0.107692307692308,
-0.0923076923076923,-0.0769230769230769,-0.0615384615384615,-0.0461538461538462,
-0.0307692307692308,-0.0153846153846154,0.),(-1.,1.),.UNSPECIFIED.)
GEOMETRIC_REPRESENTATION_ITEM()
RATIONAL_B_SPLINE_SURFACE(((1.,1.),(1.,1.),(1.,1.),(1.,1.),(1.,1.),(1.,
1.),(1.,1.),(1.,1.),(1.,1.),(1.,1.),(1.,1.),(1.,1.),(1.,1.),(1.,1.),(1.,
1.),(1.,1.),(1.,1.),(1.,1.),(1.,1.),(1.,1.),(1.,1.),(1.,1.),(1.,1.),(1.,
1.),(1.,1.),(1.,1.),(1.,1.),(1.,1.),(1.,1.),(1.,1.),(1.,1.),(1.,1.),(1.,
1.),(1.,1.),(1.,1.),(1.,1.),(1.,1.),(1.,1.),(1.,1.),(1.,1.),(1.,1.),(1.,
1.),(1.,1.),(1.,1.),(1.,1.),(1.,1.),(1.,1.),(1.,1.),(1.,1.),(1.,1.),(1.,
1.),(1.,1.),(1.,1.),(1.,1.),(1.,1.),(1.,1.),(1.,1.),(1.,1.),(1.,1.),(1.,
1.),(1.,1.),(1.,1.),(1.,1.),(1.,1.),(1.,1.),(1.,1.),(1.,1.),(1.,1.),(1.,
1.),(1.,1.)))
REPRESENTATION_ITEM('')
SURFACE()
);
#82=(
BOUNDED_SURFACE()
B_SPLINE_SURFACE(5,1,((#47312,#47313),(#47314,#47315),(#47316,#47317),(#47318,
#47319),(#47320,#47321),(#47322,#47323),(#47324,#47325),(#47326,#47327),
(#47328,#47329),(#47330,#47331),(#47332,#47333),(#47334,#47335),(#47336,
#47337),(#47338,#47339),(#47340,#47341),(#47342,#47343),(#47344,#47345),
(#47346,#47347),(#47348,#47349),(#47350,#47351),(#47352,#47353),(#47354,
#47355),(#47356,#47357),(#47358,#47359),(#47360,#47361),(#47362,#47363),
(#47364,#47365),(#47366,#47367),(#47368,#47369),(#47370,#47371),(#47372,
#47373),(#47374,#47375),(#47376,#47377),(#47378,#47379),(#47380,#47381),
(#47382,#47383),(#47384,#47385),(#47386,#47387),(#47388,#47389),(#47390,
#47391),(#47392,#47393),(#47394,#47395),(#47396,#47397),(#47398,#47399),
(#47400,#47401),(#47402,#47403),(#47404,#47405),(#47406,#47407),(#47408,
#47409),(#47410,#47411),(#47412,#47413),(#47414,#47415),(#47416,#47417),
(#47418,#47419),(#47420,#47421),(#47422,#47423),(#47424,#47425),(#47426,
#47427),(#47428,#47429),(#47430,#47431),(#47432,#47433),(#47434,#47435),
(#47436,#47437),(#47438,#47439),(#47440,#47441),(#47442,#47443),(#47444,
#47445),(#47446,#47447),(#47448,#47449),(#47450,#47451)),.UNSPECIFIED.,
 .F.,.F.,.F.)
B_SPLINE_SURFACE_WITH_KNOTS((6,1,1,1,1,1,1,1,1,1,1,1,1,1,1,1,1,1,1,1,1,
1,1,1,1,1,1,1,1,1,1,1,1,1,1,1,1,1,1,1,1,1,1,1,1,1,1,1,1,1,1,1,1,1,1,1,1,
1,1,1,1,1,1,1,1,6),(2,2),(-1.,-0.984615384615383,-0.969230769230768,-0.953846153846152,
-0.938461538461537,-0.923076923076922,-0.907692307692306,-0.892307692307691,
-0.876923076923076,-0.86153846153846,-0.846153846153845,-0.83076923076923,
-0.815384615384614,-0.799999999999999,-0.784615384615384,-0.769230769230768,
-0.753846153846153,-0.738461538461538,-0.723076923076922,-0.707692307692307,
-0.692307692307692,-0.676923076923076,-0.661538461538461,-0.646153846153846,
-0.63076923076923,-0.615384615384615,-0.6,-0.584615384615384,-0.569230769230769,
-0.553846153846154,-0.538461538461538,-0.523076923076923,-0.507692307692308,
-0.492307692307692,-0.476923076923077,-0.461538461538462,-0.446153846153846,
-0.430769230769231,-0.415384615384615,-0.4,-0.384615384615385,-0.369230769230769,
-0.353846153846154,-0.338461538461538,-0.323076923076923,-0.307692307692308,
-0.292307692307692,-0.276923076923077,-0.261538461538462,-0.246153846153846,
-0.230769230769231,-0.215384615384615,-0.2,-0.184615384615385,-0.169230769230769,
-0.153846153846154,-0.138461538461538,-0.123076923076923,-0.107692307692308,
-0.0923076923076923,-0.0769230769230769,-0.0615384615384615,-0.0461538461538462,
-0.0307692307692308,-0.0153846153846154,0.),(-1.,1.),.UNSPECIFIED.)
GEOMETRIC_REPRESENTATION_ITEM()
RATIONAL_B_SPLINE_SURFACE(((1.,1.),(1.,1.),(1.,1.),(1.,1.),(1.,1.),(1.,
1.),(1.,1.),(1.,1.),(1.,1.),(1.,1.),(1.,1.),(1.,1.),(1.,1.),(1.,1.),(1.,
1.),(1.,1.),(1.,1.),(1.,1.),(1.,1.),(1.,1.),(1.,1.),(1.,1.),(1.,1.),(1.,
1.),(1.,1.),(1.,1.),(1.,1.),(1.,1.),(1.,1.),(1.,1.),(1.,1.),(1.,1.),(1.,
1.),(1.,1.),(1.,1.),(1.,1.),(1.,1.),(1.,1.),(1.,1.),(1.,1.),(1.,1.),(1.,
1.),(1.,1.),(1.,1.),(1.,1.),(1.,1.),(1.,1.),(1.,1.),(1.,1.),(1.,1.),(1.,
1.),(1.,1.),(1.,1.),(1.,1.),(1.,1.),(1.,1.),(1.,1.),(1.,1.),(1.,1.),(1.,
1.),(1.,1.),(1.,1.),(1.,1.),(1.,1.),(1.,1.),(1.,1.),(1.,1.),(1.,1.),(1.,
1.),(1.,1.)))
REPRESENTATION_ITEM('')
SURFACE()
);
#83=(
BOUNDED_SURFACE()
B_SPLINE_SURFACE(5,1,((#47528,#47529),(#47530,#47531),(#47532,#47533),(#47534,
#47535),(#47536,#47537),(#47538,#47539),(#47540,#47541),(#47542,#47543),
(#47544,#47545),(#47546,#47547),(#47548,#47549),(#47550,#47551),(#47552,
#47553),(#47554,#47555),(#47556,#47557),(#47558,#47559),(#47560,#47561),
(#47562,#47563),(#47564,#47565),(#47566,#47567),(#47568,#47569),(#47570,
#47571),(#47572,#47573),(#47574,#47575),(#47576,#47577),(#47578,#47579),
(#47580,#47581),(#47582,#47583),(#47584,#47585),(#47586,#47587),(#47588,
#47589),(#47590,#47591),(#47592,#47593),(#47594,#47595),(#47596,#47597),
(#47598,#47599),(#47600,#47601),(#47602,#47603),(#47604,#47605),(#47606,
#47607),(#47608,#47609),(#47610,#47611),(#47612,#47613),(#47614,#47615),
(#47616,#47617),(#47618,#47619),(#47620,#47621),(#47622,#47623),(#47624,
#47625),(#47626,#47627),(#47628,#47629),(#47630,#47631),(#47632,#47633),
(#47634,#47635),(#47636,#47637),(#47638,#47639),(#47640,#47641),(#47642,
#47643),(#47644,#47645),(#47646,#47647),(#47648,#47649),(#47650,#47651),
(#47652,#47653),(#47654,#47655),(#47656,#47657),(#47658,#47659),(#47660,
#47661),(#47662,#47663),(#47664,#47665),(#47666,#47667)),.UNSPECIFIED.,
 .F.,.F.,.F.)
B_SPLINE_SURFACE_WITH_KNOTS((6,1,1,1,1,1,1,1,1,1,1,1,1,1,1,1,1,1,1,1,1,
1,1,1,1,1,1,1,1,1,1,1,1,1,1,1,1,1,1,1,1,1,1,1,1,1,1,1,1,1,1,1,1,1,1,1,1,
1,1,1,1,1,1,1,1,6),(2,2),(-1.,-0.984615384615383,-0.969230769230768,-0.953846153846152,
-0.938461538461537,-0.923076923076922,-0.907692307692306,-0.892307692307691,
-0.876923076923076,-0.86153846153846,-0.846153846153845,-0.83076923076923,
-0.815384615384614,-0.799999999999999,-0.784615384615384,-0.769230769230768,
-0.753846153846153,-0.738461538461538,-0.723076923076922,-0.707692307692307,
-0.692307692307692,-0.676923076923076,-0.661538461538461,-0.646153846153846,
-0.63076923076923,-0.615384615384615,-0.6,-0.584615384615384,-0.569230769230769,
-0.553846153846154,-0.538461538461538,-0.523076923076923,-0.507692307692308,
-0.492307692307692,-0.476923076923077,-0.461538461538462,-0.446153846153846,
-0.430769230769231,-0.415384615384615,-0.4,-0.384615384615385,-0.369230769230769,
-0.353846153846154,-0.338461538461538,-0.323076923076923,-0.307692307692308,
-0.292307692307692,-0.276923076923077,-0.261538461538462,-0.246153846153846,
-0.230769230769231,-0.215384615384615,-0.2,-0.184615384615385,-0.169230769230769,
-0.153846153846154,-0.138461538461538,-0.123076923076923,-0.107692307692308,
-0.0923076923076923,-0.0769230769230769,-0.0615384615384615,-0.0461538461538462,
-0.0307692307692308,-0.0153846153846154,0.),(-1.,1.),.UNSPECIFIED.)
GEOMETRIC_REPRESENTATION_ITEM()
RATIONAL_B_SPLINE_SURFACE(((1.,1.),(1.,1.),(1.,1.),(1.,1.),(1.,1.),(1.,
1.),(1.,1.),(1.,1.),(1.,1.),(1.,1.),(1.,1.),(1.,1.),(1.,1.),(1.,1.),(1.,
1.),(1.,1.),(1.,1.),(1.,1.),(1.,1.),(1.,1.),(1.,1.),(1.,1.),(1.,1.),(1.,
1.),(1.,1.),(1.,1.),(1.,1.),(1.,1.),(1.,1.),(1.,1.),(1.,1.),(1.,1.),(1.,
1.),(1.,1.),(1.,1.),(1.,1.),(1.,1.),(1.,1.),(1.,1.),(1.,1.),(1.,1.),(1.,
1.),(1.,1.),(1.,1.),(1.,1.),(1.,1.),(1.,1.),(1.,1.),(1.,1.),(1.,1.),(1.,
1.),(1.,1.),(1.,1.),(1.,1.),(1.,1.),(1.,1.),(1.,1.),(1.,1.),(1.,1.),(1.,
1.),(1.,1.),(1.,1.),(1.,1.),(1.,1.),(1.,1.),(1.,1.),(1.,1.),(1.,1.),(1.,
1.),(1.,1.)))
REPRESENTATION_ITEM('')
SURFACE()
);
#84=(
BOUNDED_SURFACE()
B_SPLINE_SURFACE(5,1,((#47744,#47745),(#47746,#47747),(#47748,#47749),(#47750,
#47751),(#47752,#47753),(#47754,#47755),(#47756,#47757),(#47758,#47759),
(#47760,#47761),(#47762,#47763),(#47764,#47765),(#47766,#47767),(#47768,
#47769),(#47770,#47771),(#47772,#47773),(#47774,#47775),(#47776,#47777),
(#47778,#47779),(#47780,#47781),(#47782,#47783),(#47784,#47785),(#47786,
#47787),(#47788,#47789),(#47790,#47791),(#47792,#47793),(#47794,#47795),
(#47796,#47797),(#47798,#47799),(#47800,#47801),(#47802,#47803),(#47804,
#47805),(#47806,#47807),(#47808,#47809),(#47810,#47811),(#47812,#47813),
(#47814,#47815),(#47816,#47817),(#47818,#47819),(#47820,#47821),(#47822,
#47823),(#47824,#47825),(#47826,#47827),(#47828,#47829),(#47830,#47831),
(#47832,#47833),(#47834,#47835),(#47836,#47837),(#47838,#47839),(#47840,
#47841),(#47842,#47843),(#47844,#47845),(#47846,#47847),(#47848,#47849),
(#47850,#47851),(#47852,#47853),(#47854,#47855),(#47856,#47857),(#47858,
#47859),(#47860,#47861),(#47862,#47863),(#47864,#47865),(#47866,#47867),
(#47868,#47869),(#47870,#47871),(#47872,#47873),(#47874,#47875),(#47876,
#47877),(#47878,#47879),(#47880,#47881),(#47882,#47883)),.UNSPECIFIED.,
 .F.,.F.,.F.)
B_SPLINE_SURFACE_WITH_KNOTS((6,1,1,1,1,1,1,1,1,1,1,1,1,1,1,1,1,1,1,1,1,
1,1,1,1,1,1,1,1,1,1,1,1,1,1,1,1,1,1,1,1,1,1,1,1,1,1,1,1,1,1,1,1,1,1,1,1,
1,1,1,1,1,1,1,1,6),(2,2),(-1.,-0.984615384615383,-0.969230769230768,-0.953846153846152,
-0.938461538461537,-0.923076923076922,-0.907692307692306,-0.892307692307691,
-0.876923076923076,-0.86153846153846,-0.846153846153845,-0.83076923076923,
-0.815384615384614,-0.799999999999999,-0.784615384615384,-0.769230769230768,
-0.753846153846153,-0.738461538461538,-0.723076923076922,-0.707692307692307,
-0.692307692307692,-0.676923076923076,-0.661538461538461,-0.646153846153846,
-0.63076923076923,-0.615384615384615,-0.6,-0.584615384615384,-0.569230769230769,
-0.553846153846154,-0.538461538461538,-0.523076923076923,-0.507692307692308,
-0.492307692307692,-0.476923076923077,-0.461538461538462,-0.446153846153846,
-0.430769230769231,-0.415384615384615,-0.4,-0.384615384615385,-0.369230769230769,
-0.353846153846154,-0.338461538461538,-0.323076923076923,-0.307692307692308,
-0.292307692307692,-0.276923076923077,-0.261538461538462,-0.246153846153846,
-0.230769230769231,-0.215384615384615,-0.2,-0.184615384615385,-0.169230769230769,
-0.153846153846154,-0.138461538461538,-0.123076923076923,-0.107692307692308,
-0.0923076923076923,-0.0769230769230769,-0.0615384615384615,-0.0461538461538462,
-0.0307692307692308,-0.0153846153846154,0.),(-1.,1.),.UNSPECIFIED.)
GEOMETRIC_REPRESENTATION_ITEM()
RATIONAL_B_SPLINE_SURFACE(((1.,1.),(1.,1.),(1.,1.),(1.,1.),(1.,1.),(1.,
1.),(1.,1.),(1.,1.),(1.,1.),(1.,1.),(1.,1.),(1.,1.),(1.,1.),(1.,1.),(1.,
1.),(1.,1.),(1.,1.),(1.,1.),(1.,1.),(1.,1.),(1.,1.),(1.,1.),(1.,1.),(1.,
1.),(1.,1.),(1.,1.),(1.,1.),(1.,1.),(1.,1.),(1.,1.),(1.,1.),(1.,1.),(1.,
1.),(1.,1.),(1.,1.),(1.,1.),(1.,1.),(1.,1.),(1.,1.),(1.,1.),(1.,1.),(1.,
1.),(1.,1.),(1.,1.),(1.,1.),(1.,1.),(1.,1.),(1.,1.),(1.,1.),(1.,1.),(1.,
1.),(1.,1.),(1.,1.),(1.,1.),(1.,1.),(1.,1.),(1.,1.),(1.,1.),(1.,1.),(1.,
1.),(1.,1.),(1.,1.),(1.,1.),(1.,1.),(1.,1.),(1.,1.),(1.,1.),(1.,1.),(1.,
1.),(1.,1.)))
REPRESENTATION_ITEM('')
SURFACE()
);
#85=(
BOUNDED_SURFACE()
B_SPLINE_SURFACE(5,1,((#47960,#47961),(#47962,#47963),(#47964,#47965),(#47966,
#47967),(#47968,#47969),(#47970,#47971),(#47972,#47973),(#47974,#47975),
(#47976,#47977),(#47978,#47979),(#47980,#47981),(#47982,#47983),(#47984,
#47985),(#47986,#47987),(#47988,#47989),(#47990,#47991),(#47992,#47993),
(#47994,#47995),(#47996,#47997),(#47998,#47999),(#48000,#48001),(#48002,
#48003),(#48004,#48005),(#48006,#48007),(#48008,#48009),(#48010,#48011),
(#48012,#48013),(#48014,#48015),(#48016,#48017),(#48018,#48019),(#48020,
#48021),(#48022,#48023),(#48024,#48025),(#48026,#48027),(#48028,#48029),
(#48030,#48031),(#48032,#48033),(#48034,#48035),(#48036,#48037),(#48038,
#48039),(#48040,#48041),(#48042,#48043),(#48044,#48045),(#48046,#48047),
(#48048,#48049),(#48050,#48051),(#48052,#48053),(#48054,#48055),(#48056,
#48057),(#48058,#48059),(#48060,#48061),(#48062,#48063),(#48064,#48065),
(#48066,#48067),(#48068,#48069),(#48070,#48071),(#48072,#48073),(#48074,
#48075),(#48076,#48077),(#48078,#48079),(#48080,#48081),(#48082,#48083),
(#48084,#48085),(#48086,#48087),(#48088,#48089),(#48090,#48091),(#48092,
#48093),(#48094,#48095),(#48096,#48097),(#48098,#48099)),.UNSPECIFIED.,
 .F.,.F.,.F.)
B_SPLINE_SURFACE_WITH_KNOTS((6,1,1,1,1,1,1,1,1,1,1,1,1,1,1,1,1,1,1,1,1,
1,1,1,1,1,1,1,1,1,1,1,1,1,1,1,1,1,1,1,1,1,1,1,1,1,1,1,1,1,1,1,1,1,1,1,1,
1,1,1,1,1,1,1,1,6),(2,2),(-1.,-0.984615384615383,-0.969230769230768,-0.953846153846152,
-0.938461538461537,-0.923076923076922,-0.907692307692306,-0.892307692307691,
-0.876923076923076,-0.86153846153846,-0.846153846153845,-0.83076923076923,
-0.815384615384614,-0.799999999999999,-0.784615384615384,-0.769230769230768,
-0.753846153846153,-0.738461538461538,-0.723076923076922,-0.707692307692307,
-0.692307692307692,-0.676923076923076,-0.661538461538461,-0.646153846153846,
-0.63076923076923,-0.615384615384615,-0.6,-0.584615384615384,-0.569230769230769,
-0.553846153846154,-0.538461538461538,-0.523076923076923,-0.507692307692308,
-0.492307692307692,-0.476923076923077,-0.461538461538462,-0.446153846153846,
-0.430769230769231,-0.415384615384615,-0.4,-0.384615384615385,-0.369230769230769,
-0.353846153846154,-0.338461538461538,-0.323076923076923,-0.307692307692308,
-0.292307692307692,-0.276923076923077,-0.261538461538462,-0.246153846153846,
-0.230769230769231,-0.215384615384615,-0.2,-0.184615384615385,-0.169230769230769,
-0.153846153846154,-0.138461538461538,-0.123076923076923,-0.107692307692308,
-0.0923076923076923,-0.0769230769230769,-0.0615384615384615,-0.0461538461538462,
-0.0307692307692308,-0.0153846153846154,0.),(-1.,1.),.UNSPECIFIED.)
GEOMETRIC_REPRESENTATION_ITEM()
RATIONAL_B_SPLINE_SURFACE(((1.,1.),(1.,1.),(1.,1.),(1.,1.),(1.,1.),(1.,
1.),(1.,1.),(1.,1.),(1.,1.),(1.,1.),(1.,1.),(1.,1.),(1.,1.),(1.,1.),(1.,
1.),(1.,1.),(1.,1.),(1.,1.),(1.,1.),(1.,1.),(1.,1.),(1.,1.),(1.,1.),(1.,
1.),(1.,1.),(1.,1.),(1.,1.),(1.,1.),(1.,1.),(1.,1.),(1.,1.),(1.,1.),(1.,
1.),(1.,1.),(1.,1.),(1.,1.),(1.,1.),(1.,1.),(1.,1.),(1.,1.),(1.,1.),(1.,
1.),(1.,1.),(1.,1.),(1.,1.),(1.,1.),(1.,1.),(1.,1.),(1.,1.),(1.,1.),(1.,
1.),(1.,1.),(1.,1.),(1.,1.),(1.,1.),(1.,1.),(1.,1.),(1.,1.),(1.,1.),(1.,
1.),(1.,1.),(1.,1.),(1.,1.),(1.,1.),(1.,1.),(1.,1.),(1.,1.),(1.,1.),(1.,
1.),(1.,1.)))
REPRESENTATION_ITEM('')
SURFACE()
);
#86=(
BOUNDED_SURFACE()
B_SPLINE_SURFACE(5,1,((#48176,#48177),(#48178,#48179),(#48180,#48181),(#48182,
#48183),(#48184,#48185),(#48186,#48187),(#48188,#48189),(#48190,#48191),
(#48192,#48193),(#48194,#48195),(#48196,#48197),(#48198,#48199),(#48200,
#48201),(#48202,#48203),(#48204,#48205),(#48206,#48207),(#48208,#48209),
(#48210,#48211),(#48212,#48213),(#48214,#48215),(#48216,#48217),(#48218,
#48219),(#48220,#48221),(#48222,#48223),(#48224,#48225),(#48226,#48227),
(#48228,#48229),(#48230,#48231),(#48232,#48233),(#48234,#48235),(#48236,
#48237),(#48238,#48239),(#48240,#48241),(#48242,#48243),(#48244,#48245),
(#48246,#48247),(#48248,#48249),(#48250,#48251),(#48252,#48253),(#48254,
#48255),(#48256,#48257),(#48258,#48259),(#48260,#48261),(#48262,#48263),
(#48264,#48265),(#48266,#48267),(#48268,#48269),(#48270,#48271),(#48272,
#48273),(#48274,#48275),(#48276,#48277),(#48278,#48279),(#48280,#48281),
(#48282,#48283),(#48284,#48285),(#48286,#48287),(#48288,#48289),(#48290,
#48291),(#48292,#48293),(#48294,#48295),(#48296,#48297),(#48298,#48299),
(#48300,#48301),(#48302,#48303),(#48304,#48305),(#48306,#48307),(#48308,
#48309),(#48310,#48311),(#48312,#48313),(#48314,#48315)),.UNSPECIFIED.,
 .F.,.F.,.F.)
B_SPLINE_SURFACE_WITH_KNOTS((6,1,1,1,1,1,1,1,1,1,1,1,1,1,1,1,1,1,1,1,1,
1,1,1,1,1,1,1,1,1,1,1,1,1,1,1,1,1,1,1,1,1,1,1,1,1,1,1,1,1,1,1,1,1,1,1,1,
1,1,1,1,1,1,1,1,6),(2,2),(-1.,-0.984615384615383,-0.969230769230768,-0.953846153846152,
-0.938461538461537,-0.923076923076922,-0.907692307692306,-0.892307692307691,
-0.876923076923076,-0.86153846153846,-0.846153846153845,-0.83076923076923,
-0.815384615384614,-0.799999999999999,-0.784615384615384,-0.769230769230768,
-0.753846153846153,-0.738461538461538,-0.723076923076922,-0.707692307692307,
-0.692307692307692,-0.676923076923076,-0.661538461538461,-0.646153846153846,
-0.63076923076923,-0.615384615384615,-0.6,-0.584615384615384,-0.569230769230769,
-0.553846153846154,-0.538461538461538,-0.523076923076923,-0.507692307692308,
-0.492307692307692,-0.476923076923077,-0.461538461538462,-0.446153846153846,
-0.430769230769231,-0.415384615384615,-0.4,-0.384615384615385,-0.369230769230769,
-0.353846153846154,-0.338461538461538,-0.323076923076923,-0.307692307692308,
-0.292307692307692,-0.276923076923077,-0.261538461538462,-0.246153846153846,
-0.230769230769231,-0.215384615384615,-0.2,-0.184615384615385,-0.169230769230769,
-0.153846153846154,-0.138461538461538,-0.123076923076923,-0.107692307692308,
-0.0923076923076923,-0.0769230769230769,-0.0615384615384615,-0.0461538461538462,
-0.0307692307692308,-0.0153846153846154,0.),(-1.,1.),.UNSPECIFIED.)
GEOMETRIC_REPRESENTATION_ITEM()
RATIONAL_B_SPLINE_SURFACE(((1.,1.),(1.,1.),(1.,1.),(1.,1.),(1.,1.),(1.,
1.),(1.,1.),(1.,1.),(1.,1.),(1.,1.),(1.,1.),(1.,1.),(1.,1.),(1.,1.),(1.,
1.),(1.,1.),(1.,1.),(1.,1.),(1.,1.),(1.,1.),(1.,1.),(1.,1.),(1.,1.),(1.,
1.),(1.,1.),(1.,1.),(1.,1.),(1.,1.),(1.,1.),(1.,1.),(1.,1.),(1.,1.),(1.,
1.),(1.,1.),(1.,1.),(1.,1.),(1.,1.),(1.,1.),(1.,1.),(1.,1.),(1.,1.),(1.,
1.),(1.,1.),(1.,1.),(1.,1.),(1.,1.),(1.,1.),(1.,1.),(1.,1.),(1.,1.),(1.,
1.),(1.,1.),(1.,1.),(1.,1.),(1.,1.),(1.,1.),(1.,1.),(1.,1.),(1.,1.),(1.,
1.),(1.,1.),(1.,1.),(1.,1.),(1.,1.),(1.,1.),(1.,1.),(1.,1.),(1.,1.),(1.,
1.),(1.,1.)))
REPRESENTATION_ITEM('')
SURFACE()
);
#87=(
BOUNDED_SURFACE()
B_SPLINE_SURFACE(5,1,((#48392,#48393),(#48394,#48395),(#48396,#48397),(#48398,
#48399),(#48400,#48401),(#48402,#48403),(#48404,#48405),(#48406,#48407),
(#48408,#48409),(#48410,#48411),(#48412,#48413),(#48414,#48415),(#48416,
#48417),(#48418,#48419),(#48420,#48421),(#48422,#48423),(#48424,#48425),
(#48426,#48427),(#48428,#48429),(#48430,#48431),(#48432,#48433),(#48434,
#48435),(#48436,#48437),(#48438,#48439),(#48440,#48441),(#48442,#48443),
(#48444,#48445),(#48446,#48447),(#48448,#48449),(#48450,#48451),(#48452,
#48453),(#48454,#48455),(#48456,#48457),(#48458,#48459),(#48460,#48461),
(#48462,#48463),(#48464,#48465),(#48466,#48467),(#48468,#48469),(#48470,
#48471),(#48472,#48473),(#48474,#48475),(#48476,#48477),(#48478,#48479),
(#48480,#48481),(#48482,#48483),(#48484,#48485),(#48486,#48487),(#48488,
#48489),(#48490,#48491),(#48492,#48493),(#48494,#48495),(#48496,#48497),
(#48498,#48499),(#48500,#48501),(#48502,#48503),(#48504,#48505),(#48506,
#48507),(#48508,#48509),(#48510,#48511),(#48512,#48513),(#48514,#48515),
(#48516,#48517),(#48518,#48519),(#48520,#48521),(#48522,#48523),(#48524,
#48525),(#48526,#48527),(#48528,#48529),(#48530,#48531)),.UNSPECIFIED.,
 .F.,.F.,.F.)
B_SPLINE_SURFACE_WITH_KNOTS((6,1,1,1,1,1,1,1,1,1,1,1,1,1,1,1,1,1,1,1,1,
1,1,1,1,1,1,1,1,1,1,1,1,1,1,1,1,1,1,1,1,1,1,1,1,1,1,1,1,1,1,1,1,1,1,1,1,
1,1,1,1,1,1,1,1,6),(2,2),(-1.,-0.984615384615383,-0.969230769230768,-0.953846153846152,
-0.938461538461537,-0.923076923076922,-0.907692307692306,-0.892307692307691,
-0.876923076923076,-0.86153846153846,-0.846153846153845,-0.83076923076923,
-0.815384615384614,-0.799999999999999,-0.784615384615384,-0.769230769230768,
-0.753846153846153,-0.738461538461538,-0.723076923076922,-0.707692307692307,
-0.692307692307692,-0.676923076923076,-0.661538461538461,-0.646153846153846,
-0.63076923076923,-0.615384615384615,-0.6,-0.584615384615384,-0.569230769230769,
-0.553846153846154,-0.538461538461538,-0.523076923076923,-0.507692307692308,
-0.492307692307692,-0.476923076923077,-0.461538461538462,-0.446153846153846,
-0.430769230769231,-0.415384615384615,-0.4,-0.384615384615385,-0.369230769230769,
-0.353846153846154,-0.338461538461538,-0.323076923076923,-0.307692307692308,
-0.292307692307692,-0.276923076923077,-0.261538461538462,-0.246153846153846,
-0.230769230769231,-0.215384615384615,-0.2,-0.184615384615385,-0.169230769230769,
-0.153846153846154,-0.138461538461538,-0.123076923076923,-0.107692307692308,
-0.0923076923076923,-0.0769230769230769,-0.0615384615384615,-0.0461538461538462,
-0.0307692307692308,-0.0153846153846154,0.),(-1.,1.),.UNSPECIFIED.)
GEOMETRIC_REPRESENTATION_ITEM()
RATIONAL_B_SPLINE_SURFACE(((1.,1.),(1.,1.),(1.,1.),(1.,1.),(1.,1.),(1.,
1.),(1.,1.),(1.,1.),(1.,1.),(1.,1.),(1.,1.),(1.,1.),(1.,1.),(1.,1.),(1.,
1.),(1.,1.),(1.,1.),(1.,1.),(1.,1.),(1.,1.),(1.,1.),(1.,1.),(1.,1.),(1.,
1.),(1.,1.),(1.,1.),(1.,1.),(1.,1.),(1.,1.),(1.,1.),(1.,1.),(1.,1.),(1.,
1.),(1.,1.),(1.,1.),(1.,1.),(1.,1.),(1.,1.),(1.,1.),(1.,1.),(1.,1.),(1.,
1.),(1.,1.),(1.,1.),(1.,1.),(1.,1.),(1.,1.),(1.,1.),(1.,1.),(1.,1.),(1.,
1.),(1.,1.),(1.,1.),(1.,1.),(1.,1.),(1.,1.),(1.,1.),(1.,1.),(1.,1.),(1.,
1.),(1.,1.),(1.,1.),(1.,1.),(1.,1.),(1.,1.),(1.,1.),(1.,1.),(1.,1.),(1.,
1.),(1.,1.)))
REPRESENTATION_ITEM('')
SURFACE()
);
#88=(
BOUNDED_SURFACE()
B_SPLINE_SURFACE(5,1,((#48608,#48609),(#48610,#48611),(#48612,#48613),(#48614,
#48615),(#48616,#48617),(#48618,#48619),(#48620,#48621),(#48622,#48623),
(#48624,#48625),(#48626,#48627),(#48628,#48629),(#48630,#48631),(#48632,
#48633),(#48634,#48635),(#48636,#48637),(#48638,#48639),(#48640,#48641),
(#48642,#48643),(#48644,#48645),(#48646,#48647),(#48648,#48649),(#48650,
#48651),(#48652,#48653),(#48654,#48655),(#48656,#48657),(#48658,#48659),
(#48660,#48661),(#48662,#48663),(#48664,#48665),(#48666,#48667),(#48668,
#48669),(#48670,#48671),(#48672,#48673),(#48674,#48675),(#48676,#48677),
(#48678,#48679),(#48680,#48681),(#48682,#48683),(#48684,#48685),(#48686,
#48687),(#48688,#48689),(#48690,#48691),(#48692,#48693),(#48694,#48695),
(#48696,#48697),(#48698,#48699),(#48700,#48701),(#48702,#48703),(#48704,
#48705),(#48706,#48707),(#48708,#48709),(#48710,#48711),(#48712,#48713),
(#48714,#48715),(#48716,#48717),(#48718,#48719),(#48720,#48721),(#48722,
#48723),(#48724,#48725),(#48726,#48727),(#48728,#48729),(#48730,#48731),
(#48732,#48733),(#48734,#48735),(#48736,#48737),(#48738,#48739),(#48740,
#48741),(#48742,#48743),(#48744,#48745),(#48746,#48747)),.UNSPECIFIED.,
 .F.,.F.,.F.)
B_SPLINE_SURFACE_WITH_KNOTS((6,1,1,1,1,1,1,1,1,1,1,1,1,1,1,1,1,1,1,1,1,
1,1,1,1,1,1,1,1,1,1,1,1,1,1,1,1,1,1,1,1,1,1,1,1,1,1,1,1,1,1,1,1,1,1,1,1,
1,1,1,1,1,1,1,1,6),(2,2),(-1.,-0.984615384615383,-0.969230769230768,-0.953846153846152,
-0.938461538461537,-0.923076923076922,-0.907692307692306,-0.892307692307691,
-0.876923076923076,-0.86153846153846,-0.846153846153845,-0.83076923076923,
-0.815384615384614,-0.799999999999999,-0.784615384615384,-0.769230769230768,
-0.753846153846153,-0.738461538461538,-0.723076923076922,-0.707692307692307,
-0.692307692307692,-0.676923076923076,-0.661538461538461,-0.646153846153846,
-0.63076923076923,-0.615384615384615,-0.6,-0.584615384615384,-0.569230769230769,
-0.553846153846154,-0.538461538461538,-0.523076923076923,-0.507692307692308,
-0.492307692307692,-0.476923076923077,-0.461538461538462,-0.446153846153846,
-0.430769230769231,-0.415384615384615,-0.4,-0.384615384615385,-0.369230769230769,
-0.353846153846154,-0.338461538461538,-0.323076923076923,-0.307692307692308,
-0.292307692307692,-0.276923076923077,-0.261538461538462,-0.246153846153846,
-0.230769230769231,-0.215384615384615,-0.2,-0.184615384615385,-0.169230769230769,
-0.153846153846154,-0.138461538461538,-0.123076923076923,-0.107692307692308,
-0.0923076923076923,-0.0769230769230769,-0.0615384615384615,-0.0461538461538462,
-0.0307692307692308,-0.0153846153846154,0.),(-1.,1.),.UNSPECIFIED.)
GEOMETRIC_REPRESENTATION_ITEM()
RATIONAL_B_SPLINE_SURFACE(((1.,1.),(1.,1.),(1.,1.),(1.,1.),(1.,1.),(1.,
1.),(1.,1.),(1.,1.),(1.,1.),(1.,1.),(1.,1.),(1.,1.),(1.,1.),(1.,1.),(1.,
1.),(1.,1.),(1.,1.),(1.,1.),(1.,1.),(1.,1.),(1.,1.),(1.,1.),(1.,1.),(1.,
1.),(1.,1.),(1.,1.),(1.,1.),(1.,1.),(1.,1.),(1.,1.),(1.,1.),(1.,1.),(1.,
1.),(1.,1.),(1.,1.),(1.,1.),(1.,1.),(1.,1.),(1.,1.),(1.,1.),(1.,1.),(1.,
1.),(1.,1.),(1.,1.),(1.,1.),(1.,1.),(1.,1.),(1.,1.),(1.,1.),(1.,1.),(1.,
1.),(1.,1.),(1.,1.),(1.,1.),(1.,1.),(1.,1.),(1.,1.),(1.,1.),(1.,1.),(1.,
1.),(1.,1.),(1.,1.),(1.,1.),(1.,1.),(1.,1.),(1.,1.),(1.,1.),(1.,1.),(1.,
1.),(1.,1.)))
REPRESENTATION_ITEM('')
SURFACE()
);
#89=(
BOUNDED_SURFACE()
B_SPLINE_SURFACE(5,1,((#48824,#48825),(#48826,#48827),(#48828,#48829),(#48830,
#48831),(#48832,#48833),(#48834,#48835),(#48836,#48837),(#48838,#48839),
(#48840,#48841),(#48842,#48843),(#48844,#48845),(#48846,#48847),(#48848,
#48849),(#48850,#48851),(#48852,#48853),(#48854,#48855),(#48856,#48857),
(#48858,#48859),(#48860,#48861),(#48862,#48863),(#48864,#48865),(#48866,
#48867),(#48868,#48869),(#48870,#48871),(#48872,#48873),(#48874,#48875),
(#48876,#48877),(#48878,#48879),(#48880,#48881),(#48882,#48883),(#48884,
#48885),(#48886,#48887),(#48888,#48889),(#48890,#48891),(#48892,#48893),
(#48894,#48895),(#48896,#48897),(#48898,#48899),(#48900,#48901),(#48902,
#48903),(#48904,#48905),(#48906,#48907),(#48908,#48909),(#48910,#48911),
(#48912,#48913),(#48914,#48915),(#48916,#48917),(#48918,#48919),(#48920,
#48921),(#48922,#48923),(#48924,#48925),(#48926,#48927),(#48928,#48929),
(#48930,#48931),(#48932,#48933),(#48934,#48935),(#48936,#48937),(#48938,
#48939),(#48940,#48941),(#48942,#48943),(#48944,#48945),(#48946,#48947),
(#48948,#48949),(#48950,#48951),(#48952,#48953),(#48954,#48955),(#48956,
#48957),(#48958,#48959),(#48960,#48961),(#48962,#48963)),.UNSPECIFIED.,
 .F.,.F.,.F.)
B_SPLINE_SURFACE_WITH_KNOTS((6,1,1,1,1,1,1,1,1,1,1,1,1,1,1,1,1,1,1,1,1,
1,1,1,1,1,1,1,1,1,1,1,1,1,1,1,1,1,1,1,1,1,1,1,1,1,1,1,1,1,1,1,1,1,1,1,1,
1,1,1,1,1,1,1,1,6),(2,2),(-1.,-0.984615384615383,-0.969230769230768,-0.953846153846152,
-0.938461538461537,-0.923076923076922,-0.907692307692306,-0.892307692307691,
-0.876923076923076,-0.86153846153846,-0.846153846153845,-0.83076923076923,
-0.815384615384614,-0.799999999999999,-0.784615384615384,-0.769230769230768,
-0.753846153846153,-0.738461538461538,-0.723076923076922,-0.707692307692307,
-0.692307692307692,-0.676923076923076,-0.661538461538461,-0.646153846153846,
-0.63076923076923,-0.615384615384615,-0.6,-0.584615384615384,-0.569230769230769,
-0.553846153846154,-0.538461538461538,-0.523076923076923,-0.507692307692308,
-0.492307692307692,-0.476923076923077,-0.461538461538462,-0.446153846153846,
-0.430769230769231,-0.415384615384615,-0.4,-0.384615384615385,-0.369230769230769,
-0.353846153846154,-0.338461538461538,-0.323076923076923,-0.307692307692308,
-0.292307692307692,-0.276923076923077,-0.261538461538462,-0.246153846153846,
-0.230769230769231,-0.215384615384615,-0.2,-0.184615384615385,-0.169230769230769,
-0.153846153846154,-0.138461538461538,-0.123076923076923,-0.107692307692308,
-0.0923076923076923,-0.0769230769230769,-0.0615384615384615,-0.0461538461538462,
-0.0307692307692308,-0.0153846153846154,0.),(-1.,1.),.UNSPECIFIED.)
GEOMETRIC_REPRESENTATION_ITEM()
RATIONAL_B_SPLINE_SURFACE(((1.,1.),(1.,1.),(1.,1.),(1.,1.),(1.,1.),(1.,
1.),(1.,1.),(1.,1.),(1.,1.),(1.,1.),(1.,1.),(1.,1.),(1.,1.),(1.,1.),(1.,
1.),(1.,1.),(1.,1.),(1.,1.),(1.,1.),(1.,1.),(1.,1.),(1.,1.),(1.,1.),(1.,
1.),(1.,1.),(1.,1.),(1.,1.),(1.,1.),(1.,1.),(1.,1.),(1.,1.),(1.,1.),(1.,
1.),(1.,1.),(1.,1.),(1.,1.),(1.,1.),(1.,1.),(1.,1.),(1.,1.),(1.,1.),(1.,
1.),(1.,1.),(1.,1.),(1.,1.),(1.,1.),(1.,1.),(1.,1.),(1.,1.),(1.,1.),(1.,
1.),(1.,1.),(1.,1.),(1.,1.),(1.,1.),(1.,1.),(1.,1.),(1.,1.),(1.,1.),(1.,
1.),(1.,1.),(1.,1.),(1.,1.),(1.,1.),(1.,1.),(1.,1.),(1.,1.),(1.,1.),(1.,
1.),(1.,1.)))
REPRESENTATION_ITEM('')
SURFACE()
);
#90=(
BOUNDED_SURFACE()
B_SPLINE_SURFACE(5,1,((#49040,#49041),(#49042,#49043),(#49044,#49045),(#49046,
#49047),(#49048,#49049),(#49050,#49051),(#49052,#49053),(#49054,#49055),
(#49056,#49057),(#49058,#49059),(#49060,#49061),(#49062,#49063),(#49064,
#49065),(#49066,#49067),(#49068,#49069),(#49070,#49071),(#49072,#49073),
(#49074,#49075),(#49076,#49077),(#49078,#49079),(#49080,#49081),(#49082,
#49083),(#49084,#49085),(#49086,#49087),(#49088,#49089),(#49090,#49091),
(#49092,#49093),(#49094,#49095),(#49096,#49097),(#49098,#49099),(#49100,
#49101),(#49102,#49103),(#49104,#49105),(#49106,#49107),(#49108,#49109),
(#49110,#49111),(#49112,#49113),(#49114,#49115),(#49116,#49117),(#49118,
#49119),(#49120,#49121),(#49122,#49123),(#49124,#49125),(#49126,#49127),
(#49128,#49129),(#49130,#49131),(#49132,#49133),(#49134,#49135),(#49136,
#49137),(#49138,#49139),(#49140,#49141),(#49142,#49143),(#49144,#49145),
(#49146,#49147),(#49148,#49149),(#49150,#49151),(#49152,#49153),(#49154,
#49155),(#49156,#49157),(#49158,#49159),(#49160,#49161),(#49162,#49163),
(#49164,#49165),(#49166,#49167),(#49168,#49169),(#49170,#49171),(#49172,
#49173),(#49174,#49175),(#49176,#49177),(#49178,#49179)),.UNSPECIFIED.,
 .F.,.F.,.F.)
B_SPLINE_SURFACE_WITH_KNOTS((6,1,1,1,1,1,1,1,1,1,1,1,1,1,1,1,1,1,1,1,1,
1,1,1,1,1,1,1,1,1,1,1,1,1,1,1,1,1,1,1,1,1,1,1,1,1,1,1,1,1,1,1,1,1,1,1,1,
1,1,1,1,1,1,1,1,6),(2,2),(-1.,-0.984615384615383,-0.969230769230768,-0.953846153846152,
-0.938461538461537,-0.923076923076922,-0.907692307692306,-0.892307692307691,
-0.876923076923076,-0.86153846153846,-0.846153846153845,-0.83076923076923,
-0.815384615384614,-0.799999999999999,-0.784615384615384,-0.769230769230768,
-0.753846153846153,-0.738461538461538,-0.723076923076922,-0.707692307692307,
-0.692307692307692,-0.676923076923076,-0.661538461538461,-0.646153846153846,
-0.63076923076923,-0.615384615384615,-0.6,-0.584615384615384,-0.569230769230769,
-0.553846153846154,-0.538461538461538,-0.523076923076923,-0.507692307692308,
-0.492307692307692,-0.476923076923077,-0.461538461538462,-0.446153846153846,
-0.430769230769231,-0.415384615384615,-0.4,-0.384615384615385,-0.369230769230769,
-0.353846153846154,-0.338461538461538,-0.323076923076923,-0.307692307692308,
-0.292307692307692,-0.276923076923077,-0.261538461538462,-0.246153846153846,
-0.230769230769231,-0.215384615384615,-0.2,-0.184615384615385,-0.169230769230769,
-0.153846153846154,-0.138461538461538,-0.123076923076923,-0.107692307692308,
-0.0923076923076923,-0.0769230769230769,-0.0615384615384615,-0.0461538461538462,
-0.0307692307692308,-0.0153846153846154,0.),(-1.,1.),.UNSPECIFIED.)
GEOMETRIC_REPRESENTATION_ITEM()
RATIONAL_B_SPLINE_SURFACE(((1.,1.),(1.,1.),(1.,1.),(1.,1.),(1.,1.),(1.,
1.),(1.,1.),(1.,1.),(1.,1.),(1.,1.),(1.,1.),(1.,1.),(1.,1.),(1.,1.),(1.,
1.),(1.,1.),(1.,1.),(1.,1.),(1.,1.),(1.,1.),(1.,1.),(1.,1.),(1.,1.),(1.,
1.),(1.,1.),(1.,1.),(1.,1.),(1.,1.),(1.,1.),(1.,1.),(1.,1.),(1.,1.),(1.,
1.),(1.,1.),(1.,1.),(1.,1.),(1.,1.),(1.,1.),(1.,1.),(1.,1.),(1.,1.),(1.,
1.),(1.,1.),(1.,1.),(1.,1.),(1.,1.),(1.,1.),(1.,1.),(1.,1.),(1.,1.),(1.,
1.),(1.,1.),(1.,1.),(1.,1.),(1.,1.),(1.,1.),(1.,1.),(1.,1.),(1.,1.),(1.,
1.),(1.,1.),(1.,1.),(1.,1.),(1.,1.),(1.,1.),(1.,1.),(1.,1.),(1.,1.),(1.,
1.),(1.,1.)))
REPRESENTATION_ITEM('')
SURFACE()
);
#91=(
BOUNDED_SURFACE()
B_SPLINE_SURFACE(5,1,((#55478,#55479),(#55480,#55481),(#55482,#55483),(#55484,
#55485),(#55486,#55487),(#55488,#55489),(#55490,#55491),(#55492,#55493),
(#55494,#55495),(#55496,#55497),(#55498,#55499),(#55500,#55501),(#55502,
#55503),(#55504,#55505),(#55506,#55507),(#55508,#55509),(#55510,#55511),
(#55512,#55513),(#55514,#55515),(#55516,#55517),(#55518,#55519),(#55520,
#55521),(#55522,#55523),(#55524,#55525),(#55526,#55527),(#55528,#55529),
(#55530,#55531),(#55532,#55533),(#55534,#55535),(#55536,#55537),(#55538,
#55539),(#55540,#55541),(#55542,#55543),(#55544,#55545),(#55546,#55547),
(#55548,#55549),(#55550,#55551),(#55552,#55553),(#55554,#55555),(#55556,
#55557),(#55558,#55559),(#55560,#55561),(#55562,#55563),(#55564,#55565),
(#55566,#55567),(#55568,#55569),(#55570,#55571),(#55572,#55573),(#55574,
#55575),(#55576,#55577),(#55578,#55579),(#55580,#55581),(#55582,#55583),
(#55584,#55585),(#55586,#55587),(#55588,#55589),(#55590,#55591),(#55592,
#55593),(#55594,#55595),(#55596,#55597),(#55598,#55599),(#55600,#55601),
(#55602,#55603),(#55604,#55605),(#55606,#55607),(#55608,#55609),(#55610,
#55611),(#55612,#55613),(#55614,#55615),(#55616,#55617)),.UNSPECIFIED.,
 .F.,.F.,.F.)
B_SPLINE_SURFACE_WITH_KNOTS((6,1,1,1,1,1,1,1,1,1,1,1,1,1,1,1,1,1,1,1,1,
1,1,1,1,1,1,1,1,1,1,1,1,1,1,1,1,1,1,1,1,1,1,1,1,1,1,1,1,1,1,1,1,1,1,1,1,
1,1,1,1,1,1,1,1,6),(2,2),(-1.,-0.984615384615383,-0.969230769230768,-0.953846153846152,
-0.938461538461537,-0.923076923076922,-0.907692307692306,-0.892307692307691,
-0.876923076923076,-0.86153846153846,-0.846153846153845,-0.83076923076923,
-0.815384615384614,-0.799999999999999,-0.784615384615384,-0.769230769230768,
-0.753846153846153,-0.738461538461538,-0.723076923076922,-0.707692307692307,
-0.692307692307692,-0.676923076923076,-0.661538461538461,-0.646153846153846,
-0.63076923076923,-0.615384615384615,-0.6,-0.584615384615384,-0.569230769230769,
-0.553846153846154,-0.538461538461538,-0.523076923076923,-0.507692307692308,
-0.492307692307692,-0.476923076923077,-0.461538461538462,-0.446153846153846,
-0.430769230769231,-0.415384615384615,-0.4,-0.384615384615385,-0.369230769230769,
-0.353846153846154,-0.338461538461538,-0.323076923076923,-0.307692307692308,
-0.292307692307692,-0.276923076923077,-0.261538461538462,-0.246153846153846,
-0.230769230769231,-0.215384615384615,-0.2,-0.184615384615385,-0.169230769230769,
-0.153846153846154,-0.138461538461538,-0.123076923076923,-0.107692307692308,
-0.0923076923076923,-0.0769230769230769,-0.0615384615384615,-0.0461538461538462,
-0.0307692307692308,-0.0153846153846154,0.),(-1.,1.),.UNSPECIFIED.)
GEOMETRIC_REPRESENTATION_ITEM()
RATIONAL_B_SPLINE_SURFACE(((1.,1.),(1.,1.),(1.,1.),(1.,1.),(1.,1.),(1.,
1.),(1.,1.),(1.,1.),(1.,1.),(1.,1.),(1.,1.),(1.,1.),(1.,1.),(1.,1.),(1.,
1.),(1.,1.),(1.,1.),(1.,1.),(1.,1.),(1.,1.),(1.,1.),(1.,1.),(1.,1.),(1.,
1.),(1.,1.),(1.,1.),(1.,1.),(1.,1.),(1.,1.),(1.,1.),(1.,1.),(1.,1.),(1.,
1.),(1.,1.),(1.,1.),(1.,1.),(1.,1.),(1.,1.),(1.,1.),(1.,1.),(1.,1.),(1.,
1.),(1.,1.),(1.,1.),(1.,1.),(1.,1.),(1.,1.),(1.,1.),(1.,1.),(1.,1.),(1.,
1.),(1.,1.),(1.,1.),(1.,1.),(1.,1.),(1.,1.),(1.,1.),(1.,1.),(1.,1.),(1.,
1.),(1.,1.),(1.,1.),(1.,1.),(1.,1.),(1.,1.),(1.,1.),(1.,1.),(1.,1.),(1.,
1.),(1.,1.)))
REPRESENTATION_ITEM('')
SURFACE()
);
#92=(
BOUNDED_SURFACE()
B_SPLINE_SURFACE(5,1,((#55697,#55698),(#55699,#55700),(#55701,#55702),(#55703,
#55704),(#55705,#55706),(#55707,#55708),(#55709,#55710),(#55711,#55712),
(#55713,#55714),(#55715,#55716),(#55717,#55718),(#55719,#55720),(#55721,
#55722),(#55723,#55724),(#55725,#55726),(#55727,#55728),(#55729,#55730),
(#55731,#55732),(#55733,#55734),(#55735,#55736),(#55737,#55738),(#55739,
#55740),(#55741,#55742),(#55743,#55744),(#55745,#55746),(#55747,#55748),
(#55749,#55750),(#55751,#55752),(#55753,#55754),(#55755,#55756),(#55757,
#55758),(#55759,#55760),(#55761,#55762),(#55763,#55764),(#55765,#55766),
(#55767,#55768),(#55769,#55770),(#55771,#55772),(#55773,#55774),(#55775,
#55776),(#55777,#55778),(#55779,#55780),(#55781,#55782),(#55783,#55784),
(#55785,#55786),(#55787,#55788),(#55789,#55790),(#55791,#55792),(#55793,
#55794),(#55795,#55796),(#55797,#55798),(#55799,#55800),(#55801,#55802),
(#55803,#55804),(#55805,#55806),(#55807,#55808),(#55809,#55810),(#55811,
#55812),(#55813,#55814),(#55815,#55816),(#55817,#55818),(#55819,#55820),
(#55821,#55822),(#55823,#55824),(#55825,#55826),(#55827,#55828),(#55829,
#55830),(#55831,#55832),(#55833,#55834),(#55835,#55836)),.UNSPECIFIED.,
 .F.,.F.,.F.)
B_SPLINE_SURFACE_WITH_KNOTS((6,1,1,1,1,1,1,1,1,1,1,1,1,1,1,1,1,1,1,1,1,
1,1,1,1,1,1,1,1,1,1,1,1,1,1,1,1,1,1,1,1,1,1,1,1,1,1,1,1,1,1,1,1,1,1,1,1,
1,1,1,1,1,1,1,1,6),(2,2),(-1.,-0.984615384615383,-0.969230769230768,-0.953846153846152,
-0.938461538461537,-0.923076923076922,-0.907692307692306,-0.892307692307691,
-0.876923076923076,-0.86153846153846,-0.846153846153845,-0.83076923076923,
-0.815384615384614,-0.799999999999999,-0.784615384615384,-0.769230769230768,
-0.753846153846153,-0.738461538461538,-0.723076923076922,-0.707692307692307,
-0.692307692307692,-0.676923076923076,-0.661538461538461,-0.646153846153846,
-0.63076923076923,-0.615384615384615,-0.6,-0.584615384615384,-0.569230769230769,
-0.553846153846154,-0.538461538461538,-0.523076923076923,-0.507692307692308,
-0.492307692307692,-0.476923076923077,-0.461538461538462,-0.446153846153846,
-0.430769230769231,-0.415384615384615,-0.4,-0.384615384615385,-0.369230769230769,
-0.353846153846154,-0.338461538461538,-0.323076923076923,-0.307692307692308,
-0.292307692307692,-0.276923076923077,-0.261538461538462,-0.246153846153846,
-0.230769230769231,-0.215384615384615,-0.2,-0.184615384615385,-0.169230769230769,
-0.153846153846154,-0.138461538461538,-0.123076923076923,-0.107692307692308,
-0.0923076923076923,-0.0769230769230769,-0.0615384615384615,-0.0461538461538462,
-0.0307692307692308,-0.0153846153846154,0.),(-1.,1.),.UNSPECIFIED.)
GEOMETRIC_REPRESENTATION_ITEM()
RATIONAL_B_SPLINE_SURFACE(((1.,1.),(1.,1.),(1.,1.),(1.,1.),(1.,1.),(1.,
1.),(1.,1.),(1.,1.),(1.,1.),(1.,1.),(1.,1.),(1.,1.),(1.,1.),(1.,1.),(1.,
1.),(1.,1.),(1.,1.),(1.,1.),(1.,1.),(1.,1.),(1.,1.),(1.,1.),(1.,1.),(1.,
1.),(1.,1.),(1.,1.),(1.,1.),(1.,1.),(1.,1.),(1.,1.),(1.,1.),(1.,1.),(1.,
1.),(1.,1.),(1.,1.),(1.,1.),(1.,1.),(1.,1.),(1.,1.),(1.,1.),(1.,1.),(1.,
1.),(1.,1.),(1.,1.),(1.,1.),(1.,1.),(1.,1.),(1.,1.),(1.,1.),(1.,1.),(1.,
1.),(1.,1.),(1.,1.),(1.,1.),(1.,1.),(1.,1.),(1.,1.),(1.,1.),(1.,1.),(1.,
1.),(1.,1.),(1.,1.),(1.,1.),(1.,1.),(1.,1.),(1.,1.),(1.,1.),(1.,1.),(1.,
1.),(1.,1.)))
REPRESENTATION_ITEM('')
SURFACE()
);
#93=(
BOUNDED_SURFACE()
B_SPLINE_SURFACE(5,1,((#55927,#55928),(#55929,#55930),(#55931,#55932),(#55933,
#55934),(#55935,#55936),(#55937,#55938),(#55939,#55940),(#55941,#55942),
(#55943,#55944),(#55945,#55946),(#55947,#55948),(#55949,#55950),(#55951,
#55952),(#55953,#55954),(#55955,#55956),(#55957,#55958),(#55959,#55960),
(#55961,#55962),(#55963,#55964),(#55965,#55966),(#55967,#55968),(#55969,
#55970),(#55971,#55972),(#55973,#55974),(#55975,#55976),(#55977,#55978),
(#55979,#55980),(#55981,#55982),(#55983,#55984),(#55985,#55986),(#55987,
#55988),(#55989,#55990),(#55991,#55992),(#55993,#55994),(#55995,#55996),
(#55997,#55998),(#55999,#56000),(#56001,#56002),(#56003,#56004),(#56005,
#56006),(#56007,#56008),(#56009,#56010),(#56011,#56012),(#56013,#56014),
(#56015,#56016),(#56017,#56018),(#56019,#56020),(#56021,#56022),(#56023,
#56024),(#56025,#56026),(#56027,#56028),(#56029,#56030),(#56031,#56032),
(#56033,#56034),(#56035,#56036),(#56037,#56038),(#56039,#56040),(#56041,
#56042),(#56043,#56044),(#56045,#56046),(#56047,#56048),(#56049,#56050),
(#56051,#56052),(#56053,#56054),(#56055,#56056),(#56057,#56058),(#56059,
#56060),(#56061,#56062),(#56063,#56064),(#56065,#56066)),.UNSPECIFIED.,
 .F.,.F.,.F.)
B_SPLINE_SURFACE_WITH_KNOTS((6,1,1,1,1,1,1,1,1,1,1,1,1,1,1,1,1,1,1,1,1,
1,1,1,1,1,1,1,1,1,1,1,1,1,1,1,1,1,1,1,1,1,1,1,1,1,1,1,1,1,1,1,1,1,1,1,1,
1,1,1,1,1,1,1,1,6),(2,2),(-1.,-0.984615384615383,-0.969230769230768,-0.953846153846152,
-0.938461538461537,-0.923076923076922,-0.907692307692306,-0.892307692307691,
-0.876923076923076,-0.86153846153846,-0.846153846153845,-0.83076923076923,
-0.815384615384614,-0.799999999999999,-0.784615384615384,-0.769230769230768,
-0.753846153846153,-0.738461538461538,-0.723076923076922,-0.707692307692307,
-0.692307692307692,-0.676923076923076,-0.661538461538461,-0.646153846153846,
-0.63076923076923,-0.615384615384615,-0.6,-0.584615384615384,-0.569230769230769,
-0.553846153846154,-0.538461538461538,-0.523076923076923,-0.507692307692308,
-0.492307692307692,-0.476923076923077,-0.461538461538462,-0.446153846153846,
-0.430769230769231,-0.415384615384615,-0.4,-0.384615384615385,-0.369230769230769,
-0.353846153846154,-0.338461538461538,-0.323076923076923,-0.307692307692308,
-0.292307692307692,-0.276923076923077,-0.261538461538462,-0.246153846153846,
-0.230769230769231,-0.215384615384615,-0.2,-0.184615384615385,-0.169230769230769,
-0.153846153846154,-0.138461538461538,-0.123076923076923,-0.107692307692308,
-0.0923076923076923,-0.0769230769230769,-0.0615384615384615,-0.0461538461538462,
-0.0307692307692308,-0.0153846153846154,0.),(-1.,1.),.UNSPECIFIED.)
GEOMETRIC_REPRESENTATION_ITEM()
RATIONAL_B_SPLINE_SURFACE(((1.,1.),(1.,1.),(1.,1.),(1.,1.),(1.,1.),(1.,
1.),(1.,1.),(1.,1.),(1.,1.),(1.,1.),(1.,1.),(1.,1.),(1.,1.),(1.,1.),(1.,
1.),(1.,1.),(1.,1.),(1.,1.),(1.,1.),(1.,1.),(1.,1.),(1.,1.),(1.,1.),(1.,
1.),(1.,1.),(1.,1.),(1.,1.),(1.,1.),(1.,1.),(1.,1.),(1.,1.),(1.,1.),(1.,
1.),(1.,1.),(1.,1.),(1.,1.),(1.,1.),(1.,1.),(1.,1.),(1.,1.),(1.,1.),(1.,
1.),(1.,1.),(1.,1.),(1.,1.),(1.,1.),(1.,1.),(1.,1.),(1.,1.),(1.,1.),(1.,
1.),(1.,1.),(1.,1.),(1.,1.),(1.,1.),(1.,1.),(1.,1.),(1.,1.),(1.,1.),(1.,
1.),(1.,1.),(1.,1.),(1.,1.),(1.,1.),(1.,1.),(1.,1.),(1.,1.),(1.,1.),(1.,
1.),(1.,1.)))
REPRESENTATION_ITEM('')
SURFACE()
);
#94=(
BOUNDED_SURFACE()
B_SPLINE_SURFACE(5,1,((#56139,#56140),(#56141,#56142),(#56143,#56144),(#56145,
#56146),(#56147,#56148),(#56149,#56150),(#56151,#56152),(#56153,#56154),
(#56155,#56156),(#56157,#56158),(#56159,#56160),(#56161,#56162),(#56163,
#56164),(#56165,#56166),(#56167,#56168),(#56169,#56170),(#56171,#56172),
(#56173,#56174),(#56175,#56176),(#56177,#56178),(#56179,#56180),(#56181,
#56182),(#56183,#56184),(#56185,#56186),(#56187,#56188),(#56189,#56190),
(#56191,#56192),(#56193,#56194),(#56195,#56196),(#56197,#56198),(#56199,
#56200),(#56201,#56202),(#56203,#56204),(#56205,#56206),(#56207,#56208),
(#56209,#56210),(#56211,#56212),(#56213,#56214),(#56215,#56216),(#56217,
#56218),(#56219,#56220),(#56221,#56222),(#56223,#56224),(#56225,#56226),
(#56227,#56228),(#56229,#56230),(#56231,#56232),(#56233,#56234),(#56235,
#56236),(#56237,#56238),(#56239,#56240),(#56241,#56242),(#56243,#56244),
(#56245,#56246),(#56247,#56248),(#56249,#56250),(#56251,#56252),(#56253,
#56254),(#56255,#56256),(#56257,#56258),(#56259,#56260),(#56261,#56262),
(#56263,#56264),(#56265,#56266),(#56267,#56268),(#56269,#56270),(#56271,
#56272),(#56273,#56274),(#56275,#56276),(#56277,#56278)),.UNSPECIFIED.,
 .F.,.F.,.F.)
B_SPLINE_SURFACE_WITH_KNOTS((6,1,1,1,1,1,1,1,1,1,1,1,1,1,1,1,1,1,1,1,1,
1,1,1,1,1,1,1,1,1,1,1,1,1,1,1,1,1,1,1,1,1,1,1,1,1,1,1,1,1,1,1,1,1,1,1,1,
1,1,1,1,1,1,1,1,6),(2,2),(-1.,-0.984615384615383,-0.969230769230768,-0.953846153846152,
-0.938461538461537,-0.923076923076922,-0.907692307692306,-0.892307692307691,
-0.876923076923076,-0.86153846153846,-0.846153846153845,-0.83076923076923,
-0.815384615384614,-0.799999999999999,-0.784615384615384,-0.769230769230768,
-0.753846153846153,-0.738461538461538,-0.723076923076922,-0.707692307692307,
-0.692307692307692,-0.676923076923076,-0.661538461538461,-0.646153846153846,
-0.63076923076923,-0.615384615384615,-0.6,-0.584615384615384,-0.569230769230769,
-0.553846153846154,-0.538461538461538,-0.523076923076923,-0.507692307692308,
-0.492307692307692,-0.476923076923077,-0.461538461538462,-0.446153846153846,
-0.430769230769231,-0.415384615384615,-0.4,-0.384615384615385,-0.369230769230769,
-0.353846153846154,-0.338461538461538,-0.323076923076923,-0.307692307692308,
-0.292307692307692,-0.276923076923077,-0.261538461538462,-0.246153846153846,
-0.230769230769231,-0.215384615384615,-0.2,-0.184615384615385,-0.169230769230769,
-0.153846153846154,-0.138461538461538,-0.123076923076923,-0.107692307692308,
-0.0923076923076923,-0.0769230769230769,-0.0615384615384615,-0.0461538461538462,
-0.0307692307692308,-0.0153846153846154,0.),(-1.,1.),.UNSPECIFIED.)
GEOMETRIC_REPRESENTATION_ITEM()
RATIONAL_B_SPLINE_SURFACE(((1.,1.),(1.,1.),(1.,1.),(1.,1.),(1.,1.),(1.,
1.),(1.,1.),(1.,1.),(1.,1.),(1.,1.),(1.,1.),(1.,1.),(1.,1.),(1.,1.),(1.,
1.),(1.,1.),(1.,1.),(1.,1.),(1.,1.),(1.,1.),(1.,1.),(1.,1.),(1.,1.),(1.,
1.),(1.,1.),(1.,1.),(1.,1.),(1.,1.),(1.,1.),(1.,1.),(1.,1.),(1.,1.),(1.,
1.),(1.,1.),(1.,1.),(1.,1.),(1.,1.),(1.,1.),(1.,1.),(1.,1.),(1.,1.),(1.,
1.),(1.,1.),(1.,1.),(1.,1.),(1.,1.),(1.,1.),(1.,1.),(1.,1.),(1.,1.),(1.,
1.),(1.,1.),(1.,1.),(1.,1.),(1.,1.),(1.,1.),(1.,1.),(1.,1.),(1.,1.),(1.,
1.),(1.,1.),(1.,1.),(1.,1.),(1.,1.),(1.,1.),(1.,1.),(1.,1.),(1.,1.),(1.,
1.),(1.,1.)))
REPRESENTATION_ITEM('')
SURFACE()
);
#95=(
BOUNDED_SURFACE()
B_SPLINE_SURFACE(5,1,((#56369,#56370),(#56371,#56372),(#56373,#56374),(#56375,
#56376),(#56377,#56378),(#56379,#56380),(#56381,#56382),(#56383,#56384),
(#56385,#56386),(#56387,#56388),(#56389,#56390),(#56391,#56392),(#56393,
#56394),(#56395,#56396),(#56397,#56398),(#56399,#56400),(#56401,#56402),
(#56403,#56404),(#56405,#56406),(#56407,#56408),(#56409,#56410),(#56411,
#56412),(#56413,#56414),(#56415,#56416),(#56417,#56418),(#56419,#56420),
(#56421,#56422),(#56423,#56424),(#56425,#56426),(#56427,#56428),(#56429,
#56430),(#56431,#56432),(#56433,#56434),(#56435,#56436),(#56437,#56438),
(#56439,#56440),(#56441,#56442),(#56443,#56444),(#56445,#56446),(#56447,
#56448),(#56449,#56450),(#56451,#56452),(#56453,#56454),(#56455,#56456),
(#56457,#56458),(#56459,#56460),(#56461,#56462),(#56463,#56464),(#56465,
#56466),(#56467,#56468),(#56469,#56470),(#56471,#56472),(#56473,#56474),
(#56475,#56476),(#56477,#56478),(#56479,#56480),(#56481,#56482),(#56483,
#56484),(#56485,#56486),(#56487,#56488),(#56489,#56490),(#56491,#56492),
(#56493,#56494),(#56495,#56496),(#56497,#56498),(#56499,#56500),(#56501,
#56502),(#56503,#56504),(#56505,#56506),(#56507,#56508)),.UNSPECIFIED.,
 .F.,.F.,.F.)
B_SPLINE_SURFACE_WITH_KNOTS((6,1,1,1,1,1,1,1,1,1,1,1,1,1,1,1,1,1,1,1,1,
1,1,1,1,1,1,1,1,1,1,1,1,1,1,1,1,1,1,1,1,1,1,1,1,1,1,1,1,1,1,1,1,1,1,1,1,
1,1,1,1,1,1,1,1,6),(2,2),(-1.,-0.984615384615383,-0.969230769230768,-0.953846153846152,
-0.938461538461537,-0.923076923076922,-0.907692307692306,-0.892307692307691,
-0.876923076923076,-0.86153846153846,-0.846153846153845,-0.83076923076923,
-0.815384615384614,-0.799999999999999,-0.784615384615384,-0.769230769230768,
-0.753846153846153,-0.738461538461538,-0.723076923076922,-0.707692307692307,
-0.692307692307692,-0.676923076923076,-0.661538461538461,-0.646153846153846,
-0.63076923076923,-0.615384615384615,-0.6,-0.584615384615384,-0.569230769230769,
-0.553846153846154,-0.538461538461538,-0.523076923076923,-0.507692307692308,
-0.492307692307692,-0.476923076923077,-0.461538461538462,-0.446153846153846,
-0.430769230769231,-0.415384615384615,-0.4,-0.384615384615385,-0.369230769230769,
-0.353846153846154,-0.338461538461538,-0.323076923076923,-0.307692307692308,
-0.292307692307692,-0.276923076923077,-0.261538461538462,-0.246153846153846,
-0.230769230769231,-0.215384615384615,-0.2,-0.184615384615385,-0.169230769230769,
-0.153846153846154,-0.138461538461538,-0.123076923076923,-0.107692307692308,
-0.0923076923076923,-0.0769230769230769,-0.0615384615384615,-0.0461538461538462,
-0.0307692307692308,-0.0153846153846154,0.),(-1.,1.),.UNSPECIFIED.)
GEOMETRIC_REPRESENTATION_ITEM()
RATIONAL_B_SPLINE_SURFACE(((1.,1.),(1.,1.),(1.,1.),(1.,1.),(1.,1.),(1.,
1.),(1.,1.),(1.,1.),(1.,1.),(1.,1.),(1.,1.),(1.,1.),(1.,1.),(1.,1.),(1.,
1.),(1.,1.),(1.,1.),(1.,1.),(1.,1.),(1.,1.),(1.,1.),(1.,1.),(1.,1.),(1.,
1.),(1.,1.),(1.,1.),(1.,1.),(1.,1.),(1.,1.),(1.,1.),(1.,1.),(1.,1.),(1.,
1.),(1.,1.),(1.,1.),(1.,1.),(1.,1.),(1.,1.),(1.,1.),(1.,1.),(1.,1.),(1.,
1.),(1.,1.),(1.,1.),(1.,1.),(1.,1.),(1.,1.),(1.,1.),(1.,1.),(1.,1.),(1.,
1.),(1.,1.),(1.,1.),(1.,1.),(1.,1.),(1.,1.),(1.,1.),(1.,1.),(1.,1.),(1.,
1.),(1.,1.),(1.,1.),(1.,1.),(1.,1.),(1.,1.),(1.,1.),(1.,1.),(1.,1.),(1.,
1.),(1.,1.)))
REPRESENTATION_ITEM('')
SURFACE()
);
#96=(
BOUNDED_SURFACE()
B_SPLINE_SURFACE(5,1,((#56581,#56582),(#56583,#56584),(#56585,#56586),(#56587,
#56588),(#56589,#56590),(#56591,#56592),(#56593,#56594),(#56595,#56596),
(#56597,#56598),(#56599,#56600),(#56601,#56602),(#56603,#56604),(#56605,
#56606),(#56607,#56608),(#56609,#56610),(#56611,#56612),(#56613,#56614),
(#56615,#56616),(#56617,#56618),(#56619,#56620),(#56621,#56622),(#56623,
#56624),(#56625,#56626),(#56627,#56628),(#56629,#56630),(#56631,#56632),
(#56633,#56634),(#56635,#56636),(#56637,#56638),(#56639,#56640),(#56641,
#56642),(#56643,#56644),(#56645,#56646),(#56647,#56648),(#56649,#56650),
(#56651,#56652),(#56653,#56654),(#56655,#56656),(#56657,#56658),(#56659,
#56660),(#56661,#56662),(#56663,#56664),(#56665,#56666),(#56667,#56668),
(#56669,#56670),(#56671,#56672),(#56673,#56674),(#56675,#56676),(#56677,
#56678),(#56679,#56680),(#56681,#56682),(#56683,#56684),(#56685,#56686),
(#56687,#56688),(#56689,#56690),(#56691,#56692),(#56693,#56694),(#56695,
#56696),(#56697,#56698),(#56699,#56700),(#56701,#56702),(#56703,#56704),
(#56705,#56706),(#56707,#56708),(#56709,#56710),(#56711,#56712),(#56713,
#56714),(#56715,#56716),(#56717,#56718),(#56719,#56720)),.UNSPECIFIED.,
 .F.,.F.,.F.)
B_SPLINE_SURFACE_WITH_KNOTS((6,1,1,1,1,1,1,1,1,1,1,1,1,1,1,1,1,1,1,1,1,
1,1,1,1,1,1,1,1,1,1,1,1,1,1,1,1,1,1,1,1,1,1,1,1,1,1,1,1,1,1,1,1,1,1,1,1,
1,1,1,1,1,1,1,1,6),(2,2),(-1.,-0.984615384615383,-0.969230769230768,-0.953846153846152,
-0.938461538461537,-0.923076923076922,-0.907692307692306,-0.892307692307691,
-0.876923076923076,-0.86153846153846,-0.846153846153845,-0.83076923076923,
-0.815384615384614,-0.799999999999999,-0.784615384615384,-0.769230769230768,
-0.753846153846153,-0.738461538461538,-0.723076923076922,-0.707692307692307,
-0.692307692307692,-0.676923076923076,-0.661538461538461,-0.646153846153846,
-0.63076923076923,-0.615384615384615,-0.6,-0.584615384615384,-0.569230769230769,
-0.553846153846154,-0.538461538461538,-0.523076923076923,-0.507692307692308,
-0.492307692307692,-0.476923076923077,-0.461538461538462,-0.446153846153846,
-0.430769230769231,-0.415384615384615,-0.4,-0.384615384615385,-0.369230769230769,
-0.353846153846154,-0.338461538461538,-0.323076923076923,-0.307692307692308,
-0.292307692307692,-0.276923076923077,-0.261538461538462,-0.246153846153846,
-0.230769230769231,-0.215384615384615,-0.2,-0.184615384615385,-0.169230769230769,
-0.153846153846154,-0.138461538461538,-0.123076923076923,-0.107692307692308,
-0.0923076923076923,-0.0769230769230769,-0.0615384615384615,-0.0461538461538462,
-0.0307692307692308,-0.0153846153846154,0.),(-1.,1.),.UNSPECIFIED.)
GEOMETRIC_REPRESENTATION_ITEM()
RATIONAL_B_SPLINE_SURFACE(((1.,1.),(1.,1.),(1.,1.),(1.,1.),(1.,1.),(1.,
1.),(1.,1.),(1.,1.),(1.,1.),(1.,1.),(1.,1.),(1.,1.),(1.,1.),(1.,1.),(1.,
1.),(1.,1.),(1.,1.),(1.,1.),(1.,1.),(1.,1.),(1.,1.),(1.,1.),(1.,1.),(1.,
1.),(1.,1.),(1.,1.),(1.,1.),(1.,1.),(1.,1.),(1.,1.),(1.,1.),(1.,1.),(1.,
1.),(1.,1.),(1.,1.),(1.,1.),(1.,1.),(1.,1.),(1.,1.),(1.,1.),(1.,1.),(1.,
1.),(1.,1.),(1.,1.),(1.,1.),(1.,1.),(1.,1.),(1.,1.),(1.,1.),(1.,1.),(1.,
1.),(1.,1.),(1.,1.),(1.,1.),(1.,1.),(1.,1.),(1.,1.),(1.,1.),(1.,1.),(1.,
1.),(1.,1.),(1.,1.),(1.,1.),(1.,1.),(1.,1.),(1.,1.),(1.,1.),(1.,1.),(1.,
1.),(1.,1.)))
REPRESENTATION_ITEM('')
SURFACE()
);
#97=(
BOUNDED_SURFACE()
B_SPLINE_SURFACE(5,1,((#56811,#56812),(#56813,#56814),(#56815,#56816),(#56817,
#56818),(#56819,#56820),(#56821,#56822),(#56823,#56824),(#56825,#56826),
(#56827,#56828),(#56829,#56830),(#56831,#56832),(#56833,#56834),(#56835,
#56836),(#56837,#56838),(#56839,#56840),(#56841,#56842),(#56843,#56844),
(#56845,#56846),(#56847,#56848),(#56849,#56850),(#56851,#56852),(#56853,
#56854),(#56855,#56856),(#56857,#56858),(#56859,#56860),(#56861,#56862),
(#56863,#56864),(#56865,#56866),(#56867,#56868),(#56869,#56870),(#56871,
#56872),(#56873,#56874),(#56875,#56876),(#56877,#56878),(#56879,#56880),
(#56881,#56882),(#56883,#56884),(#56885,#56886),(#56887,#56888),(#56889,
#56890),(#56891,#56892),(#56893,#56894),(#56895,#56896),(#56897,#56898),
(#56899,#56900),(#56901,#56902),(#56903,#56904),(#56905,#56906),(#56907,
#56908),(#56909,#56910),(#56911,#56912),(#56913,#56914),(#56915,#56916),
(#56917,#56918),(#56919,#56920),(#56921,#56922),(#56923,#56924),(#56925,
#56926),(#56927,#56928),(#56929,#56930),(#56931,#56932),(#56933,#56934),
(#56935,#56936),(#56937,#56938),(#56939,#56940),(#56941,#56942),(#56943,
#56944),(#56945,#56946),(#56947,#56948),(#56949,#56950)),.UNSPECIFIED.,
 .F.,.F.,.F.)
B_SPLINE_SURFACE_WITH_KNOTS((6,1,1,1,1,1,1,1,1,1,1,1,1,1,1,1,1,1,1,1,1,
1,1,1,1,1,1,1,1,1,1,1,1,1,1,1,1,1,1,1,1,1,1,1,1,1,1,1,1,1,1,1,1,1,1,1,1,
1,1,1,1,1,1,1,1,6),(2,2),(-1.,-0.984615384615383,-0.969230769230768,-0.953846153846152,
-0.938461538461537,-0.923076923076922,-0.907692307692306,-0.892307692307691,
-0.876923076923076,-0.86153846153846,-0.846153846153845,-0.83076923076923,
-0.815384615384614,-0.799999999999999,-0.784615384615384,-0.769230769230768,
-0.753846153846153,-0.738461538461538,-0.723076923076922,-0.707692307692307,
-0.692307692307692,-0.676923076923076,-0.661538461538461,-0.646153846153846,
-0.63076923076923,-0.615384615384615,-0.6,-0.584615384615384,-0.569230769230769,
-0.553846153846154,-0.538461538461538,-0.523076923076923,-0.507692307692308,
-0.492307692307692,-0.476923076923077,-0.461538461538462,-0.446153846153846,
-0.430769230769231,-0.415384615384615,-0.4,-0.384615384615385,-0.369230769230769,
-0.353846153846154,-0.338461538461538,-0.323076923076923,-0.307692307692308,
-0.292307692307692,-0.276923076923077,-0.261538461538462,-0.246153846153846,
-0.230769230769231,-0.215384615384615,-0.2,-0.184615384615385,-0.169230769230769,
-0.153846153846154,-0.138461538461538,-0.123076923076923,-0.107692307692308,
-0.0923076923076923,-0.0769230769230769,-0.0615384615384615,-0.0461538461538462,
-0.0307692307692308,-0.0153846153846154,0.),(-1.,1.),.UNSPECIFIED.)
GEOMETRIC_REPRESENTATION_ITEM()
RATIONAL_B_SPLINE_SURFACE(((1.,1.),(1.,1.),(1.,1.),(1.,1.),(1.,1.),(1.,
1.),(1.,1.),(1.,1.),(1.,1.),(1.,1.),(1.,1.),(1.,1.),(1.,1.),(1.,1.),(1.,
1.),(1.,1.),(1.,1.),(1.,1.),(1.,1.),(1.,1.),(1.,1.),(1.,1.),(1.,1.),(1.,
1.),(1.,1.),(1.,1.),(1.,1.),(1.,1.),(1.,1.),(1.,1.),(1.,1.),(1.,1.),(1.,
1.),(1.,1.),(1.,1.),(1.,1.),(1.,1.),(1.,1.),(1.,1.),(1.,1.),(1.,1.),(1.,
1.),(1.,1.),(1.,1.),(1.,1.),(1.,1.),(1.,1.),(1.,1.),(1.,1.),(1.,1.),(1.,
1.),(1.,1.),(1.,1.),(1.,1.),(1.,1.),(1.,1.),(1.,1.),(1.,1.),(1.,1.),(1.,
1.),(1.,1.),(1.,1.),(1.,1.),(1.,1.),(1.,1.),(1.,1.),(1.,1.),(1.,1.),(1.,
1.),(1.,1.)))
REPRESENTATION_ITEM('')
SURFACE()
);
#98=(
BOUNDED_SURFACE()
B_SPLINE_SURFACE(5,1,((#57023,#57024),(#57025,#57026),(#57027,#57028),(#57029,
#57030),(#57031,#57032),(#57033,#57034),(#57035,#57036),(#57037,#57038),
(#57039,#57040),(#57041,#57042),(#57043,#57044),(#57045,#57046),(#57047,
#57048),(#57049,#57050),(#57051,#57052),(#57053,#57054),(#57055,#57056),
(#57057,#57058),(#57059,#57060),(#57061,#57062),(#57063,#57064),(#57065,
#57066),(#57067,#57068),(#57069,#57070),(#57071,#57072),(#57073,#57074),
(#57075,#57076),(#57077,#57078),(#57079,#57080),(#57081,#57082),(#57083,
#57084),(#57085,#57086),(#57087,#57088),(#57089,#57090),(#57091,#57092),
(#57093,#57094),(#57095,#57096),(#57097,#57098),(#57099,#57100),(#57101,
#57102),(#57103,#57104),(#57105,#57106),(#57107,#57108),(#57109,#57110),
(#57111,#57112),(#57113,#57114),(#57115,#57116),(#57117,#57118),(#57119,
#57120),(#57121,#57122),(#57123,#57124),(#57125,#57126),(#57127,#57128),
(#57129,#57130),(#57131,#57132),(#57133,#57134),(#57135,#57136),(#57137,
#57138),(#57139,#57140),(#57141,#57142),(#57143,#57144),(#57145,#57146),
(#57147,#57148),(#57149,#57150),(#57151,#57152),(#57153,#57154),(#57155,
#57156),(#57157,#57158),(#57159,#57160),(#57161,#57162)),.UNSPECIFIED.,
 .F.,.F.,.F.)
B_SPLINE_SURFACE_WITH_KNOTS((6,1,1,1,1,1,1,1,1,1,1,1,1,1,1,1,1,1,1,1,1,
1,1,1,1,1,1,1,1,1,1,1,1,1,1,1,1,1,1,1,1,1,1,1,1,1,1,1,1,1,1,1,1,1,1,1,1,
1,1,1,1,1,1,1,1,6),(2,2),(-1.,-0.984615384615383,-0.969230769230768,-0.953846153846152,
-0.938461538461537,-0.923076923076922,-0.907692307692306,-0.892307692307691,
-0.876923076923076,-0.86153846153846,-0.846153846153845,-0.83076923076923,
-0.815384615384614,-0.799999999999999,-0.784615384615384,-0.769230769230768,
-0.753846153846153,-0.738461538461538,-0.723076923076922,-0.707692307692307,
-0.692307692307692,-0.676923076923076,-0.661538461538461,-0.646153846153846,
-0.63076923076923,-0.615384615384615,-0.6,-0.584615384615384,-0.569230769230769,
-0.553846153846154,-0.538461538461538,-0.523076923076923,-0.507692307692308,
-0.492307692307692,-0.476923076923077,-0.461538461538462,-0.446153846153846,
-0.430769230769231,-0.415384615384615,-0.4,-0.384615384615385,-0.369230769230769,
-0.353846153846154,-0.338461538461538,-0.323076923076923,-0.307692307692308,
-0.292307692307692,-0.276923076923077,-0.261538461538462,-0.246153846153846,
-0.230769230769231,-0.215384615384615,-0.2,-0.184615384615385,-0.169230769230769,
-0.153846153846154,-0.138461538461538,-0.123076923076923,-0.107692307692308,
-0.0923076923076923,-0.0769230769230769,-0.0615384615384615,-0.0461538461538462,
-0.0307692307692308,-0.0153846153846154,0.),(-1.,1.),.UNSPECIFIED.)
GEOMETRIC_REPRESENTATION_ITEM()
RATIONAL_B_SPLINE_SURFACE(((1.,1.),(1.,1.),(1.,1.),(1.,1.),(1.,1.),(1.,
1.),(1.,1.),(1.,1.),(1.,1.),(1.,1.),(1.,1.),(1.,1.),(1.,1.),(1.,1.),(1.,
1.),(1.,1.),(1.,1.),(1.,1.),(1.,1.),(1.,1.),(1.,1.),(1.,1.),(1.,1.),(1.,
1.),(1.,1.),(1.,1.),(1.,1.),(1.,1.),(1.,1.),(1.,1.),(1.,1.),(1.,1.),(1.,
1.),(1.,1.),(1.,1.),(1.,1.),(1.,1.),(1.,1.),(1.,1.),(1.,1.),(1.,1.),(1.,
1.),(1.,1.),(1.,1.),(1.,1.),(1.,1.),(1.,1.),(1.,1.),(1.,1.),(1.,1.),(1.,
1.),(1.,1.),(1.,1.),(1.,1.),(1.,1.),(1.,1.),(1.,1.),(1.,1.),(1.,1.),(1.,
1.),(1.,1.),(1.,1.),(1.,1.),(1.,1.),(1.,1.),(1.,1.),(1.,1.),(1.,1.),(1.,
1.),(1.,1.)))
REPRESENTATION_ITEM('')
SURFACE()
);
#99=(
BOUNDED_SURFACE()
B_SPLINE_SURFACE(5,1,((#57253,#57254),(#57255,#57256),(#57257,#57258),(#57259,
#57260),(#57261,#57262),(#57263,#57264),(#57265,#57266),(#57267,#57268),
(#57269,#57270),(#57271,#57272),(#57273,#57274),(#57275,#57276),(#57277,
#57278),(#57279,#57280),(#57281,#57282),(#57283,#57284),(#57285,#57286),
(#57287,#57288),(#57289,#57290),(#57291,#57292),(#57293,#57294),(#57295,
#57296),(#57297,#57298),(#57299,#57300),(#57301,#57302),(#57303,#57304),
(#57305,#57306),(#57307,#57308),(#57309,#57310),(#57311,#57312),(#57313,
#57314),(#57315,#57316),(#57317,#57318),(#57319,#57320),(#57321,#57322),
(#57323,#57324),(#57325,#57326),(#57327,#57328),(#57329,#57330),(#57331,
#57332),(#57333,#57334),(#57335,#57336),(#57337,#57338),(#57339,#57340),
(#57341,#57342),(#57343,#57344),(#57345,#57346),(#57347,#57348),(#57349,
#57350),(#57351,#57352),(#57353,#57354),(#57355,#57356),(#57357,#57358),
(#57359,#57360),(#57361,#57362),(#57363,#57364),(#57365,#57366),(#57367,
#57368),(#57369,#57370),(#57371,#57372),(#57373,#57374),(#57375,#57376),
(#57377,#57378),(#57379,#57380),(#57381,#57382),(#57383,#57384),(#57385,
#57386),(#57387,#57388),(#57389,#57390),(#57391,#57392)),.UNSPECIFIED.,
 .F.,.F.,.F.)
B_SPLINE_SURFACE_WITH_KNOTS((6,1,1,1,1,1,1,1,1,1,1,1,1,1,1,1,1,1,1,1,1,
1,1,1,1,1,1,1,1,1,1,1,1,1,1,1,1,1,1,1,1,1,1,1,1,1,1,1,1,1,1,1,1,1,1,1,1,
1,1,1,1,1,1,1,1,6),(2,2),(-1.,-0.984615384615383,-0.969230769230768,-0.953846153846152,
-0.938461538461537,-0.923076923076922,-0.907692307692306,-0.892307692307691,
-0.876923076923076,-0.86153846153846,-0.846153846153845,-0.83076923076923,
-0.815384615384614,-0.799999999999999,-0.784615384615384,-0.769230769230768,
-0.753846153846153,-0.738461538461538,-0.723076923076922,-0.707692307692307,
-0.692307692307692,-0.676923076923076,-0.661538461538461,-0.646153846153846,
-0.63076923076923,-0.615384615384615,-0.6,-0.584615384615384,-0.569230769230769,
-0.553846153846154,-0.538461538461538,-0.523076923076923,-0.507692307692308,
-0.492307692307692,-0.476923076923077,-0.461538461538462,-0.446153846153846,
-0.430769230769231,-0.415384615384615,-0.4,-0.384615384615385,-0.369230769230769,
-0.353846153846154,-0.338461538461538,-0.323076923076923,-0.307692307692308,
-0.292307692307692,-0.276923076923077,-0.261538461538462,-0.246153846153846,
-0.230769230769231,-0.215384615384615,-0.2,-0.184615384615385,-0.169230769230769,
-0.153846153846154,-0.138461538461538,-0.123076923076923,-0.107692307692308,
-0.0923076923076923,-0.0769230769230769,-0.0615384615384615,-0.0461538461538462,
-0.0307692307692308,-0.0153846153846154,0.),(-1.,1.),.UNSPECIFIED.)
GEOMETRIC_REPRESENTATION_ITEM()
RATIONAL_B_SPLINE_SURFACE(((1.,1.),(1.,1.),(1.,1.),(1.,1.),(1.,1.),(1.,
1.),(1.,1.),(1.,1.),(1.,1.),(1.,1.),(1.,1.),(1.,1.),(1.,1.),(1.,1.),(1.,
1.),(1.,1.),(1.,1.),(1.,1.),(1.,1.),(1.,1.),(1.,1.),(1.,1.),(1.,1.),(1.,
1.),(1.,1.),(1.,1.),(1.,1.),(1.,1.),(1.,1.),(1.,1.),(1.,1.),(1.,1.),(1.,
1.),(1.,1.),(1.,1.),(1.,1.),(1.,1.),(1.,1.),(1.,1.),(1.,1.),(1.,1.),(1.,
1.),(1.,1.),(1.,1.),(1.,1.),(1.,1.),(1.,1.),(1.,1.),(1.,1.),(1.,1.),(1.,
1.),(1.,1.),(1.,1.),(1.,1.),(1.,1.),(1.,1.),(1.,1.),(1.,1.),(1.,1.),(1.,
1.),(1.,1.),(1.,1.),(1.,1.),(1.,1.),(1.,1.),(1.,1.),(1.,1.),(1.,1.),(1.,
1.),(1.,1.)))
REPRESENTATION_ITEM('')
SURFACE()
);
#100=(
BOUNDED_SURFACE()
B_SPLINE_SURFACE(5,1,((#57465,#57466),(#57467,#57468),(#57469,#57470),(#57471,
#57472),(#57473,#57474),(#57475,#57476),(#57477,#57478),(#57479,#57480),
(#57481,#57482),(#57483,#57484),(#57485,#57486),(#57487,#57488),(#57489,
#57490),(#57491,#57492),(#57493,#57494),(#57495,#57496),(#57497,#57498),
(#57499,#57500),(#57501,#57502),(#57503,#57504),(#57505,#57506),(#57507,
#57508),(#57509,#57510),(#57511,#57512),(#57513,#57514),(#57515,#57516),
(#57517,#57518),(#57519,#57520),(#57521,#57522),(#57523,#57524),(#57525,
#57526),(#57527,#57528),(#57529,#57530),(#57531,#57532),(#57533,#57534),
(#57535,#57536),(#57537,#57538),(#57539,#57540),(#57541,#57542),(#57543,
#57544),(#57545,#57546),(#57547,#57548),(#57549,#57550),(#57551,#57552),
(#57553,#57554),(#57555,#57556),(#57557,#57558),(#57559,#57560),(#57561,
#57562),(#57563,#57564),(#57565,#57566),(#57567,#57568),(#57569,#57570),
(#57571,#57572),(#57573,#57574),(#57575,#57576),(#57577,#57578),(#57579,
#57580),(#57581,#57582),(#57583,#57584),(#57585,#57586),(#57587,#57588),
(#57589,#57590),(#57591,#57592),(#57593,#57594),(#57595,#57596),(#57597,
#57598),(#57599,#57600),(#57601,#57602),(#57603,#57604)),.UNSPECIFIED.,
 .F.,.F.,.F.)
B_SPLINE_SURFACE_WITH_KNOTS((6,1,1,1,1,1,1,1,1,1,1,1,1,1,1,1,1,1,1,1,1,
1,1,1,1,1,1,1,1,1,1,1,1,1,1,1,1,1,1,1,1,1,1,1,1,1,1,1,1,1,1,1,1,1,1,1,1,
1,1,1,1,1,1,1,1,6),(2,2),(-1.,-0.984615384615383,-0.969230769230768,-0.953846153846152,
-0.938461538461537,-0.923076923076922,-0.907692307692306,-0.892307692307691,
-0.876923076923076,-0.86153846153846,-0.846153846153845,-0.83076923076923,
-0.815384615384614,-0.799999999999999,-0.784615384615384,-0.769230769230768,
-0.753846153846153,-0.738461538461538,-0.723076923076922,-0.707692307692307,
-0.692307692307692,-0.676923076923076,-0.661538461538461,-0.646153846153846,
-0.63076923076923,-0.615384615384615,-0.6,-0.584615384615384,-0.569230769230769,
-0.553846153846154,-0.538461538461538,-0.523076923076923,-0.507692307692308,
-0.492307692307692,-0.476923076923077,-0.461538461538462,-0.446153846153846,
-0.430769230769231,-0.415384615384615,-0.4,-0.384615384615385,-0.369230769230769,
-0.353846153846154,-0.338461538461538,-0.323076923076923,-0.307692307692308,
-0.292307692307692,-0.276923076923077,-0.261538461538462,-0.246153846153846,
-0.230769230769231,-0.215384615384615,-0.2,-0.184615384615385,-0.169230769230769,
-0.153846153846154,-0.138461538461538,-0.123076923076923,-0.107692307692308,
-0.0923076923076923,-0.0769230769230769,-0.0615384615384615,-0.0461538461538462,
-0.0307692307692308,-0.0153846153846154,0.),(-1.,1.),.UNSPECIFIED.)
GEOMETRIC_REPRESENTATION_ITEM()
RATIONAL_B_SPLINE_SURFACE(((1.,1.),(1.,1.),(1.,1.),(1.,1.),(1.,1.),(1.,
1.),(1.,1.),(1.,1.),(1.,1.),(1.,1.),(1.,1.),(1.,1.),(1.,1.),(1.,1.),(1.,
1.),(1.,1.),(1.,1.),(1.,1.),(1.,1.),(1.,1.),(1.,1.),(1.,1.),(1.,1.),(1.,
1.),(1.,1.),(1.,1.),(1.,1.),(1.,1.),(1.,1.),(1.,1.),(1.,1.),(1.,1.),(1.,
1.),(1.,1.),(1.,1.),(1.,1.),(1.,1.),(1.,1.),(1.,1.),(1.,1.),(1.,1.),(1.,
1.),(1.,1.),(1.,1.),(1.,1.),(1.,1.),(1.,1.),(1.,1.),(1.,1.),(1.,1.),(1.,
1.),(1.,1.),(1.,1.),(1.,1.),(1.,1.),(1.,1.),(1.,1.),(1.,1.),(1.,1.),(1.,
1.),(1.,1.),(1.,1.),(1.,1.),(1.,1.),(1.,1.),(1.,1.),(1.,1.),(1.,1.),(1.,
1.),(1.,1.)))
REPRESENTATION_ITEM('')
SURFACE()
);
#101=(
BOUNDED_SURFACE()
B_SPLINE_SURFACE(5,1,((#57695,#57696),(#57697,#57698),(#57699,#57700),(#57701,
#57702),(#57703,#57704),(#57705,#57706),(#57707,#57708),(#57709,#57710),
(#57711,#57712),(#57713,#57714),(#57715,#57716),(#57717,#57718),(#57719,
#57720),(#57721,#57722),(#57723,#57724),(#57725,#57726),(#57727,#57728),
(#57729,#57730),(#57731,#57732),(#57733,#57734),(#57735,#57736),(#57737,
#57738),(#57739,#57740),(#57741,#57742),(#57743,#57744),(#57745,#57746),
(#57747,#57748),(#57749,#57750),(#57751,#57752),(#57753,#57754),(#57755,
#57756),(#57757,#57758),(#57759,#57760),(#57761,#57762),(#57763,#57764),
(#57765,#57766),(#57767,#57768),(#57769,#57770),(#57771,#57772),(#57773,
#57774),(#57775,#57776),(#57777,#57778),(#57779,#57780),(#57781,#57782),
(#57783,#57784),(#57785,#57786),(#57787,#57788),(#57789,#57790),(#57791,
#57792),(#57793,#57794),(#57795,#57796),(#57797,#57798),(#57799,#57800),
(#57801,#57802),(#57803,#57804),(#57805,#57806),(#57807,#57808),(#57809,
#57810),(#57811,#57812),(#57813,#57814),(#57815,#57816),(#57817,#57818),
(#57819,#57820),(#57821,#57822),(#57823,#57824),(#57825,#57826),(#57827,
#57828),(#57829,#57830),(#57831,#57832),(#57833,#57834)),.UNSPECIFIED.,
 .F.,.F.,.F.)
B_SPLINE_SURFACE_WITH_KNOTS((6,1,1,1,1,1,1,1,1,1,1,1,1,1,1,1,1,1,1,1,1,
1,1,1,1,1,1,1,1,1,1,1,1,1,1,1,1,1,1,1,1,1,1,1,1,1,1,1,1,1,1,1,1,1,1,1,1,
1,1,1,1,1,1,1,1,6),(2,2),(-1.,-0.984615384615383,-0.969230769230768,-0.953846153846152,
-0.938461538461537,-0.923076923076922,-0.907692307692306,-0.892307692307691,
-0.876923076923076,-0.86153846153846,-0.846153846153845,-0.83076923076923,
-0.815384615384614,-0.799999999999999,-0.784615384615384,-0.769230769230768,
-0.753846153846153,-0.738461538461538,-0.723076923076922,-0.707692307692307,
-0.692307692307692,-0.676923076923076,-0.661538461538461,-0.646153846153846,
-0.63076923076923,-0.615384615384615,-0.6,-0.584615384615384,-0.569230769230769,
-0.553846153846154,-0.538461538461538,-0.523076923076923,-0.507692307692308,
-0.492307692307692,-0.476923076923077,-0.461538461538462,-0.446153846153846,
-0.430769230769231,-0.415384615384615,-0.4,-0.384615384615385,-0.369230769230769,
-0.353846153846154,-0.338461538461538,-0.323076923076923,-0.307692307692308,
-0.292307692307692,-0.276923076923077,-0.261538461538462,-0.246153846153846,
-0.230769230769231,-0.215384615384615,-0.2,-0.184615384615385,-0.169230769230769,
-0.153846153846154,-0.138461538461538,-0.123076923076923,-0.107692307692308,
-0.0923076923076923,-0.0769230769230769,-0.0615384615384615,-0.0461538461538462,
-0.0307692307692308,-0.0153846153846154,0.),(-1.,1.),.UNSPECIFIED.)
GEOMETRIC_REPRESENTATION_ITEM()
RATIONAL_B_SPLINE_SURFACE(((1.,1.),(1.,1.),(1.,1.),(1.,1.),(1.,1.),(1.,
1.),(1.,1.),(1.,1.),(1.,1.),(1.,1.),(1.,1.),(1.,1.),(1.,1.),(1.,1.),(1.,
1.),(1.,1.),(1.,1.),(1.,1.),(1.,1.),(1.,1.),(1.,1.),(1.,1.),(1.,1.),(1.,
1.),(1.,1.),(1.,1.),(1.,1.),(1.,1.),(1.,1.),(1.,1.),(1.,1.),(1.,1.),(1.,
1.),(1.,1.),(1.,1.),(1.,1.),(1.,1.),(1.,1.),(1.,1.),(1.,1.),(1.,1.),(1.,
1.),(1.,1.),(1.,1.),(1.,1.),(1.,1.),(1.,1.),(1.,1.),(1.,1.),(1.,1.),(1.,
1.),(1.,1.),(1.,1.),(1.,1.),(1.,1.),(1.,1.),(1.,1.),(1.,1.),(1.,1.),(1.,
1.),(1.,1.),(1.,1.),(1.,1.),(1.,1.),(1.,1.),(1.,1.),(1.,1.),(1.,1.),(1.,
1.),(1.,1.)))
REPRESENTATION_ITEM('')
SURFACE()
);
#102=(
BOUNDED_SURFACE()
B_SPLINE_SURFACE(5,1,((#57907,#57908),(#57909,#57910),(#57911,#57912),(#57913,
#57914),(#57915,#57916),(#57917,#57918),(#57919,#57920),(#57921,#57922),
(#57923,#57924),(#57925,#57926),(#57927,#57928),(#57929,#57930),(#57931,
#57932),(#57933,#57934),(#57935,#57936),(#57937,#57938),(#57939,#57940),
(#57941,#57942),(#57943,#57944),(#57945,#57946),(#57947,#57948),(#57949,
#57950),(#57951,#57952),(#57953,#57954),(#57955,#57956),(#57957,#57958),
(#57959,#57960),(#57961,#57962),(#57963,#57964),(#57965,#57966),(#57967,
#57968),(#57969,#57970),(#57971,#57972),(#57973,#57974),(#57975,#57976),
(#57977,#57978),(#57979,#57980),(#57981,#57982),(#57983,#57984),(#57985,
#57986),(#57987,#57988),(#57989,#57990),(#57991,#57992),(#57993,#57994),
(#57995,#57996),(#57997,#57998),(#57999,#58000),(#58001,#58002),(#58003,
#58004),(#58005,#58006),(#58007,#58008),(#58009,#58010),(#58011,#58012),
(#58013,#58014),(#58015,#58016),(#58017,#58018),(#58019,#58020),(#58021,
#58022),(#58023,#58024),(#58025,#58026),(#58027,#58028),(#58029,#58030),
(#58031,#58032),(#58033,#58034),(#58035,#58036),(#58037,#58038),(#58039,
#58040),(#58041,#58042),(#58043,#58044),(#58045,#58046)),.UNSPECIFIED.,
 .F.,.F.,.F.)
B_SPLINE_SURFACE_WITH_KNOTS((6,1,1,1,1,1,1,1,1,1,1,1,1,1,1,1,1,1,1,1,1,
1,1,1,1,1,1,1,1,1,1,1,1,1,1,1,1,1,1,1,1,1,1,1,1,1,1,1,1,1,1,1,1,1,1,1,1,
1,1,1,1,1,1,1,1,6),(2,2),(-1.,-0.984615384615383,-0.969230769230768,-0.953846153846152,
-0.938461538461537,-0.923076923076922,-0.907692307692306,-0.892307692307691,
-0.876923076923076,-0.86153846153846,-0.846153846153845,-0.83076923076923,
-0.815384615384614,-0.799999999999999,-0.784615384615384,-0.769230769230768,
-0.753846153846153,-0.738461538461538,-0.723076923076922,-0.707692307692307,
-0.692307692307692,-0.676923076923076,-0.661538461538461,-0.646153846153846,
-0.63076923076923,-0.615384615384615,-0.6,-0.584615384615384,-0.569230769230769,
-0.553846153846154,-0.538461538461538,-0.523076923076923,-0.507692307692308,
-0.492307692307692,-0.476923076923077,-0.461538461538462,-0.446153846153846,
-0.430769230769231,-0.415384615384615,-0.4,-0.384615384615385,-0.369230769230769,
-0.353846153846154,-0.338461538461538,-0.323076923076923,-0.307692307692308,
-0.292307692307692,-0.276923076923077,-0.261538461538462,-0.246153846153846,
-0.230769230769231,-0.215384615384615,-0.2,-0.184615384615385,-0.169230769230769,
-0.153846153846154,-0.138461538461538,-0.123076923076923,-0.107692307692308,
-0.0923076923076923,-0.0769230769230769,-0.0615384615384615,-0.0461538461538462,
-0.0307692307692308,-0.0153846153846154,0.),(-1.,1.),.UNSPECIFIED.)
GEOMETRIC_REPRESENTATION_ITEM()
RATIONAL_B_SPLINE_SURFACE(((1.,1.),(1.,1.),(1.,1.),(1.,1.),(1.,1.),(1.,
1.),(1.,1.),(1.,1.),(1.,1.),(1.,1.),(1.,1.),(1.,1.),(1.,1.),(1.,1.),(1.,
1.),(1.,1.),(1.,1.),(1.,1.),(1.,1.),(1.,1.),(1.,1.),(1.,1.),(1.,1.),(1.,
1.),(1.,1.),(1.,1.),(1.,1.),(1.,1.),(1.,1.),(1.,1.),(1.,1.),(1.,1.),(1.,
1.),(1.,1.),(1.,1.),(1.,1.),(1.,1.),(1.,1.),(1.,1.),(1.,1.),(1.,1.),(1.,
1.),(1.,1.),(1.,1.),(1.,1.),(1.,1.),(1.,1.),(1.,1.),(1.,1.),(1.,1.),(1.,
1.),(1.,1.),(1.,1.),(1.,1.),(1.,1.),(1.,1.),(1.,1.),(1.,1.),(1.,1.),(1.,
1.),(1.,1.),(1.,1.),(1.,1.),(1.,1.),(1.,1.),(1.,1.),(1.,1.),(1.,1.),(1.,
1.),(1.,1.)))
REPRESENTATION_ITEM('')
SURFACE()
);
#103=(
BOUNDED_SURFACE()
B_SPLINE_SURFACE(5,1,((#58137,#58138),(#58139,#58140),(#58141,#58142),(#58143,
#58144),(#58145,#58146),(#58147,#58148),(#58149,#58150),(#58151,#58152),
(#58153,#58154),(#58155,#58156),(#58157,#58158),(#58159,#58160),(#58161,
#58162),(#58163,#58164),(#58165,#58166),(#58167,#58168),(#58169,#58170),
(#58171,#58172),(#58173,#58174),(#58175,#58176),(#58177,#58178),(#58179,
#58180),(#58181,#58182),(#58183,#58184),(#58185,#58186),(#58187,#58188),
(#58189,#58190),(#58191,#58192),(#58193,#58194),(#58195,#58196),(#58197,
#58198),(#58199,#58200),(#58201,#58202),(#58203,#58204),(#58205,#58206),
(#58207,#58208),(#58209,#58210),(#58211,#58212),(#58213,#58214),(#58215,
#58216),(#58217,#58218),(#58219,#58220),(#58221,#58222),(#58223,#58224),
(#58225,#58226),(#58227,#58228),(#58229,#58230),(#58231,#58232),(#58233,
#58234),(#58235,#58236),(#58237,#58238),(#58239,#58240),(#58241,#58242),
(#58243,#58244),(#58245,#58246),(#58247,#58248),(#58249,#58250),(#58251,
#58252),(#58253,#58254),(#58255,#58256),(#58257,#58258),(#58259,#58260),
(#58261,#58262),(#58263,#58264),(#58265,#58266),(#58267,#58268),(#58269,
#58270),(#58271,#58272),(#58273,#58274),(#58275,#58276)),.UNSPECIFIED.,
 .F.,.F.,.F.)
B_SPLINE_SURFACE_WITH_KNOTS((6,1,1,1,1,1,1,1,1,1,1,1,1,1,1,1,1,1,1,1,1,
1,1,1,1,1,1,1,1,1,1,1,1,1,1,1,1,1,1,1,1,1,1,1,1,1,1,1,1,1,1,1,1,1,1,1,1,
1,1,1,1,1,1,1,1,6),(2,2),(-1.,-0.984615384615383,-0.969230769230768,-0.953846153846152,
-0.938461538461537,-0.923076923076922,-0.907692307692306,-0.892307692307691,
-0.876923076923076,-0.86153846153846,-0.846153846153845,-0.83076923076923,
-0.815384615384614,-0.799999999999999,-0.784615384615384,-0.769230769230768,
-0.753846153846153,-0.738461538461538,-0.723076923076922,-0.707692307692307,
-0.692307692307692,-0.676923076923076,-0.661538461538461,-0.646153846153846,
-0.63076923076923,-0.615384615384615,-0.6,-0.584615384615384,-0.569230769230769,
-0.553846153846154,-0.538461538461538,-0.523076923076923,-0.507692307692308,
-0.492307692307692,-0.476923076923077,-0.461538461538462,-0.446153846153846,
-0.430769230769231,-0.415384615384615,-0.4,-0.384615384615385,-0.369230769230769,
-0.353846153846154,-0.338461538461538,-0.323076923076923,-0.307692307692308,
-0.292307692307692,-0.276923076923077,-0.261538461538462,-0.246153846153846,
-0.230769230769231,-0.215384615384615,-0.2,-0.184615384615385,-0.169230769230769,
-0.153846153846154,-0.138461538461538,-0.123076923076923,-0.107692307692308,
-0.0923076923076923,-0.0769230769230769,-0.0615384615384615,-0.0461538461538462,
-0.0307692307692308,-0.0153846153846154,0.),(-1.,1.),.UNSPECIFIED.)
GEOMETRIC_REPRESENTATION_ITEM()
RATIONAL_B_SPLINE_SURFACE(((1.,1.),(1.,1.),(1.,1.),(1.,1.),(1.,1.),(1.,
1.),(1.,1.),(1.,1.),(1.,1.),(1.,1.),(1.,1.),(1.,1.),(1.,1.),(1.,1.),(1.,
1.),(1.,1.),(1.,1.),(1.,1.),(1.,1.),(1.,1.),(1.,1.),(1.,1.),(1.,1.),(1.,
1.),(1.,1.),(1.,1.),(1.,1.),(1.,1.),(1.,1.),(1.,1.),(1.,1.),(1.,1.),(1.,
1.),(1.,1.),(1.,1.),(1.,1.),(1.,1.),(1.,1.),(1.,1.),(1.,1.),(1.,1.),(1.,
1.),(1.,1.),(1.,1.),(1.,1.),(1.,1.),(1.,1.),(1.,1.),(1.,1.),(1.,1.),(1.,
1.),(1.,1.),(1.,1.),(1.,1.),(1.,1.),(1.,1.),(1.,1.),(1.,1.),(1.,1.),(1.,
1.),(1.,1.),(1.,1.),(1.,1.),(1.,1.),(1.,1.),(1.,1.),(1.,1.),(1.,1.),(1.,
1.),(1.,1.)))
REPRESENTATION_ITEM('')
SURFACE()
);
#104=(
BOUNDED_SURFACE()
B_SPLINE_SURFACE(5,1,((#58349,#58350),(#58351,#58352),(#58353,#58354),(#58355,
#58356),(#58357,#58358),(#58359,#58360),(#58361,#58362),(#58363,#58364),
(#58365,#58366),(#58367,#58368),(#58369,#58370),(#58371,#58372),(#58373,
#58374),(#58375,#58376),(#58377,#58378),(#58379,#58380),(#58381,#58382),
(#58383,#58384),(#58385,#58386),(#58387,#58388),(#58389,#58390),(#58391,
#58392),(#58393,#58394),(#58395,#58396),(#58397,#58398),(#58399,#58400),
(#58401,#58402),(#58403,#58404),(#58405,#58406),(#58407,#58408),(#58409,
#58410),(#58411,#58412),(#58413,#58414),(#58415,#58416),(#58417,#58418),
(#58419,#58420),(#58421,#58422),(#58423,#58424),(#58425,#58426),(#58427,
#58428),(#58429,#58430),(#58431,#58432),(#58433,#58434),(#58435,#58436),
(#58437,#58438),(#58439,#58440),(#58441,#58442),(#58443,#58444),(#58445,
#58446),(#58447,#58448),(#58449,#58450),(#58451,#58452),(#58453,#58454),
(#58455,#58456),(#58457,#58458),(#58459,#58460),(#58461,#58462),(#58463,
#58464),(#58465,#58466),(#58467,#58468),(#58469,#58470),(#58471,#58472),
(#58473,#58474),(#58475,#58476),(#58477,#58478),(#58479,#58480),(#58481,
#58482),(#58483,#58484),(#58485,#58486),(#58487,#58488)),.UNSPECIFIED.,
 .F.,.F.,.F.)
B_SPLINE_SURFACE_WITH_KNOTS((6,1,1,1,1,1,1,1,1,1,1,1,1,1,1,1,1,1,1,1,1,
1,1,1,1,1,1,1,1,1,1,1,1,1,1,1,1,1,1,1,1,1,1,1,1,1,1,1,1,1,1,1,1,1,1,1,1,
1,1,1,1,1,1,1,1,6),(2,2),(-1.,-0.984615384615383,-0.969230769230768,-0.953846153846152,
-0.938461538461537,-0.923076923076922,-0.907692307692306,-0.892307692307691,
-0.876923076923076,-0.86153846153846,-0.846153846153845,-0.83076923076923,
-0.815384615384614,-0.799999999999999,-0.784615384615384,-0.769230769230768,
-0.753846153846153,-0.738461538461538,-0.723076923076922,-0.707692307692307,
-0.692307692307692,-0.676923076923076,-0.661538461538461,-0.646153846153846,
-0.63076923076923,-0.615384615384615,-0.6,-0.584615384615384,-0.569230769230769,
-0.553846153846154,-0.538461538461538,-0.523076923076923,-0.507692307692308,
-0.492307692307692,-0.476923076923077,-0.461538461538462,-0.446153846153846,
-0.430769230769231,-0.415384615384615,-0.4,-0.384615384615385,-0.369230769230769,
-0.353846153846154,-0.338461538461538,-0.323076923076923,-0.307692307692308,
-0.292307692307692,-0.276923076923077,-0.261538461538462,-0.246153846153846,
-0.230769230769231,-0.215384615384615,-0.2,-0.184615384615385,-0.169230769230769,
-0.153846153846154,-0.138461538461538,-0.123076923076923,-0.107692307692308,
-0.0923076923076923,-0.0769230769230769,-0.0615384615384615,-0.0461538461538462,
-0.0307692307692308,-0.0153846153846154,0.),(-1.,1.),.UNSPECIFIED.)
GEOMETRIC_REPRESENTATION_ITEM()
RATIONAL_B_SPLINE_SURFACE(((1.,1.),(1.,1.),(1.,1.),(1.,1.),(1.,1.),(1.,
1.),(1.,1.),(1.,1.),(1.,1.),(1.,1.),(1.,1.),(1.,1.),(1.,1.),(1.,1.),(1.,
1.),(1.,1.),(1.,1.),(1.,1.),(1.,1.),(1.,1.),(1.,1.),(1.,1.),(1.,1.),(1.,
1.),(1.,1.),(1.,1.),(1.,1.),(1.,1.),(1.,1.),(1.,1.),(1.,1.),(1.,1.),(1.,
1.),(1.,1.),(1.,1.),(1.,1.),(1.,1.),(1.,1.),(1.,1.),(1.,1.),(1.,1.),(1.,
1.),(1.,1.),(1.,1.),(1.,1.),(1.,1.),(1.,1.),(1.,1.),(1.,1.),(1.,1.),(1.,
1.),(1.,1.),(1.,1.),(1.,1.),(1.,1.),(1.,1.),(1.,1.),(1.,1.),(1.,1.),(1.,
1.),(1.,1.),(1.,1.),(1.,1.),(1.,1.),(1.,1.),(1.,1.),(1.,1.),(1.,1.),(1.,
1.),(1.,1.)))
REPRESENTATION_ITEM('')
SURFACE()
);
#105=(
BOUNDED_SURFACE()
B_SPLINE_SURFACE(5,1,((#58579,#58580),(#58581,#58582),(#58583,#58584),(#58585,
#58586),(#58587,#58588),(#58589,#58590),(#58591,#58592),(#58593,#58594),
(#58595,#58596),(#58597,#58598),(#58599,#58600),(#58601,#58602),(#58603,
#58604),(#58605,#58606),(#58607,#58608),(#58609,#58610),(#58611,#58612),
(#58613,#58614),(#58615,#58616),(#58617,#58618),(#58619,#58620),(#58621,
#58622),(#58623,#58624),(#58625,#58626),(#58627,#58628),(#58629,#58630),
(#58631,#58632),(#58633,#58634),(#58635,#58636),(#58637,#58638),(#58639,
#58640),(#58641,#58642),(#58643,#58644),(#58645,#58646),(#58647,#58648),
(#58649,#58650),(#58651,#58652),(#58653,#58654),(#58655,#58656),(#58657,
#58658),(#58659,#58660),(#58661,#58662),(#58663,#58664),(#58665,#58666),
(#58667,#58668),(#58669,#58670),(#58671,#58672),(#58673,#58674),(#58675,
#58676),(#58677,#58678),(#58679,#58680),(#58681,#58682),(#58683,#58684),
(#58685,#58686),(#58687,#58688),(#58689,#58690),(#58691,#58692),(#58693,
#58694),(#58695,#58696),(#58697,#58698),(#58699,#58700),(#58701,#58702),
(#58703,#58704),(#58705,#58706),(#58707,#58708),(#58709,#58710),(#58711,
#58712),(#58713,#58714),(#58715,#58716),(#58717,#58718)),.UNSPECIFIED.,
 .F.,.F.,.F.)
B_SPLINE_SURFACE_WITH_KNOTS((6,1,1,1,1,1,1,1,1,1,1,1,1,1,1,1,1,1,1,1,1,
1,1,1,1,1,1,1,1,1,1,1,1,1,1,1,1,1,1,1,1,1,1,1,1,1,1,1,1,1,1,1,1,1,1,1,1,
1,1,1,1,1,1,1,1,6),(2,2),(-1.,-0.984615384615383,-0.969230769230768,-0.953846153846152,
-0.938461538461537,-0.923076923076922,-0.907692307692306,-0.892307692307691,
-0.876923076923076,-0.86153846153846,-0.846153846153845,-0.83076923076923,
-0.815384615384614,-0.799999999999999,-0.784615384615384,-0.769230769230768,
-0.753846153846153,-0.738461538461538,-0.723076923076922,-0.707692307692307,
-0.692307692307692,-0.676923076923076,-0.661538461538461,-0.646153846153846,
-0.63076923076923,-0.615384615384615,-0.6,-0.584615384615384,-0.569230769230769,
-0.553846153846154,-0.538461538461538,-0.523076923076923,-0.507692307692308,
-0.492307692307692,-0.476923076923077,-0.461538461538462,-0.446153846153846,
-0.430769230769231,-0.415384615384615,-0.4,-0.384615384615385,-0.369230769230769,
-0.353846153846154,-0.338461538461538,-0.323076923076923,-0.307692307692308,
-0.292307692307692,-0.276923076923077,-0.261538461538462,-0.246153846153846,
-0.230769230769231,-0.215384615384615,-0.2,-0.184615384615385,-0.169230769230769,
-0.153846153846154,-0.138461538461538,-0.123076923076923,-0.107692307692308,
-0.0923076923076923,-0.0769230769230769,-0.0615384615384615,-0.0461538461538462,
-0.0307692307692308,-0.0153846153846154,0.),(-1.,1.),.UNSPECIFIED.)
GEOMETRIC_REPRESENTATION_ITEM()
RATIONAL_B_SPLINE_SURFACE(((1.,1.),(1.,1.),(1.,1.),(1.,1.),(1.,1.),(1.,
1.),(1.,1.),(1.,1.),(1.,1.),(1.,1.),(1.,1.),(1.,1.),(1.,1.),(1.,1.),(1.,
1.),(1.,1.),(1.,1.),(1.,1.),(1.,1.),(1.,1.),(1.,1.),(1.,1.),(1.,1.),(1.,
1.),(1.,1.),(1.,1.),(1.,1.),(1.,1.),(1.,1.),(1.,1.),(1.,1.),(1.,1.),(1.,
1.),(1.,1.),(1.,1.),(1.,1.),(1.,1.),(1.,1.),(1.,1.),(1.,1.),(1.,1.),(1.,
1.),(1.,1.),(1.,1.),(1.,1.),(1.,1.),(1.,1.),(1.,1.),(1.,1.),(1.,1.),(1.,
1.),(1.,1.),(1.,1.),(1.,1.),(1.,1.),(1.,1.),(1.,1.),(1.,1.),(1.,1.),(1.,
1.),(1.,1.),(1.,1.),(1.,1.),(1.,1.),(1.,1.),(1.,1.),(1.,1.),(1.,1.),(1.,
1.),(1.,1.)))
REPRESENTATION_ITEM('')
SURFACE()
);
#106=(
BOUNDED_SURFACE()
B_SPLINE_SURFACE(5,1,((#58791,#58792),(#58793,#58794),(#58795,#58796),(#58797,
#58798),(#58799,#58800),(#58801,#58802),(#58803,#58804),(#58805,#58806),
(#58807,#58808),(#58809,#58810),(#58811,#58812),(#58813,#58814),(#58815,
#58816),(#58817,#58818),(#58819,#58820),(#58821,#58822),(#58823,#58824),
(#58825,#58826),(#58827,#58828),(#58829,#58830),(#58831,#58832),(#58833,
#58834),(#58835,#58836),(#58837,#58838),(#58839,#58840),(#58841,#58842),
(#58843,#58844),(#58845,#58846),(#58847,#58848),(#58849,#58850),(#58851,
#58852),(#58853,#58854),(#58855,#58856),(#58857,#58858),(#58859,#58860),
(#58861,#58862),(#58863,#58864),(#58865,#58866),(#58867,#58868),(#58869,
#58870),(#58871,#58872),(#58873,#58874),(#58875,#58876),(#58877,#58878),
(#58879,#58880),(#58881,#58882),(#58883,#58884),(#58885,#58886),(#58887,
#58888),(#58889,#58890),(#58891,#58892),(#58893,#58894),(#58895,#58896),
(#58897,#58898),(#58899,#58900),(#58901,#58902),(#58903,#58904),(#58905,
#58906),(#58907,#58908),(#58909,#58910),(#58911,#58912),(#58913,#58914),
(#58915,#58916),(#58917,#58918),(#58919,#58920),(#58921,#58922),(#58923,
#58924),(#58925,#58926),(#58927,#58928),(#58929,#58930)),.UNSPECIFIED.,
 .F.,.F.,.F.)
B_SPLINE_SURFACE_WITH_KNOTS((6,1,1,1,1,1,1,1,1,1,1,1,1,1,1,1,1,1,1,1,1,
1,1,1,1,1,1,1,1,1,1,1,1,1,1,1,1,1,1,1,1,1,1,1,1,1,1,1,1,1,1,1,1,1,1,1,1,
1,1,1,1,1,1,1,1,6),(2,2),(-1.,-0.984615384615383,-0.969230769230768,-0.953846153846152,
-0.938461538461537,-0.923076923076922,-0.907692307692306,-0.892307692307691,
-0.876923076923076,-0.86153846153846,-0.846153846153845,-0.83076923076923,
-0.815384615384614,-0.799999999999999,-0.784615384615384,-0.769230769230768,
-0.753846153846153,-0.738461538461538,-0.723076923076922,-0.707692307692307,
-0.692307692307692,-0.676923076923076,-0.661538461538461,-0.646153846153846,
-0.63076923076923,-0.615384615384615,-0.6,-0.584615384615384,-0.569230769230769,
-0.553846153846154,-0.538461538461538,-0.523076923076923,-0.507692307692308,
-0.492307692307692,-0.476923076923077,-0.461538461538462,-0.446153846153846,
-0.430769230769231,-0.415384615384615,-0.4,-0.384615384615385,-0.369230769230769,
-0.353846153846154,-0.338461538461538,-0.323076923076923,-0.307692307692308,
-0.292307692307692,-0.276923076923077,-0.261538461538462,-0.246153846153846,
-0.230769230769231,-0.215384615384615,-0.2,-0.184615384615385,-0.169230769230769,
-0.153846153846154,-0.138461538461538,-0.123076923076923,-0.107692307692308,
-0.0923076923076923,-0.0769230769230769,-0.0615384615384615,-0.0461538461538462,
-0.0307692307692308,-0.0153846153846154,0.),(-1.,1.),.UNSPECIFIED.)
GEOMETRIC_REPRESENTATION_ITEM()
RATIONAL_B_SPLINE_SURFACE(((1.,1.),(1.,1.),(1.,1.),(1.,1.),(1.,1.),(1.,
1.),(1.,1.),(1.,1.),(1.,1.),(1.,1.),(1.,1.),(1.,1.),(1.,1.),(1.,1.),(1.,
1.),(1.,1.),(1.,1.),(1.,1.),(1.,1.),(1.,1.),(1.,1.),(1.,1.),(1.,1.),(1.,
1.),(1.,1.),(1.,1.),(1.,1.),(1.,1.),(1.,1.),(1.,1.),(1.,1.),(1.,1.),(1.,
1.),(1.,1.),(1.,1.),(1.,1.),(1.,1.),(1.,1.),(1.,1.),(1.,1.),(1.,1.),(1.,
1.),(1.,1.),(1.,1.),(1.,1.),(1.,1.),(1.,1.),(1.,1.),(1.,1.),(1.,1.),(1.,
1.),(1.,1.),(1.,1.),(1.,1.),(1.,1.),(1.,1.),(1.,1.),(1.,1.),(1.,1.),(1.,
1.),(1.,1.),(1.,1.),(1.,1.),(1.,1.),(1.,1.),(1.,1.),(1.,1.),(1.,1.),(1.,
1.),(1.,1.)))
REPRESENTATION_ITEM('')
SURFACE()
);
#107=(
BOUNDED_SURFACE()
B_SPLINE_SURFACE(5,1,((#59021,#59022),(#59023,#59024),(#59025,#59026),(#59027,
#59028),(#59029,#59030),(#59031,#59032),(#59033,#59034),(#59035,#59036),
(#59037,#59038),(#59039,#59040),(#59041,#59042),(#59043,#59044),(#59045,
#59046),(#59047,#59048),(#59049,#59050),(#59051,#59052),(#59053,#59054),
(#59055,#59056),(#59057,#59058),(#59059,#59060),(#59061,#59062),(#59063,
#59064),(#59065,#59066),(#59067,#59068),(#59069,#59070),(#59071,#59072),
(#59073,#59074),(#59075,#59076),(#59077,#59078),(#59079,#59080),(#59081,
#59082),(#59083,#59084),(#59085,#59086),(#59087,#59088),(#59089,#59090),
(#59091,#59092),(#59093,#59094),(#59095,#59096),(#59097,#59098),(#59099,
#59100),(#59101,#59102),(#59103,#59104),(#59105,#59106),(#59107,#59108),
(#59109,#59110),(#59111,#59112),(#59113,#59114),(#59115,#59116),(#59117,
#59118),(#59119,#59120),(#59121,#59122),(#59123,#59124),(#59125,#59126),
(#59127,#59128),(#59129,#59130),(#59131,#59132),(#59133,#59134),(#59135,
#59136),(#59137,#59138),(#59139,#59140),(#59141,#59142),(#59143,#59144),
(#59145,#59146),(#59147,#59148),(#59149,#59150),(#59151,#59152),(#59153,
#59154),(#59155,#59156),(#59157,#59158),(#59159,#59160)),.UNSPECIFIED.,
 .F.,.F.,.F.)
B_SPLINE_SURFACE_WITH_KNOTS((6,1,1,1,1,1,1,1,1,1,1,1,1,1,1,1,1,1,1,1,1,
1,1,1,1,1,1,1,1,1,1,1,1,1,1,1,1,1,1,1,1,1,1,1,1,1,1,1,1,1,1,1,1,1,1,1,1,
1,1,1,1,1,1,1,1,6),(2,2),(-1.,-0.984615384615383,-0.969230769230768,-0.953846153846152,
-0.938461538461537,-0.923076923076922,-0.907692307692306,-0.892307692307691,
-0.876923076923076,-0.86153846153846,-0.846153846153845,-0.83076923076923,
-0.815384615384614,-0.799999999999999,-0.784615384615384,-0.769230769230768,
-0.753846153846153,-0.738461538461538,-0.723076923076922,-0.707692307692307,
-0.692307692307692,-0.676923076923076,-0.661538461538461,-0.646153846153846,
-0.63076923076923,-0.615384615384615,-0.6,-0.584615384615384,-0.569230769230769,
-0.553846153846154,-0.538461538461538,-0.523076923076923,-0.507692307692308,
-0.492307692307692,-0.476923076923077,-0.461538461538462,-0.446153846153846,
-0.430769230769231,-0.415384615384615,-0.4,-0.384615384615385,-0.369230769230769,
-0.353846153846154,-0.338461538461538,-0.323076923076923,-0.307692307692308,
-0.292307692307692,-0.276923076923077,-0.261538461538462,-0.246153846153846,
-0.230769230769231,-0.215384615384615,-0.2,-0.184615384615385,-0.169230769230769,
-0.153846153846154,-0.138461538461538,-0.123076923076923,-0.107692307692308,
-0.0923076923076923,-0.0769230769230769,-0.0615384615384615,-0.0461538461538462,
-0.0307692307692308,-0.0153846153846154,0.),(-1.,1.),.UNSPECIFIED.)
GEOMETRIC_REPRESENTATION_ITEM()
RATIONAL_B_SPLINE_SURFACE(((1.,1.),(1.,1.),(1.,1.),(1.,1.),(1.,1.),(1.,
1.),(1.,1.),(1.,1.),(1.,1.),(1.,1.),(1.,1.),(1.,1.),(1.,1.),(1.,1.),(1.,
1.),(1.,1.),(1.,1.),(1.,1.),(1.,1.),(1.,1.),(1.,1.),(1.,1.),(1.,1.),(1.,
1.),(1.,1.),(1.,1.),(1.,1.),(1.,1.),(1.,1.),(1.,1.),(1.,1.),(1.,1.),(1.,
1.),(1.,1.),(1.,1.),(1.,1.),(1.,1.),(1.,1.),(1.,1.),(1.,1.),(1.,1.),(1.,
1.),(1.,1.),(1.,1.),(1.,1.),(1.,1.),(1.,1.),(1.,1.),(1.,1.),(1.,1.),(1.,
1.),(1.,1.),(1.,1.),(1.,1.),(1.,1.),(1.,1.),(1.,1.),(1.,1.),(1.,1.),(1.,
1.),(1.,1.),(1.,1.),(1.,1.),(1.,1.),(1.,1.),(1.,1.),(1.,1.),(1.,1.),(1.,
1.),(1.,1.)))
REPRESENTATION_ITEM('')
SURFACE()
);
#108=(
BOUNDED_SURFACE()
B_SPLINE_SURFACE(5,1,((#59233,#59234),(#59235,#59236),(#59237,#59238),(#59239,
#59240),(#59241,#59242),(#59243,#59244),(#59245,#59246),(#59247,#59248),
(#59249,#59250),(#59251,#59252),(#59253,#59254),(#59255,#59256),(#59257,
#59258),(#59259,#59260),(#59261,#59262),(#59263,#59264),(#59265,#59266),
(#59267,#59268),(#59269,#59270),(#59271,#59272),(#59273,#59274),(#59275,
#59276),(#59277,#59278),(#59279,#59280),(#59281,#59282),(#59283,#59284),
(#59285,#59286),(#59287,#59288),(#59289,#59290),(#59291,#59292),(#59293,
#59294),(#59295,#59296),(#59297,#59298),(#59299,#59300),(#59301,#59302),
(#59303,#59304),(#59305,#59306),(#59307,#59308),(#59309,#59310),(#59311,
#59312),(#59313,#59314),(#59315,#59316),(#59317,#59318),(#59319,#59320),
(#59321,#59322),(#59323,#59324),(#59325,#59326),(#59327,#59328),(#59329,
#59330),(#59331,#59332),(#59333,#59334),(#59335,#59336),(#59337,#59338),
(#59339,#59340),(#59341,#59342),(#59343,#59344),(#59345,#59346),(#59347,
#59348),(#59349,#59350),(#59351,#59352),(#59353,#59354),(#59355,#59356),
(#59357,#59358),(#59359,#59360),(#59361,#59362),(#59363,#59364),(#59365,
#59366),(#59367,#59368),(#59369,#59370),(#59371,#59372)),.UNSPECIFIED.,
 .F.,.F.,.F.)
B_SPLINE_SURFACE_WITH_KNOTS((6,1,1,1,1,1,1,1,1,1,1,1,1,1,1,1,1,1,1,1,1,
1,1,1,1,1,1,1,1,1,1,1,1,1,1,1,1,1,1,1,1,1,1,1,1,1,1,1,1,1,1,1,1,1,1,1,1,
1,1,1,1,1,1,1,1,6),(2,2),(-1.,-0.984615384615383,-0.969230769230768,-0.953846153846152,
-0.938461538461537,-0.923076923076922,-0.907692307692306,-0.892307692307691,
-0.876923076923076,-0.86153846153846,-0.846153846153845,-0.83076923076923,
-0.815384615384614,-0.799999999999999,-0.784615384615384,-0.769230769230768,
-0.753846153846153,-0.738461538461538,-0.723076923076922,-0.707692307692307,
-0.692307692307692,-0.676923076923076,-0.661538461538461,-0.646153846153846,
-0.63076923076923,-0.615384615384615,-0.6,-0.584615384615384,-0.569230769230769,
-0.553846153846154,-0.538461538461538,-0.523076923076923,-0.507692307692308,
-0.492307692307692,-0.476923076923077,-0.461538461538462,-0.446153846153846,
-0.430769230769231,-0.415384615384615,-0.4,-0.384615384615385,-0.369230769230769,
-0.353846153846154,-0.338461538461538,-0.323076923076923,-0.307692307692308,
-0.292307692307692,-0.276923076923077,-0.261538461538462,-0.246153846153846,
-0.230769230769231,-0.215384615384615,-0.2,-0.184615384615385,-0.169230769230769,
-0.153846153846154,-0.138461538461538,-0.123076923076923,-0.107692307692308,
-0.0923076923076923,-0.0769230769230769,-0.0615384615384615,-0.0461538461538462,
-0.0307692307692308,-0.0153846153846154,0.),(-1.,1.),.UNSPECIFIED.)
GEOMETRIC_REPRESENTATION_ITEM()
RATIONAL_B_SPLINE_SURFACE(((1.,1.),(1.,1.),(1.,1.),(1.,1.),(1.,1.),(1.,
1.),(1.,1.),(1.,1.),(1.,1.),(1.,1.),(1.,1.),(1.,1.),(1.,1.),(1.,1.),(1.,
1.),(1.,1.),(1.,1.),(1.,1.),(1.,1.),(1.,1.),(1.,1.),(1.,1.),(1.,1.),(1.,
1.),(1.,1.),(1.,1.),(1.,1.),(1.,1.),(1.,1.),(1.,1.),(1.,1.),(1.,1.),(1.,
1.),(1.,1.),(1.,1.),(1.,1.),(1.,1.),(1.,1.),(1.,1.),(1.,1.),(1.,1.),(1.,
1.),(1.,1.),(1.,1.),(1.,1.),(1.,1.),(1.,1.),(1.,1.),(1.,1.),(1.,1.),(1.,
1.),(1.,1.),(1.,1.),(1.,1.),(1.,1.),(1.,1.),(1.,1.),(1.,1.),(1.,1.),(1.,
1.),(1.,1.),(1.,1.),(1.,1.),(1.,1.),(1.,1.),(1.,1.),(1.,1.),(1.,1.),(1.,
1.),(1.,1.)))
REPRESENTATION_ITEM('')
SURFACE()
);
#109=(
BOUNDED_SURFACE()
B_SPLINE_SURFACE(5,1,((#59463,#59464),(#59465,#59466),(#59467,#59468),(#59469,
#59470),(#59471,#59472),(#59473,#59474),(#59475,#59476),(#59477,#59478),
(#59479,#59480),(#59481,#59482),(#59483,#59484),(#59485,#59486),(#59487,
#59488),(#59489,#59490),(#59491,#59492),(#59493,#59494),(#59495,#59496),
(#59497,#59498),(#59499,#59500),(#59501,#59502),(#59503,#59504),(#59505,
#59506),(#59507,#59508),(#59509,#59510),(#59511,#59512),(#59513,#59514),
(#59515,#59516),(#59517,#59518),(#59519,#59520),(#59521,#59522),(#59523,
#59524),(#59525,#59526),(#59527,#59528),(#59529,#59530),(#59531,#59532),
(#59533,#59534),(#59535,#59536),(#59537,#59538),(#59539,#59540),(#59541,
#59542),(#59543,#59544),(#59545,#59546),(#59547,#59548),(#59549,#59550),
(#59551,#59552),(#59553,#59554),(#59555,#59556),(#59557,#59558),(#59559,
#59560),(#59561,#59562),(#59563,#59564),(#59565,#59566),(#59567,#59568),
(#59569,#59570),(#59571,#59572),(#59573,#59574),(#59575,#59576),(#59577,
#59578),(#59579,#59580),(#59581,#59582),(#59583,#59584),(#59585,#59586),
(#59587,#59588),(#59589,#59590),(#59591,#59592),(#59593,#59594),(#59595,
#59596),(#59597,#59598),(#59599,#59600),(#59601,#59602)),.UNSPECIFIED.,
 .F.,.F.,.F.)
B_SPLINE_SURFACE_WITH_KNOTS((6,1,1,1,1,1,1,1,1,1,1,1,1,1,1,1,1,1,1,1,1,
1,1,1,1,1,1,1,1,1,1,1,1,1,1,1,1,1,1,1,1,1,1,1,1,1,1,1,1,1,1,1,1,1,1,1,1,
1,1,1,1,1,1,1,1,6),(2,2),(-1.,-0.984615384615383,-0.969230769230768,-0.953846153846152,
-0.938461538461537,-0.923076923076922,-0.907692307692306,-0.892307692307691,
-0.876923076923076,-0.86153846153846,-0.846153846153845,-0.83076923076923,
-0.815384615384614,-0.799999999999999,-0.784615384615384,-0.769230769230768,
-0.753846153846153,-0.738461538461538,-0.723076923076922,-0.707692307692307,
-0.692307692307692,-0.676923076923076,-0.661538461538461,-0.646153846153846,
-0.63076923076923,-0.615384615384615,-0.6,-0.584615384615384,-0.569230769230769,
-0.553846153846154,-0.538461538461538,-0.523076923076923,-0.507692307692308,
-0.492307692307692,-0.476923076923077,-0.461538461538462,-0.446153846153846,
-0.430769230769231,-0.415384615384615,-0.4,-0.384615384615385,-0.369230769230769,
-0.353846153846154,-0.338461538461538,-0.323076923076923,-0.307692307692308,
-0.292307692307692,-0.276923076923077,-0.261538461538462,-0.246153846153846,
-0.230769230769231,-0.215384615384615,-0.2,-0.184615384615385,-0.169230769230769,
-0.153846153846154,-0.138461538461538,-0.123076923076923,-0.107692307692308,
-0.0923076923076923,-0.0769230769230769,-0.0615384615384615,-0.0461538461538462,
-0.0307692307692308,-0.0153846153846154,0.),(-1.,1.),.UNSPECIFIED.)
GEOMETRIC_REPRESENTATION_ITEM()
RATIONAL_B_SPLINE_SURFACE(((1.,1.),(1.,1.),(1.,1.),(1.,1.),(1.,1.),(1.,
1.),(1.,1.),(1.,1.),(1.,1.),(1.,1.),(1.,1.),(1.,1.),(1.,1.),(1.,1.),(1.,
1.),(1.,1.),(1.,1.),(1.,1.),(1.,1.),(1.,1.),(1.,1.),(1.,1.),(1.,1.),(1.,
1.),(1.,1.),(1.,1.),(1.,1.),(1.,1.),(1.,1.),(1.,1.),(1.,1.),(1.,1.),(1.,
1.),(1.,1.),(1.,1.),(1.,1.),(1.,1.),(1.,1.),(1.,1.),(1.,1.),(1.,1.),(1.,
1.),(1.,1.),(1.,1.),(1.,1.),(1.,1.),(1.,1.),(1.,1.),(1.,1.),(1.,1.),(1.,
1.),(1.,1.),(1.,1.),(1.,1.),(1.,1.),(1.,1.),(1.,1.),(1.,1.),(1.,1.),(1.,
1.),(1.,1.),(1.,1.),(1.,1.),(1.,1.),(1.,1.),(1.,1.),(1.,1.),(1.,1.),(1.,
1.),(1.,1.)))
REPRESENTATION_ITEM('')
SURFACE()
);
#110=(
BOUNDED_SURFACE()
B_SPLINE_SURFACE(5,1,((#59675,#59676),(#59677,#59678),(#59679,#59680),(#59681,
#59682),(#59683,#59684),(#59685,#59686),(#59687,#59688),(#59689,#59690),
(#59691,#59692),(#59693,#59694),(#59695,#59696),(#59697,#59698),(#59699,
#59700),(#59701,#59702),(#59703,#59704),(#59705,#59706),(#59707,#59708),
(#59709,#59710),(#59711,#59712),(#59713,#59714),(#59715,#59716),(#59717,
#59718),(#59719,#59720),(#59721,#59722),(#59723,#59724),(#59725,#59726),
(#59727,#59728),(#59729,#59730),(#59731,#59732),(#59733,#59734),(#59735,
#59736),(#59737,#59738),(#59739,#59740),(#59741,#59742),(#59743,#59744),
(#59745,#59746),(#59747,#59748),(#59749,#59750),(#59751,#59752),(#59753,
#59754),(#59755,#59756),(#59757,#59758),(#59759,#59760),(#59761,#59762),
(#59763,#59764),(#59765,#59766),(#59767,#59768),(#59769,#59770),(#59771,
#59772),(#59773,#59774),(#59775,#59776),(#59777,#59778),(#59779,#59780),
(#59781,#59782),(#59783,#59784),(#59785,#59786),(#59787,#59788),(#59789,
#59790),(#59791,#59792),(#59793,#59794),(#59795,#59796),(#59797,#59798),
(#59799,#59800),(#59801,#59802),(#59803,#59804),(#59805,#59806),(#59807,
#59808),(#59809,#59810),(#59811,#59812),(#59813,#59814)),.UNSPECIFIED.,
 .F.,.F.,.F.)
B_SPLINE_SURFACE_WITH_KNOTS((6,1,1,1,1,1,1,1,1,1,1,1,1,1,1,1,1,1,1,1,1,
1,1,1,1,1,1,1,1,1,1,1,1,1,1,1,1,1,1,1,1,1,1,1,1,1,1,1,1,1,1,1,1,1,1,1,1,
1,1,1,1,1,1,1,1,6),(2,2),(-1.,-0.984615384615383,-0.969230769230768,-0.953846153846152,
-0.938461538461537,-0.923076923076922,-0.907692307692306,-0.892307692307691,
-0.876923076923076,-0.86153846153846,-0.846153846153845,-0.83076923076923,
-0.815384615384614,-0.799999999999999,-0.784615384615384,-0.769230769230768,
-0.753846153846153,-0.738461538461538,-0.723076923076922,-0.707692307692307,
-0.692307692307692,-0.676923076923076,-0.661538461538461,-0.646153846153846,
-0.63076923076923,-0.615384615384615,-0.6,-0.584615384615384,-0.569230769230769,
-0.553846153846154,-0.538461538461538,-0.523076923076923,-0.507692307692308,
-0.492307692307692,-0.476923076923077,-0.461538461538462,-0.446153846153846,
-0.430769230769231,-0.415384615384615,-0.4,-0.384615384615385,-0.369230769230769,
-0.353846153846154,-0.338461538461538,-0.323076923076923,-0.307692307692308,
-0.292307692307692,-0.276923076923077,-0.261538461538462,-0.246153846153846,
-0.230769230769231,-0.215384615384615,-0.2,-0.184615384615385,-0.169230769230769,
-0.153846153846154,-0.138461538461538,-0.123076923076923,-0.107692307692308,
-0.0923076923076923,-0.0769230769230769,-0.0615384615384615,-0.0461538461538462,
-0.0307692307692308,-0.0153846153846154,0.),(-1.,1.),.UNSPECIFIED.)
GEOMETRIC_REPRESENTATION_ITEM()
RATIONAL_B_SPLINE_SURFACE(((1.,1.),(1.,1.),(1.,1.),(1.,1.),(1.,1.),(1.,
1.),(1.,1.),(1.,1.),(1.,1.),(1.,1.),(1.,1.),(1.,1.),(1.,1.),(1.,1.),(1.,
1.),(1.,1.),(1.,1.),(1.,1.),(1.,1.),(1.,1.),(1.,1.),(1.,1.),(1.,1.),(1.,
1.),(1.,1.),(1.,1.),(1.,1.),(1.,1.),(1.,1.),(1.,1.),(1.,1.),(1.,1.),(1.,
1.),(1.,1.),(1.,1.),(1.,1.),(1.,1.),(1.,1.),(1.,1.),(1.,1.),(1.,1.),(1.,
1.),(1.,1.),(1.,1.),(1.,1.),(1.,1.),(1.,1.),(1.,1.),(1.,1.),(1.,1.),(1.,
1.),(1.,1.),(1.,1.),(1.,1.),(1.,1.),(1.,1.),(1.,1.),(1.,1.),(1.,1.),(1.,
1.),(1.,1.),(1.,1.),(1.,1.),(1.,1.),(1.,1.),(1.,1.),(1.,1.),(1.,1.),(1.,
1.),(1.,1.)))
REPRESENTATION_ITEM('')
SURFACE()
);
#111=(
BOUNDED_SURFACE()
B_SPLINE_SURFACE(5,1,((#59905,#59906),(#59907,#59908),(#59909,#59910),(#59911,
#59912),(#59913,#59914),(#59915,#59916),(#59917,#59918),(#59919,#59920),
(#59921,#59922),(#59923,#59924),(#59925,#59926),(#59927,#59928),(#59929,
#59930),(#59931,#59932),(#59933,#59934),(#59935,#59936),(#59937,#59938),
(#59939,#59940),(#59941,#59942),(#59943,#59944),(#59945,#59946),(#59947,
#59948),(#59949,#59950),(#59951,#59952),(#59953,#59954),(#59955,#59956),
(#59957,#59958),(#59959,#59960),(#59961,#59962),(#59963,#59964),(#59965,
#59966),(#59967,#59968),(#59969,#59970),(#59971,#59972),(#59973,#59974),
(#59975,#59976),(#59977,#59978),(#59979,#59980),(#59981,#59982),(#59983,
#59984),(#59985,#59986),(#59987,#59988),(#59989,#59990),(#59991,#59992),
(#59993,#59994),(#59995,#59996),(#59997,#59998),(#59999,#60000),(#60001,
#60002),(#60003,#60004),(#60005,#60006),(#60007,#60008),(#60009,#60010),
(#60011,#60012),(#60013,#60014),(#60015,#60016),(#60017,#60018),(#60019,
#60020),(#60021,#60022),(#60023,#60024),(#60025,#60026),(#60027,#60028),
(#60029,#60030),(#60031,#60032),(#60033,#60034),(#60035,#60036),(#60037,
#60038),(#60039,#60040),(#60041,#60042),(#60043,#60044)),.UNSPECIFIED.,
 .F.,.F.,.F.)
B_SPLINE_SURFACE_WITH_KNOTS((6,1,1,1,1,1,1,1,1,1,1,1,1,1,1,1,1,1,1,1,1,
1,1,1,1,1,1,1,1,1,1,1,1,1,1,1,1,1,1,1,1,1,1,1,1,1,1,1,1,1,1,1,1,1,1,1,1,
1,1,1,1,1,1,1,1,6),(2,2),(-1.,-0.984615384615383,-0.969230769230768,-0.953846153846152,
-0.938461538461537,-0.923076923076922,-0.907692307692306,-0.892307692307691,
-0.876923076923076,-0.86153846153846,-0.846153846153845,-0.83076923076923,
-0.815384615384614,-0.799999999999999,-0.784615384615384,-0.769230769230768,
-0.753846153846153,-0.738461538461538,-0.723076923076922,-0.707692307692307,
-0.692307692307692,-0.676923076923076,-0.661538461538461,-0.646153846153846,
-0.63076923076923,-0.615384615384615,-0.6,-0.584615384615384,-0.569230769230769,
-0.553846153846154,-0.538461538461538,-0.523076923076923,-0.507692307692308,
-0.492307692307692,-0.476923076923077,-0.461538461538462,-0.446153846153846,
-0.430769230769231,-0.415384615384615,-0.4,-0.384615384615385,-0.369230769230769,
-0.353846153846154,-0.338461538461538,-0.323076923076923,-0.307692307692308,
-0.292307692307692,-0.276923076923077,-0.261538461538462,-0.246153846153846,
-0.230769230769231,-0.215384615384615,-0.2,-0.184615384615385,-0.169230769230769,
-0.153846153846154,-0.138461538461538,-0.123076923076923,-0.107692307692308,
-0.0923076923076923,-0.0769230769230769,-0.0615384615384615,-0.0461538461538462,
-0.0307692307692308,-0.0153846153846154,0.),(-1.,1.),.UNSPECIFIED.)
GEOMETRIC_REPRESENTATION_ITEM()
RATIONAL_B_SPLINE_SURFACE(((1.,1.),(1.,1.),(1.,1.),(1.,1.),(1.,1.),(1.,
1.),(1.,1.),(1.,1.),(1.,1.),(1.,1.),(1.,1.),(1.,1.),(1.,1.),(1.,1.),(1.,
1.),(1.,1.),(1.,1.),(1.,1.),(1.,1.),(1.,1.),(1.,1.),(1.,1.),(1.,1.),(1.,
1.),(1.,1.),(1.,1.),(1.,1.),(1.,1.),(1.,1.),(1.,1.),(1.,1.),(1.,1.),(1.,
1.),(1.,1.),(1.,1.),(1.,1.),(1.,1.),(1.,1.),(1.,1.),(1.,1.),(1.,1.),(1.,
1.),(1.,1.),(1.,1.),(1.,1.),(1.,1.),(1.,1.),(1.,1.),(1.,1.),(1.,1.),(1.,
1.),(1.,1.),(1.,1.),(1.,1.),(1.,1.),(1.,1.),(1.,1.),(1.,1.),(1.,1.),(1.,
1.),(1.,1.),(1.,1.),(1.,1.),(1.,1.),(1.,1.),(1.,1.),(1.,1.),(1.,1.),(1.,
1.),(1.,1.)))
REPRESENTATION_ITEM('')
SURFACE()
);
#112=(
BOUNDED_SURFACE()
B_SPLINE_SURFACE(5,1,((#60117,#60118),(#60119,#60120),(#60121,#60122),(#60123,
#60124),(#60125,#60126),(#60127,#60128),(#60129,#60130),(#60131,#60132),
(#60133,#60134),(#60135,#60136),(#60137,#60138),(#60139,#60140),(#60141,
#60142),(#60143,#60144),(#60145,#60146),(#60147,#60148),(#60149,#60150),
(#60151,#60152),(#60153,#60154),(#60155,#60156),(#60157,#60158),(#60159,
#60160),(#60161,#60162),(#60163,#60164),(#60165,#60166),(#60167,#60168),
(#60169,#60170),(#60171,#60172),(#60173,#60174),(#60175,#60176),(#60177,
#60178),(#60179,#60180),(#60181,#60182),(#60183,#60184),(#60185,#60186),
(#60187,#60188),(#60189,#60190),(#60191,#60192),(#60193,#60194),(#60195,
#60196),(#60197,#60198),(#60199,#60200),(#60201,#60202),(#60203,#60204),
(#60205,#60206),(#60207,#60208),(#60209,#60210),(#60211,#60212),(#60213,
#60214),(#60215,#60216),(#60217,#60218),(#60219,#60220),(#60221,#60222),
(#60223,#60224),(#60225,#60226),(#60227,#60228),(#60229,#60230),(#60231,
#60232),(#60233,#60234),(#60235,#60236),(#60237,#60238),(#60239,#60240),
(#60241,#60242),(#60243,#60244),(#60245,#60246),(#60247,#60248),(#60249,
#60250),(#60251,#60252),(#60253,#60254),(#60255,#60256)),.UNSPECIFIED.,
 .F.,.F.,.F.)
B_SPLINE_SURFACE_WITH_KNOTS((6,1,1,1,1,1,1,1,1,1,1,1,1,1,1,1,1,1,1,1,1,
1,1,1,1,1,1,1,1,1,1,1,1,1,1,1,1,1,1,1,1,1,1,1,1,1,1,1,1,1,1,1,1,1,1,1,1,
1,1,1,1,1,1,1,1,6),(2,2),(-1.,-0.984615384615383,-0.969230769230768,-0.953846153846152,
-0.938461538461537,-0.923076923076922,-0.907692307692306,-0.892307692307691,
-0.876923076923076,-0.86153846153846,-0.846153846153845,-0.83076923076923,
-0.815384615384614,-0.799999999999999,-0.784615384615384,-0.769230769230768,
-0.753846153846153,-0.738461538461538,-0.723076923076922,-0.707692307692307,
-0.692307692307692,-0.676923076923076,-0.661538461538461,-0.646153846153846,
-0.63076923076923,-0.615384615384615,-0.6,-0.584615384615384,-0.569230769230769,
-0.553846153846154,-0.538461538461538,-0.523076923076923,-0.507692307692308,
-0.492307692307692,-0.476923076923077,-0.461538461538462,-0.446153846153846,
-0.430769230769231,-0.415384615384615,-0.4,-0.384615384615385,-0.369230769230769,
-0.353846153846154,-0.338461538461538,-0.323076923076923,-0.307692307692308,
-0.292307692307692,-0.276923076923077,-0.261538461538462,-0.246153846153846,
-0.230769230769231,-0.215384615384615,-0.2,-0.184615384615385,-0.169230769230769,
-0.153846153846154,-0.138461538461538,-0.123076923076923,-0.107692307692308,
-0.0923076923076923,-0.0769230769230769,-0.0615384615384615,-0.0461538461538462,
-0.0307692307692308,-0.0153846153846154,0.),(-1.,1.),.UNSPECIFIED.)
GEOMETRIC_REPRESENTATION_ITEM()
RATIONAL_B_SPLINE_SURFACE(((1.,1.),(1.,1.),(1.,1.),(1.,1.),(1.,1.),(1.,
1.),(1.,1.),(1.,1.),(1.,1.),(1.,1.),(1.,1.),(1.,1.),(1.,1.),(1.,1.),(1.,
1.),(1.,1.),(1.,1.),(1.,1.),(1.,1.),(1.,1.),(1.,1.),(1.,1.),(1.,1.),(1.,
1.),(1.,1.),(1.,1.),(1.,1.),(1.,1.),(1.,1.),(1.,1.),(1.,1.),(1.,1.),(1.,
1.),(1.,1.),(1.,1.),(1.,1.),(1.,1.),(1.,1.),(1.,1.),(1.,1.),(1.,1.),(1.,
1.),(1.,1.),(1.,1.),(1.,1.),(1.,1.),(1.,1.),(1.,1.),(1.,1.),(1.,1.),(1.,
1.),(1.,1.),(1.,1.),(1.,1.),(1.,1.),(1.,1.),(1.,1.),(1.,1.),(1.,1.),(1.,
1.),(1.,1.),(1.,1.),(1.,1.),(1.,1.),(1.,1.),(1.,1.),(1.,1.),(1.,1.),(1.,
1.),(1.,1.)))
REPRESENTATION_ITEM('')
SURFACE()
);
#113=(
BOUNDED_SURFACE()
B_SPLINE_SURFACE(5,1,((#60347,#60348),(#60349,#60350),(#60351,#60352),(#60353,
#60354),(#60355,#60356),(#60357,#60358),(#60359,#60360),(#60361,#60362),
(#60363,#60364),(#60365,#60366),(#60367,#60368),(#60369,#60370),(#60371,
#60372),(#60373,#60374),(#60375,#60376),(#60377,#60378),(#60379,#60380),
(#60381,#60382),(#60383,#60384),(#60385,#60386),(#60387,#60388),(#60389,
#60390),(#60391,#60392),(#60393,#60394),(#60395,#60396),(#60397,#60398),
(#60399,#60400),(#60401,#60402),(#60403,#60404),(#60405,#60406),(#60407,
#60408),(#60409,#60410),(#60411,#60412),(#60413,#60414),(#60415,#60416),
(#60417,#60418),(#60419,#60420),(#60421,#60422),(#60423,#60424),(#60425,
#60426),(#60427,#60428),(#60429,#60430),(#60431,#60432),(#60433,#60434),
(#60435,#60436),(#60437,#60438),(#60439,#60440),(#60441,#60442),(#60443,
#60444),(#60445,#60446),(#60447,#60448),(#60449,#60450),(#60451,#60452),
(#60453,#60454),(#60455,#60456),(#60457,#60458),(#60459,#60460),(#60461,
#60462),(#60463,#60464),(#60465,#60466),(#60467,#60468),(#60469,#60470),
(#60471,#60472),(#60473,#60474),(#60475,#60476),(#60477,#60478),(#60479,
#60480),(#60481,#60482),(#60483,#60484),(#60485,#60486)),.UNSPECIFIED.,
 .F.,.F.,.F.)
B_SPLINE_SURFACE_WITH_KNOTS((6,1,1,1,1,1,1,1,1,1,1,1,1,1,1,1,1,1,1,1,1,
1,1,1,1,1,1,1,1,1,1,1,1,1,1,1,1,1,1,1,1,1,1,1,1,1,1,1,1,1,1,1,1,1,1,1,1,
1,1,1,1,1,1,1,1,6),(2,2),(-1.,-0.984615384615383,-0.969230769230768,-0.953846153846152,
-0.938461538461537,-0.923076923076922,-0.907692307692306,-0.892307692307691,
-0.876923076923076,-0.86153846153846,-0.846153846153845,-0.83076923076923,
-0.815384615384614,-0.799999999999999,-0.784615384615384,-0.769230769230768,
-0.753846153846153,-0.738461538461538,-0.723076923076922,-0.707692307692307,
-0.692307692307692,-0.676923076923076,-0.661538461538461,-0.646153846153846,
-0.63076923076923,-0.615384615384615,-0.6,-0.584615384615384,-0.569230769230769,
-0.553846153846154,-0.538461538461538,-0.523076923076923,-0.507692307692308,
-0.492307692307692,-0.476923076923077,-0.461538461538462,-0.446153846153846,
-0.430769230769231,-0.415384615384615,-0.4,-0.384615384615385,-0.369230769230769,
-0.353846153846154,-0.338461538461538,-0.323076923076923,-0.307692307692308,
-0.292307692307692,-0.276923076923077,-0.261538461538462,-0.246153846153846,
-0.230769230769231,-0.215384615384615,-0.2,-0.184615384615385,-0.169230769230769,
-0.153846153846154,-0.138461538461538,-0.123076923076923,-0.107692307692308,
-0.0923076923076923,-0.0769230769230769,-0.0615384615384615,-0.0461538461538462,
-0.0307692307692308,-0.0153846153846154,0.),(-1.,1.),.UNSPECIFIED.)
GEOMETRIC_REPRESENTATION_ITEM()
RATIONAL_B_SPLINE_SURFACE(((1.,1.),(1.,1.),(1.,1.),(1.,1.),(1.,1.),(1.,
1.),(1.,1.),(1.,1.),(1.,1.),(1.,1.),(1.,1.),(1.,1.),(1.,1.),(1.,1.),(1.,
1.),(1.,1.),(1.,1.),(1.,1.),(1.,1.),(1.,1.),(1.,1.),(1.,1.),(1.,1.),(1.,
1.),(1.,1.),(1.,1.),(1.,1.),(1.,1.),(1.,1.),(1.,1.),(1.,1.),(1.,1.),(1.,
1.),(1.,1.),(1.,1.),(1.,1.),(1.,1.),(1.,1.),(1.,1.),(1.,1.),(1.,1.),(1.,
1.),(1.,1.),(1.,1.),(1.,1.),(1.,1.),(1.,1.),(1.,1.),(1.,1.),(1.,1.),(1.,
1.),(1.,1.),(1.,1.),(1.,1.),(1.,1.),(1.,1.),(1.,1.),(1.,1.),(1.,1.),(1.,
1.),(1.,1.),(1.,1.),(1.,1.),(1.,1.),(1.,1.),(1.,1.),(1.,1.),(1.,1.),(1.,
1.),(1.,1.)))
REPRESENTATION_ITEM('')
SURFACE()
);
#114=(
BOUNDED_SURFACE()
B_SPLINE_SURFACE(5,1,((#60559,#60560),(#60561,#60562),(#60563,#60564),(#60565,
#60566),(#60567,#60568),(#60569,#60570),(#60571,#60572),(#60573,#60574),
(#60575,#60576),(#60577,#60578),(#60579,#60580),(#60581,#60582),(#60583,
#60584),(#60585,#60586),(#60587,#60588),(#60589,#60590),(#60591,#60592),
(#60593,#60594),(#60595,#60596),(#60597,#60598),(#60599,#60600),(#60601,
#60602),(#60603,#60604),(#60605,#60606),(#60607,#60608),(#60609,#60610),
(#60611,#60612),(#60613,#60614),(#60615,#60616),(#60617,#60618),(#60619,
#60620),(#60621,#60622),(#60623,#60624),(#60625,#60626),(#60627,#60628),
(#60629,#60630),(#60631,#60632),(#60633,#60634),(#60635,#60636),(#60637,
#60638),(#60639,#60640),(#60641,#60642),(#60643,#60644),(#60645,#60646),
(#60647,#60648),(#60649,#60650),(#60651,#60652),(#60653,#60654),(#60655,
#60656),(#60657,#60658),(#60659,#60660),(#60661,#60662),(#60663,#60664),
(#60665,#60666),(#60667,#60668),(#60669,#60670),(#60671,#60672),(#60673,
#60674),(#60675,#60676),(#60677,#60678),(#60679,#60680),(#60681,#60682),
(#60683,#60684),(#60685,#60686),(#60687,#60688),(#60689,#60690),(#60691,
#60692),(#60693,#60694),(#60695,#60696),(#60697,#60698)),.UNSPECIFIED.,
 .F.,.F.,.F.)
B_SPLINE_SURFACE_WITH_KNOTS((6,1,1,1,1,1,1,1,1,1,1,1,1,1,1,1,1,1,1,1,1,
1,1,1,1,1,1,1,1,1,1,1,1,1,1,1,1,1,1,1,1,1,1,1,1,1,1,1,1,1,1,1,1,1,1,1,1,
1,1,1,1,1,1,1,1,6),(2,2),(-1.,-0.984615384615383,-0.969230769230768,-0.953846153846152,
-0.938461538461537,-0.923076923076922,-0.907692307692306,-0.892307692307691,
-0.876923076923076,-0.86153846153846,-0.846153846153845,-0.83076923076923,
-0.815384615384614,-0.799999999999999,-0.784615384615384,-0.769230769230768,
-0.753846153846153,-0.738461538461538,-0.723076923076922,-0.707692307692307,
-0.692307692307692,-0.676923076923076,-0.661538461538461,-0.646153846153846,
-0.63076923076923,-0.615384615384615,-0.6,-0.584615384615384,-0.569230769230769,
-0.553846153846154,-0.538461538461538,-0.523076923076923,-0.507692307692308,
-0.492307692307692,-0.476923076923077,-0.461538461538462,-0.446153846153846,
-0.430769230769231,-0.415384615384615,-0.4,-0.384615384615385,-0.369230769230769,
-0.353846153846154,-0.338461538461538,-0.323076923076923,-0.307692307692308,
-0.292307692307692,-0.276923076923077,-0.261538461538462,-0.246153846153846,
-0.230769230769231,-0.215384615384615,-0.2,-0.184615384615385,-0.169230769230769,
-0.153846153846154,-0.138461538461538,-0.123076923076923,-0.107692307692308,
-0.0923076923076923,-0.0769230769230769,-0.0615384615384615,-0.0461538461538462,
-0.0307692307692308,-0.0153846153846154,0.),(-1.,1.),.UNSPECIFIED.)
GEOMETRIC_REPRESENTATION_ITEM()
RATIONAL_B_SPLINE_SURFACE(((1.,1.),(1.,1.),(1.,1.),(1.,1.),(1.,1.),(1.,
1.),(1.,1.),(1.,1.),(1.,1.),(1.,1.),(1.,1.),(1.,1.),(1.,1.),(1.,1.),(1.,
1.),(1.,1.),(1.,1.),(1.,1.),(1.,1.),(1.,1.),(1.,1.),(1.,1.),(1.,1.),(1.,
1.),(1.,1.),(1.,1.),(1.,1.),(1.,1.),(1.,1.),(1.,1.),(1.,1.),(1.,1.),(1.,
1.),(1.,1.),(1.,1.),(1.,1.),(1.,1.),(1.,1.),(1.,1.),(1.,1.),(1.,1.),(1.,
1.),(1.,1.),(1.,1.),(1.,1.),(1.,1.),(1.,1.),(1.,1.),(1.,1.),(1.,1.),(1.,
1.),(1.,1.),(1.,1.),(1.,1.),(1.,1.),(1.,1.),(1.,1.),(1.,1.),(1.,1.),(1.,
1.),(1.,1.),(1.,1.),(1.,1.),(1.,1.),(1.,1.),(1.,1.),(1.,1.),(1.,1.),(1.,
1.),(1.,1.)))
REPRESENTATION_ITEM('')
SURFACE()
);
#115=(
BOUNDED_SURFACE()
B_SPLINE_SURFACE(5,1,((#60789,#60790),(#60791,#60792),(#60793,#60794),(#60795,
#60796),(#60797,#60798),(#60799,#60800),(#60801,#60802),(#60803,#60804),
(#60805,#60806),(#60807,#60808),(#60809,#60810),(#60811,#60812),(#60813,
#60814),(#60815,#60816),(#60817,#60818),(#60819,#60820),(#60821,#60822),
(#60823,#60824),(#60825,#60826),(#60827,#60828),(#60829,#60830),(#60831,
#60832),(#60833,#60834),(#60835,#60836),(#60837,#60838),(#60839,#60840),
(#60841,#60842),(#60843,#60844),(#60845,#60846),(#60847,#60848),(#60849,
#60850),(#60851,#60852),(#60853,#60854),(#60855,#60856),(#60857,#60858),
(#60859,#60860),(#60861,#60862),(#60863,#60864),(#60865,#60866),(#60867,
#60868),(#60869,#60870),(#60871,#60872),(#60873,#60874),(#60875,#60876),
(#60877,#60878),(#60879,#60880),(#60881,#60882),(#60883,#60884),(#60885,
#60886),(#60887,#60888),(#60889,#60890),(#60891,#60892),(#60893,#60894),
(#60895,#60896),(#60897,#60898),(#60899,#60900),(#60901,#60902),(#60903,
#60904),(#60905,#60906),(#60907,#60908),(#60909,#60910),(#60911,#60912),
(#60913,#60914),(#60915,#60916),(#60917,#60918),(#60919,#60920),(#60921,
#60922),(#60923,#60924),(#60925,#60926),(#60927,#60928)),.UNSPECIFIED.,
 .F.,.F.,.F.)
B_SPLINE_SURFACE_WITH_KNOTS((6,1,1,1,1,1,1,1,1,1,1,1,1,1,1,1,1,1,1,1,1,
1,1,1,1,1,1,1,1,1,1,1,1,1,1,1,1,1,1,1,1,1,1,1,1,1,1,1,1,1,1,1,1,1,1,1,1,
1,1,1,1,1,1,1,1,6),(2,2),(-1.,-0.984615384615383,-0.969230769230768,-0.953846153846152,
-0.938461538461537,-0.923076923076922,-0.907692307692306,-0.892307692307691,
-0.876923076923076,-0.86153846153846,-0.846153846153845,-0.83076923076923,
-0.815384615384614,-0.799999999999999,-0.784615384615384,-0.769230769230768,
-0.753846153846153,-0.738461538461538,-0.723076923076922,-0.707692307692307,
-0.692307692307692,-0.676923076923076,-0.661538461538461,-0.646153846153846,
-0.63076923076923,-0.615384615384615,-0.6,-0.584615384615384,-0.569230769230769,
-0.553846153846154,-0.538461538461538,-0.523076923076923,-0.507692307692308,
-0.492307692307692,-0.476923076923077,-0.461538461538462,-0.446153846153846,
-0.430769230769231,-0.415384615384615,-0.4,-0.384615384615385,-0.369230769230769,
-0.353846153846154,-0.338461538461538,-0.323076923076923,-0.307692307692308,
-0.292307692307692,-0.276923076923077,-0.261538461538462,-0.246153846153846,
-0.230769230769231,-0.215384615384615,-0.2,-0.184615384615385,-0.169230769230769,
-0.153846153846154,-0.138461538461538,-0.123076923076923,-0.107692307692308,
-0.0923076923076923,-0.0769230769230769,-0.0615384615384615,-0.0461538461538462,
-0.0307692307692308,-0.0153846153846154,0.),(-1.,1.),.UNSPECIFIED.)
GEOMETRIC_REPRESENTATION_ITEM()
RATIONAL_B_SPLINE_SURFACE(((1.,1.),(1.,1.),(1.,1.),(1.,1.),(1.,1.),(1.,
1.),(1.,1.),(1.,1.),(1.,1.),(1.,1.),(1.,1.),(1.,1.),(1.,1.),(1.,1.),(1.,
1.),(1.,1.),(1.,1.),(1.,1.),(1.,1.),(1.,1.),(1.,1.),(1.,1.),(1.,1.),(1.,
1.),(1.,1.),(1.,1.),(1.,1.),(1.,1.),(1.,1.),(1.,1.),(1.,1.),(1.,1.),(1.,
1.),(1.,1.),(1.,1.),(1.,1.),(1.,1.),(1.,1.),(1.,1.),(1.,1.),(1.,1.),(1.,
1.),(1.,1.),(1.,1.),(1.,1.),(1.,1.),(1.,1.),(1.,1.),(1.,1.),(1.,1.),(1.,
1.),(1.,1.),(1.,1.),(1.,1.),(1.,1.),(1.,1.),(1.,1.),(1.,1.),(1.,1.),(1.,
1.),(1.,1.),(1.,1.),(1.,1.),(1.,1.),(1.,1.),(1.,1.),(1.,1.),(1.,1.),(1.,
1.),(1.,1.)))
REPRESENTATION_ITEM('')
SURFACE()
);
#116=(
BOUNDED_SURFACE()
B_SPLINE_SURFACE(5,1,((#61001,#61002),(#61003,#61004),(#61005,#61006),(#61007,
#61008),(#61009,#61010),(#61011,#61012),(#61013,#61014),(#61015,#61016),
(#61017,#61018),(#61019,#61020),(#61021,#61022),(#61023,#61024),(#61025,
#61026),(#61027,#61028),(#61029,#61030),(#61031,#61032),(#61033,#61034),
(#61035,#61036),(#61037,#61038),(#61039,#61040),(#61041,#61042),(#61043,
#61044),(#61045,#61046),(#61047,#61048),(#61049,#61050),(#61051,#61052),
(#61053,#61054),(#61055,#61056),(#61057,#61058),(#61059,#61060),(#61061,
#61062),(#61063,#61064),(#61065,#61066),(#61067,#61068),(#61069,#61070),
(#61071,#61072),(#61073,#61074),(#61075,#61076),(#61077,#61078),(#61079,
#61080),(#61081,#61082),(#61083,#61084),(#61085,#61086),(#61087,#61088),
(#61089,#61090),(#61091,#61092),(#61093,#61094),(#61095,#61096),(#61097,
#61098),(#61099,#61100),(#61101,#61102),(#61103,#61104),(#61105,#61106),
(#61107,#61108),(#61109,#61110),(#61111,#61112),(#61113,#61114),(#61115,
#61116),(#61117,#61118),(#61119,#61120),(#61121,#61122),(#61123,#61124),
(#61125,#61126),(#61127,#61128),(#61129,#61130),(#61131,#61132),(#61133,
#61134),(#61135,#61136),(#61137,#61138),(#61139,#61140)),.UNSPECIFIED.,
 .F.,.F.,.F.)
B_SPLINE_SURFACE_WITH_KNOTS((6,1,1,1,1,1,1,1,1,1,1,1,1,1,1,1,1,1,1,1,1,
1,1,1,1,1,1,1,1,1,1,1,1,1,1,1,1,1,1,1,1,1,1,1,1,1,1,1,1,1,1,1,1,1,1,1,1,
1,1,1,1,1,1,1,1,6),(2,2),(-1.,-0.984615384615383,-0.969230769230768,-0.953846153846152,
-0.938461538461537,-0.923076923076922,-0.907692307692306,-0.892307692307691,
-0.876923076923076,-0.86153846153846,-0.846153846153845,-0.83076923076923,
-0.815384615384614,-0.799999999999999,-0.784615384615384,-0.769230769230768,
-0.753846153846153,-0.738461538461538,-0.723076923076922,-0.707692307692307,
-0.692307692307692,-0.676923076923076,-0.661538461538461,-0.646153846153846,
-0.63076923076923,-0.615384615384615,-0.6,-0.584615384615384,-0.569230769230769,
-0.553846153846154,-0.538461538461538,-0.523076923076923,-0.507692307692308,
-0.492307692307692,-0.476923076923077,-0.461538461538462,-0.446153846153846,
-0.430769230769231,-0.415384615384615,-0.4,-0.384615384615385,-0.369230769230769,
-0.353846153846154,-0.338461538461538,-0.323076923076923,-0.307692307692308,
-0.292307692307692,-0.276923076923077,-0.261538461538462,-0.246153846153846,
-0.230769230769231,-0.215384615384615,-0.2,-0.184615384615385,-0.169230769230769,
-0.153846153846154,-0.138461538461538,-0.123076923076923,-0.107692307692308,
-0.0923076923076923,-0.0769230769230769,-0.0615384615384615,-0.0461538461538462,
-0.0307692307692308,-0.0153846153846154,0.),(-1.,1.),.UNSPECIFIED.)
GEOMETRIC_REPRESENTATION_ITEM()
RATIONAL_B_SPLINE_SURFACE(((1.,1.),(1.,1.),(1.,1.),(1.,1.),(1.,1.),(1.,
1.),(1.,1.),(1.,1.),(1.,1.),(1.,1.),(1.,1.),(1.,1.),(1.,1.),(1.,1.),(1.,
1.),(1.,1.),(1.,1.),(1.,1.),(1.,1.),(1.,1.),(1.,1.),(1.,1.),(1.,1.),(1.,
1.),(1.,1.),(1.,1.),(1.,1.),(1.,1.),(1.,1.),(1.,1.),(1.,1.),(1.,1.),(1.,
1.),(1.,1.),(1.,1.),(1.,1.),(1.,1.),(1.,1.),(1.,1.),(1.,1.),(1.,1.),(1.,
1.),(1.,1.),(1.,1.),(1.,1.),(1.,1.),(1.,1.),(1.,1.),(1.,1.),(1.,1.),(1.,
1.),(1.,1.),(1.,1.),(1.,1.),(1.,1.),(1.,1.),(1.,1.),(1.,1.),(1.,1.),(1.,
1.),(1.,1.),(1.,1.),(1.,1.),(1.,1.),(1.,1.),(1.,1.),(1.,1.),(1.,1.),(1.,
1.),(1.,1.)))
REPRESENTATION_ITEM('')
SURFACE()
);
#117=(
BOUNDED_SURFACE()
B_SPLINE_SURFACE(5,1,((#61231,#61232),(#61233,#61234),(#61235,#61236),(#61237,
#61238),(#61239,#61240),(#61241,#61242),(#61243,#61244),(#61245,#61246),
(#61247,#61248),(#61249,#61250),(#61251,#61252),(#61253,#61254),(#61255,
#61256),(#61257,#61258),(#61259,#61260),(#61261,#61262),(#61263,#61264),
(#61265,#61266),(#61267,#61268),(#61269,#61270),(#61271,#61272),(#61273,
#61274),(#61275,#61276),(#61277,#61278),(#61279,#61280),(#61281,#61282),
(#61283,#61284),(#61285,#61286),(#61287,#61288),(#61289,#61290),(#61291,
#61292),(#61293,#61294),(#61295,#61296),(#61297,#61298),(#61299,#61300),
(#61301,#61302),(#61303,#61304),(#61305,#61306),(#61307,#61308),(#61309,
#61310),(#61311,#61312),(#61313,#61314),(#61315,#61316),(#61317,#61318),
(#61319,#61320),(#61321,#61322),(#61323,#61324),(#61325,#61326),(#61327,
#61328),(#61329,#61330),(#61331,#61332),(#61333,#61334),(#61335,#61336),
(#61337,#61338),(#61339,#61340),(#61341,#61342),(#61343,#61344),(#61345,
#61346),(#61347,#61348),(#61349,#61350),(#61351,#61352),(#61353,#61354),
(#61355,#61356),(#61357,#61358),(#61359,#61360),(#61361,#61362),(#61363,
#61364),(#61365,#61366),(#61367,#61368),(#61369,#61370)),.UNSPECIFIED.,
 .F.,.F.,.F.)
B_SPLINE_SURFACE_WITH_KNOTS((6,1,1,1,1,1,1,1,1,1,1,1,1,1,1,1,1,1,1,1,1,
1,1,1,1,1,1,1,1,1,1,1,1,1,1,1,1,1,1,1,1,1,1,1,1,1,1,1,1,1,1,1,1,1,1,1,1,
1,1,1,1,1,1,1,1,6),(2,2),(-1.,-0.984615384615383,-0.969230769230768,-0.953846153846152,
-0.938461538461537,-0.923076923076922,-0.907692307692306,-0.892307692307691,
-0.876923076923076,-0.86153846153846,-0.846153846153845,-0.83076923076923,
-0.815384615384614,-0.799999999999999,-0.784615384615384,-0.769230769230768,
-0.753846153846153,-0.738461538461538,-0.723076923076922,-0.707692307692307,
-0.692307692307692,-0.676923076923076,-0.661538461538461,-0.646153846153846,
-0.63076923076923,-0.615384615384615,-0.6,-0.584615384615384,-0.569230769230769,
-0.553846153846154,-0.538461538461538,-0.523076923076923,-0.507692307692308,
-0.492307692307692,-0.476923076923077,-0.461538461538462,-0.446153846153846,
-0.430769230769231,-0.415384615384615,-0.4,-0.384615384615385,-0.369230769230769,
-0.353846153846154,-0.338461538461538,-0.323076923076923,-0.307692307692308,
-0.292307692307692,-0.276923076923077,-0.261538461538462,-0.246153846153846,
-0.230769230769231,-0.215384615384615,-0.2,-0.184615384615385,-0.169230769230769,
-0.153846153846154,-0.138461538461538,-0.123076923076923,-0.107692307692308,
-0.0923076923076923,-0.0769230769230769,-0.0615384615384615,-0.0461538461538462,
-0.0307692307692308,-0.0153846153846154,0.),(-1.,1.),.UNSPECIFIED.)
GEOMETRIC_REPRESENTATION_ITEM()
RATIONAL_B_SPLINE_SURFACE(((1.,1.),(1.,1.),(1.,1.),(1.,1.),(1.,1.),(1.,
1.),(1.,1.),(1.,1.),(1.,1.),(1.,1.),(1.,1.),(1.,1.),(1.,1.),(1.,1.),(1.,
1.),(1.,1.),(1.,1.),(1.,1.),(1.,1.),(1.,1.),(1.,1.),(1.,1.),(1.,1.),(1.,
1.),(1.,1.),(1.,1.),(1.,1.),(1.,1.),(1.,1.),(1.,1.),(1.,1.),(1.,1.),(1.,
1.),(1.,1.),(1.,1.),(1.,1.),(1.,1.),(1.,1.),(1.,1.),(1.,1.),(1.,1.),(1.,
1.),(1.,1.),(1.,1.),(1.,1.),(1.,1.),(1.,1.),(1.,1.),(1.,1.),(1.,1.),(1.,
1.),(1.,1.),(1.,1.),(1.,1.),(1.,1.),(1.,1.),(1.,1.),(1.,1.),(1.,1.),(1.,
1.),(1.,1.),(1.,1.),(1.,1.),(1.,1.),(1.,1.),(1.,1.),(1.,1.),(1.,1.),(1.,
1.),(1.,1.)))
REPRESENTATION_ITEM('')
SURFACE()
);
#118=(
BOUNDED_SURFACE()
B_SPLINE_SURFACE(5,1,((#61443,#61444),(#61445,#61446),(#61447,#61448),(#61449,
#61450),(#61451,#61452),(#61453,#61454),(#61455,#61456),(#61457,#61458),
(#61459,#61460),(#61461,#61462),(#61463,#61464),(#61465,#61466),(#61467,
#61468),(#61469,#61470),(#61471,#61472),(#61473,#61474),(#61475,#61476),
(#61477,#61478),(#61479,#61480),(#61481,#61482),(#61483,#61484),(#61485,
#61486),(#61487,#61488),(#61489,#61490),(#61491,#61492),(#61493,#61494),
(#61495,#61496),(#61497,#61498),(#61499,#61500),(#61501,#61502),(#61503,
#61504),(#61505,#61506),(#61507,#61508),(#61509,#61510),(#61511,#61512),
(#61513,#61514),(#61515,#61516),(#61517,#61518),(#61519,#61520),(#61521,
#61522),(#61523,#61524),(#61525,#61526),(#61527,#61528),(#61529,#61530),
(#61531,#61532),(#61533,#61534),(#61535,#61536),(#61537,#61538),(#61539,
#61540),(#61541,#61542),(#61543,#61544),(#61545,#61546),(#61547,#61548),
(#61549,#61550),(#61551,#61552),(#61553,#61554),(#61555,#61556),(#61557,
#61558),(#61559,#61560),(#61561,#61562),(#61563,#61564),(#61565,#61566),
(#61567,#61568),(#61569,#61570),(#61571,#61572),(#61573,#61574),(#61575,
#61576),(#61577,#61578),(#61579,#61580),(#61581,#61582)),.UNSPECIFIED.,
 .F.,.F.,.F.)
B_SPLINE_SURFACE_WITH_KNOTS((6,1,1,1,1,1,1,1,1,1,1,1,1,1,1,1,1,1,1,1,1,
1,1,1,1,1,1,1,1,1,1,1,1,1,1,1,1,1,1,1,1,1,1,1,1,1,1,1,1,1,1,1,1,1,1,1,1,
1,1,1,1,1,1,1,1,6),(2,2),(-1.,-0.984615384615383,-0.969230769230768,-0.953846153846152,
-0.938461538461537,-0.923076923076922,-0.907692307692306,-0.892307692307691,
-0.876923076923076,-0.86153846153846,-0.846153846153845,-0.83076923076923,
-0.815384615384614,-0.799999999999999,-0.784615384615384,-0.769230769230768,
-0.753846153846153,-0.738461538461538,-0.723076923076922,-0.707692307692307,
-0.692307692307692,-0.676923076923076,-0.661538461538461,-0.646153846153846,
-0.63076923076923,-0.615384615384615,-0.6,-0.584615384615384,-0.569230769230769,
-0.553846153846154,-0.538461538461538,-0.523076923076923,-0.507692307692308,
-0.492307692307692,-0.476923076923077,-0.461538461538462,-0.446153846153846,
-0.430769230769231,-0.415384615384615,-0.4,-0.384615384615385,-0.369230769230769,
-0.353846153846154,-0.338461538461538,-0.323076923076923,-0.307692307692308,
-0.292307692307692,-0.276923076923077,-0.261538461538462,-0.246153846153846,
-0.230769230769231,-0.215384615384615,-0.2,-0.184615384615385,-0.169230769230769,
-0.153846153846154,-0.138461538461538,-0.123076923076923,-0.107692307692308,
-0.0923076923076923,-0.0769230769230769,-0.0615384615384615,-0.0461538461538462,
-0.0307692307692308,-0.0153846153846154,0.),(-1.,1.),.UNSPECIFIED.)
GEOMETRIC_REPRESENTATION_ITEM()
RATIONAL_B_SPLINE_SURFACE(((1.,1.),(1.,1.),(1.,1.),(1.,1.),(1.,1.),(1.,
1.),(1.,1.),(1.,1.),(1.,1.),(1.,1.),(1.,1.),(1.,1.),(1.,1.),(1.,1.),(1.,
1.),(1.,1.),(1.,1.),(1.,1.),(1.,1.),(1.,1.),(1.,1.),(1.,1.),(1.,1.),(1.,
1.),(1.,1.),(1.,1.),(1.,1.),(1.,1.),(1.,1.),(1.,1.),(1.,1.),(1.,1.),(1.,
1.),(1.,1.),(1.,1.),(1.,1.),(1.,1.),(1.,1.),(1.,1.),(1.,1.),(1.,1.),(1.,
1.),(1.,1.),(1.,1.),(1.,1.),(1.,1.),(1.,1.),(1.,1.),(1.,1.),(1.,1.),(1.,
1.),(1.,1.),(1.,1.),(1.,1.),(1.,1.),(1.,1.),(1.,1.),(1.,1.),(1.,1.),(1.,
1.),(1.,1.),(1.,1.),(1.,1.),(1.,1.),(1.,1.),(1.,1.),(1.,1.),(1.,1.),(1.,
1.),(1.,1.)))
REPRESENTATION_ITEM('')
SURFACE()
);
#119=(
BOUNDED_SURFACE()
B_SPLINE_SURFACE(5,1,((#61673,#61674),(#61675,#61676),(#61677,#61678),(#61679,
#61680),(#61681,#61682),(#61683,#61684),(#61685,#61686),(#61687,#61688),
(#61689,#61690),(#61691,#61692),(#61693,#61694),(#61695,#61696),(#61697,
#61698),(#61699,#61700),(#61701,#61702),(#61703,#61704),(#61705,#61706),
(#61707,#61708),(#61709,#61710),(#61711,#61712),(#61713,#61714),(#61715,
#61716),(#61717,#61718),(#61719,#61720),(#61721,#61722),(#61723,#61724),
(#61725,#61726),(#61727,#61728),(#61729,#61730),(#61731,#61732),(#61733,
#61734),(#61735,#61736),(#61737,#61738),(#61739,#61740),(#61741,#61742),
(#61743,#61744),(#61745,#61746),(#61747,#61748),(#61749,#61750),(#61751,
#61752),(#61753,#61754),(#61755,#61756),(#61757,#61758),(#61759,#61760),
(#61761,#61762),(#61763,#61764),(#61765,#61766),(#61767,#61768),(#61769,
#61770),(#61771,#61772),(#61773,#61774),(#61775,#61776),(#61777,#61778),
(#61779,#61780),(#61781,#61782),(#61783,#61784),(#61785,#61786),(#61787,
#61788),(#61789,#61790),(#61791,#61792),(#61793,#61794),(#61795,#61796),
(#61797,#61798),(#61799,#61800),(#61801,#61802),(#61803,#61804),(#61805,
#61806),(#61807,#61808),(#61809,#61810),(#61811,#61812)),.UNSPECIFIED.,
 .F.,.F.,.F.)
B_SPLINE_SURFACE_WITH_KNOTS((6,1,1,1,1,1,1,1,1,1,1,1,1,1,1,1,1,1,1,1,1,
1,1,1,1,1,1,1,1,1,1,1,1,1,1,1,1,1,1,1,1,1,1,1,1,1,1,1,1,1,1,1,1,1,1,1,1,
1,1,1,1,1,1,1,1,6),(2,2),(-1.,-0.984615384615383,-0.969230769230768,-0.953846153846152,
-0.938461538461537,-0.923076923076922,-0.907692307692306,-0.892307692307691,
-0.876923076923076,-0.86153846153846,-0.846153846153845,-0.83076923076923,
-0.815384615384614,-0.799999999999999,-0.784615384615384,-0.769230769230768,
-0.753846153846153,-0.738461538461538,-0.723076923076922,-0.707692307692307,
-0.692307692307692,-0.676923076923076,-0.661538461538461,-0.646153846153846,
-0.63076923076923,-0.615384615384615,-0.6,-0.584615384615384,-0.569230769230769,
-0.553846153846154,-0.538461538461538,-0.523076923076923,-0.507692307692308,
-0.492307692307692,-0.476923076923077,-0.461538461538462,-0.446153846153846,
-0.430769230769231,-0.415384615384615,-0.4,-0.384615384615385,-0.369230769230769,
-0.353846153846154,-0.338461538461538,-0.323076923076923,-0.307692307692308,
-0.292307692307692,-0.276923076923077,-0.261538461538462,-0.246153846153846,
-0.230769230769231,-0.215384615384615,-0.2,-0.184615384615385,-0.169230769230769,
-0.153846153846154,-0.138461538461538,-0.123076923076923,-0.107692307692308,
-0.0923076923076923,-0.0769230769230769,-0.0615384615384615,-0.0461538461538462,
-0.0307692307692308,-0.0153846153846154,0.),(-1.,1.),.UNSPECIFIED.)
GEOMETRIC_REPRESENTATION_ITEM()
RATIONAL_B_SPLINE_SURFACE(((1.,1.),(1.,1.),(1.,1.),(1.,1.),(1.,1.),(1.,
1.),(1.,1.),(1.,1.),(1.,1.),(1.,1.),(1.,1.),(1.,1.),(1.,1.),(1.,1.),(1.,
1.),(1.,1.),(1.,1.),(1.,1.),(1.,1.),(1.,1.),(1.,1.),(1.,1.),(1.,1.),(1.,
1.),(1.,1.),(1.,1.),(1.,1.),(1.,1.),(1.,1.),(1.,1.),(1.,1.),(1.,1.),(1.,
1.),(1.,1.),(1.,1.),(1.,1.),(1.,1.),(1.,1.),(1.,1.),(1.,1.),(1.,1.),(1.,
1.),(1.,1.),(1.,1.),(1.,1.),(1.,1.),(1.,1.),(1.,1.),(1.,1.),(1.,1.),(1.,
1.),(1.,1.),(1.,1.),(1.,1.),(1.,1.),(1.,1.),(1.,1.),(1.,1.),(1.,1.),(1.,
1.),(1.,1.),(1.,1.),(1.,1.),(1.,1.),(1.,1.),(1.,1.),(1.,1.),(1.,1.),(1.,
1.),(1.,1.)))
REPRESENTATION_ITEM('')
SURFACE()
);
#120=(
BOUNDED_SURFACE()
B_SPLINE_SURFACE(5,1,((#61885,#61886),(#61887,#61888),(#61889,#61890),(#61891,
#61892),(#61893,#61894),(#61895,#61896),(#61897,#61898),(#61899,#61900),
(#61901,#61902),(#61903,#61904),(#61905,#61906),(#61907,#61908),(#61909,
#61910),(#61911,#61912),(#61913,#61914),(#61915,#61916),(#61917,#61918),
(#61919,#61920),(#61921,#61922),(#61923,#61924),(#61925,#61926),(#61927,
#61928),(#61929,#61930),(#61931,#61932),(#61933,#61934),(#61935,#61936),
(#61937,#61938),(#61939,#61940),(#61941,#61942),(#61943,#61944),(#61945,
#61946),(#61947,#61948),(#61949,#61950),(#61951,#61952),(#61953,#61954),
(#61955,#61956),(#61957,#61958),(#61959,#61960),(#61961,#61962),(#61963,
#61964),(#61965,#61966),(#61967,#61968),(#61969,#61970),(#61971,#61972),
(#61973,#61974),(#61975,#61976),(#61977,#61978),(#61979,#61980),(#61981,
#61982),(#61983,#61984),(#61985,#61986),(#61987,#61988),(#61989,#61990),
(#61991,#61992),(#61993,#61994),(#61995,#61996),(#61997,#61998),(#61999,
#62000),(#62001,#62002),(#62003,#62004),(#62005,#62006),(#62007,#62008),
(#62009,#62010),(#62011,#62012),(#62013,#62014),(#62015,#62016),(#62017,
#62018),(#62019,#62020),(#62021,#62022),(#62023,#62024)),.UNSPECIFIED.,
 .F.,.F.,.F.)
B_SPLINE_SURFACE_WITH_KNOTS((6,1,1,1,1,1,1,1,1,1,1,1,1,1,1,1,1,1,1,1,1,
1,1,1,1,1,1,1,1,1,1,1,1,1,1,1,1,1,1,1,1,1,1,1,1,1,1,1,1,1,1,1,1,1,1,1,1,
1,1,1,1,1,1,1,1,6),(2,2),(-1.,-0.984615384615383,-0.969230769230768,-0.953846153846152,
-0.938461538461537,-0.923076923076922,-0.907692307692306,-0.892307692307691,
-0.876923076923076,-0.86153846153846,-0.846153846153845,-0.83076923076923,
-0.815384615384614,-0.799999999999999,-0.784615384615384,-0.769230769230768,
-0.753846153846153,-0.738461538461538,-0.723076923076922,-0.707692307692307,
-0.692307692307692,-0.676923076923076,-0.661538461538461,-0.646153846153846,
-0.63076923076923,-0.615384615384615,-0.6,-0.584615384615384,-0.569230769230769,
-0.553846153846154,-0.538461538461538,-0.523076923076923,-0.507692307692308,
-0.492307692307692,-0.476923076923077,-0.461538461538462,-0.446153846153846,
-0.430769230769231,-0.415384615384615,-0.4,-0.384615384615385,-0.369230769230769,
-0.353846153846154,-0.338461538461538,-0.323076923076923,-0.307692307692308,
-0.292307692307692,-0.276923076923077,-0.261538461538462,-0.246153846153846,
-0.230769230769231,-0.215384615384615,-0.2,-0.184615384615385,-0.169230769230769,
-0.153846153846154,-0.138461538461538,-0.123076923076923,-0.107692307692308,
-0.0923076923076923,-0.0769230769230769,-0.0615384615384615,-0.0461538461538462,
-0.0307692307692308,-0.0153846153846154,0.),(-1.,1.),.UNSPECIFIED.)
GEOMETRIC_REPRESENTATION_ITEM()
RATIONAL_B_SPLINE_SURFACE(((1.,1.),(1.,1.),(1.,1.),(1.,1.),(1.,1.),(1.,
1.),(1.,1.),(1.,1.),(1.,1.),(1.,1.),(1.,1.),(1.,1.),(1.,1.),(1.,1.),(1.,
1.),(1.,1.),(1.,1.),(1.,1.),(1.,1.),(1.,1.),(1.,1.),(1.,1.),(1.,1.),(1.,
1.),(1.,1.),(1.,1.),(1.,1.),(1.,1.),(1.,1.),(1.,1.),(1.,1.),(1.,1.),(1.,
1.),(1.,1.),(1.,1.),(1.,1.),(1.,1.),(1.,1.),(1.,1.),(1.,1.),(1.,1.),(1.,
1.),(1.,1.),(1.,1.),(1.,1.),(1.,1.),(1.,1.),(1.,1.),(1.,1.),(1.,1.),(1.,
1.),(1.,1.),(1.,1.),(1.,1.),(1.,1.),(1.,1.),(1.,1.),(1.,1.),(1.,1.),(1.,
1.),(1.,1.),(1.,1.),(1.,1.),(1.,1.),(1.,1.),(1.,1.),(1.,1.),(1.,1.),(1.,
1.),(1.,1.)))
REPRESENTATION_ITEM('')
SURFACE()
);
#121=(
BOUNDED_SURFACE()
B_SPLINE_SURFACE(5,1,((#62115,#62116),(#62117,#62118),(#62119,#62120),(#62121,
#62122),(#62123,#62124),(#62125,#62126),(#62127,#62128),(#62129,#62130),
(#62131,#62132),(#62133,#62134),(#62135,#62136),(#62137,#62138),(#62139,
#62140),(#62141,#62142),(#62143,#62144),(#62145,#62146),(#62147,#62148),
(#62149,#62150),(#62151,#62152),(#62153,#62154),(#62155,#62156),(#62157,
#62158),(#62159,#62160),(#62161,#62162),(#62163,#62164),(#62165,#62166),
(#62167,#62168),(#62169,#62170),(#62171,#62172),(#62173,#62174),(#62175,
#62176),(#62177,#62178),(#62179,#62180),(#62181,#62182),(#62183,#62184),
(#62185,#62186),(#62187,#62188),(#62189,#62190),(#62191,#62192),(#62193,
#62194),(#62195,#62196),(#62197,#62198),(#62199,#62200),(#62201,#62202),
(#62203,#62204),(#62205,#62206),(#62207,#62208),(#62209,#62210),(#62211,
#62212),(#62213,#62214),(#62215,#62216),(#62217,#62218),(#62219,#62220),
(#62221,#62222),(#62223,#62224),(#62225,#62226),(#62227,#62228),(#62229,
#62230),(#62231,#62232),(#62233,#62234),(#62235,#62236),(#62237,#62238),
(#62239,#62240),(#62241,#62242),(#62243,#62244),(#62245,#62246),(#62247,
#62248),(#62249,#62250),(#62251,#62252),(#62253,#62254)),.UNSPECIFIED.,
 .F.,.F.,.F.)
B_SPLINE_SURFACE_WITH_KNOTS((6,1,1,1,1,1,1,1,1,1,1,1,1,1,1,1,1,1,1,1,1,
1,1,1,1,1,1,1,1,1,1,1,1,1,1,1,1,1,1,1,1,1,1,1,1,1,1,1,1,1,1,1,1,1,1,1,1,
1,1,1,1,1,1,1,1,6),(2,2),(-1.,-0.984615384615383,-0.969230769230768,-0.953846153846152,
-0.938461538461537,-0.923076923076922,-0.907692307692306,-0.892307692307691,
-0.876923076923076,-0.86153846153846,-0.846153846153845,-0.83076923076923,
-0.815384615384614,-0.799999999999999,-0.784615384615384,-0.769230769230768,
-0.753846153846153,-0.738461538461538,-0.723076923076922,-0.707692307692307,
-0.692307692307692,-0.676923076923076,-0.661538461538461,-0.646153846153846,
-0.63076923076923,-0.615384615384615,-0.6,-0.584615384615384,-0.569230769230769,
-0.553846153846154,-0.538461538461538,-0.523076923076923,-0.507692307692308,
-0.492307692307692,-0.476923076923077,-0.461538461538462,-0.446153846153846,
-0.430769230769231,-0.415384615384615,-0.4,-0.384615384615385,-0.369230769230769,
-0.353846153846154,-0.338461538461538,-0.323076923076923,-0.307692307692308,
-0.292307692307692,-0.276923076923077,-0.261538461538462,-0.246153846153846,
-0.230769230769231,-0.215384615384615,-0.2,-0.184615384615385,-0.169230769230769,
-0.153846153846154,-0.138461538461538,-0.123076923076923,-0.107692307692308,
-0.0923076923076923,-0.0769230769230769,-0.0615384615384615,-0.0461538461538462,
-0.0307692307692308,-0.0153846153846154,0.),(-1.,1.),.UNSPECIFIED.)
GEOMETRIC_REPRESENTATION_ITEM()
RATIONAL_B_SPLINE_SURFACE(((1.,1.),(1.,1.),(1.,1.),(1.,1.),(1.,1.),(1.,
1.),(1.,1.),(1.,1.),(1.,1.),(1.,1.),(1.,1.),(1.,1.),(1.,1.),(1.,1.),(1.,
1.),(1.,1.),(1.,1.),(1.,1.),(1.,1.),(1.,1.),(1.,1.),(1.,1.),(1.,1.),(1.,
1.),(1.,1.),(1.,1.),(1.,1.),(1.,1.),(1.,1.),(1.,1.),(1.,1.),(1.,1.),(1.,
1.),(1.,1.),(1.,1.),(1.,1.),(1.,1.),(1.,1.),(1.,1.),(1.,1.),(1.,1.),(1.,
1.),(1.,1.),(1.,1.),(1.,1.),(1.,1.),(1.,1.),(1.,1.),(1.,1.),(1.,1.),(1.,
1.),(1.,1.),(1.,1.),(1.,1.),(1.,1.),(1.,1.),(1.,1.),(1.,1.),(1.,1.),(1.,
1.),(1.,1.),(1.,1.),(1.,1.),(1.,1.),(1.,1.),(1.,1.),(1.,1.),(1.,1.),(1.,
1.),(1.,1.)))
REPRESENTATION_ITEM('')
SURFACE()
);
#122=(
BOUNDED_SURFACE()
B_SPLINE_SURFACE(5,1,((#62327,#62328),(#62329,#62330),(#62331,#62332),(#62333,
#62334),(#62335,#62336),(#62337,#62338),(#62339,#62340),(#62341,#62342),
(#62343,#62344),(#62345,#62346),(#62347,#62348),(#62349,#62350),(#62351,
#62352),(#62353,#62354),(#62355,#62356),(#62357,#62358),(#62359,#62360),
(#62361,#62362),(#62363,#62364),(#62365,#62366),(#62367,#62368),(#62369,
#62370),(#62371,#62372),(#62373,#62374),(#62375,#62376),(#62377,#62378),
(#62379,#62380),(#62381,#62382),(#62383,#62384),(#62385,#62386),(#62387,
#62388),(#62389,#62390),(#62391,#62392),(#62393,#62394),(#62395,#62396),
(#62397,#62398),(#62399,#62400),(#62401,#62402),(#62403,#62404),(#62405,
#62406),(#62407,#62408),(#62409,#62410),(#62411,#62412),(#62413,#62414),
(#62415,#62416),(#62417,#62418),(#62419,#62420),(#62421,#62422),(#62423,
#62424),(#62425,#62426),(#62427,#62428),(#62429,#62430),(#62431,#62432),
(#62433,#62434),(#62435,#62436),(#62437,#62438),(#62439,#62440),(#62441,
#62442),(#62443,#62444),(#62445,#62446),(#62447,#62448),(#62449,#62450),
(#62451,#62452),(#62453,#62454),(#62455,#62456),(#62457,#62458),(#62459,
#62460),(#62461,#62462),(#62463,#62464),(#62465,#62466)),.UNSPECIFIED.,
 .F.,.F.,.F.)
B_SPLINE_SURFACE_WITH_KNOTS((6,1,1,1,1,1,1,1,1,1,1,1,1,1,1,1,1,1,1,1,1,
1,1,1,1,1,1,1,1,1,1,1,1,1,1,1,1,1,1,1,1,1,1,1,1,1,1,1,1,1,1,1,1,1,1,1,1,
1,1,1,1,1,1,1,1,6),(2,2),(-1.,-0.984615384615383,-0.969230769230768,-0.953846153846152,
-0.938461538461537,-0.923076923076922,-0.907692307692306,-0.892307692307691,
-0.876923076923076,-0.86153846153846,-0.846153846153845,-0.83076923076923,
-0.815384615384614,-0.799999999999999,-0.784615384615384,-0.769230769230768,
-0.753846153846153,-0.738461538461538,-0.723076923076922,-0.707692307692307,
-0.692307692307692,-0.676923076923076,-0.661538461538461,-0.646153846153846,
-0.63076923076923,-0.615384615384615,-0.6,-0.584615384615384,-0.569230769230769,
-0.553846153846154,-0.538461538461538,-0.523076923076923,-0.507692307692308,
-0.492307692307692,-0.476923076923077,-0.461538461538462,-0.446153846153846,
-0.430769230769231,-0.415384615384615,-0.4,-0.384615384615385,-0.369230769230769,
-0.353846153846154,-0.338461538461538,-0.323076923076923,-0.307692307692308,
-0.292307692307692,-0.276923076923077,-0.261538461538462,-0.246153846153846,
-0.230769230769231,-0.215384615384615,-0.2,-0.184615384615385,-0.169230769230769,
-0.153846153846154,-0.138461538461538,-0.123076923076923,-0.107692307692308,
-0.0923076923076923,-0.0769230769230769,-0.0615384615384615,-0.0461538461538462,
-0.0307692307692308,-0.0153846153846154,0.),(-1.,1.),.UNSPECIFIED.)
GEOMETRIC_REPRESENTATION_ITEM()
RATIONAL_B_SPLINE_SURFACE(((1.,1.),(1.,1.),(1.,1.),(1.,1.),(1.,1.),(1.,
1.),(1.,1.),(1.,1.),(1.,1.),(1.,1.),(1.,1.),(1.,1.),(1.,1.),(1.,1.),(1.,
1.),(1.,1.),(1.,1.),(1.,1.),(1.,1.),(1.,1.),(1.,1.),(1.,1.),(1.,1.),(1.,
1.),(1.,1.),(1.,1.),(1.,1.),(1.,1.),(1.,1.),(1.,1.),(1.,1.),(1.,1.),(1.,
1.),(1.,1.),(1.,1.),(1.,1.),(1.,1.),(1.,1.),(1.,1.),(1.,1.),(1.,1.),(1.,
1.),(1.,1.),(1.,1.),(1.,1.),(1.,1.),(1.,1.),(1.,1.),(1.,1.),(1.,1.),(1.,
1.),(1.,1.),(1.,1.),(1.,1.),(1.,1.),(1.,1.),(1.,1.),(1.,1.),(1.,1.),(1.,
1.),(1.,1.),(1.,1.),(1.,1.),(1.,1.),(1.,1.),(1.,1.),(1.,1.),(1.,1.),(1.,
1.),(1.,1.)))
REPRESENTATION_ITEM('')
SURFACE()
);
#123=(
BOUNDED_SURFACE()
B_SPLINE_SURFACE(5,1,((#62557,#62558),(#62559,#62560),(#62561,#62562),(#62563,
#62564),(#62565,#62566),(#62567,#62568),(#62569,#62570),(#62571,#62572),
(#62573,#62574),(#62575,#62576),(#62577,#62578),(#62579,#62580),(#62581,
#62582),(#62583,#62584),(#62585,#62586),(#62587,#62588),(#62589,#62590),
(#62591,#62592),(#62593,#62594),(#62595,#62596),(#62597,#62598),(#62599,
#62600),(#62601,#62602),(#62603,#62604),(#62605,#62606),(#62607,#62608),
(#62609,#62610),(#62611,#62612),(#62613,#62614),(#62615,#62616),(#62617,
#62618),(#62619,#62620),(#62621,#62622),(#62623,#62624),(#62625,#62626),
(#62627,#62628),(#62629,#62630),(#62631,#62632),(#62633,#62634),(#62635,
#62636),(#62637,#62638),(#62639,#62640),(#62641,#62642),(#62643,#62644),
(#62645,#62646),(#62647,#62648),(#62649,#62650),(#62651,#62652),(#62653,
#62654),(#62655,#62656),(#62657,#62658),(#62659,#62660),(#62661,#62662),
(#62663,#62664),(#62665,#62666),(#62667,#62668),(#62669,#62670),(#62671,
#62672),(#62673,#62674),(#62675,#62676),(#62677,#62678),(#62679,#62680),
(#62681,#62682),(#62683,#62684),(#62685,#62686),(#62687,#62688),(#62689,
#62690),(#62691,#62692),(#62693,#62694),(#62695,#62696)),.UNSPECIFIED.,
 .F.,.F.,.F.)
B_SPLINE_SURFACE_WITH_KNOTS((6,1,1,1,1,1,1,1,1,1,1,1,1,1,1,1,1,1,1,1,1,
1,1,1,1,1,1,1,1,1,1,1,1,1,1,1,1,1,1,1,1,1,1,1,1,1,1,1,1,1,1,1,1,1,1,1,1,
1,1,1,1,1,1,1,1,6),(2,2),(-1.,-0.984615384615383,-0.969230769230768,-0.953846153846152,
-0.938461538461537,-0.923076923076922,-0.907692307692306,-0.892307692307691,
-0.876923076923076,-0.86153846153846,-0.846153846153845,-0.83076923076923,
-0.815384615384614,-0.799999999999999,-0.784615384615384,-0.769230769230768,
-0.753846153846153,-0.738461538461538,-0.723076923076922,-0.707692307692307,
-0.692307692307692,-0.676923076923076,-0.661538461538461,-0.646153846153846,
-0.63076923076923,-0.615384615384615,-0.6,-0.584615384615384,-0.569230769230769,
-0.553846153846154,-0.538461538461538,-0.523076923076923,-0.507692307692308,
-0.492307692307692,-0.476923076923077,-0.461538461538462,-0.446153846153846,
-0.430769230769231,-0.415384615384615,-0.4,-0.384615384615385,-0.369230769230769,
-0.353846153846154,-0.338461538461538,-0.323076923076923,-0.307692307692308,
-0.292307692307692,-0.276923076923077,-0.261538461538462,-0.246153846153846,
-0.230769230769231,-0.215384615384615,-0.2,-0.184615384615385,-0.169230769230769,
-0.153846153846154,-0.138461538461538,-0.123076923076923,-0.107692307692308,
-0.0923076923076923,-0.0769230769230769,-0.0615384615384615,-0.0461538461538462,
-0.0307692307692308,-0.0153846153846154,0.),(-1.,1.),.UNSPECIFIED.)
GEOMETRIC_REPRESENTATION_ITEM()
RATIONAL_B_SPLINE_SURFACE(((1.,1.),(1.,1.),(1.,1.),(1.,1.),(1.,1.),(1.,
1.),(1.,1.),(1.,1.),(1.,1.),(1.,1.),(1.,1.),(1.,1.),(1.,1.),(1.,1.),(1.,
1.),(1.,1.),(1.,1.),(1.,1.),(1.,1.),(1.,1.),(1.,1.),(1.,1.),(1.,1.),(1.,
1.),(1.,1.),(1.,1.),(1.,1.),(1.,1.),(1.,1.),(1.,1.),(1.,1.),(1.,1.),(1.,
1.),(1.,1.),(1.,1.),(1.,1.),(1.,1.),(1.,1.),(1.,1.),(1.,1.),(1.,1.),(1.,
1.),(1.,1.),(1.,1.),(1.,1.),(1.,1.),(1.,1.),(1.,1.),(1.,1.),(1.,1.),(1.,
1.),(1.,1.),(1.,1.),(1.,1.),(1.,1.),(1.,1.),(1.,1.),(1.,1.),(1.,1.),(1.,
1.),(1.,1.),(1.,1.),(1.,1.),(1.,1.),(1.,1.),(1.,1.),(1.,1.),(1.,1.),(1.,
1.),(1.,1.)))
REPRESENTATION_ITEM('')
SURFACE()
);
#124=(
BOUNDED_SURFACE()
B_SPLINE_SURFACE(5,1,((#62769,#62770),(#62771,#62772),(#62773,#62774),(#62775,
#62776),(#62777,#62778),(#62779,#62780),(#62781,#62782),(#62783,#62784),
(#62785,#62786),(#62787,#62788),(#62789,#62790),(#62791,#62792),(#62793,
#62794),(#62795,#62796),(#62797,#62798),(#62799,#62800),(#62801,#62802),
(#62803,#62804),(#62805,#62806),(#62807,#62808),(#62809,#62810),(#62811,
#62812),(#62813,#62814),(#62815,#62816),(#62817,#62818),(#62819,#62820),
(#62821,#62822),(#62823,#62824),(#62825,#62826),(#62827,#62828),(#62829,
#62830),(#62831,#62832),(#62833,#62834),(#62835,#62836),(#62837,#62838),
(#62839,#62840),(#62841,#62842),(#62843,#62844),(#62845,#62846),(#62847,
#62848),(#62849,#62850),(#62851,#62852),(#62853,#62854),(#62855,#62856),
(#62857,#62858),(#62859,#62860),(#62861,#62862),(#62863,#62864),(#62865,
#62866),(#62867,#62868),(#62869,#62870),(#62871,#62872),(#62873,#62874),
(#62875,#62876),(#62877,#62878),(#62879,#62880),(#62881,#62882),(#62883,
#62884),(#62885,#62886),(#62887,#62888),(#62889,#62890),(#62891,#62892),
(#62893,#62894),(#62895,#62896),(#62897,#62898),(#62899,#62900),(#62901,
#62902),(#62903,#62904),(#62905,#62906),(#62907,#62908)),.UNSPECIFIED.,
 .F.,.F.,.F.)
B_SPLINE_SURFACE_WITH_KNOTS((6,1,1,1,1,1,1,1,1,1,1,1,1,1,1,1,1,1,1,1,1,
1,1,1,1,1,1,1,1,1,1,1,1,1,1,1,1,1,1,1,1,1,1,1,1,1,1,1,1,1,1,1,1,1,1,1,1,
1,1,1,1,1,1,1,1,6),(2,2),(-1.,-0.984615384615383,-0.969230769230768,-0.953846153846152,
-0.938461538461537,-0.923076923076922,-0.907692307692306,-0.892307692307691,
-0.876923076923076,-0.86153846153846,-0.846153846153845,-0.83076923076923,
-0.815384615384614,-0.799999999999999,-0.784615384615384,-0.769230769230768,
-0.753846153846153,-0.738461538461538,-0.723076923076922,-0.707692307692307,
-0.692307692307692,-0.676923076923076,-0.661538461538461,-0.646153846153846,
-0.63076923076923,-0.615384615384615,-0.6,-0.584615384615384,-0.569230769230769,
-0.553846153846154,-0.538461538461538,-0.523076923076923,-0.507692307692308,
-0.492307692307692,-0.476923076923077,-0.461538461538462,-0.446153846153846,
-0.430769230769231,-0.415384615384615,-0.4,-0.384615384615385,-0.369230769230769,
-0.353846153846154,-0.338461538461538,-0.323076923076923,-0.307692307692308,
-0.292307692307692,-0.276923076923077,-0.261538461538462,-0.246153846153846,
-0.230769230769231,-0.215384615384615,-0.2,-0.184615384615385,-0.169230769230769,
-0.153846153846154,-0.138461538461538,-0.123076923076923,-0.107692307692308,
-0.0923076923076923,-0.0769230769230769,-0.0615384615384615,-0.0461538461538462,
-0.0307692307692308,-0.0153846153846154,0.),(-1.,1.),.UNSPECIFIED.)
GEOMETRIC_REPRESENTATION_ITEM()
RATIONAL_B_SPLINE_SURFACE(((1.,1.),(1.,1.),(1.,1.),(1.,1.),(1.,1.),(1.,
1.),(1.,1.),(1.,1.),(1.,1.),(1.,1.),(1.,1.),(1.,1.),(1.,1.),(1.,1.),(1.,
1.),(1.,1.),(1.,1.),(1.,1.),(1.,1.),(1.,1.),(1.,1.),(1.,1.),(1.,1.),(1.,
1.),(1.,1.),(1.,1.),(1.,1.),(1.,1.),(1.,1.),(1.,1.),(1.,1.),(1.,1.),(1.,
1.),(1.,1.),(1.,1.),(1.,1.),(1.,1.),(1.,1.),(1.,1.),(1.,1.),(1.,1.),(1.,
1.),(1.,1.),(1.,1.),(1.,1.),(1.,1.),(1.,1.),(1.,1.),(1.,1.),(1.,1.),(1.,
1.),(1.,1.),(1.,1.),(1.,1.),(1.,1.),(1.,1.),(1.,1.),(1.,1.),(1.,1.),(1.,
1.),(1.,1.),(1.,1.),(1.,1.),(1.,1.),(1.,1.),(1.,1.),(1.,1.),(1.,1.),(1.,
1.),(1.,1.)))
REPRESENTATION_ITEM('')
SURFACE()
);
#125=(
BOUNDED_SURFACE()
B_SPLINE_SURFACE(5,1,((#62999,#63000),(#63001,#63002),(#63003,#63004),(#63005,
#63006),(#63007,#63008),(#63009,#63010),(#63011,#63012),(#63013,#63014),
(#63015,#63016),(#63017,#63018),(#63019,#63020),(#63021,#63022),(#63023,
#63024),(#63025,#63026),(#63027,#63028),(#63029,#63030),(#63031,#63032),
(#63033,#63034),(#63035,#63036),(#63037,#63038),(#63039,#63040),(#63041,
#63042),(#63043,#63044),(#63045,#63046),(#63047,#63048),(#63049,#63050),
(#63051,#63052),(#63053,#63054),(#63055,#63056),(#63057,#63058),(#63059,
#63060),(#63061,#63062),(#63063,#63064),(#63065,#63066),(#63067,#63068),
(#63069,#63070),(#63071,#63072),(#63073,#63074),(#63075,#63076),(#63077,
#63078),(#63079,#63080),(#63081,#63082),(#63083,#63084),(#63085,#63086),
(#63087,#63088),(#63089,#63090),(#63091,#63092),(#63093,#63094),(#63095,
#63096),(#63097,#63098),(#63099,#63100),(#63101,#63102),(#63103,#63104),
(#63105,#63106),(#63107,#63108),(#63109,#63110),(#63111,#63112),(#63113,
#63114),(#63115,#63116),(#63117,#63118),(#63119,#63120),(#63121,#63122),
(#63123,#63124),(#63125,#63126),(#63127,#63128),(#63129,#63130),(#63131,
#63132),(#63133,#63134),(#63135,#63136),(#63137,#63138)),.UNSPECIFIED.,
 .F.,.F.,.F.)
B_SPLINE_SURFACE_WITH_KNOTS((6,1,1,1,1,1,1,1,1,1,1,1,1,1,1,1,1,1,1,1,1,
1,1,1,1,1,1,1,1,1,1,1,1,1,1,1,1,1,1,1,1,1,1,1,1,1,1,1,1,1,1,1,1,1,1,1,1,
1,1,1,1,1,1,1,1,6),(2,2),(-1.,-0.984615384615383,-0.969230769230768,-0.953846153846152,
-0.938461538461537,-0.923076923076922,-0.907692307692306,-0.892307692307691,
-0.876923076923076,-0.86153846153846,-0.846153846153845,-0.83076923076923,
-0.815384615384614,-0.799999999999999,-0.784615384615384,-0.769230769230768,
-0.753846153846153,-0.738461538461538,-0.723076923076922,-0.707692307692307,
-0.692307692307692,-0.676923076923076,-0.661538461538461,-0.646153846153846,
-0.63076923076923,-0.615384615384615,-0.6,-0.584615384615384,-0.569230769230769,
-0.553846153846154,-0.538461538461538,-0.523076923076923,-0.507692307692308,
-0.492307692307692,-0.476923076923077,-0.461538461538462,-0.446153846153846,
-0.430769230769231,-0.415384615384615,-0.4,-0.384615384615385,-0.369230769230769,
-0.353846153846154,-0.338461538461538,-0.323076923076923,-0.307692307692308,
-0.292307692307692,-0.276923076923077,-0.261538461538462,-0.246153846153846,
-0.230769230769231,-0.215384615384615,-0.2,-0.184615384615385,-0.169230769230769,
-0.153846153846154,-0.138461538461538,-0.123076923076923,-0.107692307692308,
-0.0923076923076923,-0.0769230769230769,-0.0615384615384615,-0.0461538461538462,
-0.0307692307692308,-0.0153846153846154,0.),(-1.,1.),.UNSPECIFIED.)
GEOMETRIC_REPRESENTATION_ITEM()
RATIONAL_B_SPLINE_SURFACE(((1.,1.),(1.,1.),(1.,1.),(1.,1.),(1.,1.),(1.,
1.),(1.,1.),(1.,1.),(1.,1.),(1.,1.),(1.,1.),(1.,1.),(1.,1.),(1.,1.),(1.,
1.),(1.,1.),(1.,1.),(1.,1.),(1.,1.),(1.,1.),(1.,1.),(1.,1.),(1.,1.),(1.,
1.),(1.,1.),(1.,1.),(1.,1.),(1.,1.),(1.,1.),(1.,1.),(1.,1.),(1.,1.),(1.,
1.),(1.,1.),(1.,1.),(1.,1.),(1.,1.),(1.,1.),(1.,1.),(1.,1.),(1.,1.),(1.,
1.),(1.,1.),(1.,1.),(1.,1.),(1.,1.),(1.,1.),(1.,1.),(1.,1.),(1.,1.),(1.,
1.),(1.,1.),(1.,1.),(1.,1.),(1.,1.),(1.,1.),(1.,1.),(1.,1.),(1.,1.),(1.,
1.),(1.,1.),(1.,1.),(1.,1.),(1.,1.),(1.,1.),(1.,1.),(1.,1.),(1.,1.),(1.,
1.),(1.,1.)))
REPRESENTATION_ITEM('')
SURFACE()
);
#126=(
BOUNDED_SURFACE()
B_SPLINE_SURFACE(5,1,((#63211,#63212),(#63213,#63214),(#63215,#63216),(#63217,
#63218),(#63219,#63220),(#63221,#63222),(#63223,#63224),(#63225,#63226),
(#63227,#63228),(#63229,#63230),(#63231,#63232),(#63233,#63234),(#63235,
#63236),(#63237,#63238),(#63239,#63240),(#63241,#63242),(#63243,#63244),
(#63245,#63246),(#63247,#63248),(#63249,#63250),(#63251,#63252),(#63253,
#63254),(#63255,#63256),(#63257,#63258),(#63259,#63260),(#63261,#63262),
(#63263,#63264),(#63265,#63266),(#63267,#63268),(#63269,#63270),(#63271,
#63272),(#63273,#63274),(#63275,#63276),(#63277,#63278),(#63279,#63280),
(#63281,#63282),(#63283,#63284),(#63285,#63286),(#63287,#63288),(#63289,
#63290),(#63291,#63292),(#63293,#63294),(#63295,#63296),(#63297,#63298),
(#63299,#63300),(#63301,#63302),(#63303,#63304),(#63305,#63306),(#63307,
#63308),(#63309,#63310),(#63311,#63312),(#63313,#63314),(#63315,#63316),
(#63317,#63318),(#63319,#63320),(#63321,#63322),(#63323,#63324),(#63325,
#63326),(#63327,#63328),(#63329,#63330),(#63331,#63332),(#63333,#63334),
(#63335,#63336),(#63337,#63338),(#63339,#63340),(#63341,#63342),(#63343,
#63344),(#63345,#63346),(#63347,#63348),(#63349,#63350)),.UNSPECIFIED.,
 .F.,.F.,.F.)
B_SPLINE_SURFACE_WITH_KNOTS((6,1,1,1,1,1,1,1,1,1,1,1,1,1,1,1,1,1,1,1,1,
1,1,1,1,1,1,1,1,1,1,1,1,1,1,1,1,1,1,1,1,1,1,1,1,1,1,1,1,1,1,1,1,1,1,1,1,
1,1,1,1,1,1,1,1,6),(2,2),(-1.,-0.984615384615383,-0.969230769230768,-0.953846153846152,
-0.938461538461537,-0.923076923076922,-0.907692307692306,-0.892307692307691,
-0.876923076923076,-0.86153846153846,-0.846153846153845,-0.83076923076923,
-0.815384615384614,-0.799999999999999,-0.784615384615384,-0.769230769230768,
-0.753846153846153,-0.738461538461538,-0.723076923076922,-0.707692307692307,
-0.692307692307692,-0.676923076923076,-0.661538461538461,-0.646153846153846,
-0.63076923076923,-0.615384615384615,-0.6,-0.584615384615384,-0.569230769230769,
-0.553846153846154,-0.538461538461538,-0.523076923076923,-0.507692307692308,
-0.492307692307692,-0.476923076923077,-0.461538461538462,-0.446153846153846,
-0.430769230769231,-0.415384615384615,-0.4,-0.384615384615385,-0.369230769230769,
-0.353846153846154,-0.338461538461538,-0.323076923076923,-0.307692307692308,
-0.292307692307692,-0.276923076923077,-0.261538461538462,-0.246153846153846,
-0.230769230769231,-0.215384615384615,-0.2,-0.184615384615385,-0.169230769230769,
-0.153846153846154,-0.138461538461538,-0.123076923076923,-0.107692307692308,
-0.0923076923076923,-0.0769230769230769,-0.0615384615384615,-0.0461538461538462,
-0.0307692307692308,-0.0153846153846154,0.),(-1.,1.),.UNSPECIFIED.)
GEOMETRIC_REPRESENTATION_ITEM()
RATIONAL_B_SPLINE_SURFACE(((1.,1.),(1.,1.),(1.,1.),(1.,1.),(1.,1.),(1.,
1.),(1.,1.),(1.,1.),(1.,1.),(1.,1.),(1.,1.),(1.,1.),(1.,1.),(1.,1.),(1.,
1.),(1.,1.),(1.,1.),(1.,1.),(1.,1.),(1.,1.),(1.,1.),(1.,1.),(1.,1.),(1.,
1.),(1.,1.),(1.,1.),(1.,1.),(1.,1.),(1.,1.),(1.,1.),(1.,1.),(1.,1.),(1.,
1.),(1.,1.),(1.,1.),(1.,1.),(1.,1.),(1.,1.),(1.,1.),(1.,1.),(1.,1.),(1.,
1.),(1.,1.),(1.,1.),(1.,1.),(1.,1.),(1.,1.),(1.,1.),(1.,1.),(1.,1.),(1.,
1.),(1.,1.),(1.,1.),(1.,1.),(1.,1.),(1.,1.),(1.,1.),(1.,1.),(1.,1.),(1.,
1.),(1.,1.),(1.,1.),(1.,1.),(1.,1.),(1.,1.),(1.,1.),(1.,1.),(1.,1.),(1.,
1.),(1.,1.)))
REPRESENTATION_ITEM('')
SURFACE()
);
#127=(
BOUNDED_SURFACE()
B_SPLINE_SURFACE(5,1,((#63441,#63442),(#63443,#63444),(#63445,#63446),(#63447,
#63448),(#63449,#63450),(#63451,#63452),(#63453,#63454),(#63455,#63456),
(#63457,#63458),(#63459,#63460),(#63461,#63462),(#63463,#63464),(#63465,
#63466),(#63467,#63468),(#63469,#63470),(#63471,#63472),(#63473,#63474),
(#63475,#63476),(#63477,#63478),(#63479,#63480),(#63481,#63482),(#63483,
#63484),(#63485,#63486),(#63487,#63488),(#63489,#63490),(#63491,#63492),
(#63493,#63494),(#63495,#63496),(#63497,#63498),(#63499,#63500),(#63501,
#63502),(#63503,#63504),(#63505,#63506),(#63507,#63508),(#63509,#63510),
(#63511,#63512),(#63513,#63514),(#63515,#63516),(#63517,#63518),(#63519,
#63520),(#63521,#63522),(#63523,#63524),(#63525,#63526),(#63527,#63528),
(#63529,#63530),(#63531,#63532),(#63533,#63534),(#63535,#63536),(#63537,
#63538),(#63539,#63540),(#63541,#63542),(#63543,#63544),(#63545,#63546),
(#63547,#63548),(#63549,#63550),(#63551,#63552),(#63553,#63554),(#63555,
#63556),(#63557,#63558),(#63559,#63560),(#63561,#63562),(#63563,#63564),
(#63565,#63566),(#63567,#63568),(#63569,#63570),(#63571,#63572),(#63573,
#63574),(#63575,#63576),(#63577,#63578),(#63579,#63580)),.UNSPECIFIED.,
 .F.,.F.,.F.)
B_SPLINE_SURFACE_WITH_KNOTS((6,1,1,1,1,1,1,1,1,1,1,1,1,1,1,1,1,1,1,1,1,
1,1,1,1,1,1,1,1,1,1,1,1,1,1,1,1,1,1,1,1,1,1,1,1,1,1,1,1,1,1,1,1,1,1,1,1,
1,1,1,1,1,1,1,1,6),(2,2),(-1.,-0.984615384615383,-0.969230769230768,-0.953846153846152,
-0.938461538461537,-0.923076923076922,-0.907692307692306,-0.892307692307691,
-0.876923076923076,-0.86153846153846,-0.846153846153845,-0.83076923076923,
-0.815384615384614,-0.799999999999999,-0.784615384615384,-0.769230769230768,
-0.753846153846153,-0.738461538461538,-0.723076923076922,-0.707692307692307,
-0.692307692307692,-0.676923076923076,-0.661538461538461,-0.646153846153846,
-0.63076923076923,-0.615384615384615,-0.6,-0.584615384615384,-0.569230769230769,
-0.553846153846154,-0.538461538461538,-0.523076923076923,-0.507692307692308,
-0.492307692307692,-0.476923076923077,-0.461538461538462,-0.446153846153846,
-0.430769230769231,-0.415384615384615,-0.4,-0.384615384615385,-0.369230769230769,
-0.353846153846154,-0.338461538461538,-0.323076923076923,-0.307692307692308,
-0.292307692307692,-0.276923076923077,-0.261538461538462,-0.246153846153846,
-0.230769230769231,-0.215384615384615,-0.2,-0.184615384615385,-0.169230769230769,
-0.153846153846154,-0.138461538461538,-0.123076923076923,-0.107692307692308,
-0.0923076923076923,-0.0769230769230769,-0.0615384615384615,-0.0461538461538462,
-0.0307692307692308,-0.0153846153846154,0.),(-1.,1.),.UNSPECIFIED.)
GEOMETRIC_REPRESENTATION_ITEM()
RATIONAL_B_SPLINE_SURFACE(((1.,1.),(1.,1.),(1.,1.),(1.,1.),(1.,1.),(1.,
1.),(1.,1.),(1.,1.),(1.,1.),(1.,1.),(1.,1.),(1.,1.),(1.,1.),(1.,1.),(1.,
1.),(1.,1.),(1.,1.),(1.,1.),(1.,1.),(1.,1.),(1.,1.),(1.,1.),(1.,1.),(1.,
1.),(1.,1.),(1.,1.),(1.,1.),(1.,1.),(1.,1.),(1.,1.),(1.,1.),(1.,1.),(1.,
1.),(1.,1.),(1.,1.),(1.,1.),(1.,1.),(1.,1.),(1.,1.),(1.,1.),(1.,1.),(1.,
1.),(1.,1.),(1.,1.),(1.,1.),(1.,1.),(1.,1.),(1.,1.),(1.,1.),(1.,1.),(1.,
1.),(1.,1.),(1.,1.),(1.,1.),(1.,1.),(1.,1.),(1.,1.),(1.,1.),(1.,1.),(1.,
1.),(1.,1.),(1.,1.),(1.,1.),(1.,1.),(1.,1.),(1.,1.),(1.,1.),(1.,1.),(1.,
1.),(1.,1.)))
REPRESENTATION_ITEM('')
SURFACE()
);
#128=(
BOUNDED_SURFACE()
B_SPLINE_SURFACE(5,1,((#63653,#63654),(#63655,#63656),(#63657,#63658),(#63659,
#63660),(#63661,#63662),(#63663,#63664),(#63665,#63666),(#63667,#63668),
(#63669,#63670),(#63671,#63672),(#63673,#63674),(#63675,#63676),(#63677,
#63678),(#63679,#63680),(#63681,#63682),(#63683,#63684),(#63685,#63686),
(#63687,#63688),(#63689,#63690),(#63691,#63692),(#63693,#63694),(#63695,
#63696),(#63697,#63698),(#63699,#63700),(#63701,#63702),(#63703,#63704),
(#63705,#63706),(#63707,#63708),(#63709,#63710),(#63711,#63712),(#63713,
#63714),(#63715,#63716),(#63717,#63718),(#63719,#63720),(#63721,#63722),
(#63723,#63724),(#63725,#63726),(#63727,#63728),(#63729,#63730),(#63731,
#63732),(#63733,#63734),(#63735,#63736),(#63737,#63738),(#63739,#63740),
(#63741,#63742),(#63743,#63744),(#63745,#63746),(#63747,#63748),(#63749,
#63750),(#63751,#63752),(#63753,#63754),(#63755,#63756),(#63757,#63758),
(#63759,#63760),(#63761,#63762),(#63763,#63764),(#63765,#63766),(#63767,
#63768),(#63769,#63770),(#63771,#63772),(#63773,#63774),(#63775,#63776),
(#63777,#63778),(#63779,#63780),(#63781,#63782),(#63783,#63784),(#63785,
#63786),(#63787,#63788),(#63789,#63790),(#63791,#63792)),.UNSPECIFIED.,
 .F.,.F.,.F.)
B_SPLINE_SURFACE_WITH_KNOTS((6,1,1,1,1,1,1,1,1,1,1,1,1,1,1,1,1,1,1,1,1,
1,1,1,1,1,1,1,1,1,1,1,1,1,1,1,1,1,1,1,1,1,1,1,1,1,1,1,1,1,1,1,1,1,1,1,1,
1,1,1,1,1,1,1,1,6),(2,2),(-1.,-0.984615384615383,-0.969230769230768,-0.953846153846152,
-0.938461538461537,-0.923076923076922,-0.907692307692306,-0.892307692307691,
-0.876923076923076,-0.86153846153846,-0.846153846153845,-0.83076923076923,
-0.815384615384614,-0.799999999999999,-0.784615384615384,-0.769230769230768,
-0.753846153846153,-0.738461538461538,-0.723076923076922,-0.707692307692307,
-0.692307692307692,-0.676923076923076,-0.661538461538461,-0.646153846153846,
-0.63076923076923,-0.615384615384615,-0.6,-0.584615384615384,-0.569230769230769,
-0.553846153846154,-0.538461538461538,-0.523076923076923,-0.507692307692308,
-0.492307692307692,-0.476923076923077,-0.461538461538462,-0.446153846153846,
-0.430769230769231,-0.415384615384615,-0.4,-0.384615384615385,-0.369230769230769,
-0.353846153846154,-0.338461538461538,-0.323076923076923,-0.307692307692308,
-0.292307692307692,-0.276923076923077,-0.261538461538462,-0.246153846153846,
-0.230769230769231,-0.215384615384615,-0.2,-0.184615384615385,-0.169230769230769,
-0.153846153846154,-0.138461538461538,-0.123076923076923,-0.107692307692308,
-0.0923076923076923,-0.0769230769230769,-0.0615384615384615,-0.0461538461538462,
-0.0307692307692308,-0.0153846153846154,0.),(-1.,1.),.UNSPECIFIED.)
GEOMETRIC_REPRESENTATION_ITEM()
RATIONAL_B_SPLINE_SURFACE(((1.,1.),(1.,1.),(1.,1.),(1.,1.),(1.,1.),(1.,
1.),(1.,1.),(1.,1.),(1.,1.),(1.,1.),(1.,1.),(1.,1.),(1.,1.),(1.,1.),(1.,
1.),(1.,1.),(1.,1.),(1.,1.),(1.,1.),(1.,1.),(1.,1.),(1.,1.),(1.,1.),(1.,
1.),(1.,1.),(1.,1.),(1.,1.),(1.,1.),(1.,1.),(1.,1.),(1.,1.),(1.,1.),(1.,
1.),(1.,1.),(1.,1.),(1.,1.),(1.,1.),(1.,1.),(1.,1.),(1.,1.),(1.,1.),(1.,
1.),(1.,1.),(1.,1.),(1.,1.),(1.,1.),(1.,1.),(1.,1.),(1.,1.),(1.,1.),(1.,
1.),(1.,1.),(1.,1.),(1.,1.),(1.,1.),(1.,1.),(1.,1.),(1.,1.),(1.,1.),(1.,
1.),(1.,1.),(1.,1.),(1.,1.),(1.,1.),(1.,1.),(1.,1.),(1.,1.),(1.,1.),(1.,
1.),(1.,1.)))
REPRESENTATION_ITEM('')
SURFACE()
);
#129=(
BOUNDED_SURFACE()
B_SPLINE_SURFACE(5,1,((#63883,#63884),(#63885,#63886),(#63887,#63888),(#63889,
#63890),(#63891,#63892),(#63893,#63894),(#63895,#63896),(#63897,#63898),
(#63899,#63900),(#63901,#63902),(#63903,#63904),(#63905,#63906),(#63907,
#63908),(#63909,#63910),(#63911,#63912),(#63913,#63914),(#63915,#63916),
(#63917,#63918),(#63919,#63920),(#63921,#63922),(#63923,#63924),(#63925,
#63926),(#63927,#63928),(#63929,#63930),(#63931,#63932),(#63933,#63934),
(#63935,#63936),(#63937,#63938),(#63939,#63940),(#63941,#63942),(#63943,
#63944),(#63945,#63946),(#63947,#63948),(#63949,#63950),(#63951,#63952),
(#63953,#63954),(#63955,#63956),(#63957,#63958),(#63959,#63960),(#63961,
#63962),(#63963,#63964),(#63965,#63966),(#63967,#63968),(#63969,#63970),
(#63971,#63972),(#63973,#63974),(#63975,#63976),(#63977,#63978),(#63979,
#63980),(#63981,#63982),(#63983,#63984),(#63985,#63986),(#63987,#63988),
(#63989,#63990),(#63991,#63992),(#63993,#63994),(#63995,#63996),(#63997,
#63998),(#63999,#64000),(#64001,#64002),(#64003,#64004),(#64005,#64006),
(#64007,#64008),(#64009,#64010),(#64011,#64012),(#64013,#64014),(#64015,
#64016),(#64017,#64018),(#64019,#64020),(#64021,#64022)),.UNSPECIFIED.,
 .F.,.F.,.F.)
B_SPLINE_SURFACE_WITH_KNOTS((6,1,1,1,1,1,1,1,1,1,1,1,1,1,1,1,1,1,1,1,1,
1,1,1,1,1,1,1,1,1,1,1,1,1,1,1,1,1,1,1,1,1,1,1,1,1,1,1,1,1,1,1,1,1,1,1,1,
1,1,1,1,1,1,1,1,6),(2,2),(-1.,-0.984615384615383,-0.969230769230768,-0.953846153846152,
-0.938461538461537,-0.923076923076922,-0.907692307692306,-0.892307692307691,
-0.876923076923076,-0.86153846153846,-0.846153846153845,-0.83076923076923,
-0.815384615384614,-0.799999999999999,-0.784615384615384,-0.769230769230768,
-0.753846153846153,-0.738461538461538,-0.723076923076922,-0.707692307692307,
-0.692307692307692,-0.676923076923076,-0.661538461538461,-0.646153846153846,
-0.63076923076923,-0.615384615384615,-0.6,-0.584615384615384,-0.569230769230769,
-0.553846153846154,-0.538461538461538,-0.523076923076923,-0.507692307692308,
-0.492307692307692,-0.476923076923077,-0.461538461538462,-0.446153846153846,
-0.430769230769231,-0.415384615384615,-0.4,-0.384615384615385,-0.369230769230769,
-0.353846153846154,-0.338461538461538,-0.323076923076923,-0.307692307692308,
-0.292307692307692,-0.276923076923077,-0.261538461538462,-0.246153846153846,
-0.230769230769231,-0.215384615384615,-0.2,-0.184615384615385,-0.169230769230769,
-0.153846153846154,-0.138461538461538,-0.123076923076923,-0.107692307692308,
-0.0923076923076923,-0.0769230769230769,-0.0615384615384615,-0.0461538461538462,
-0.0307692307692308,-0.0153846153846154,0.),(-1.,1.),.UNSPECIFIED.)
GEOMETRIC_REPRESENTATION_ITEM()
RATIONAL_B_SPLINE_SURFACE(((1.,1.),(1.,1.),(1.,1.),(1.,1.),(1.,1.),(1.,
1.),(1.,1.),(1.,1.),(1.,1.),(1.,1.),(1.,1.),(1.,1.),(1.,1.),(1.,1.),(1.,
1.),(1.,1.),(1.,1.),(1.,1.),(1.,1.),(1.,1.),(1.,1.),(1.,1.),(1.,1.),(1.,
1.),(1.,1.),(1.,1.),(1.,1.),(1.,1.),(1.,1.),(1.,1.),(1.,1.),(1.,1.),(1.,
1.),(1.,1.),(1.,1.),(1.,1.),(1.,1.),(1.,1.),(1.,1.),(1.,1.),(1.,1.),(1.,
1.),(1.,1.),(1.,1.),(1.,1.),(1.,1.),(1.,1.),(1.,1.),(1.,1.),(1.,1.),(1.,
1.),(1.,1.),(1.,1.),(1.,1.),(1.,1.),(1.,1.),(1.,1.),(1.,1.),(1.,1.),(1.,
1.),(1.,1.),(1.,1.),(1.,1.),(1.,1.),(1.,1.),(1.,1.),(1.,1.),(1.,1.),(1.,
1.),(1.,1.)))
REPRESENTATION_ITEM('')
SURFACE()
);
#130=(
BOUNDED_SURFACE()
B_SPLINE_SURFACE(5,1,((#64095,#64096),(#64097,#64098),(#64099,#64100),(#64101,
#64102),(#64103,#64104),(#64105,#64106),(#64107,#64108),(#64109,#64110),
(#64111,#64112),(#64113,#64114),(#64115,#64116),(#64117,#64118),(#64119,
#64120),(#64121,#64122),(#64123,#64124),(#64125,#64126),(#64127,#64128),
(#64129,#64130),(#64131,#64132),(#64133,#64134),(#64135,#64136),(#64137,
#64138),(#64139,#64140),(#64141,#64142),(#64143,#64144),(#64145,#64146),
(#64147,#64148),(#64149,#64150),(#64151,#64152),(#64153,#64154),(#64155,
#64156),(#64157,#64158),(#64159,#64160),(#64161,#64162),(#64163,#64164),
(#64165,#64166),(#64167,#64168),(#64169,#64170),(#64171,#64172),(#64173,
#64174),(#64175,#64176),(#64177,#64178),(#64179,#64180),(#64181,#64182),
(#64183,#64184),(#64185,#64186),(#64187,#64188),(#64189,#64190),(#64191,
#64192),(#64193,#64194),(#64195,#64196),(#64197,#64198),(#64199,#64200),
(#64201,#64202),(#64203,#64204),(#64205,#64206),(#64207,#64208),(#64209,
#64210),(#64211,#64212),(#64213,#64214),(#64215,#64216),(#64217,#64218),
(#64219,#64220),(#64221,#64222),(#64223,#64224),(#64225,#64226),(#64227,
#64228),(#64229,#64230),(#64231,#64232),(#64233,#64234)),.UNSPECIFIED.,
 .F.,.F.,.F.)
B_SPLINE_SURFACE_WITH_KNOTS((6,1,1,1,1,1,1,1,1,1,1,1,1,1,1,1,1,1,1,1,1,
1,1,1,1,1,1,1,1,1,1,1,1,1,1,1,1,1,1,1,1,1,1,1,1,1,1,1,1,1,1,1,1,1,1,1,1,
1,1,1,1,1,1,1,1,6),(2,2),(-1.,-0.984615384615383,-0.969230769230768,-0.953846153846152,
-0.938461538461537,-0.923076923076922,-0.907692307692306,-0.892307692307691,
-0.876923076923076,-0.86153846153846,-0.846153846153845,-0.83076923076923,
-0.815384615384614,-0.799999999999999,-0.784615384615384,-0.769230769230768,
-0.753846153846153,-0.738461538461538,-0.723076923076922,-0.707692307692307,
-0.692307692307692,-0.676923076923076,-0.661538461538461,-0.646153846153846,
-0.63076923076923,-0.615384615384615,-0.6,-0.584615384615384,-0.569230769230769,
-0.553846153846154,-0.538461538461538,-0.523076923076923,-0.507692307692308,
-0.492307692307692,-0.476923076923077,-0.461538461538462,-0.446153846153846,
-0.430769230769231,-0.415384615384615,-0.4,-0.384615384615385,-0.369230769230769,
-0.353846153846154,-0.338461538461538,-0.323076923076923,-0.307692307692308,
-0.292307692307692,-0.276923076923077,-0.261538461538462,-0.246153846153846,
-0.230769230769231,-0.215384615384615,-0.2,-0.184615384615385,-0.169230769230769,
-0.153846153846154,-0.138461538461538,-0.123076923076923,-0.107692307692308,
-0.0923076923076923,-0.0769230769230769,-0.0615384615384615,-0.0461538461538462,
-0.0307692307692308,-0.0153846153846154,0.),(-1.,1.),.UNSPECIFIED.)
GEOMETRIC_REPRESENTATION_ITEM()
RATIONAL_B_SPLINE_SURFACE(((1.,1.),(1.,1.),(1.,1.),(1.,1.),(1.,1.),(1.,
1.),(1.,1.),(1.,1.),(1.,1.),(1.,1.),(1.,1.),(1.,1.),(1.,1.),(1.,1.),(1.,
1.),(1.,1.),(1.,1.),(1.,1.),(1.,1.),(1.,1.),(1.,1.),(1.,1.),(1.,1.),(1.,
1.),(1.,1.),(1.,1.),(1.,1.),(1.,1.),(1.,1.),(1.,1.),(1.,1.),(1.,1.),(1.,
1.),(1.,1.),(1.,1.),(1.,1.),(1.,1.),(1.,1.),(1.,1.),(1.,1.),(1.,1.),(1.,
1.),(1.,1.),(1.,1.),(1.,1.),(1.,1.),(1.,1.),(1.,1.),(1.,1.),(1.,1.),(1.,
1.),(1.,1.),(1.,1.),(1.,1.),(1.,1.),(1.,1.),(1.,1.),(1.,1.),(1.,1.),(1.,
1.),(1.,1.),(1.,1.),(1.,1.),(1.,1.),(1.,1.),(1.,1.),(1.,1.),(1.,1.),(1.,
1.),(1.,1.)))
REPRESENTATION_ITEM('')
SURFACE()
);
#131=(
BOUNDED_SURFACE()
B_SPLINE_SURFACE(5,1,((#64325,#64326),(#64327,#64328),(#64329,#64330),(#64331,
#64332),(#64333,#64334),(#64335,#64336),(#64337,#64338),(#64339,#64340),
(#64341,#64342),(#64343,#64344),(#64345,#64346),(#64347,#64348),(#64349,
#64350),(#64351,#64352),(#64353,#64354),(#64355,#64356),(#64357,#64358),
(#64359,#64360),(#64361,#64362),(#64363,#64364),(#64365,#64366),(#64367,
#64368),(#64369,#64370),(#64371,#64372),(#64373,#64374),(#64375,#64376),
(#64377,#64378),(#64379,#64380),(#64381,#64382),(#64383,#64384),(#64385,
#64386),(#64387,#64388),(#64389,#64390),(#64391,#64392),(#64393,#64394),
(#64395,#64396),(#64397,#64398),(#64399,#64400),(#64401,#64402),(#64403,
#64404),(#64405,#64406),(#64407,#64408),(#64409,#64410),(#64411,#64412),
(#64413,#64414),(#64415,#64416),(#64417,#64418),(#64419,#64420),(#64421,
#64422),(#64423,#64424),(#64425,#64426),(#64427,#64428),(#64429,#64430),
(#64431,#64432),(#64433,#64434),(#64435,#64436),(#64437,#64438),(#64439,
#64440),(#64441,#64442),(#64443,#64444),(#64445,#64446),(#64447,#64448),
(#64449,#64450),(#64451,#64452),(#64453,#64454),(#64455,#64456),(#64457,
#64458),(#64459,#64460),(#64461,#64462),(#64463,#64464)),.UNSPECIFIED.,
 .F.,.F.,.F.)
B_SPLINE_SURFACE_WITH_KNOTS((6,1,1,1,1,1,1,1,1,1,1,1,1,1,1,1,1,1,1,1,1,
1,1,1,1,1,1,1,1,1,1,1,1,1,1,1,1,1,1,1,1,1,1,1,1,1,1,1,1,1,1,1,1,1,1,1,1,
1,1,1,1,1,1,1,1,6),(2,2),(-1.,-0.984615384615383,-0.969230769230768,-0.953846153846152,
-0.938461538461537,-0.923076923076922,-0.907692307692306,-0.892307692307691,
-0.876923076923076,-0.86153846153846,-0.846153846153845,-0.83076923076923,
-0.815384615384614,-0.799999999999999,-0.784615384615384,-0.769230769230768,
-0.753846153846153,-0.738461538461538,-0.723076923076922,-0.707692307692307,
-0.692307692307692,-0.676923076923076,-0.661538461538461,-0.646153846153846,
-0.63076923076923,-0.615384615384615,-0.6,-0.584615384615384,-0.569230769230769,
-0.553846153846154,-0.538461538461538,-0.523076923076923,-0.507692307692308,
-0.492307692307692,-0.476923076923077,-0.461538461538462,-0.446153846153846,
-0.430769230769231,-0.415384615384615,-0.4,-0.384615384615385,-0.369230769230769,
-0.353846153846154,-0.338461538461538,-0.323076923076923,-0.307692307692308,
-0.292307692307692,-0.276923076923077,-0.261538461538462,-0.246153846153846,
-0.230769230769231,-0.215384615384615,-0.2,-0.184615384615385,-0.169230769230769,
-0.153846153846154,-0.138461538461538,-0.123076923076923,-0.107692307692308,
-0.0923076923076923,-0.0769230769230769,-0.0615384615384615,-0.0461538461538462,
-0.0307692307692308,-0.0153846153846154,0.),(-1.,1.),.UNSPECIFIED.)
GEOMETRIC_REPRESENTATION_ITEM()
RATIONAL_B_SPLINE_SURFACE(((1.,1.),(1.,1.),(1.,1.),(1.,1.),(1.,1.),(1.,
1.),(1.,1.),(1.,1.),(1.,1.),(1.,1.),(1.,1.),(1.,1.),(1.,1.),(1.,1.),(1.,
1.),(1.,1.),(1.,1.),(1.,1.),(1.,1.),(1.,1.),(1.,1.),(1.,1.),(1.,1.),(1.,
1.),(1.,1.),(1.,1.),(1.,1.),(1.,1.),(1.,1.),(1.,1.),(1.,1.),(1.,1.),(1.,
1.),(1.,1.),(1.,1.),(1.,1.),(1.,1.),(1.,1.),(1.,1.),(1.,1.),(1.,1.),(1.,
1.),(1.,1.),(1.,1.),(1.,1.),(1.,1.),(1.,1.),(1.,1.),(1.,1.),(1.,1.),(1.,
1.),(1.,1.),(1.,1.),(1.,1.),(1.,1.),(1.,1.),(1.,1.),(1.,1.),(1.,1.),(1.,
1.),(1.,1.),(1.,1.),(1.,1.),(1.,1.),(1.,1.),(1.,1.),(1.,1.),(1.,1.),(1.,
1.),(1.,1.)))
REPRESENTATION_ITEM('')
SURFACE()
);
#132=(
BOUNDED_SURFACE()
B_SPLINE_SURFACE(5,1,((#64537,#64538),(#64539,#64540),(#64541,#64542),(#64543,
#64544),(#64545,#64546),(#64547,#64548),(#64549,#64550),(#64551,#64552),
(#64553,#64554),(#64555,#64556),(#64557,#64558),(#64559,#64560),(#64561,
#64562),(#64563,#64564),(#64565,#64566),(#64567,#64568),(#64569,#64570),
(#64571,#64572),(#64573,#64574),(#64575,#64576),(#64577,#64578),(#64579,
#64580),(#64581,#64582),(#64583,#64584),(#64585,#64586),(#64587,#64588),
(#64589,#64590),(#64591,#64592),(#64593,#64594),(#64595,#64596),(#64597,
#64598),(#64599,#64600),(#64601,#64602),(#64603,#64604),(#64605,#64606),
(#64607,#64608),(#64609,#64610),(#64611,#64612),(#64613,#64614),(#64615,
#64616),(#64617,#64618),(#64619,#64620),(#64621,#64622),(#64623,#64624),
(#64625,#64626),(#64627,#64628),(#64629,#64630),(#64631,#64632),(#64633,
#64634),(#64635,#64636),(#64637,#64638),(#64639,#64640),(#64641,#64642),
(#64643,#64644),(#64645,#64646),(#64647,#64648),(#64649,#64650),(#64651,
#64652),(#64653,#64654),(#64655,#64656),(#64657,#64658),(#64659,#64660),
(#64661,#64662),(#64663,#64664),(#64665,#64666),(#64667,#64668),(#64669,
#64670),(#64671,#64672),(#64673,#64674),(#64675,#64676)),.UNSPECIFIED.,
 .F.,.F.,.F.)
B_SPLINE_SURFACE_WITH_KNOTS((6,1,1,1,1,1,1,1,1,1,1,1,1,1,1,1,1,1,1,1,1,
1,1,1,1,1,1,1,1,1,1,1,1,1,1,1,1,1,1,1,1,1,1,1,1,1,1,1,1,1,1,1,1,1,1,1,1,
1,1,1,1,1,1,1,1,6),(2,2),(-1.,-0.984615384615383,-0.969230769230768,-0.953846153846152,
-0.938461538461537,-0.923076923076922,-0.907692307692306,-0.892307692307691,
-0.876923076923076,-0.86153846153846,-0.846153846153845,-0.83076923076923,
-0.815384615384614,-0.799999999999999,-0.784615384615384,-0.769230769230768,
-0.753846153846153,-0.738461538461538,-0.723076923076922,-0.707692307692307,
-0.692307692307692,-0.676923076923076,-0.661538461538461,-0.646153846153846,
-0.63076923076923,-0.615384615384615,-0.6,-0.584615384615384,-0.569230769230769,
-0.553846153846154,-0.538461538461538,-0.523076923076923,-0.507692307692308,
-0.492307692307692,-0.476923076923077,-0.461538461538462,-0.446153846153846,
-0.430769230769231,-0.415384615384615,-0.4,-0.384615384615385,-0.369230769230769,
-0.353846153846154,-0.338461538461538,-0.323076923076923,-0.307692307692308,
-0.292307692307692,-0.276923076923077,-0.261538461538462,-0.246153846153846,
-0.230769230769231,-0.215384615384615,-0.2,-0.184615384615385,-0.169230769230769,
-0.153846153846154,-0.138461538461538,-0.123076923076923,-0.107692307692308,
-0.0923076923076923,-0.0769230769230769,-0.0615384615384615,-0.0461538461538462,
-0.0307692307692308,-0.0153846153846154,0.),(-1.,1.),.UNSPECIFIED.)
GEOMETRIC_REPRESENTATION_ITEM()
RATIONAL_B_SPLINE_SURFACE(((1.,1.),(1.,1.),(1.,1.),(1.,1.),(1.,1.),(1.,
1.),(1.,1.),(1.,1.),(1.,1.),(1.,1.),(1.,1.),(1.,1.),(1.,1.),(1.,1.),(1.,
1.),(1.,1.),(1.,1.),(1.,1.),(1.,1.),(1.,1.),(1.,1.),(1.,1.),(1.,1.),(1.,
1.),(1.,1.),(1.,1.),(1.,1.),(1.,1.),(1.,1.),(1.,1.),(1.,1.),(1.,1.),(1.,
1.),(1.,1.),(1.,1.),(1.,1.),(1.,1.),(1.,1.),(1.,1.),(1.,1.),(1.,1.),(1.,
1.),(1.,1.),(1.,1.),(1.,1.),(1.,1.),(1.,1.),(1.,1.),(1.,1.),(1.,1.),(1.,
1.),(1.,1.),(1.,1.),(1.,1.),(1.,1.),(1.,1.),(1.,1.),(1.,1.),(1.,1.),(1.,
1.),(1.,1.),(1.,1.),(1.,1.),(1.,1.),(1.,1.),(1.,1.),(1.,1.),(1.,1.),(1.,
1.),(1.,1.)))
REPRESENTATION_ITEM('')
SURFACE()
);
#133=(
BOUNDED_SURFACE()
B_SPLINE_SURFACE(5,1,((#64767,#64768),(#64769,#64770),(#64771,#64772),(#64773,
#64774),(#64775,#64776),(#64777,#64778),(#64779,#64780),(#64781,#64782),
(#64783,#64784),(#64785,#64786),(#64787,#64788),(#64789,#64790),(#64791,
#64792),(#64793,#64794),(#64795,#64796),(#64797,#64798),(#64799,#64800),
(#64801,#64802),(#64803,#64804),(#64805,#64806),(#64807,#64808),(#64809,
#64810),(#64811,#64812),(#64813,#64814),(#64815,#64816),(#64817,#64818),
(#64819,#64820),(#64821,#64822),(#64823,#64824),(#64825,#64826),(#64827,
#64828),(#64829,#64830),(#64831,#64832),(#64833,#64834),(#64835,#64836),
(#64837,#64838),(#64839,#64840),(#64841,#64842),(#64843,#64844),(#64845,
#64846),(#64847,#64848),(#64849,#64850),(#64851,#64852),(#64853,#64854),
(#64855,#64856),(#64857,#64858),(#64859,#64860),(#64861,#64862),(#64863,
#64864),(#64865,#64866),(#64867,#64868),(#64869,#64870),(#64871,#64872),
(#64873,#64874),(#64875,#64876),(#64877,#64878),(#64879,#64880),(#64881,
#64882),(#64883,#64884),(#64885,#64886),(#64887,#64888),(#64889,#64890),
(#64891,#64892),(#64893,#64894),(#64895,#64896),(#64897,#64898),(#64899,
#64900),(#64901,#64902),(#64903,#64904),(#64905,#64906)),.UNSPECIFIED.,
 .F.,.F.,.F.)
B_SPLINE_SURFACE_WITH_KNOTS((6,1,1,1,1,1,1,1,1,1,1,1,1,1,1,1,1,1,1,1,1,
1,1,1,1,1,1,1,1,1,1,1,1,1,1,1,1,1,1,1,1,1,1,1,1,1,1,1,1,1,1,1,1,1,1,1,1,
1,1,1,1,1,1,1,1,6),(2,2),(-1.,-0.984615384615383,-0.969230769230768,-0.953846153846152,
-0.938461538461537,-0.923076923076922,-0.907692307692306,-0.892307692307691,
-0.876923076923076,-0.86153846153846,-0.846153846153845,-0.83076923076923,
-0.815384615384614,-0.799999999999999,-0.784615384615384,-0.769230769230768,
-0.753846153846153,-0.738461538461538,-0.723076923076922,-0.707692307692307,
-0.692307692307692,-0.676923076923076,-0.661538461538461,-0.646153846153846,
-0.63076923076923,-0.615384615384615,-0.6,-0.584615384615384,-0.569230769230769,
-0.553846153846154,-0.538461538461538,-0.523076923076923,-0.507692307692308,
-0.492307692307692,-0.476923076923077,-0.461538461538462,-0.446153846153846,
-0.430769230769231,-0.415384615384615,-0.4,-0.384615384615385,-0.369230769230769,
-0.353846153846154,-0.338461538461538,-0.323076923076923,-0.307692307692308,
-0.292307692307692,-0.276923076923077,-0.261538461538462,-0.246153846153846,
-0.230769230769231,-0.215384615384615,-0.2,-0.184615384615385,-0.169230769230769,
-0.153846153846154,-0.138461538461538,-0.123076923076923,-0.107692307692308,
-0.0923076923076923,-0.0769230769230769,-0.0615384615384615,-0.0461538461538462,
-0.0307692307692308,-0.0153846153846154,0.),(-1.,1.),.UNSPECIFIED.)
GEOMETRIC_REPRESENTATION_ITEM()
RATIONAL_B_SPLINE_SURFACE(((1.,1.),(1.,1.),(1.,1.),(1.,1.),(1.,1.),(1.,
1.),(1.,1.),(1.,1.),(1.,1.),(1.,1.),(1.,1.),(1.,1.),(1.,1.),(1.,1.),(1.,
1.),(1.,1.),(1.,1.),(1.,1.),(1.,1.),(1.,1.),(1.,1.),(1.,1.),(1.,1.),(1.,
1.),(1.,1.),(1.,1.),(1.,1.),(1.,1.),(1.,1.),(1.,1.),(1.,1.),(1.,1.),(1.,
1.),(1.,1.),(1.,1.),(1.,1.),(1.,1.),(1.,1.),(1.,1.),(1.,1.),(1.,1.),(1.,
1.),(1.,1.),(1.,1.),(1.,1.),(1.,1.),(1.,1.),(1.,1.),(1.,1.),(1.,1.),(1.,
1.),(1.,1.),(1.,1.),(1.,1.),(1.,1.),(1.,1.),(1.,1.),(1.,1.),(1.,1.),(1.,
1.),(1.,1.),(1.,1.),(1.,1.),(1.,1.),(1.,1.),(1.,1.),(1.,1.),(1.,1.),(1.,
1.),(1.,1.)))
REPRESENTATION_ITEM('')
SURFACE()
);
#134=(
BOUNDED_SURFACE()
B_SPLINE_SURFACE(5,1,((#64979,#64980),(#64981,#64982),(#64983,#64984),(#64985,
#64986),(#64987,#64988),(#64989,#64990),(#64991,#64992),(#64993,#64994),
(#64995,#64996),(#64997,#64998),(#64999,#65000),(#65001,#65002),(#65003,
#65004),(#65005,#65006),(#65007,#65008),(#65009,#65010),(#65011,#65012),
(#65013,#65014),(#65015,#65016),(#65017,#65018),(#65019,#65020),(#65021,
#65022),(#65023,#65024),(#65025,#65026),(#65027,#65028),(#65029,#65030),
(#65031,#65032),(#65033,#65034),(#65035,#65036),(#65037,#65038),(#65039,
#65040),(#65041,#65042),(#65043,#65044),(#65045,#65046),(#65047,#65048),
(#65049,#65050),(#65051,#65052),(#65053,#65054),(#65055,#65056),(#65057,
#65058),(#65059,#65060),(#65061,#65062),(#65063,#65064),(#65065,#65066),
(#65067,#65068),(#65069,#65070),(#65071,#65072),(#65073,#65074),(#65075,
#65076),(#65077,#65078),(#65079,#65080),(#65081,#65082),(#65083,#65084),
(#65085,#65086),(#65087,#65088),(#65089,#65090),(#65091,#65092),(#65093,
#65094),(#65095,#65096),(#65097,#65098),(#65099,#65100),(#65101,#65102),
(#65103,#65104),(#65105,#65106),(#65107,#65108),(#65109,#65110),(#65111,
#65112),(#65113,#65114),(#65115,#65116),(#65117,#65118)),.UNSPECIFIED.,
 .F.,.F.,.F.)
B_SPLINE_SURFACE_WITH_KNOTS((6,1,1,1,1,1,1,1,1,1,1,1,1,1,1,1,1,1,1,1,1,
1,1,1,1,1,1,1,1,1,1,1,1,1,1,1,1,1,1,1,1,1,1,1,1,1,1,1,1,1,1,1,1,1,1,1,1,
1,1,1,1,1,1,1,1,6),(2,2),(-1.,-0.984615384615383,-0.969230769230768,-0.953846153846152,
-0.938461538461537,-0.923076923076922,-0.907692307692306,-0.892307692307691,
-0.876923076923076,-0.86153846153846,-0.846153846153845,-0.83076923076923,
-0.815384615384614,-0.799999999999999,-0.784615384615384,-0.769230769230768,
-0.753846153846153,-0.738461538461538,-0.723076923076922,-0.707692307692307,
-0.692307692307692,-0.676923076923076,-0.661538461538461,-0.646153846153846,
-0.63076923076923,-0.615384615384615,-0.6,-0.584615384615384,-0.569230769230769,
-0.553846153846154,-0.538461538461538,-0.523076923076923,-0.507692307692308,
-0.492307692307692,-0.476923076923077,-0.461538461538462,-0.446153846153846,
-0.430769230769231,-0.415384615384615,-0.4,-0.384615384615385,-0.369230769230769,
-0.353846153846154,-0.338461538461538,-0.323076923076923,-0.307692307692308,
-0.292307692307692,-0.276923076923077,-0.261538461538462,-0.246153846153846,
-0.230769230769231,-0.215384615384615,-0.2,-0.184615384615385,-0.169230769230769,
-0.153846153846154,-0.138461538461538,-0.123076923076923,-0.107692307692308,
-0.0923076923076923,-0.0769230769230769,-0.0615384615384615,-0.0461538461538462,
-0.0307692307692308,-0.0153846153846154,0.),(-1.,1.),.UNSPECIFIED.)
GEOMETRIC_REPRESENTATION_ITEM()
RATIONAL_B_SPLINE_SURFACE(((1.,1.),(1.,1.),(1.,1.),(1.,1.),(1.,1.),(1.,
1.),(1.,1.),(1.,1.),(1.,1.),(1.,1.),(1.,1.),(1.,1.),(1.,1.),(1.,1.),(1.,
1.),(1.,1.),(1.,1.),(1.,1.),(1.,1.),(1.,1.),(1.,1.),(1.,1.),(1.,1.),(1.,
1.),(1.,1.),(1.,1.),(1.,1.),(1.,1.),(1.,1.),(1.,1.),(1.,1.),(1.,1.),(1.,
1.),(1.,1.),(1.,1.),(1.,1.),(1.,1.),(1.,1.),(1.,1.),(1.,1.),(1.,1.),(1.,
1.),(1.,1.),(1.,1.),(1.,1.),(1.,1.),(1.,1.),(1.,1.),(1.,1.),(1.,1.),(1.,
1.),(1.,1.),(1.,1.),(1.,1.),(1.,1.),(1.,1.),(1.,1.),(1.,1.),(1.,1.),(1.,
1.),(1.,1.),(1.,1.),(1.,1.),(1.,1.),(1.,1.),(1.,1.),(1.,1.),(1.,1.),(1.,
1.),(1.,1.)))
REPRESENTATION_ITEM('')
SURFACE()
);
#135=(
BOUNDED_SURFACE()
B_SPLINE_SURFACE(5,1,((#65209,#65210),(#65211,#65212),(#65213,#65214),(#65215,
#65216),(#65217,#65218),(#65219,#65220),(#65221,#65222),(#65223,#65224),
(#65225,#65226),(#65227,#65228),(#65229,#65230),(#65231,#65232),(#65233,
#65234),(#65235,#65236),(#65237,#65238),(#65239,#65240),(#65241,#65242),
(#65243,#65244),(#65245,#65246),(#65247,#65248),(#65249,#65250),(#65251,
#65252),(#65253,#65254),(#65255,#65256),(#65257,#65258),(#65259,#65260),
(#65261,#65262),(#65263,#65264),(#65265,#65266),(#65267,#65268),(#65269,
#65270),(#65271,#65272),(#65273,#65274),(#65275,#65276),(#65277,#65278),
(#65279,#65280),(#65281,#65282),(#65283,#65284),(#65285,#65286),(#65287,
#65288),(#65289,#65290),(#65291,#65292),(#65293,#65294),(#65295,#65296),
(#65297,#65298),(#65299,#65300),(#65301,#65302),(#65303,#65304),(#65305,
#65306),(#65307,#65308),(#65309,#65310),(#65311,#65312),(#65313,#65314),
(#65315,#65316),(#65317,#65318),(#65319,#65320),(#65321,#65322),(#65323,
#65324),(#65325,#65326),(#65327,#65328),(#65329,#65330),(#65331,#65332),
(#65333,#65334),(#65335,#65336),(#65337,#65338),(#65339,#65340),(#65341,
#65342),(#65343,#65344),(#65345,#65346),(#65347,#65348)),.UNSPECIFIED.,
 .F.,.F.,.F.)
B_SPLINE_SURFACE_WITH_KNOTS((6,1,1,1,1,1,1,1,1,1,1,1,1,1,1,1,1,1,1,1,1,
1,1,1,1,1,1,1,1,1,1,1,1,1,1,1,1,1,1,1,1,1,1,1,1,1,1,1,1,1,1,1,1,1,1,1,1,
1,1,1,1,1,1,1,1,6),(2,2),(-1.,-0.984615384615383,-0.969230769230768,-0.953846153846152,
-0.938461538461537,-0.923076923076922,-0.907692307692306,-0.892307692307691,
-0.876923076923076,-0.86153846153846,-0.846153846153845,-0.83076923076923,
-0.815384615384614,-0.799999999999999,-0.784615384615384,-0.769230769230768,
-0.753846153846153,-0.738461538461538,-0.723076923076922,-0.707692307692307,
-0.692307692307692,-0.676923076923076,-0.661538461538461,-0.646153846153846,
-0.63076923076923,-0.615384615384615,-0.6,-0.584615384615384,-0.569230769230769,
-0.553846153846154,-0.538461538461538,-0.523076923076923,-0.507692307692308,
-0.492307692307692,-0.476923076923077,-0.461538461538462,-0.446153846153846,
-0.430769230769231,-0.415384615384615,-0.4,-0.384615384615385,-0.369230769230769,
-0.353846153846154,-0.338461538461538,-0.323076923076923,-0.307692307692308,
-0.292307692307692,-0.276923076923077,-0.261538461538462,-0.246153846153846,
-0.230769230769231,-0.215384615384615,-0.2,-0.184615384615385,-0.169230769230769,
-0.153846153846154,-0.138461538461538,-0.123076923076923,-0.107692307692308,
-0.0923076923076923,-0.0769230769230769,-0.0615384615384615,-0.0461538461538462,
-0.0307692307692308,-0.0153846153846154,0.),(-1.,1.),.UNSPECIFIED.)
GEOMETRIC_REPRESENTATION_ITEM()
RATIONAL_B_SPLINE_SURFACE(((1.,1.),(1.,1.),(1.,1.),(1.,1.),(1.,1.),(1.,
1.),(1.,1.),(1.,1.),(1.,1.),(1.,1.),(1.,1.),(1.,1.),(1.,1.),(1.,1.),(1.,
1.),(1.,1.),(1.,1.),(1.,1.),(1.,1.),(1.,1.),(1.,1.),(1.,1.),(1.,1.),(1.,
1.),(1.,1.),(1.,1.),(1.,1.),(1.,1.),(1.,1.),(1.,1.),(1.,1.),(1.,1.),(1.,
1.),(1.,1.),(1.,1.),(1.,1.),(1.,1.),(1.,1.),(1.,1.),(1.,1.),(1.,1.),(1.,
1.),(1.,1.),(1.,1.),(1.,1.),(1.,1.),(1.,1.),(1.,1.),(1.,1.),(1.,1.),(1.,
1.),(1.,1.),(1.,1.),(1.,1.),(1.,1.),(1.,1.),(1.,1.),(1.,1.),(1.,1.),(1.,
1.),(1.,1.),(1.,1.),(1.,1.),(1.,1.),(1.,1.),(1.,1.),(1.,1.),(1.,1.),(1.,
1.),(1.,1.)))
REPRESENTATION_ITEM('')
SURFACE()
);
#136=(
BOUNDED_SURFACE()
B_SPLINE_SURFACE(5,1,((#65421,#65422),(#65423,#65424),(#65425,#65426),(#65427,
#65428),(#65429,#65430),(#65431,#65432),(#65433,#65434),(#65435,#65436),
(#65437,#65438),(#65439,#65440),(#65441,#65442),(#65443,#65444),(#65445,
#65446),(#65447,#65448),(#65449,#65450),(#65451,#65452),(#65453,#65454),
(#65455,#65456),(#65457,#65458),(#65459,#65460),(#65461,#65462),(#65463,
#65464),(#65465,#65466),(#65467,#65468),(#65469,#65470),(#65471,#65472),
(#65473,#65474),(#65475,#65476),(#65477,#65478),(#65479,#65480),(#65481,
#65482),(#65483,#65484),(#65485,#65486),(#65487,#65488),(#65489,#65490),
(#65491,#65492),(#65493,#65494),(#65495,#65496),(#65497,#65498),(#65499,
#65500),(#65501,#65502),(#65503,#65504),(#65505,#65506),(#65507,#65508),
(#65509,#65510),(#65511,#65512),(#65513,#65514),(#65515,#65516),(#65517,
#65518),(#65519,#65520),(#65521,#65522),(#65523,#65524),(#65525,#65526),
(#65527,#65528),(#65529,#65530),(#65531,#65532),(#65533,#65534),(#65535,
#65536),(#65537,#65538),(#65539,#65540),(#65541,#65542),(#65543,#65544),
(#65545,#65546),(#65547,#65548),(#65549,#65550),(#65551,#65552),(#65553,
#65554),(#65555,#65556),(#65557,#65558),(#65559,#65560)),.UNSPECIFIED.,
 .F.,.F.,.F.)
B_SPLINE_SURFACE_WITH_KNOTS((6,1,1,1,1,1,1,1,1,1,1,1,1,1,1,1,1,1,1,1,1,
1,1,1,1,1,1,1,1,1,1,1,1,1,1,1,1,1,1,1,1,1,1,1,1,1,1,1,1,1,1,1,1,1,1,1,1,
1,1,1,1,1,1,1,1,6),(2,2),(-1.,-0.984615384615383,-0.969230769230768,-0.953846153846152,
-0.938461538461537,-0.923076923076922,-0.907692307692306,-0.892307692307691,
-0.876923076923076,-0.86153846153846,-0.846153846153845,-0.83076923076923,
-0.815384615384614,-0.799999999999999,-0.784615384615384,-0.769230769230768,
-0.753846153846153,-0.738461538461538,-0.723076923076922,-0.707692307692307,
-0.692307692307692,-0.676923076923076,-0.661538461538461,-0.646153846153846,
-0.63076923076923,-0.615384615384615,-0.6,-0.584615384615384,-0.569230769230769,
-0.553846153846154,-0.538461538461538,-0.523076923076923,-0.507692307692308,
-0.492307692307692,-0.476923076923077,-0.461538461538462,-0.446153846153846,
-0.430769230769231,-0.415384615384615,-0.4,-0.384615384615385,-0.369230769230769,
-0.353846153846154,-0.338461538461538,-0.323076923076923,-0.307692307692308,
-0.292307692307692,-0.276923076923077,-0.261538461538462,-0.246153846153846,
-0.230769230769231,-0.215384615384615,-0.2,-0.184615384615385,-0.169230769230769,
-0.153846153846154,-0.138461538461538,-0.123076923076923,-0.107692307692308,
-0.0923076923076923,-0.0769230769230769,-0.0615384615384615,-0.0461538461538462,
-0.0307692307692308,-0.0153846153846154,0.),(-1.,1.),.UNSPECIFIED.)
GEOMETRIC_REPRESENTATION_ITEM()
RATIONAL_B_SPLINE_SURFACE(((1.,1.),(1.,1.),(1.,1.),(1.,1.),(1.,1.),(1.,
1.),(1.,1.),(1.,1.),(1.,1.),(1.,1.),(1.,1.),(1.,1.),(1.,1.),(1.,1.),(1.,
1.),(1.,1.),(1.,1.),(1.,1.),(1.,1.),(1.,1.),(1.,1.),(1.,1.),(1.,1.),(1.,
1.),(1.,1.),(1.,1.),(1.,1.),(1.,1.),(1.,1.),(1.,1.),(1.,1.),(1.,1.),(1.,
1.),(1.,1.),(1.,1.),(1.,1.),(1.,1.),(1.,1.),(1.,1.),(1.,1.),(1.,1.),(1.,
1.),(1.,1.),(1.,1.),(1.,1.),(1.,1.),(1.,1.),(1.,1.),(1.,1.),(1.,1.),(1.,
1.),(1.,1.),(1.,1.),(1.,1.),(1.,1.),(1.,1.),(1.,1.),(1.,1.),(1.,1.),(1.,
1.),(1.,1.),(1.,1.),(1.,1.),(1.,1.),(1.,1.),(1.,1.),(1.,1.),(1.,1.),(1.,
1.),(1.,1.)))
REPRESENTATION_ITEM('')
SURFACE()
);
#137=(
BOUNDED_SURFACE()
B_SPLINE_SURFACE(5,1,((#65651,#65652),(#65653,#65654),(#65655,#65656),(#65657,
#65658),(#65659,#65660),(#65661,#65662),(#65663,#65664),(#65665,#65666),
(#65667,#65668),(#65669,#65670),(#65671,#65672),(#65673,#65674),(#65675,
#65676),(#65677,#65678),(#65679,#65680),(#65681,#65682),(#65683,#65684),
(#65685,#65686),(#65687,#65688),(#65689,#65690),(#65691,#65692),(#65693,
#65694),(#65695,#65696),(#65697,#65698),(#65699,#65700),(#65701,#65702),
(#65703,#65704),(#65705,#65706),(#65707,#65708),(#65709,#65710),(#65711,
#65712),(#65713,#65714),(#65715,#65716),(#65717,#65718),(#65719,#65720),
(#65721,#65722),(#65723,#65724),(#65725,#65726),(#65727,#65728),(#65729,
#65730),(#65731,#65732),(#65733,#65734),(#65735,#65736),(#65737,#65738),
(#65739,#65740),(#65741,#65742),(#65743,#65744),(#65745,#65746),(#65747,
#65748),(#65749,#65750),(#65751,#65752),(#65753,#65754),(#65755,#65756),
(#65757,#65758),(#65759,#65760),(#65761,#65762),(#65763,#65764),(#65765,
#65766),(#65767,#65768),(#65769,#65770),(#65771,#65772),(#65773,#65774),
(#65775,#65776),(#65777,#65778),(#65779,#65780),(#65781,#65782),(#65783,
#65784),(#65785,#65786),(#65787,#65788),(#65789,#65790)),.UNSPECIFIED.,
 .F.,.F.,.F.)
B_SPLINE_SURFACE_WITH_KNOTS((6,1,1,1,1,1,1,1,1,1,1,1,1,1,1,1,1,1,1,1,1,
1,1,1,1,1,1,1,1,1,1,1,1,1,1,1,1,1,1,1,1,1,1,1,1,1,1,1,1,1,1,1,1,1,1,1,1,
1,1,1,1,1,1,1,1,6),(2,2),(-1.,-0.984615384615383,-0.969230769230768,-0.953846153846152,
-0.938461538461537,-0.923076923076922,-0.907692307692306,-0.892307692307691,
-0.876923076923076,-0.86153846153846,-0.846153846153845,-0.83076923076923,
-0.815384615384614,-0.799999999999999,-0.784615384615384,-0.769230769230768,
-0.753846153846153,-0.738461538461538,-0.723076923076922,-0.707692307692307,
-0.692307692307692,-0.676923076923076,-0.661538461538461,-0.646153846153846,
-0.63076923076923,-0.615384615384615,-0.6,-0.584615384615384,-0.569230769230769,
-0.553846153846154,-0.538461538461538,-0.523076923076923,-0.507692307692308,
-0.492307692307692,-0.476923076923077,-0.461538461538462,-0.446153846153846,
-0.430769230769231,-0.415384615384615,-0.4,-0.384615384615385,-0.369230769230769,
-0.353846153846154,-0.338461538461538,-0.323076923076923,-0.307692307692308,
-0.292307692307692,-0.276923076923077,-0.261538461538462,-0.246153846153846,
-0.230769230769231,-0.215384615384615,-0.2,-0.184615384615385,-0.169230769230769,
-0.153846153846154,-0.138461538461538,-0.123076923076923,-0.107692307692308,
-0.0923076923076923,-0.0769230769230769,-0.0615384615384615,-0.0461538461538462,
-0.0307692307692308,-0.0153846153846154,0.),(-1.,1.),.UNSPECIFIED.)
GEOMETRIC_REPRESENTATION_ITEM()
RATIONAL_B_SPLINE_SURFACE(((1.,1.),(1.,1.),(1.,1.),(1.,1.),(1.,1.),(1.,
1.),(1.,1.),(1.,1.),(1.,1.),(1.,1.),(1.,1.),(1.,1.),(1.,1.),(1.,1.),(1.,
1.),(1.,1.),(1.,1.),(1.,1.),(1.,1.),(1.,1.),(1.,1.),(1.,1.),(1.,1.),(1.,
1.),(1.,1.),(1.,1.),(1.,1.),(1.,1.),(1.,1.),(1.,1.),(1.,1.),(1.,1.),(1.,
1.),(1.,1.),(1.,1.),(1.,1.),(1.,1.),(1.,1.),(1.,1.),(1.,1.),(1.,1.),(1.,
1.),(1.,1.),(1.,1.),(1.,1.),(1.,1.),(1.,1.),(1.,1.),(1.,1.),(1.,1.),(1.,
1.),(1.,1.),(1.,1.),(1.,1.),(1.,1.),(1.,1.),(1.,1.),(1.,1.),(1.,1.),(1.,
1.),(1.,1.),(1.,1.),(1.,1.),(1.,1.),(1.,1.),(1.,1.),(1.,1.),(1.,1.),(1.,
1.),(1.,1.)))
REPRESENTATION_ITEM('')
SURFACE()
);
#138=(
BOUNDED_SURFACE()
B_SPLINE_SURFACE(5,1,((#65863,#65864),(#65865,#65866),(#65867,#65868),(#65869,
#65870),(#65871,#65872),(#65873,#65874),(#65875,#65876),(#65877,#65878),
(#65879,#65880),(#65881,#65882),(#65883,#65884),(#65885,#65886),(#65887,
#65888),(#65889,#65890),(#65891,#65892),(#65893,#65894),(#65895,#65896),
(#65897,#65898),(#65899,#65900),(#65901,#65902),(#65903,#65904),(#65905,
#65906),(#65907,#65908),(#65909,#65910),(#65911,#65912),(#65913,#65914),
(#65915,#65916),(#65917,#65918),(#65919,#65920),(#65921,#65922),(#65923,
#65924),(#65925,#65926),(#65927,#65928),(#65929,#65930),(#65931,#65932),
(#65933,#65934),(#65935,#65936),(#65937,#65938),(#65939,#65940),(#65941,
#65942),(#65943,#65944),(#65945,#65946),(#65947,#65948),(#65949,#65950),
(#65951,#65952),(#65953,#65954),(#65955,#65956),(#65957,#65958),(#65959,
#65960),(#65961,#65962),(#65963,#65964),(#65965,#65966),(#65967,#65968),
(#65969,#65970),(#65971,#65972),(#65973,#65974),(#65975,#65976),(#65977,
#65978),(#65979,#65980),(#65981,#65982),(#65983,#65984),(#65985,#65986),
(#65987,#65988),(#65989,#65990),(#65991,#65992),(#65993,#65994),(#65995,
#65996),(#65997,#65998),(#65999,#66000),(#66001,#66002)),.UNSPECIFIED.,
 .F.,.F.,.F.)
B_SPLINE_SURFACE_WITH_KNOTS((6,1,1,1,1,1,1,1,1,1,1,1,1,1,1,1,1,1,1,1,1,
1,1,1,1,1,1,1,1,1,1,1,1,1,1,1,1,1,1,1,1,1,1,1,1,1,1,1,1,1,1,1,1,1,1,1,1,
1,1,1,1,1,1,1,1,6),(2,2),(-1.,-0.984615384615383,-0.969230769230768,-0.953846153846152,
-0.938461538461537,-0.923076923076922,-0.907692307692306,-0.892307692307691,
-0.876923076923076,-0.86153846153846,-0.846153846153845,-0.83076923076923,
-0.815384615384614,-0.799999999999999,-0.784615384615384,-0.769230769230768,
-0.753846153846153,-0.738461538461538,-0.723076923076922,-0.707692307692307,
-0.692307692307692,-0.676923076923076,-0.661538461538461,-0.646153846153846,
-0.63076923076923,-0.615384615384615,-0.6,-0.584615384615384,-0.569230769230769,
-0.553846153846154,-0.538461538461538,-0.523076923076923,-0.507692307692308,
-0.492307692307692,-0.476923076923077,-0.461538461538462,-0.446153846153846,
-0.430769230769231,-0.415384615384615,-0.4,-0.384615384615385,-0.369230769230769,
-0.353846153846154,-0.338461538461538,-0.323076923076923,-0.307692307692308,
-0.292307692307692,-0.276923076923077,-0.261538461538462,-0.246153846153846,
-0.230769230769231,-0.215384615384615,-0.2,-0.184615384615385,-0.169230769230769,
-0.153846153846154,-0.138461538461538,-0.123076923076923,-0.107692307692308,
-0.0923076923076923,-0.0769230769230769,-0.0615384615384615,-0.0461538461538462,
-0.0307692307692308,-0.0153846153846154,0.),(-1.,1.),.UNSPECIFIED.)
GEOMETRIC_REPRESENTATION_ITEM()
RATIONAL_B_SPLINE_SURFACE(((1.,1.),(1.,1.),(1.,1.),(1.,1.),(1.,1.),(1.,
1.),(1.,1.),(1.,1.),(1.,1.),(1.,1.),(1.,1.),(1.,1.),(1.,1.),(1.,1.),(1.,
1.),(1.,1.),(1.,1.),(1.,1.),(1.,1.),(1.,1.),(1.,1.),(1.,1.),(1.,1.),(1.,
1.),(1.,1.),(1.,1.),(1.,1.),(1.,1.),(1.,1.),(1.,1.),(1.,1.),(1.,1.),(1.,
1.),(1.,1.),(1.,1.),(1.,1.),(1.,1.),(1.,1.),(1.,1.),(1.,1.),(1.,1.),(1.,
1.),(1.,1.),(1.,1.),(1.,1.),(1.,1.),(1.,1.),(1.,1.),(1.,1.),(1.,1.),(1.,
1.),(1.,1.),(1.,1.),(1.,1.),(1.,1.),(1.,1.),(1.,1.),(1.,1.),(1.,1.),(1.,
1.),(1.,1.),(1.,1.),(1.,1.),(1.,1.),(1.,1.),(1.,1.),(1.,1.),(1.,1.),(1.,
1.),(1.,1.)))
REPRESENTATION_ITEM('')
SURFACE()
);
#139=(
BOUNDED_SURFACE()
B_SPLINE_SURFACE(5,1,((#66093,#66094),(#66095,#66096),(#66097,#66098),(#66099,
#66100),(#66101,#66102),(#66103,#66104),(#66105,#66106),(#66107,#66108),
(#66109,#66110),(#66111,#66112),(#66113,#66114),(#66115,#66116),(#66117,
#66118),(#66119,#66120),(#66121,#66122),(#66123,#66124),(#66125,#66126),
(#66127,#66128),(#66129,#66130),(#66131,#66132),(#66133,#66134),(#66135,
#66136),(#66137,#66138),(#66139,#66140),(#66141,#66142),(#66143,#66144),
(#66145,#66146),(#66147,#66148),(#66149,#66150),(#66151,#66152),(#66153,
#66154),(#66155,#66156),(#66157,#66158),(#66159,#66160),(#66161,#66162),
(#66163,#66164),(#66165,#66166),(#66167,#66168),(#66169,#66170),(#66171,
#66172),(#66173,#66174),(#66175,#66176),(#66177,#66178),(#66179,#66180),
(#66181,#66182),(#66183,#66184),(#66185,#66186),(#66187,#66188),(#66189,
#66190),(#66191,#66192),(#66193,#66194),(#66195,#66196),(#66197,#66198),
(#66199,#66200),(#66201,#66202),(#66203,#66204),(#66205,#66206),(#66207,
#66208),(#66209,#66210),(#66211,#66212),(#66213,#66214),(#66215,#66216),
(#66217,#66218),(#66219,#66220),(#66221,#66222),(#66223,#66224),(#66225,
#66226),(#66227,#66228),(#66229,#66230),(#66231,#66232)),.UNSPECIFIED.,
 .F.,.F.,.F.)
B_SPLINE_SURFACE_WITH_KNOTS((6,1,1,1,1,1,1,1,1,1,1,1,1,1,1,1,1,1,1,1,1,
1,1,1,1,1,1,1,1,1,1,1,1,1,1,1,1,1,1,1,1,1,1,1,1,1,1,1,1,1,1,1,1,1,1,1,1,
1,1,1,1,1,1,1,1,6),(2,2),(-1.,-0.984615384615383,-0.969230769230768,-0.953846153846152,
-0.938461538461537,-0.923076923076922,-0.907692307692306,-0.892307692307691,
-0.876923076923076,-0.86153846153846,-0.846153846153845,-0.83076923076923,
-0.815384615384614,-0.799999999999999,-0.784615384615384,-0.769230769230768,
-0.753846153846153,-0.738461538461538,-0.723076923076922,-0.707692307692307,
-0.692307692307692,-0.676923076923076,-0.661538461538461,-0.646153846153846,
-0.63076923076923,-0.615384615384615,-0.6,-0.584615384615384,-0.569230769230769,
-0.553846153846154,-0.538461538461538,-0.523076923076923,-0.507692307692308,
-0.492307692307692,-0.476923076923077,-0.461538461538462,-0.446153846153846,
-0.430769230769231,-0.415384615384615,-0.4,-0.384615384615385,-0.369230769230769,
-0.353846153846154,-0.338461538461538,-0.323076923076923,-0.307692307692308,
-0.292307692307692,-0.276923076923077,-0.261538461538462,-0.246153846153846,
-0.230769230769231,-0.215384615384615,-0.2,-0.184615384615385,-0.169230769230769,
-0.153846153846154,-0.138461538461538,-0.123076923076923,-0.107692307692308,
-0.0923076923076923,-0.0769230769230769,-0.0615384615384615,-0.0461538461538462,
-0.0307692307692308,-0.0153846153846154,0.),(-1.,1.),.UNSPECIFIED.)
GEOMETRIC_REPRESENTATION_ITEM()
RATIONAL_B_SPLINE_SURFACE(((1.,1.),(1.,1.),(1.,1.),(1.,1.),(1.,1.),(1.,
1.),(1.,1.),(1.,1.),(1.,1.),(1.,1.),(1.,1.),(1.,1.),(1.,1.),(1.,1.),(1.,
1.),(1.,1.),(1.,1.),(1.,1.),(1.,1.),(1.,1.),(1.,1.),(1.,1.),(1.,1.),(1.,
1.),(1.,1.),(1.,1.),(1.,1.),(1.,1.),(1.,1.),(1.,1.),(1.,1.),(1.,1.),(1.,
1.),(1.,1.),(1.,1.),(1.,1.),(1.,1.),(1.,1.),(1.,1.),(1.,1.),(1.,1.),(1.,
1.),(1.,1.),(1.,1.),(1.,1.),(1.,1.),(1.,1.),(1.,1.),(1.,1.),(1.,1.),(1.,
1.),(1.,1.),(1.,1.),(1.,1.),(1.,1.),(1.,1.),(1.,1.),(1.,1.),(1.,1.),(1.,
1.),(1.,1.),(1.,1.),(1.,1.),(1.,1.),(1.,1.),(1.,1.),(1.,1.),(1.,1.),(1.,
1.),(1.,1.)))
REPRESENTATION_ITEM('')
SURFACE()
);
#140=(
BOUNDED_SURFACE()
B_SPLINE_SURFACE(5,1,((#66305,#66306),(#66307,#66308),(#66309,#66310),(#66311,
#66312),(#66313,#66314),(#66315,#66316),(#66317,#66318),(#66319,#66320),
(#66321,#66322),(#66323,#66324),(#66325,#66326),(#66327,#66328),(#66329,
#66330),(#66331,#66332),(#66333,#66334),(#66335,#66336),(#66337,#66338),
(#66339,#66340),(#66341,#66342),(#66343,#66344),(#66345,#66346),(#66347,
#66348),(#66349,#66350),(#66351,#66352),(#66353,#66354),(#66355,#66356),
(#66357,#66358),(#66359,#66360),(#66361,#66362),(#66363,#66364),(#66365,
#66366),(#66367,#66368),(#66369,#66370),(#66371,#66372),(#66373,#66374),
(#66375,#66376),(#66377,#66378),(#66379,#66380),(#66381,#66382),(#66383,
#66384),(#66385,#66386),(#66387,#66388),(#66389,#66390),(#66391,#66392),
(#66393,#66394),(#66395,#66396),(#66397,#66398),(#66399,#66400),(#66401,
#66402),(#66403,#66404),(#66405,#66406),(#66407,#66408),(#66409,#66410),
(#66411,#66412),(#66413,#66414),(#66415,#66416),(#66417,#66418),(#66419,
#66420),(#66421,#66422),(#66423,#66424),(#66425,#66426),(#66427,#66428),
(#66429,#66430),(#66431,#66432),(#66433,#66434),(#66435,#66436),(#66437,
#66438),(#66439,#66440),(#66441,#66442),(#66443,#66444)),.UNSPECIFIED.,
 .F.,.F.,.F.)
B_SPLINE_SURFACE_WITH_KNOTS((6,1,1,1,1,1,1,1,1,1,1,1,1,1,1,1,1,1,1,1,1,
1,1,1,1,1,1,1,1,1,1,1,1,1,1,1,1,1,1,1,1,1,1,1,1,1,1,1,1,1,1,1,1,1,1,1,1,
1,1,1,1,1,1,1,1,6),(2,2),(-1.,-0.984615384615383,-0.969230769230768,-0.953846153846152,
-0.938461538461537,-0.923076923076922,-0.907692307692306,-0.892307692307691,
-0.876923076923076,-0.86153846153846,-0.846153846153845,-0.83076923076923,
-0.815384615384614,-0.799999999999999,-0.784615384615384,-0.769230769230768,
-0.753846153846153,-0.738461538461538,-0.723076923076922,-0.707692307692307,
-0.692307692307692,-0.676923076923076,-0.661538461538461,-0.646153846153846,
-0.63076923076923,-0.615384615384615,-0.6,-0.584615384615384,-0.569230769230769,
-0.553846153846154,-0.538461538461538,-0.523076923076923,-0.507692307692308,
-0.492307692307692,-0.476923076923077,-0.461538461538462,-0.446153846153846,
-0.430769230769231,-0.415384615384615,-0.4,-0.384615384615385,-0.369230769230769,
-0.353846153846154,-0.338461538461538,-0.323076923076923,-0.307692307692308,
-0.292307692307692,-0.276923076923077,-0.261538461538462,-0.246153846153846,
-0.230769230769231,-0.215384615384615,-0.2,-0.184615384615385,-0.169230769230769,
-0.153846153846154,-0.138461538461538,-0.123076923076923,-0.107692307692308,
-0.0923076923076923,-0.0769230769230769,-0.0615384615384615,-0.0461538461538462,
-0.0307692307692308,-0.0153846153846154,0.),(-1.,1.),.UNSPECIFIED.)
GEOMETRIC_REPRESENTATION_ITEM()
RATIONAL_B_SPLINE_SURFACE(((1.,1.),(1.,1.),(1.,1.),(1.,1.),(1.,1.),(1.,
1.),(1.,1.),(1.,1.),(1.,1.),(1.,1.),(1.,1.),(1.,1.),(1.,1.),(1.,1.),(1.,
1.),(1.,1.),(1.,1.),(1.,1.),(1.,1.),(1.,1.),(1.,1.),(1.,1.),(1.,1.),(1.,
1.),(1.,1.),(1.,1.),(1.,1.),(1.,1.),(1.,1.),(1.,1.),(1.,1.),(1.,1.),(1.,
1.),(1.,1.),(1.,1.),(1.,1.),(1.,1.),(1.,1.),(1.,1.),(1.,1.),(1.,1.),(1.,
1.),(1.,1.),(1.,1.),(1.,1.),(1.,1.),(1.,1.),(1.,1.),(1.,1.),(1.,1.),(1.,
1.),(1.,1.),(1.,1.),(1.,1.),(1.,1.),(1.,1.),(1.,1.),(1.,1.),(1.,1.),(1.,
1.),(1.,1.),(1.,1.),(1.,1.),(1.,1.),(1.,1.),(1.,1.),(1.,1.),(1.,1.),(1.,
1.),(1.,1.)))
REPRESENTATION_ITEM('')
SURFACE()
);
#141=(
BOUNDED_SURFACE()
B_SPLINE_SURFACE(5,1,((#66535,#66536),(#66537,#66538),(#66539,#66540),(#66541,
#66542),(#66543,#66544),(#66545,#66546),(#66547,#66548),(#66549,#66550),
(#66551,#66552),(#66553,#66554),(#66555,#66556),(#66557,#66558),(#66559,
#66560),(#66561,#66562),(#66563,#66564),(#66565,#66566),(#66567,#66568),
(#66569,#66570),(#66571,#66572),(#66573,#66574),(#66575,#66576),(#66577,
#66578),(#66579,#66580),(#66581,#66582),(#66583,#66584),(#66585,#66586),
(#66587,#66588),(#66589,#66590),(#66591,#66592),(#66593,#66594),(#66595,
#66596),(#66597,#66598),(#66599,#66600),(#66601,#66602),(#66603,#66604),
(#66605,#66606),(#66607,#66608),(#66609,#66610),(#66611,#66612),(#66613,
#66614),(#66615,#66616),(#66617,#66618),(#66619,#66620),(#66621,#66622),
(#66623,#66624),(#66625,#66626),(#66627,#66628),(#66629,#66630),(#66631,
#66632),(#66633,#66634),(#66635,#66636),(#66637,#66638),(#66639,#66640),
(#66641,#66642),(#66643,#66644),(#66645,#66646),(#66647,#66648),(#66649,
#66650),(#66651,#66652),(#66653,#66654),(#66655,#66656),(#66657,#66658),
(#66659,#66660),(#66661,#66662),(#66663,#66664),(#66665,#66666),(#66667,
#66668),(#66669,#66670),(#66671,#66672),(#66673,#66674)),.UNSPECIFIED.,
 .F.,.F.,.F.)
B_SPLINE_SURFACE_WITH_KNOTS((6,1,1,1,1,1,1,1,1,1,1,1,1,1,1,1,1,1,1,1,1,
1,1,1,1,1,1,1,1,1,1,1,1,1,1,1,1,1,1,1,1,1,1,1,1,1,1,1,1,1,1,1,1,1,1,1,1,
1,1,1,1,1,1,1,1,6),(2,2),(-1.,-0.984615384615383,-0.969230769230768,-0.953846153846152,
-0.938461538461537,-0.923076923076922,-0.907692307692306,-0.892307692307691,
-0.876923076923076,-0.86153846153846,-0.846153846153845,-0.83076923076923,
-0.815384615384614,-0.799999999999999,-0.784615384615384,-0.769230769230768,
-0.753846153846153,-0.738461538461538,-0.723076923076922,-0.707692307692307,
-0.692307692307692,-0.676923076923076,-0.661538461538461,-0.646153846153846,
-0.63076923076923,-0.615384615384615,-0.6,-0.584615384615384,-0.569230769230769,
-0.553846153846154,-0.538461538461538,-0.523076923076923,-0.507692307692308,
-0.492307692307692,-0.476923076923077,-0.461538461538462,-0.446153846153846,
-0.430769230769231,-0.415384615384615,-0.4,-0.384615384615385,-0.369230769230769,
-0.353846153846154,-0.338461538461538,-0.323076923076923,-0.307692307692308,
-0.292307692307692,-0.276923076923077,-0.261538461538462,-0.246153846153846,
-0.230769230769231,-0.215384615384615,-0.2,-0.184615384615385,-0.169230769230769,
-0.153846153846154,-0.138461538461538,-0.123076923076923,-0.107692307692308,
-0.0923076923076923,-0.0769230769230769,-0.0615384615384615,-0.0461538461538462,
-0.0307692307692308,-0.0153846153846154,0.),(-1.,1.),.UNSPECIFIED.)
GEOMETRIC_REPRESENTATION_ITEM()
RATIONAL_B_SPLINE_SURFACE(((1.,1.),(1.,1.),(1.,1.),(1.,1.),(1.,1.),(1.,
1.),(1.,1.),(1.,1.),(1.,1.),(1.,1.),(1.,1.),(1.,1.),(1.,1.),(1.,1.),(1.,
1.),(1.,1.),(1.,1.),(1.,1.),(1.,1.),(1.,1.),(1.,1.),(1.,1.),(1.,1.),(1.,
1.),(1.,1.),(1.,1.),(1.,1.),(1.,1.),(1.,1.),(1.,1.),(1.,1.),(1.,1.),(1.,
1.),(1.,1.),(1.,1.),(1.,1.),(1.,1.),(1.,1.),(1.,1.),(1.,1.),(1.,1.),(1.,
1.),(1.,1.),(1.,1.),(1.,1.),(1.,1.),(1.,1.),(1.,1.),(1.,1.),(1.,1.),(1.,
1.),(1.,1.),(1.,1.),(1.,1.),(1.,1.),(1.,1.),(1.,1.),(1.,1.),(1.,1.),(1.,
1.),(1.,1.),(1.,1.),(1.,1.),(1.,1.),(1.,1.),(1.,1.),(1.,1.),(1.,1.),(1.,
1.),(1.,1.)))
REPRESENTATION_ITEM('')
SURFACE()
);
#142=(
BOUNDED_SURFACE()
B_SPLINE_SURFACE(5,1,((#66747,#66748),(#66749,#66750),(#66751,#66752),(#66753,
#66754),(#66755,#66756),(#66757,#66758),(#66759,#66760),(#66761,#66762),
(#66763,#66764),(#66765,#66766),(#66767,#66768),(#66769,#66770),(#66771,
#66772),(#66773,#66774),(#66775,#66776),(#66777,#66778),(#66779,#66780),
(#66781,#66782),(#66783,#66784),(#66785,#66786),(#66787,#66788),(#66789,
#66790),(#66791,#66792),(#66793,#66794),(#66795,#66796),(#66797,#66798),
(#66799,#66800),(#66801,#66802),(#66803,#66804),(#66805,#66806),(#66807,
#66808),(#66809,#66810),(#66811,#66812),(#66813,#66814),(#66815,#66816),
(#66817,#66818),(#66819,#66820),(#66821,#66822),(#66823,#66824),(#66825,
#66826),(#66827,#66828),(#66829,#66830),(#66831,#66832),(#66833,#66834),
(#66835,#66836),(#66837,#66838),(#66839,#66840),(#66841,#66842),(#66843,
#66844),(#66845,#66846),(#66847,#66848),(#66849,#66850),(#66851,#66852),
(#66853,#66854),(#66855,#66856),(#66857,#66858),(#66859,#66860),(#66861,
#66862),(#66863,#66864),(#66865,#66866),(#66867,#66868),(#66869,#66870),
(#66871,#66872),(#66873,#66874),(#66875,#66876),(#66877,#66878),(#66879,
#66880),(#66881,#66882),(#66883,#66884),(#66885,#66886)),.UNSPECIFIED.,
 .F.,.F.,.F.)
B_SPLINE_SURFACE_WITH_KNOTS((6,1,1,1,1,1,1,1,1,1,1,1,1,1,1,1,1,1,1,1,1,
1,1,1,1,1,1,1,1,1,1,1,1,1,1,1,1,1,1,1,1,1,1,1,1,1,1,1,1,1,1,1,1,1,1,1,1,
1,1,1,1,1,1,1,1,6),(2,2),(-1.,-0.984615384615383,-0.969230769230768,-0.953846153846152,
-0.938461538461537,-0.923076923076922,-0.907692307692306,-0.892307692307691,
-0.876923076923076,-0.86153846153846,-0.846153846153845,-0.83076923076923,
-0.815384615384614,-0.799999999999999,-0.784615384615384,-0.769230769230768,
-0.753846153846153,-0.738461538461538,-0.723076923076922,-0.707692307692307,
-0.692307692307692,-0.676923076923076,-0.661538461538461,-0.646153846153846,
-0.63076923076923,-0.615384615384615,-0.6,-0.584615384615384,-0.569230769230769,
-0.553846153846154,-0.538461538461538,-0.523076923076923,-0.507692307692308,
-0.492307692307692,-0.476923076923077,-0.461538461538462,-0.446153846153846,
-0.430769230769231,-0.415384615384615,-0.4,-0.384615384615385,-0.369230769230769,
-0.353846153846154,-0.338461538461538,-0.323076923076923,-0.307692307692308,
-0.292307692307692,-0.276923076923077,-0.261538461538462,-0.246153846153846,
-0.230769230769231,-0.215384615384615,-0.2,-0.184615384615385,-0.169230769230769,
-0.153846153846154,-0.138461538461538,-0.123076923076923,-0.107692307692308,
-0.0923076923076923,-0.0769230769230769,-0.0615384615384615,-0.0461538461538462,
-0.0307692307692308,-0.0153846153846154,0.),(-1.,1.),.UNSPECIFIED.)
GEOMETRIC_REPRESENTATION_ITEM()
RATIONAL_B_SPLINE_SURFACE(((1.,1.),(1.,1.),(1.,1.),(1.,1.),(1.,1.),(1.,
1.),(1.,1.),(1.,1.),(1.,1.),(1.,1.),(1.,1.),(1.,1.),(1.,1.),(1.,1.),(1.,
1.),(1.,1.),(1.,1.),(1.,1.),(1.,1.),(1.,1.),(1.,1.),(1.,1.),(1.,1.),(1.,
1.),(1.,1.),(1.,1.),(1.,1.),(1.,1.),(1.,1.),(1.,1.),(1.,1.),(1.,1.),(1.,
1.),(1.,1.),(1.,1.),(1.,1.),(1.,1.),(1.,1.),(1.,1.),(1.,1.),(1.,1.),(1.,
1.),(1.,1.),(1.,1.),(1.,1.),(1.,1.),(1.,1.),(1.,1.),(1.,1.),(1.,1.),(1.,
1.),(1.,1.),(1.,1.),(1.,1.),(1.,1.),(1.,1.),(1.,1.),(1.,1.),(1.,1.),(1.,
1.),(1.,1.),(1.,1.),(1.,1.),(1.,1.),(1.,1.),(1.,1.),(1.,1.),(1.,1.),(1.,
1.),(1.,1.)))
REPRESENTATION_ITEM('')
SURFACE()
);
#143=(
BOUNDED_SURFACE()
B_SPLINE_SURFACE(5,1,((#66977,#66978),(#66979,#66980),(#66981,#66982),(#66983,
#66984),(#66985,#66986),(#66987,#66988),(#66989,#66990),(#66991,#66992),
(#66993,#66994),(#66995,#66996),(#66997,#66998),(#66999,#67000),(#67001,
#67002),(#67003,#67004),(#67005,#67006),(#67007,#67008),(#67009,#67010),
(#67011,#67012),(#67013,#67014),(#67015,#67016),(#67017,#67018),(#67019,
#67020),(#67021,#67022),(#67023,#67024),(#67025,#67026),(#67027,#67028),
(#67029,#67030),(#67031,#67032),(#67033,#67034),(#67035,#67036),(#67037,
#67038),(#67039,#67040),(#67041,#67042),(#67043,#67044),(#67045,#67046),
(#67047,#67048),(#67049,#67050),(#67051,#67052),(#67053,#67054),(#67055,
#67056),(#67057,#67058),(#67059,#67060),(#67061,#67062),(#67063,#67064),
(#67065,#67066),(#67067,#67068),(#67069,#67070),(#67071,#67072),(#67073,
#67074),(#67075,#67076),(#67077,#67078),(#67079,#67080),(#67081,#67082),
(#67083,#67084),(#67085,#67086),(#67087,#67088),(#67089,#67090),(#67091,
#67092),(#67093,#67094),(#67095,#67096),(#67097,#67098),(#67099,#67100),
(#67101,#67102),(#67103,#67104),(#67105,#67106),(#67107,#67108),(#67109,
#67110),(#67111,#67112),(#67113,#67114),(#67115,#67116)),.UNSPECIFIED.,
 .F.,.F.,.F.)
B_SPLINE_SURFACE_WITH_KNOTS((6,1,1,1,1,1,1,1,1,1,1,1,1,1,1,1,1,1,1,1,1,
1,1,1,1,1,1,1,1,1,1,1,1,1,1,1,1,1,1,1,1,1,1,1,1,1,1,1,1,1,1,1,1,1,1,1,1,
1,1,1,1,1,1,1,1,6),(2,2),(-1.,-0.984615384615383,-0.969230769230768,-0.953846153846152,
-0.938461538461537,-0.923076923076922,-0.907692307692306,-0.892307692307691,
-0.876923076923076,-0.86153846153846,-0.846153846153845,-0.83076923076923,
-0.815384615384614,-0.799999999999999,-0.784615384615384,-0.769230769230768,
-0.753846153846153,-0.738461538461538,-0.723076923076922,-0.707692307692307,
-0.692307692307692,-0.676923076923076,-0.661538461538461,-0.646153846153846,
-0.63076923076923,-0.615384615384615,-0.6,-0.584615384615384,-0.569230769230769,
-0.553846153846154,-0.538461538461538,-0.523076923076923,-0.507692307692308,
-0.492307692307692,-0.476923076923077,-0.461538461538462,-0.446153846153846,
-0.430769230769231,-0.415384615384615,-0.4,-0.384615384615385,-0.369230769230769,
-0.353846153846154,-0.338461538461538,-0.323076923076923,-0.307692307692308,
-0.292307692307692,-0.276923076923077,-0.261538461538462,-0.246153846153846,
-0.230769230769231,-0.215384615384615,-0.2,-0.184615384615385,-0.169230769230769,
-0.153846153846154,-0.138461538461538,-0.123076923076923,-0.107692307692308,
-0.0923076923076923,-0.0769230769230769,-0.0615384615384615,-0.0461538461538462,
-0.0307692307692308,-0.0153846153846154,0.),(-1.,1.),.UNSPECIFIED.)
GEOMETRIC_REPRESENTATION_ITEM()
RATIONAL_B_SPLINE_SURFACE(((1.,1.),(1.,1.),(1.,1.),(1.,1.),(1.,1.),(1.,
1.),(1.,1.),(1.,1.),(1.,1.),(1.,1.),(1.,1.),(1.,1.),(1.,1.),(1.,1.),(1.,
1.),(1.,1.),(1.,1.),(1.,1.),(1.,1.),(1.,1.),(1.,1.),(1.,1.),(1.,1.),(1.,
1.),(1.,1.),(1.,1.),(1.,1.),(1.,1.),(1.,1.),(1.,1.),(1.,1.),(1.,1.),(1.,
1.),(1.,1.),(1.,1.),(1.,1.),(1.,1.),(1.,1.),(1.,1.),(1.,1.),(1.,1.),(1.,
1.),(1.,1.),(1.,1.),(1.,1.),(1.,1.),(1.,1.),(1.,1.),(1.,1.),(1.,1.),(1.,
1.),(1.,1.),(1.,1.),(1.,1.),(1.,1.),(1.,1.),(1.,1.),(1.,1.),(1.,1.),(1.,
1.),(1.,1.),(1.,1.),(1.,1.),(1.,1.),(1.,1.),(1.,1.),(1.,1.),(1.,1.),(1.,
1.),(1.,1.)))
REPRESENTATION_ITEM('')
SURFACE()
);
#144=(
BOUNDED_SURFACE()
B_SPLINE_SURFACE(5,1,((#67189,#67190),(#67191,#67192),(#67193,#67194),(#67195,
#67196),(#67197,#67198),(#67199,#67200),(#67201,#67202),(#67203,#67204),
(#67205,#67206),(#67207,#67208),(#67209,#67210),(#67211,#67212),(#67213,
#67214),(#67215,#67216),(#67217,#67218),(#67219,#67220),(#67221,#67222),
(#67223,#67224),(#67225,#67226),(#67227,#67228),(#67229,#67230),(#67231,
#67232),(#67233,#67234),(#67235,#67236),(#67237,#67238),(#67239,#67240),
(#67241,#67242),(#67243,#67244),(#67245,#67246),(#67247,#67248),(#67249,
#67250),(#67251,#67252),(#67253,#67254),(#67255,#67256),(#67257,#67258),
(#67259,#67260),(#67261,#67262),(#67263,#67264),(#67265,#67266),(#67267,
#67268),(#67269,#67270),(#67271,#67272),(#67273,#67274),(#67275,#67276),
(#67277,#67278),(#67279,#67280),(#67281,#67282),(#67283,#67284),(#67285,
#67286),(#67287,#67288),(#67289,#67290),(#67291,#67292),(#67293,#67294),
(#67295,#67296),(#67297,#67298),(#67299,#67300),(#67301,#67302),(#67303,
#67304),(#67305,#67306),(#67307,#67308),(#67309,#67310),(#67311,#67312),
(#67313,#67314),(#67315,#67316),(#67317,#67318),(#67319,#67320),(#67321,
#67322),(#67323,#67324),(#67325,#67326),(#67327,#67328)),.UNSPECIFIED.,
 .F.,.F.,.F.)
B_SPLINE_SURFACE_WITH_KNOTS((6,1,1,1,1,1,1,1,1,1,1,1,1,1,1,1,1,1,1,1,1,
1,1,1,1,1,1,1,1,1,1,1,1,1,1,1,1,1,1,1,1,1,1,1,1,1,1,1,1,1,1,1,1,1,1,1,1,
1,1,1,1,1,1,1,1,6),(2,2),(-1.,-0.984615384615383,-0.969230769230768,-0.953846153846152,
-0.938461538461537,-0.923076923076922,-0.907692307692306,-0.892307692307691,
-0.876923076923076,-0.86153846153846,-0.846153846153845,-0.83076923076923,
-0.815384615384614,-0.799999999999999,-0.784615384615384,-0.769230769230768,
-0.753846153846153,-0.738461538461538,-0.723076923076922,-0.707692307692307,
-0.692307692307692,-0.676923076923076,-0.661538461538461,-0.646153846153846,
-0.63076923076923,-0.615384615384615,-0.6,-0.584615384615384,-0.569230769230769,
-0.553846153846154,-0.538461538461538,-0.523076923076923,-0.507692307692308,
-0.492307692307692,-0.476923076923077,-0.461538461538462,-0.446153846153846,
-0.430769230769231,-0.415384615384615,-0.4,-0.384615384615385,-0.369230769230769,
-0.353846153846154,-0.338461538461538,-0.323076923076923,-0.307692307692308,
-0.292307692307692,-0.276923076923077,-0.261538461538462,-0.246153846153846,
-0.230769230769231,-0.215384615384615,-0.2,-0.184615384615385,-0.169230769230769,
-0.153846153846154,-0.138461538461538,-0.123076923076923,-0.107692307692308,
-0.0923076923076923,-0.0769230769230769,-0.0615384615384615,-0.0461538461538462,
-0.0307692307692308,-0.0153846153846154,0.),(-1.,1.),.UNSPECIFIED.)
GEOMETRIC_REPRESENTATION_ITEM()
RATIONAL_B_SPLINE_SURFACE(((1.,1.),(1.,1.),(1.,1.),(1.,1.),(1.,1.),(1.,
1.),(1.,1.),(1.,1.),(1.,1.),(1.,1.),(1.,1.),(1.,1.),(1.,1.),(1.,1.),(1.,
1.),(1.,1.),(1.,1.),(1.,1.),(1.,1.),(1.,1.),(1.,1.),(1.,1.),(1.,1.),(1.,
1.),(1.,1.),(1.,1.),(1.,1.),(1.,1.),(1.,1.),(1.,1.),(1.,1.),(1.,1.),(1.,
1.),(1.,1.),(1.,1.),(1.,1.),(1.,1.),(1.,1.),(1.,1.),(1.,1.),(1.,1.),(1.,
1.),(1.,1.),(1.,1.),(1.,1.),(1.,1.),(1.,1.),(1.,1.),(1.,1.),(1.,1.),(1.,
1.),(1.,1.),(1.,1.),(1.,1.),(1.,1.),(1.,1.),(1.,1.),(1.,1.),(1.,1.),(1.,
1.),(1.,1.),(1.,1.),(1.,1.),(1.,1.),(1.,1.),(1.,1.),(1.,1.),(1.,1.),(1.,
1.),(1.,1.)))
REPRESENTATION_ITEM('')
SURFACE()
);
#145=(
BOUNDED_SURFACE()
B_SPLINE_SURFACE(5,1,((#67419,#67420),(#67421,#67422),(#67423,#67424),(#67425,
#67426),(#67427,#67428),(#67429,#67430),(#67431,#67432),(#67433,#67434),
(#67435,#67436),(#67437,#67438),(#67439,#67440),(#67441,#67442),(#67443,
#67444),(#67445,#67446),(#67447,#67448),(#67449,#67450),(#67451,#67452),
(#67453,#67454),(#67455,#67456),(#67457,#67458),(#67459,#67460),(#67461,
#67462),(#67463,#67464),(#67465,#67466),(#67467,#67468),(#67469,#67470),
(#67471,#67472),(#67473,#67474),(#67475,#67476),(#67477,#67478),(#67479,
#67480),(#67481,#67482),(#67483,#67484),(#67485,#67486),(#67487,#67488),
(#67489,#67490),(#67491,#67492),(#67493,#67494),(#67495,#67496),(#67497,
#67498),(#67499,#67500),(#67501,#67502),(#67503,#67504),(#67505,#67506),
(#67507,#67508),(#67509,#67510),(#67511,#67512),(#67513,#67514),(#67515,
#67516),(#67517,#67518),(#67519,#67520),(#67521,#67522),(#67523,#67524),
(#67525,#67526),(#67527,#67528),(#67529,#67530),(#67531,#67532),(#67533,
#67534),(#67535,#67536),(#67537,#67538),(#67539,#67540),(#67541,#67542),
(#67543,#67544),(#67545,#67546),(#67547,#67548),(#67549,#67550),(#67551,
#67552),(#67553,#67554),(#67555,#67556),(#67557,#67558)),.UNSPECIFIED.,
 .F.,.F.,.F.)
B_SPLINE_SURFACE_WITH_KNOTS((6,1,1,1,1,1,1,1,1,1,1,1,1,1,1,1,1,1,1,1,1,
1,1,1,1,1,1,1,1,1,1,1,1,1,1,1,1,1,1,1,1,1,1,1,1,1,1,1,1,1,1,1,1,1,1,1,1,
1,1,1,1,1,1,1,1,6),(2,2),(-1.,-0.984615384615383,-0.969230769230768,-0.953846153846152,
-0.938461538461537,-0.923076923076922,-0.907692307692306,-0.892307692307691,
-0.876923076923076,-0.86153846153846,-0.846153846153845,-0.83076923076923,
-0.815384615384614,-0.799999999999999,-0.784615384615384,-0.769230769230768,
-0.753846153846153,-0.738461538461538,-0.723076923076922,-0.707692307692307,
-0.692307692307692,-0.676923076923076,-0.661538461538461,-0.646153846153846,
-0.63076923076923,-0.615384615384615,-0.6,-0.584615384615384,-0.569230769230769,
-0.553846153846154,-0.538461538461538,-0.523076923076923,-0.507692307692308,
-0.492307692307692,-0.476923076923077,-0.461538461538462,-0.446153846153846,
-0.430769230769231,-0.415384615384615,-0.4,-0.384615384615385,-0.369230769230769,
-0.353846153846154,-0.338461538461538,-0.323076923076923,-0.307692307692308,
-0.292307692307692,-0.276923076923077,-0.261538461538462,-0.246153846153846,
-0.230769230769231,-0.215384615384615,-0.2,-0.184615384615385,-0.169230769230769,
-0.153846153846154,-0.138461538461538,-0.123076923076923,-0.107692307692308,
-0.0923076923076923,-0.0769230769230769,-0.0615384615384615,-0.0461538461538462,
-0.0307692307692308,-0.0153846153846154,0.),(-1.,1.),.UNSPECIFIED.)
GEOMETRIC_REPRESENTATION_ITEM()
RATIONAL_B_SPLINE_SURFACE(((1.,1.),(1.,1.),(1.,1.),(1.,1.),(1.,1.),(1.,
1.),(1.,1.),(1.,1.),(1.,1.),(1.,1.),(1.,1.),(1.,1.),(1.,1.),(1.,1.),(1.,
1.),(1.,1.),(1.,1.),(1.,1.),(1.,1.),(1.,1.),(1.,1.),(1.,1.),(1.,1.),(1.,
1.),(1.,1.),(1.,1.),(1.,1.),(1.,1.),(1.,1.),(1.,1.),(1.,1.),(1.,1.),(1.,
1.),(1.,1.),(1.,1.),(1.,1.),(1.,1.),(1.,1.),(1.,1.),(1.,1.),(1.,1.),(1.,
1.),(1.,1.),(1.,1.),(1.,1.),(1.,1.),(1.,1.),(1.,1.),(1.,1.),(1.,1.),(1.,
1.),(1.,1.),(1.,1.),(1.,1.),(1.,1.),(1.,1.),(1.,1.),(1.,1.),(1.,1.),(1.,
1.),(1.,1.),(1.,1.),(1.,1.),(1.,1.),(1.,1.),(1.,1.),(1.,1.),(1.,1.),(1.,
1.),(1.,1.)))
REPRESENTATION_ITEM('')
SURFACE()
);
#146=(
BOUNDED_SURFACE()
B_SPLINE_SURFACE(5,1,((#67631,#67632),(#67633,#67634),(#67635,#67636),(#67637,
#67638),(#67639,#67640),(#67641,#67642),(#67643,#67644),(#67645,#67646),
(#67647,#67648),(#67649,#67650),(#67651,#67652),(#67653,#67654),(#67655,
#67656),(#67657,#67658),(#67659,#67660),(#67661,#67662),(#67663,#67664),
(#67665,#67666),(#67667,#67668),(#67669,#67670),(#67671,#67672),(#67673,
#67674),(#67675,#67676),(#67677,#67678),(#67679,#67680),(#67681,#67682),
(#67683,#67684),(#67685,#67686),(#67687,#67688),(#67689,#67690),(#67691,
#67692),(#67693,#67694),(#67695,#67696),(#67697,#67698),(#67699,#67700),
(#67701,#67702),(#67703,#67704),(#67705,#67706),(#67707,#67708),(#67709,
#67710),(#67711,#67712),(#67713,#67714),(#67715,#67716),(#67717,#67718),
(#67719,#67720),(#67721,#67722),(#67723,#67724),(#67725,#67726),(#67727,
#67728),(#67729,#67730),(#67731,#67732),(#67733,#67734),(#67735,#67736),
(#67737,#67738),(#67739,#67740),(#67741,#67742),(#67743,#67744),(#67745,
#67746),(#67747,#67748),(#67749,#67750),(#67751,#67752),(#67753,#67754),
(#67755,#67756),(#67757,#67758),(#67759,#67760),(#67761,#67762),(#67763,
#67764),(#67765,#67766),(#67767,#67768),(#67769,#67770)),.UNSPECIFIED.,
 .F.,.F.,.F.)
B_SPLINE_SURFACE_WITH_KNOTS((6,1,1,1,1,1,1,1,1,1,1,1,1,1,1,1,1,1,1,1,1,
1,1,1,1,1,1,1,1,1,1,1,1,1,1,1,1,1,1,1,1,1,1,1,1,1,1,1,1,1,1,1,1,1,1,1,1,
1,1,1,1,1,1,1,1,6),(2,2),(-1.,-0.984615384615383,-0.969230769230768,-0.953846153846152,
-0.938461538461537,-0.923076923076922,-0.907692307692306,-0.892307692307691,
-0.876923076923076,-0.86153846153846,-0.846153846153845,-0.83076923076923,
-0.815384615384614,-0.799999999999999,-0.784615384615384,-0.769230769230768,
-0.753846153846153,-0.738461538461538,-0.723076923076922,-0.707692307692307,
-0.692307692307692,-0.676923076923076,-0.661538461538461,-0.646153846153846,
-0.63076923076923,-0.615384615384615,-0.6,-0.584615384615384,-0.569230769230769,
-0.553846153846154,-0.538461538461538,-0.523076923076923,-0.507692307692308,
-0.492307692307692,-0.476923076923077,-0.461538461538462,-0.446153846153846,
-0.430769230769231,-0.415384615384615,-0.4,-0.384615384615385,-0.369230769230769,
-0.353846153846154,-0.338461538461538,-0.323076923076923,-0.307692307692308,
-0.292307692307692,-0.276923076923077,-0.261538461538462,-0.246153846153846,
-0.230769230769231,-0.215384615384615,-0.2,-0.184615384615385,-0.169230769230769,
-0.153846153846154,-0.138461538461538,-0.123076923076923,-0.107692307692308,
-0.0923076923076923,-0.0769230769230769,-0.0615384615384615,-0.0461538461538462,
-0.0307692307692308,-0.0153846153846154,0.),(-1.,1.),.UNSPECIFIED.)
GEOMETRIC_REPRESENTATION_ITEM()
RATIONAL_B_SPLINE_SURFACE(((1.,1.),(1.,1.),(1.,1.),(1.,1.),(1.,1.),(1.,
1.),(1.,1.),(1.,1.),(1.,1.),(1.,1.),(1.,1.),(1.,1.),(1.,1.),(1.,1.),(1.,
1.),(1.,1.),(1.,1.),(1.,1.),(1.,1.),(1.,1.),(1.,1.),(1.,1.),(1.,1.),(1.,
1.),(1.,1.),(1.,1.),(1.,1.),(1.,1.),(1.,1.),(1.,1.),(1.,1.),(1.,1.),(1.,
1.),(1.,1.),(1.,1.),(1.,1.),(1.,1.),(1.,1.),(1.,1.),(1.,1.),(1.,1.),(1.,
1.),(1.,1.),(1.,1.),(1.,1.),(1.,1.),(1.,1.),(1.,1.),(1.,1.),(1.,1.),(1.,
1.),(1.,1.),(1.,1.),(1.,1.),(1.,1.),(1.,1.),(1.,1.),(1.,1.),(1.,1.),(1.,
1.),(1.,1.),(1.,1.),(1.,1.),(1.,1.),(1.,1.),(1.,1.),(1.,1.),(1.,1.),(1.,
1.),(1.,1.)))
REPRESENTATION_ITEM('')
SURFACE()
);
#147=(
BOUNDED_SURFACE()
B_SPLINE_SURFACE(5,1,((#67861,#67862),(#67863,#67864),(#67865,#67866),(#67867,
#67868),(#67869,#67870),(#67871,#67872),(#67873,#67874),(#67875,#67876),
(#67877,#67878),(#67879,#67880),(#67881,#67882),(#67883,#67884),(#67885,
#67886),(#67887,#67888),(#67889,#67890),(#67891,#67892),(#67893,#67894),
(#67895,#67896),(#67897,#67898),(#67899,#67900),(#67901,#67902),(#67903,
#67904),(#67905,#67906),(#67907,#67908),(#67909,#67910),(#67911,#67912),
(#67913,#67914),(#67915,#67916),(#67917,#67918),(#67919,#67920),(#67921,
#67922),(#67923,#67924),(#67925,#67926),(#67927,#67928),(#67929,#67930),
(#67931,#67932),(#67933,#67934),(#67935,#67936),(#67937,#67938),(#67939,
#67940),(#67941,#67942),(#67943,#67944),(#67945,#67946),(#67947,#67948),
(#67949,#67950),(#67951,#67952),(#67953,#67954),(#67955,#67956),(#67957,
#67958),(#67959,#67960),(#67961,#67962),(#67963,#67964),(#67965,#67966),
(#67967,#67968),(#67969,#67970),(#67971,#67972),(#67973,#67974),(#67975,
#67976),(#67977,#67978),(#67979,#67980),(#67981,#67982),(#67983,#67984),
(#67985,#67986),(#67987,#67988),(#67989,#67990),(#67991,#67992),(#67993,
#67994),(#67995,#67996),(#67997,#67998),(#67999,#68000)),.UNSPECIFIED.,
 .F.,.F.,.F.)
B_SPLINE_SURFACE_WITH_KNOTS((6,1,1,1,1,1,1,1,1,1,1,1,1,1,1,1,1,1,1,1,1,
1,1,1,1,1,1,1,1,1,1,1,1,1,1,1,1,1,1,1,1,1,1,1,1,1,1,1,1,1,1,1,1,1,1,1,1,
1,1,1,1,1,1,1,1,6),(2,2),(-1.,-0.984615384615383,-0.969230769230768,-0.953846153846152,
-0.938461538461537,-0.923076923076922,-0.907692307692306,-0.892307692307691,
-0.876923076923076,-0.86153846153846,-0.846153846153845,-0.83076923076923,
-0.815384615384614,-0.799999999999999,-0.784615384615384,-0.769230769230768,
-0.753846153846153,-0.738461538461538,-0.723076923076922,-0.707692307692307,
-0.692307692307692,-0.676923076923076,-0.661538461538461,-0.646153846153846,
-0.63076923076923,-0.615384615384615,-0.6,-0.584615384615384,-0.569230769230769,
-0.553846153846154,-0.538461538461538,-0.523076923076923,-0.507692307692308,
-0.492307692307692,-0.476923076923077,-0.461538461538462,-0.446153846153846,
-0.430769230769231,-0.415384615384615,-0.4,-0.384615384615385,-0.369230769230769,
-0.353846153846154,-0.338461538461538,-0.323076923076923,-0.307692307692308,
-0.292307692307692,-0.276923076923077,-0.261538461538462,-0.246153846153846,
-0.230769230769231,-0.215384615384615,-0.2,-0.184615384615385,-0.169230769230769,
-0.153846153846154,-0.138461538461538,-0.123076923076923,-0.107692307692308,
-0.0923076923076923,-0.0769230769230769,-0.0615384615384615,-0.0461538461538462,
-0.0307692307692308,-0.0153846153846154,0.),(-1.,1.),.UNSPECIFIED.)
GEOMETRIC_REPRESENTATION_ITEM()
RATIONAL_B_SPLINE_SURFACE(((1.,1.),(1.,1.),(1.,1.),(1.,1.),(1.,1.),(1.,
1.),(1.,1.),(1.,1.),(1.,1.),(1.,1.),(1.,1.),(1.,1.),(1.,1.),(1.,1.),(1.,
1.),(1.,1.),(1.,1.),(1.,1.),(1.,1.),(1.,1.),(1.,1.),(1.,1.),(1.,1.),(1.,
1.),(1.,1.),(1.,1.),(1.,1.),(1.,1.),(1.,1.),(1.,1.),(1.,1.),(1.,1.),(1.,
1.),(1.,1.),(1.,1.),(1.,1.),(1.,1.),(1.,1.),(1.,1.),(1.,1.),(1.,1.),(1.,
1.),(1.,1.),(1.,1.),(1.,1.),(1.,1.),(1.,1.),(1.,1.),(1.,1.),(1.,1.),(1.,
1.),(1.,1.),(1.,1.),(1.,1.),(1.,1.),(1.,1.),(1.,1.),(1.,1.),(1.,1.),(1.,
1.),(1.,1.),(1.,1.),(1.,1.),(1.,1.),(1.,1.),(1.,1.),(1.,1.),(1.,1.),(1.,
1.),(1.,1.)))
REPRESENTATION_ITEM('')
SURFACE()
);
#148=(
BOUNDED_SURFACE()
B_SPLINE_SURFACE(5,1,((#68073,#68074),(#68075,#68076),(#68077,#68078),(#68079,
#68080),(#68081,#68082),(#68083,#68084),(#68085,#68086),(#68087,#68088),
(#68089,#68090),(#68091,#68092),(#68093,#68094),(#68095,#68096),(#68097,
#68098),(#68099,#68100),(#68101,#68102),(#68103,#68104),(#68105,#68106),
(#68107,#68108),(#68109,#68110),(#68111,#68112),(#68113,#68114),(#68115,
#68116),(#68117,#68118),(#68119,#68120),(#68121,#68122),(#68123,#68124),
(#68125,#68126),(#68127,#68128),(#68129,#68130),(#68131,#68132),(#68133,
#68134),(#68135,#68136),(#68137,#68138),(#68139,#68140),(#68141,#68142),
(#68143,#68144),(#68145,#68146),(#68147,#68148),(#68149,#68150),(#68151,
#68152),(#68153,#68154),(#68155,#68156),(#68157,#68158),(#68159,#68160),
(#68161,#68162),(#68163,#68164),(#68165,#68166),(#68167,#68168),(#68169,
#68170),(#68171,#68172),(#68173,#68174),(#68175,#68176),(#68177,#68178),
(#68179,#68180),(#68181,#68182),(#68183,#68184),(#68185,#68186),(#68187,
#68188),(#68189,#68190),(#68191,#68192),(#68193,#68194),(#68195,#68196),
(#68197,#68198),(#68199,#68200),(#68201,#68202),(#68203,#68204),(#68205,
#68206),(#68207,#68208),(#68209,#68210),(#68211,#68212)),.UNSPECIFIED.,
 .F.,.F.,.F.)
B_SPLINE_SURFACE_WITH_KNOTS((6,1,1,1,1,1,1,1,1,1,1,1,1,1,1,1,1,1,1,1,1,
1,1,1,1,1,1,1,1,1,1,1,1,1,1,1,1,1,1,1,1,1,1,1,1,1,1,1,1,1,1,1,1,1,1,1,1,
1,1,1,1,1,1,1,1,6),(2,2),(-1.,-0.984615384615383,-0.969230769230768,-0.953846153846152,
-0.938461538461537,-0.923076923076922,-0.907692307692306,-0.892307692307691,
-0.876923076923076,-0.86153846153846,-0.846153846153845,-0.83076923076923,
-0.815384615384614,-0.799999999999999,-0.784615384615384,-0.769230769230768,
-0.753846153846153,-0.738461538461538,-0.723076923076922,-0.707692307692307,
-0.692307692307692,-0.676923076923076,-0.661538461538461,-0.646153846153846,
-0.63076923076923,-0.615384615384615,-0.6,-0.584615384615384,-0.569230769230769,
-0.553846153846154,-0.538461538461538,-0.523076923076923,-0.507692307692308,
-0.492307692307692,-0.476923076923077,-0.461538461538462,-0.446153846153846,
-0.430769230769231,-0.415384615384615,-0.4,-0.384615384615385,-0.369230769230769,
-0.353846153846154,-0.338461538461538,-0.323076923076923,-0.307692307692308,
-0.292307692307692,-0.276923076923077,-0.261538461538462,-0.246153846153846,
-0.230769230769231,-0.215384615384615,-0.2,-0.184615384615385,-0.169230769230769,
-0.153846153846154,-0.138461538461538,-0.123076923076923,-0.107692307692308,
-0.0923076923076923,-0.0769230769230769,-0.0615384615384615,-0.0461538461538462,
-0.0307692307692308,-0.0153846153846154,0.),(-1.,1.),.UNSPECIFIED.)
GEOMETRIC_REPRESENTATION_ITEM()
RATIONAL_B_SPLINE_SURFACE(((1.,1.),(1.,1.),(1.,1.),(1.,1.),(1.,1.),(1.,
1.),(1.,1.),(1.,1.),(1.,1.),(1.,1.),(1.,1.),(1.,1.),(1.,1.),(1.,1.),(1.,
1.),(1.,1.),(1.,1.),(1.,1.),(1.,1.),(1.,1.),(1.,1.),(1.,1.),(1.,1.),(1.,
1.),(1.,1.),(1.,1.),(1.,1.),(1.,1.),(1.,1.),(1.,1.),(1.,1.),(1.,1.),(1.,
1.),(1.,1.),(1.,1.),(1.,1.),(1.,1.),(1.,1.),(1.,1.),(1.,1.),(1.,1.),(1.,
1.),(1.,1.),(1.,1.),(1.,1.),(1.,1.),(1.,1.),(1.,1.),(1.,1.),(1.,1.),(1.,
1.),(1.,1.),(1.,1.),(1.,1.),(1.,1.),(1.,1.),(1.,1.),(1.,1.),(1.,1.),(1.,
1.),(1.,1.),(1.,1.),(1.,1.),(1.,1.),(1.,1.),(1.,1.),(1.,1.),(1.,1.),(1.,
1.),(1.,1.)))
REPRESENTATION_ITEM('')
SURFACE()
);
#149=(
BOUNDED_SURFACE()
B_SPLINE_SURFACE(5,1,((#68303,#68304),(#68305,#68306),(#68307,#68308),(#68309,
#68310),(#68311,#68312),(#68313,#68314),(#68315,#68316),(#68317,#68318),
(#68319,#68320),(#68321,#68322),(#68323,#68324),(#68325,#68326),(#68327,
#68328),(#68329,#68330),(#68331,#68332),(#68333,#68334),(#68335,#68336),
(#68337,#68338),(#68339,#68340),(#68341,#68342),(#68343,#68344),(#68345,
#68346),(#68347,#68348),(#68349,#68350),(#68351,#68352),(#68353,#68354),
(#68355,#68356),(#68357,#68358),(#68359,#68360),(#68361,#68362),(#68363,
#68364),(#68365,#68366),(#68367,#68368),(#68369,#68370),(#68371,#68372),
(#68373,#68374),(#68375,#68376),(#68377,#68378),(#68379,#68380),(#68381,
#68382),(#68383,#68384),(#68385,#68386),(#68387,#68388),(#68389,#68390),
(#68391,#68392),(#68393,#68394),(#68395,#68396),(#68397,#68398),(#68399,
#68400),(#68401,#68402),(#68403,#68404),(#68405,#68406),(#68407,#68408),
(#68409,#68410),(#68411,#68412),(#68413,#68414),(#68415,#68416),(#68417,
#68418),(#68419,#68420),(#68421,#68422),(#68423,#68424),(#68425,#68426),
(#68427,#68428),(#68429,#68430),(#68431,#68432),(#68433,#68434),(#68435,
#68436),(#68437,#68438),(#68439,#68440),(#68441,#68442)),.UNSPECIFIED.,
 .F.,.F.,.F.)
B_SPLINE_SURFACE_WITH_KNOTS((6,1,1,1,1,1,1,1,1,1,1,1,1,1,1,1,1,1,1,1,1,
1,1,1,1,1,1,1,1,1,1,1,1,1,1,1,1,1,1,1,1,1,1,1,1,1,1,1,1,1,1,1,1,1,1,1,1,
1,1,1,1,1,1,1,1,6),(2,2),(-1.,-0.984615384615383,-0.969230769230768,-0.953846153846152,
-0.938461538461537,-0.923076923076922,-0.907692307692306,-0.892307692307691,
-0.876923076923076,-0.86153846153846,-0.846153846153845,-0.83076923076923,
-0.815384615384614,-0.799999999999999,-0.784615384615384,-0.769230769230768,
-0.753846153846153,-0.738461538461538,-0.723076923076922,-0.707692307692307,
-0.692307692307692,-0.676923076923076,-0.661538461538461,-0.646153846153846,
-0.63076923076923,-0.615384615384615,-0.6,-0.584615384615384,-0.569230769230769,
-0.553846153846154,-0.538461538461538,-0.523076923076923,-0.507692307692308,
-0.492307692307692,-0.476923076923077,-0.461538461538462,-0.446153846153846,
-0.430769230769231,-0.415384615384615,-0.4,-0.384615384615385,-0.369230769230769,
-0.353846153846154,-0.338461538461538,-0.323076923076923,-0.307692307692308,
-0.292307692307692,-0.276923076923077,-0.261538461538462,-0.246153846153846,
-0.230769230769231,-0.215384615384615,-0.2,-0.184615384615385,-0.169230769230769,
-0.153846153846154,-0.138461538461538,-0.123076923076923,-0.107692307692308,
-0.0923076923076923,-0.0769230769230769,-0.0615384615384615,-0.0461538461538462,
-0.0307692307692308,-0.0153846153846154,0.),(-1.,1.),.UNSPECIFIED.)
GEOMETRIC_REPRESENTATION_ITEM()
RATIONAL_B_SPLINE_SURFACE(((1.,1.),(1.,1.),(1.,1.),(1.,1.),(1.,1.),(1.,
1.),(1.,1.),(1.,1.),(1.,1.),(1.,1.),(1.,1.),(1.,1.),(1.,1.),(1.,1.),(1.,
1.),(1.,1.),(1.,1.),(1.,1.),(1.,1.),(1.,1.),(1.,1.),(1.,1.),(1.,1.),(1.,
1.),(1.,1.),(1.,1.),(1.,1.),(1.,1.),(1.,1.),(1.,1.),(1.,1.),(1.,1.),(1.,
1.),(1.,1.),(1.,1.),(1.,1.),(1.,1.),(1.,1.),(1.,1.),(1.,1.),(1.,1.),(1.,
1.),(1.,1.),(1.,1.),(1.,1.),(1.,1.),(1.,1.),(1.,1.),(1.,1.),(1.,1.),(1.,
1.),(1.,1.),(1.,1.),(1.,1.),(1.,1.),(1.,1.),(1.,1.),(1.,1.),(1.,1.),(1.,
1.),(1.,1.),(1.,1.),(1.,1.),(1.,1.),(1.,1.),(1.,1.),(1.,1.),(1.,1.),(1.,
1.),(1.,1.)))
REPRESENTATION_ITEM('')
SURFACE()
);
#150=(
BOUNDED_SURFACE()
B_SPLINE_SURFACE(5,1,((#68515,#68516),(#68517,#68518),(#68519,#68520),(#68521,
#68522),(#68523,#68524),(#68525,#68526),(#68527,#68528),(#68529,#68530),
(#68531,#68532),(#68533,#68534),(#68535,#68536),(#68537,#68538),(#68539,
#68540),(#68541,#68542),(#68543,#68544),(#68545,#68546),(#68547,#68548),
(#68549,#68550),(#68551,#68552),(#68553,#68554),(#68555,#68556),(#68557,
#68558),(#68559,#68560),(#68561,#68562),(#68563,#68564),(#68565,#68566),
(#68567,#68568),(#68569,#68570),(#68571,#68572),(#68573,#68574),(#68575,
#68576),(#68577,#68578),(#68579,#68580),(#68581,#68582),(#68583,#68584),
(#68585,#68586),(#68587,#68588),(#68589,#68590),(#68591,#68592),(#68593,
#68594),(#68595,#68596),(#68597,#68598),(#68599,#68600),(#68601,#68602),
(#68603,#68604),(#68605,#68606),(#68607,#68608),(#68609,#68610),(#68611,
#68612),(#68613,#68614),(#68615,#68616),(#68617,#68618),(#68619,#68620),
(#68621,#68622),(#68623,#68624),(#68625,#68626),(#68627,#68628),(#68629,
#68630),(#68631,#68632),(#68633,#68634),(#68635,#68636),(#68637,#68638),
(#68639,#68640),(#68641,#68642),(#68643,#68644),(#68645,#68646),(#68647,
#68648),(#68649,#68650),(#68651,#68652),(#68653,#68654)),.UNSPECIFIED.,
 .F.,.F.,.F.)
B_SPLINE_SURFACE_WITH_KNOTS((6,1,1,1,1,1,1,1,1,1,1,1,1,1,1,1,1,1,1,1,1,
1,1,1,1,1,1,1,1,1,1,1,1,1,1,1,1,1,1,1,1,1,1,1,1,1,1,1,1,1,1,1,1,1,1,1,1,
1,1,1,1,1,1,1,1,6),(2,2),(-1.,-0.984615384615383,-0.969230769230768,-0.953846153846152,
-0.938461538461537,-0.923076923076922,-0.907692307692306,-0.892307692307691,
-0.876923076923076,-0.86153846153846,-0.846153846153845,-0.83076923076923,
-0.815384615384614,-0.799999999999999,-0.784615384615384,-0.769230769230768,
-0.753846153846153,-0.738461538461538,-0.723076923076922,-0.707692307692307,
-0.692307692307692,-0.676923076923076,-0.661538461538461,-0.646153846153846,
-0.63076923076923,-0.615384615384615,-0.6,-0.584615384615384,-0.569230769230769,
-0.553846153846154,-0.538461538461538,-0.523076923076923,-0.507692307692308,
-0.492307692307692,-0.476923076923077,-0.461538461538462,-0.446153846153846,
-0.430769230769231,-0.415384615384615,-0.4,-0.384615384615385,-0.369230769230769,
-0.353846153846154,-0.338461538461538,-0.323076923076923,-0.307692307692308,
-0.292307692307692,-0.276923076923077,-0.261538461538462,-0.246153846153846,
-0.230769230769231,-0.215384615384615,-0.2,-0.184615384615385,-0.169230769230769,
-0.153846153846154,-0.138461538461538,-0.123076923076923,-0.107692307692308,
-0.0923076923076923,-0.0769230769230769,-0.0615384615384615,-0.0461538461538462,
-0.0307692307692308,-0.0153846153846154,0.),(-1.,1.),.UNSPECIFIED.)
GEOMETRIC_REPRESENTATION_ITEM()
RATIONAL_B_SPLINE_SURFACE(((1.,1.),(1.,1.),(1.,1.),(1.,1.),(1.,1.),(1.,
1.),(1.,1.),(1.,1.),(1.,1.),(1.,1.),(1.,1.),(1.,1.),(1.,1.),(1.,1.),(1.,
1.),(1.,1.),(1.,1.),(1.,1.),(1.,1.),(1.,1.),(1.,1.),(1.,1.),(1.,1.),(1.,
1.),(1.,1.),(1.,1.),(1.,1.),(1.,1.),(1.,1.),(1.,1.),(1.,1.),(1.,1.),(1.,
1.),(1.,1.),(1.,1.),(1.,1.),(1.,1.),(1.,1.),(1.,1.),(1.,1.),(1.,1.),(1.,
1.),(1.,1.),(1.,1.),(1.,1.),(1.,1.),(1.,1.),(1.,1.),(1.,1.),(1.,1.),(1.,
1.),(1.,1.),(1.,1.),(1.,1.),(1.,1.),(1.,1.),(1.,1.),(1.,1.),(1.,1.),(1.,
1.),(1.,1.),(1.,1.),(1.,1.),(1.,1.),(1.,1.),(1.,1.),(1.,1.),(1.,1.),(1.,
1.),(1.,1.)))
REPRESENTATION_ITEM('')
SURFACE()
);
#151=(
BOUNDED_SURFACE()
B_SPLINE_SURFACE(5,1,((#68745,#68746),(#68747,#68748),(#68749,#68750),(#68751,
#68752),(#68753,#68754),(#68755,#68756),(#68757,#68758),(#68759,#68760),
(#68761,#68762),(#68763,#68764),(#68765,#68766),(#68767,#68768),(#68769,
#68770),(#68771,#68772),(#68773,#68774),(#68775,#68776),(#68777,#68778),
(#68779,#68780),(#68781,#68782),(#68783,#68784),(#68785,#68786),(#68787,
#68788),(#68789,#68790),(#68791,#68792),(#68793,#68794),(#68795,#68796),
(#68797,#68798),(#68799,#68800),(#68801,#68802),(#68803,#68804),(#68805,
#68806),(#68807,#68808),(#68809,#68810),(#68811,#68812),(#68813,#68814),
(#68815,#68816),(#68817,#68818),(#68819,#68820),(#68821,#68822),(#68823,
#68824),(#68825,#68826),(#68827,#68828),(#68829,#68830),(#68831,#68832),
(#68833,#68834),(#68835,#68836),(#68837,#68838),(#68839,#68840),(#68841,
#68842),(#68843,#68844),(#68845,#68846),(#68847,#68848),(#68849,#68850),
(#68851,#68852),(#68853,#68854),(#68855,#68856),(#68857,#68858),(#68859,
#68860),(#68861,#68862),(#68863,#68864),(#68865,#68866),(#68867,#68868),
(#68869,#68870),(#68871,#68872),(#68873,#68874),(#68875,#68876),(#68877,
#68878),(#68879,#68880),(#68881,#68882),(#68883,#68884)),.UNSPECIFIED.,
 .F.,.F.,.F.)
B_SPLINE_SURFACE_WITH_KNOTS((6,1,1,1,1,1,1,1,1,1,1,1,1,1,1,1,1,1,1,1,1,
1,1,1,1,1,1,1,1,1,1,1,1,1,1,1,1,1,1,1,1,1,1,1,1,1,1,1,1,1,1,1,1,1,1,1,1,
1,1,1,1,1,1,1,1,6),(2,2),(-1.,-0.984615384615383,-0.969230769230768,-0.953846153846152,
-0.938461538461537,-0.923076923076922,-0.907692307692306,-0.892307692307691,
-0.876923076923076,-0.86153846153846,-0.846153846153845,-0.83076923076923,
-0.815384615384614,-0.799999999999999,-0.784615384615384,-0.769230769230768,
-0.753846153846153,-0.738461538461538,-0.723076923076922,-0.707692307692307,
-0.692307692307692,-0.676923076923076,-0.661538461538461,-0.646153846153846,
-0.63076923076923,-0.615384615384615,-0.6,-0.584615384615384,-0.569230769230769,
-0.553846153846154,-0.538461538461538,-0.523076923076923,-0.507692307692308,
-0.492307692307692,-0.476923076923077,-0.461538461538462,-0.446153846153846,
-0.430769230769231,-0.415384615384615,-0.4,-0.384615384615385,-0.369230769230769,
-0.353846153846154,-0.338461538461538,-0.323076923076923,-0.307692307692308,
-0.292307692307692,-0.276923076923077,-0.261538461538462,-0.246153846153846,
-0.230769230769231,-0.215384615384615,-0.2,-0.184615384615385,-0.169230769230769,
-0.153846153846154,-0.138461538461538,-0.123076923076923,-0.107692307692308,
-0.0923076923076923,-0.0769230769230769,-0.0615384615384615,-0.0461538461538462,
-0.0307692307692308,-0.0153846153846154,0.),(-1.,1.),.UNSPECIFIED.)
GEOMETRIC_REPRESENTATION_ITEM()
RATIONAL_B_SPLINE_SURFACE(((1.,1.),(1.,1.),(1.,1.),(1.,1.),(1.,1.),(1.,
1.),(1.,1.),(1.,1.),(1.,1.),(1.,1.),(1.,1.),(1.,1.),(1.,1.),(1.,1.),(1.,
1.),(1.,1.),(1.,1.),(1.,1.),(1.,1.),(1.,1.),(1.,1.),(1.,1.),(1.,1.),(1.,
1.),(1.,1.),(1.,1.),(1.,1.),(1.,1.),(1.,1.),(1.,1.),(1.,1.),(1.,1.),(1.,
1.),(1.,1.),(1.,1.),(1.,1.),(1.,1.),(1.,1.),(1.,1.),(1.,1.),(1.,1.),(1.,
1.),(1.,1.),(1.,1.),(1.,1.),(1.,1.),(1.,1.),(1.,1.),(1.,1.),(1.,1.),(1.,
1.),(1.,1.),(1.,1.),(1.,1.),(1.,1.),(1.,1.),(1.,1.),(1.,1.),(1.,1.),(1.,
1.),(1.,1.),(1.,1.),(1.,1.),(1.,1.),(1.,1.),(1.,1.),(1.,1.),(1.,1.),(1.,
1.),(1.,1.)))
REPRESENTATION_ITEM('')
SURFACE()
);
#152=(
BOUNDED_SURFACE()
B_SPLINE_SURFACE(5,1,((#68957,#68958),(#68959,#68960),(#68961,#68962),(#68963,
#68964),(#68965,#68966),(#68967,#68968),(#68969,#68970),(#68971,#68972),
(#68973,#68974),(#68975,#68976),(#68977,#68978),(#68979,#68980),(#68981,
#68982),(#68983,#68984),(#68985,#68986),(#68987,#68988),(#68989,#68990),
(#68991,#68992),(#68993,#68994),(#68995,#68996),(#68997,#68998),(#68999,
#69000),(#69001,#69002),(#69003,#69004),(#69005,#69006),(#69007,#69008),
(#69009,#69010),(#69011,#69012),(#69013,#69014),(#69015,#69016),(#69017,
#69018),(#69019,#69020),(#69021,#69022),(#69023,#69024),(#69025,#69026),
(#69027,#69028),(#69029,#69030),(#69031,#69032),(#69033,#69034),(#69035,
#69036),(#69037,#69038),(#69039,#69040),(#69041,#69042),(#69043,#69044),
(#69045,#69046),(#69047,#69048),(#69049,#69050),(#69051,#69052),(#69053,
#69054),(#69055,#69056),(#69057,#69058),(#69059,#69060),(#69061,#69062),
(#69063,#69064),(#69065,#69066),(#69067,#69068),(#69069,#69070),(#69071,
#69072),(#69073,#69074),(#69075,#69076),(#69077,#69078),(#69079,#69080),
(#69081,#69082),(#69083,#69084),(#69085,#69086),(#69087,#69088),(#69089,
#69090),(#69091,#69092),(#69093,#69094),(#69095,#69096)),.UNSPECIFIED.,
 .F.,.F.,.F.)
B_SPLINE_SURFACE_WITH_KNOTS((6,1,1,1,1,1,1,1,1,1,1,1,1,1,1,1,1,1,1,1,1,
1,1,1,1,1,1,1,1,1,1,1,1,1,1,1,1,1,1,1,1,1,1,1,1,1,1,1,1,1,1,1,1,1,1,1,1,
1,1,1,1,1,1,1,1,6),(2,2),(-1.,-0.984615384615383,-0.969230769230768,-0.953846153846152,
-0.938461538461537,-0.923076923076922,-0.907692307692306,-0.892307692307691,
-0.876923076923076,-0.86153846153846,-0.846153846153845,-0.83076923076923,
-0.815384615384614,-0.799999999999999,-0.784615384615384,-0.769230769230768,
-0.753846153846153,-0.738461538461538,-0.723076923076922,-0.707692307692307,
-0.692307692307692,-0.676923076923076,-0.661538461538461,-0.646153846153846,
-0.63076923076923,-0.615384615384615,-0.6,-0.584615384615384,-0.569230769230769,
-0.553846153846154,-0.538461538461538,-0.523076923076923,-0.507692307692308,
-0.492307692307692,-0.476923076923077,-0.461538461538462,-0.446153846153846,
-0.430769230769231,-0.415384615384615,-0.4,-0.384615384615385,-0.369230769230769,
-0.353846153846154,-0.338461538461538,-0.323076923076923,-0.307692307692308,
-0.292307692307692,-0.276923076923077,-0.261538461538462,-0.246153846153846,
-0.230769230769231,-0.215384615384615,-0.2,-0.184615384615385,-0.169230769230769,
-0.153846153846154,-0.138461538461538,-0.123076923076923,-0.107692307692308,
-0.0923076923076923,-0.0769230769230769,-0.0615384615384615,-0.0461538461538462,
-0.0307692307692308,-0.0153846153846154,0.),(-1.,1.),.UNSPECIFIED.)
GEOMETRIC_REPRESENTATION_ITEM()
RATIONAL_B_SPLINE_SURFACE(((1.,1.),(1.,1.),(1.,1.),(1.,1.),(1.,1.),(1.,
1.),(1.,1.),(1.,1.),(1.,1.),(1.,1.),(1.,1.),(1.,1.),(1.,1.),(1.,1.),(1.,
1.),(1.,1.),(1.,1.),(1.,1.),(1.,1.),(1.,1.),(1.,1.),(1.,1.),(1.,1.),(1.,
1.),(1.,1.),(1.,1.),(1.,1.),(1.,1.),(1.,1.),(1.,1.),(1.,1.),(1.,1.),(1.,
1.),(1.,1.),(1.,1.),(1.,1.),(1.,1.),(1.,1.),(1.,1.),(1.,1.),(1.,1.),(1.,
1.),(1.,1.),(1.,1.),(1.,1.),(1.,1.),(1.,1.),(1.,1.),(1.,1.),(1.,1.),(1.,
1.),(1.,1.),(1.,1.),(1.,1.),(1.,1.),(1.,1.),(1.,1.),(1.,1.),(1.,1.),(1.,
1.),(1.,1.),(1.,1.),(1.,1.),(1.,1.),(1.,1.),(1.,1.),(1.,1.),(1.,1.),(1.,
1.),(1.,1.)))
REPRESENTATION_ITEM('')
SURFACE()
);
#153=(
BOUNDED_SURFACE()
B_SPLINE_SURFACE(5,1,((#69187,#69188),(#69189,#69190),(#69191,#69192),(#69193,
#69194),(#69195,#69196),(#69197,#69198),(#69199,#69200),(#69201,#69202),
(#69203,#69204),(#69205,#69206),(#69207,#69208),(#69209,#69210),(#69211,
#69212),(#69213,#69214),(#69215,#69216),(#69217,#69218),(#69219,#69220),
(#69221,#69222),(#69223,#69224),(#69225,#69226),(#69227,#69228),(#69229,
#69230),(#69231,#69232),(#69233,#69234),(#69235,#69236),(#69237,#69238),
(#69239,#69240),(#69241,#69242),(#69243,#69244),(#69245,#69246),(#69247,
#69248),(#69249,#69250),(#69251,#69252),(#69253,#69254),(#69255,#69256),
(#69257,#69258),(#69259,#69260),(#69261,#69262),(#69263,#69264),(#69265,
#69266),(#69267,#69268),(#69269,#69270),(#69271,#69272),(#69273,#69274),
(#69275,#69276),(#69277,#69278),(#69279,#69280),(#69281,#69282),(#69283,
#69284),(#69285,#69286),(#69287,#69288),(#69289,#69290),(#69291,#69292),
(#69293,#69294),(#69295,#69296),(#69297,#69298),(#69299,#69300),(#69301,
#69302),(#69303,#69304),(#69305,#69306),(#69307,#69308),(#69309,#69310),
(#69311,#69312),(#69313,#69314),(#69315,#69316),(#69317,#69318),(#69319,
#69320),(#69321,#69322),(#69323,#69324),(#69325,#69326)),.UNSPECIFIED.,
 .F.,.F.,.F.)
B_SPLINE_SURFACE_WITH_KNOTS((6,1,1,1,1,1,1,1,1,1,1,1,1,1,1,1,1,1,1,1,1,
1,1,1,1,1,1,1,1,1,1,1,1,1,1,1,1,1,1,1,1,1,1,1,1,1,1,1,1,1,1,1,1,1,1,1,1,
1,1,1,1,1,1,1,1,6),(2,2),(-1.,-0.984615384615383,-0.969230769230768,-0.953846153846152,
-0.938461538461537,-0.923076923076922,-0.907692307692306,-0.892307692307691,
-0.876923076923076,-0.86153846153846,-0.846153846153845,-0.83076923076923,
-0.815384615384614,-0.799999999999999,-0.784615384615384,-0.769230769230768,
-0.753846153846153,-0.738461538461538,-0.723076923076922,-0.707692307692307,
-0.692307692307692,-0.676923076923076,-0.661538461538461,-0.646153846153846,
-0.63076923076923,-0.615384615384615,-0.6,-0.584615384615384,-0.569230769230769,
-0.553846153846154,-0.538461538461538,-0.523076923076923,-0.507692307692308,
-0.492307692307692,-0.476923076923077,-0.461538461538462,-0.446153846153846,
-0.430769230769231,-0.415384615384615,-0.4,-0.384615384615385,-0.369230769230769,
-0.353846153846154,-0.338461538461538,-0.323076923076923,-0.307692307692308,
-0.292307692307692,-0.276923076923077,-0.261538461538462,-0.246153846153846,
-0.230769230769231,-0.215384615384615,-0.2,-0.184615384615385,-0.169230769230769,
-0.153846153846154,-0.138461538461538,-0.123076923076923,-0.107692307692308,
-0.0923076923076923,-0.0769230769230769,-0.0615384615384615,-0.0461538461538462,
-0.0307692307692308,-0.0153846153846154,0.),(-1.,1.),.UNSPECIFIED.)
GEOMETRIC_REPRESENTATION_ITEM()
RATIONAL_B_SPLINE_SURFACE(((1.,1.),(1.,1.),(1.,1.),(1.,1.),(1.,1.),(1.,
1.),(1.,1.),(1.,1.),(1.,1.),(1.,1.),(1.,1.),(1.,1.),(1.,1.),(1.,1.),(1.,
1.),(1.,1.),(1.,1.),(1.,1.),(1.,1.),(1.,1.),(1.,1.),(1.,1.),(1.,1.),(1.,
1.),(1.,1.),(1.,1.),(1.,1.),(1.,1.),(1.,1.),(1.,1.),(1.,1.),(1.,1.),(1.,
1.),(1.,1.),(1.,1.),(1.,1.),(1.,1.),(1.,1.),(1.,1.),(1.,1.),(1.,1.),(1.,
1.),(1.,1.),(1.,1.),(1.,1.),(1.,1.),(1.,1.),(1.,1.),(1.,1.),(1.,1.),(1.,
1.),(1.,1.),(1.,1.),(1.,1.),(1.,1.),(1.,1.),(1.,1.),(1.,1.),(1.,1.),(1.,
1.),(1.,1.),(1.,1.),(1.,1.),(1.,1.),(1.,1.),(1.,1.),(1.,1.),(1.,1.),(1.,
1.),(1.,1.)))
REPRESENTATION_ITEM('')
SURFACE()
);
#154=(
BOUNDED_SURFACE()
B_SPLINE_SURFACE(5,1,((#69399,#69400),(#69401,#69402),(#69403,#69404),(#69405,
#69406),(#69407,#69408),(#69409,#69410),(#69411,#69412),(#69413,#69414),
(#69415,#69416),(#69417,#69418),(#69419,#69420),(#69421,#69422),(#69423,
#69424),(#69425,#69426),(#69427,#69428),(#69429,#69430),(#69431,#69432),
(#69433,#69434),(#69435,#69436),(#69437,#69438),(#69439,#69440),(#69441,
#69442),(#69443,#69444),(#69445,#69446),(#69447,#69448),(#69449,#69450),
(#69451,#69452),(#69453,#69454),(#69455,#69456),(#69457,#69458),(#69459,
#69460),(#69461,#69462),(#69463,#69464),(#69465,#69466),(#69467,#69468),
(#69469,#69470),(#69471,#69472),(#69473,#69474),(#69475,#69476),(#69477,
#69478),(#69479,#69480),(#69481,#69482),(#69483,#69484),(#69485,#69486),
(#69487,#69488),(#69489,#69490),(#69491,#69492),(#69493,#69494),(#69495,
#69496),(#69497,#69498),(#69499,#69500),(#69501,#69502),(#69503,#69504),
(#69505,#69506),(#69507,#69508),(#69509,#69510),(#69511,#69512),(#69513,
#69514),(#69515,#69516),(#69517,#69518),(#69519,#69520),(#69521,#69522),
(#69523,#69524),(#69525,#69526),(#69527,#69528),(#69529,#69530),(#69531,
#69532),(#69533,#69534),(#69535,#69536),(#69537,#69538)),.UNSPECIFIED.,
 .F.,.F.,.F.)
B_SPLINE_SURFACE_WITH_KNOTS((6,1,1,1,1,1,1,1,1,1,1,1,1,1,1,1,1,1,1,1,1,
1,1,1,1,1,1,1,1,1,1,1,1,1,1,1,1,1,1,1,1,1,1,1,1,1,1,1,1,1,1,1,1,1,1,1,1,
1,1,1,1,1,1,1,1,6),(2,2),(-1.,-0.984615384615383,-0.969230769230768,-0.953846153846152,
-0.938461538461537,-0.923076923076922,-0.907692307692306,-0.892307692307691,
-0.876923076923076,-0.86153846153846,-0.846153846153845,-0.83076923076923,
-0.815384615384614,-0.799999999999999,-0.784615384615384,-0.769230769230768,
-0.753846153846153,-0.738461538461538,-0.723076923076922,-0.707692307692307,
-0.692307692307692,-0.676923076923076,-0.661538461538461,-0.646153846153846,
-0.63076923076923,-0.615384615384615,-0.6,-0.584615384615384,-0.569230769230769,
-0.553846153846154,-0.538461538461538,-0.523076923076923,-0.507692307692308,
-0.492307692307692,-0.476923076923077,-0.461538461538462,-0.446153846153846,
-0.430769230769231,-0.415384615384615,-0.4,-0.384615384615385,-0.369230769230769,
-0.353846153846154,-0.338461538461538,-0.323076923076923,-0.307692307692308,
-0.292307692307692,-0.276923076923077,-0.261538461538462,-0.246153846153846,
-0.230769230769231,-0.215384615384615,-0.2,-0.184615384615385,-0.169230769230769,
-0.153846153846154,-0.138461538461538,-0.123076923076923,-0.107692307692308,
-0.0923076923076923,-0.0769230769230769,-0.0615384615384615,-0.0461538461538462,
-0.0307692307692308,-0.0153846153846154,0.),(-1.,1.),.UNSPECIFIED.)
GEOMETRIC_REPRESENTATION_ITEM()
RATIONAL_B_SPLINE_SURFACE(((1.,1.),(1.,1.),(1.,1.),(1.,1.),(1.,1.),(1.,
1.),(1.,1.),(1.,1.),(1.,1.),(1.,1.),(1.,1.),(1.,1.),(1.,1.),(1.,1.),(1.,
1.),(1.,1.),(1.,1.),(1.,1.),(1.,1.),(1.,1.),(1.,1.),(1.,1.),(1.,1.),(1.,
1.),(1.,1.),(1.,1.),(1.,1.),(1.,1.),(1.,1.),(1.,1.),(1.,1.),(1.,1.),(1.,
1.),(1.,1.),(1.,1.),(1.,1.),(1.,1.),(1.,1.),(1.,1.),(1.,1.),(1.,1.),(1.,
1.),(1.,1.),(1.,1.),(1.,1.),(1.,1.),(1.,1.),(1.,1.),(1.,1.),(1.,1.),(1.,
1.),(1.,1.),(1.,1.),(1.,1.),(1.,1.),(1.,1.),(1.,1.),(1.,1.),(1.,1.),(1.,
1.),(1.,1.),(1.,1.),(1.,1.),(1.,1.),(1.,1.),(1.,1.),(1.,1.),(1.,1.),(1.,
1.),(1.,1.)))
REPRESENTATION_ITEM('')
SURFACE()
);
#155=(
BOUNDED_SURFACE()
B_SPLINE_SURFACE(5,1,((#69629,#69630),(#69631,#69632),(#69633,#69634),(#69635,
#69636),(#69637,#69638),(#69639,#69640),(#69641,#69642),(#69643,#69644),
(#69645,#69646),(#69647,#69648),(#69649,#69650),(#69651,#69652),(#69653,
#69654),(#69655,#69656),(#69657,#69658),(#69659,#69660),(#69661,#69662),
(#69663,#69664),(#69665,#69666),(#69667,#69668),(#69669,#69670),(#69671,
#69672),(#69673,#69674),(#69675,#69676),(#69677,#69678),(#69679,#69680),
(#69681,#69682),(#69683,#69684),(#69685,#69686),(#69687,#69688),(#69689,
#69690),(#69691,#69692),(#69693,#69694),(#69695,#69696),(#69697,#69698),
(#69699,#69700),(#69701,#69702),(#69703,#69704),(#69705,#69706),(#69707,
#69708),(#69709,#69710),(#69711,#69712),(#69713,#69714),(#69715,#69716),
(#69717,#69718),(#69719,#69720),(#69721,#69722),(#69723,#69724),(#69725,
#69726),(#69727,#69728),(#69729,#69730),(#69731,#69732),(#69733,#69734),
(#69735,#69736),(#69737,#69738),(#69739,#69740),(#69741,#69742),(#69743,
#69744),(#69745,#69746),(#69747,#69748),(#69749,#69750),(#69751,#69752),
(#69753,#69754),(#69755,#69756),(#69757,#69758),(#69759,#69760),(#69761,
#69762),(#69763,#69764),(#69765,#69766),(#69767,#69768)),.UNSPECIFIED.,
 .F.,.F.,.F.)
B_SPLINE_SURFACE_WITH_KNOTS((6,1,1,1,1,1,1,1,1,1,1,1,1,1,1,1,1,1,1,1,1,
1,1,1,1,1,1,1,1,1,1,1,1,1,1,1,1,1,1,1,1,1,1,1,1,1,1,1,1,1,1,1,1,1,1,1,1,
1,1,1,1,1,1,1,1,6),(2,2),(-1.,-0.984615384615383,-0.969230769230768,-0.953846153846152,
-0.938461538461537,-0.923076923076922,-0.907692307692306,-0.892307692307691,
-0.876923076923076,-0.86153846153846,-0.846153846153845,-0.83076923076923,
-0.815384615384614,-0.799999999999999,-0.784615384615384,-0.769230769230768,
-0.753846153846153,-0.738461538461538,-0.723076923076922,-0.707692307692307,
-0.692307692307692,-0.676923076923076,-0.661538461538461,-0.646153846153846,
-0.63076923076923,-0.615384615384615,-0.6,-0.584615384615384,-0.569230769230769,
-0.553846153846154,-0.538461538461538,-0.523076923076923,-0.507692307692308,
-0.492307692307692,-0.476923076923077,-0.461538461538462,-0.446153846153846,
-0.430769230769231,-0.415384615384615,-0.4,-0.384615384615385,-0.369230769230769,
-0.353846153846154,-0.338461538461538,-0.323076923076923,-0.307692307692308,
-0.292307692307692,-0.276923076923077,-0.261538461538462,-0.246153846153846,
-0.230769230769231,-0.215384615384615,-0.2,-0.184615384615385,-0.169230769230769,
-0.153846153846154,-0.138461538461538,-0.123076923076923,-0.107692307692308,
-0.0923076923076923,-0.0769230769230769,-0.0615384615384615,-0.0461538461538462,
-0.0307692307692308,-0.0153846153846154,0.),(-1.,1.),.UNSPECIFIED.)
GEOMETRIC_REPRESENTATION_ITEM()
RATIONAL_B_SPLINE_SURFACE(((1.,1.),(1.,1.),(1.,1.),(1.,1.),(1.,1.),(1.,
1.),(1.,1.),(1.,1.),(1.,1.),(1.,1.),(1.,1.),(1.,1.),(1.,1.),(1.,1.),(1.,
1.),(1.,1.),(1.,1.),(1.,1.),(1.,1.),(1.,1.),(1.,1.),(1.,1.),(1.,1.),(1.,
1.),(1.,1.),(1.,1.),(1.,1.),(1.,1.),(1.,1.),(1.,1.),(1.,1.),(1.,1.),(1.,
1.),(1.,1.),(1.,1.),(1.,1.),(1.,1.),(1.,1.),(1.,1.),(1.,1.),(1.,1.),(1.,
1.),(1.,1.),(1.,1.),(1.,1.),(1.,1.),(1.,1.),(1.,1.),(1.,1.),(1.,1.),(1.,
1.),(1.,1.),(1.,1.),(1.,1.),(1.,1.),(1.,1.),(1.,1.),(1.,1.),(1.,1.),(1.,
1.),(1.,1.),(1.,1.),(1.,1.),(1.,1.),(1.,1.),(1.,1.),(1.,1.),(1.,1.),(1.,
1.),(1.,1.)))
REPRESENTATION_ITEM('')
SURFACE()
);
#156=(
BOUNDED_SURFACE()
B_SPLINE_SURFACE(5,1,((#69841,#69842),(#69843,#69844),(#69845,#69846),(#69847,
#69848),(#69849,#69850),(#69851,#69852),(#69853,#69854),(#69855,#69856),
(#69857,#69858),(#69859,#69860),(#69861,#69862),(#69863,#69864),(#69865,
#69866),(#69867,#69868),(#69869,#69870),(#69871,#69872),(#69873,#69874),
(#69875,#69876),(#69877,#69878),(#69879,#69880),(#69881,#69882),(#69883,
#69884),(#69885,#69886),(#69887,#69888),(#69889,#69890),(#69891,#69892),
(#69893,#69894),(#69895,#69896),(#69897,#69898),(#69899,#69900),(#69901,
#69902),(#69903,#69904),(#69905,#69906),(#69907,#69908),(#69909,#69910),
(#69911,#69912),(#69913,#69914),(#69915,#69916),(#69917,#69918),(#69919,
#69920),(#69921,#69922),(#69923,#69924),(#69925,#69926),(#69927,#69928),
(#69929,#69930),(#69931,#69932),(#69933,#69934),(#69935,#69936),(#69937,
#69938),(#69939,#69940),(#69941,#69942),(#69943,#69944),(#69945,#69946),
(#69947,#69948),(#69949,#69950),(#69951,#69952),(#69953,#69954),(#69955,
#69956),(#69957,#69958),(#69959,#69960),(#69961,#69962),(#69963,#69964),
(#69965,#69966),(#69967,#69968),(#69969,#69970),(#69971,#69972),(#69973,
#69974),(#69975,#69976),(#69977,#69978),(#69979,#69980)),.UNSPECIFIED.,
 .F.,.F.,.F.)
B_SPLINE_SURFACE_WITH_KNOTS((6,1,1,1,1,1,1,1,1,1,1,1,1,1,1,1,1,1,1,1,1,
1,1,1,1,1,1,1,1,1,1,1,1,1,1,1,1,1,1,1,1,1,1,1,1,1,1,1,1,1,1,1,1,1,1,1,1,
1,1,1,1,1,1,1,1,6),(2,2),(-1.,-0.984615384615383,-0.969230769230768,-0.953846153846152,
-0.938461538461537,-0.923076923076922,-0.907692307692306,-0.892307692307691,
-0.876923076923076,-0.86153846153846,-0.846153846153845,-0.83076923076923,
-0.815384615384614,-0.799999999999999,-0.784615384615384,-0.769230769230768,
-0.753846153846153,-0.738461538461538,-0.723076923076922,-0.707692307692307,
-0.692307692307692,-0.676923076923076,-0.661538461538461,-0.646153846153846,
-0.63076923076923,-0.615384615384615,-0.6,-0.584615384615384,-0.569230769230769,
-0.553846153846154,-0.538461538461538,-0.523076923076923,-0.507692307692308,
-0.492307692307692,-0.476923076923077,-0.461538461538462,-0.446153846153846,
-0.430769230769231,-0.415384615384615,-0.4,-0.384615384615385,-0.369230769230769,
-0.353846153846154,-0.338461538461538,-0.323076923076923,-0.307692307692308,
-0.292307692307692,-0.276923076923077,-0.261538461538462,-0.246153846153846,
-0.230769230769231,-0.215384615384615,-0.2,-0.184615384615385,-0.169230769230769,
-0.153846153846154,-0.138461538461538,-0.123076923076923,-0.107692307692308,
-0.0923076923076923,-0.0769230769230769,-0.0615384615384615,-0.0461538461538462,
-0.0307692307692308,-0.0153846153846154,0.),(-1.,1.),.UNSPECIFIED.)
GEOMETRIC_REPRESENTATION_ITEM()
RATIONAL_B_SPLINE_SURFACE(((1.,1.),(1.,1.),(1.,1.),(1.,1.),(1.,1.),(1.,
1.),(1.,1.),(1.,1.),(1.,1.),(1.,1.),(1.,1.),(1.,1.),(1.,1.),(1.,1.),(1.,
1.),(1.,1.),(1.,1.),(1.,1.),(1.,1.),(1.,1.),(1.,1.),(1.,1.),(1.,1.),(1.,
1.),(1.,1.),(1.,1.),(1.,1.),(1.,1.),(1.,1.),(1.,1.),(1.,1.),(1.,1.),(1.,
1.),(1.,1.),(1.,1.),(1.,1.),(1.,1.),(1.,1.),(1.,1.),(1.,1.),(1.,1.),(1.,
1.),(1.,1.),(1.,1.),(1.,1.),(1.,1.),(1.,1.),(1.,1.),(1.,1.),(1.,1.),(1.,
1.),(1.,1.),(1.,1.),(1.,1.),(1.,1.),(1.,1.),(1.,1.),(1.,1.),(1.,1.),(1.,
1.),(1.,1.),(1.,1.),(1.,1.),(1.,1.),(1.,1.),(1.,1.),(1.,1.),(1.,1.),(1.,
1.),(1.,1.)))
REPRESENTATION_ITEM('')
SURFACE()
);
#157=(
BOUNDED_SURFACE()
B_SPLINE_SURFACE(5,1,((#70071,#70072),(#70073,#70074),(#70075,#70076),(#70077,
#70078),(#70079,#70080),(#70081,#70082),(#70083,#70084),(#70085,#70086),
(#70087,#70088),(#70089,#70090),(#70091,#70092),(#70093,#70094),(#70095,
#70096),(#70097,#70098),(#70099,#70100),(#70101,#70102),(#70103,#70104),
(#70105,#70106),(#70107,#70108),(#70109,#70110),(#70111,#70112),(#70113,
#70114),(#70115,#70116),(#70117,#70118),(#70119,#70120),(#70121,#70122),
(#70123,#70124),(#70125,#70126),(#70127,#70128),(#70129,#70130),(#70131,
#70132),(#70133,#70134),(#70135,#70136),(#70137,#70138),(#70139,#70140),
(#70141,#70142),(#70143,#70144),(#70145,#70146),(#70147,#70148),(#70149,
#70150),(#70151,#70152),(#70153,#70154),(#70155,#70156),(#70157,#70158),
(#70159,#70160),(#70161,#70162),(#70163,#70164),(#70165,#70166),(#70167,
#70168),(#70169,#70170),(#70171,#70172),(#70173,#70174),(#70175,#70176),
(#70177,#70178),(#70179,#70180),(#70181,#70182),(#70183,#70184),(#70185,
#70186),(#70187,#70188),(#70189,#70190),(#70191,#70192),(#70193,#70194),
(#70195,#70196),(#70197,#70198),(#70199,#70200),(#70201,#70202),(#70203,
#70204),(#70205,#70206),(#70207,#70208),(#70209,#70210)),.UNSPECIFIED.,
 .F.,.F.,.F.)
B_SPLINE_SURFACE_WITH_KNOTS((6,1,1,1,1,1,1,1,1,1,1,1,1,1,1,1,1,1,1,1,1,
1,1,1,1,1,1,1,1,1,1,1,1,1,1,1,1,1,1,1,1,1,1,1,1,1,1,1,1,1,1,1,1,1,1,1,1,
1,1,1,1,1,1,1,1,6),(2,2),(-1.,-0.984615384615383,-0.969230769230768,-0.953846153846152,
-0.938461538461537,-0.923076923076922,-0.907692307692306,-0.892307692307691,
-0.876923076923076,-0.86153846153846,-0.846153846153845,-0.83076923076923,
-0.815384615384614,-0.799999999999999,-0.784615384615384,-0.769230769230768,
-0.753846153846153,-0.738461538461538,-0.723076923076922,-0.707692307692307,
-0.692307692307692,-0.676923076923076,-0.661538461538461,-0.646153846153846,
-0.63076923076923,-0.615384615384615,-0.6,-0.584615384615384,-0.569230769230769,
-0.553846153846154,-0.538461538461538,-0.523076923076923,-0.507692307692308,
-0.492307692307692,-0.476923076923077,-0.461538461538462,-0.446153846153846,
-0.430769230769231,-0.415384615384615,-0.4,-0.384615384615385,-0.369230769230769,
-0.353846153846154,-0.338461538461538,-0.323076923076923,-0.307692307692308,
-0.292307692307692,-0.276923076923077,-0.261538461538462,-0.246153846153846,
-0.230769230769231,-0.215384615384615,-0.2,-0.184615384615385,-0.169230769230769,
-0.153846153846154,-0.138461538461538,-0.123076923076923,-0.107692307692308,
-0.0923076923076923,-0.0769230769230769,-0.0615384615384615,-0.0461538461538462,
-0.0307692307692308,-0.0153846153846154,0.),(-1.,1.),.UNSPECIFIED.)
GEOMETRIC_REPRESENTATION_ITEM()
RATIONAL_B_SPLINE_SURFACE(((1.,1.),(1.,1.),(1.,1.),(1.,1.),(1.,1.),(1.,
1.),(1.,1.),(1.,1.),(1.,1.),(1.,1.),(1.,1.),(1.,1.),(1.,1.),(1.,1.),(1.,
1.),(1.,1.),(1.,1.),(1.,1.),(1.,1.),(1.,1.),(1.,1.),(1.,1.),(1.,1.),(1.,
1.),(1.,1.),(1.,1.),(1.,1.),(1.,1.),(1.,1.),(1.,1.),(1.,1.),(1.,1.),(1.,
1.),(1.,1.),(1.,1.),(1.,1.),(1.,1.),(1.,1.),(1.,1.),(1.,1.),(1.,1.),(1.,
1.),(1.,1.),(1.,1.),(1.,1.),(1.,1.),(1.,1.),(1.,1.),(1.,1.),(1.,1.),(1.,
1.),(1.,1.),(1.,1.),(1.,1.),(1.,1.),(1.,1.),(1.,1.),(1.,1.),(1.,1.),(1.,
1.),(1.,1.),(1.,1.),(1.,1.),(1.,1.),(1.,1.),(1.,1.),(1.,1.),(1.,1.),(1.,
1.),(1.,1.)))
REPRESENTATION_ITEM('')
SURFACE()
);
#158=(
BOUNDED_SURFACE()
B_SPLINE_SURFACE(5,1,((#70283,#70284),(#70285,#70286),(#70287,#70288),(#70289,
#70290),(#70291,#70292),(#70293,#70294),(#70295,#70296),(#70297,#70298),
(#70299,#70300),(#70301,#70302),(#70303,#70304),(#70305,#70306),(#70307,
#70308),(#70309,#70310),(#70311,#70312),(#70313,#70314),(#70315,#70316),
(#70317,#70318),(#70319,#70320),(#70321,#70322),(#70323,#70324),(#70325,
#70326),(#70327,#70328),(#70329,#70330),(#70331,#70332),(#70333,#70334),
(#70335,#70336),(#70337,#70338),(#70339,#70340),(#70341,#70342),(#70343,
#70344),(#70345,#70346),(#70347,#70348),(#70349,#70350),(#70351,#70352),
(#70353,#70354),(#70355,#70356),(#70357,#70358),(#70359,#70360),(#70361,
#70362),(#70363,#70364),(#70365,#70366),(#70367,#70368),(#70369,#70370),
(#70371,#70372),(#70373,#70374),(#70375,#70376),(#70377,#70378),(#70379,
#70380),(#70381,#70382),(#70383,#70384),(#70385,#70386),(#70387,#70388),
(#70389,#70390),(#70391,#70392),(#70393,#70394),(#70395,#70396),(#70397,
#70398),(#70399,#70400),(#70401,#70402),(#70403,#70404),(#70405,#70406),
(#70407,#70408),(#70409,#70410),(#70411,#70412),(#70413,#70414),(#70415,
#70416),(#70417,#70418),(#70419,#70420),(#70421,#70422)),.UNSPECIFIED.,
 .F.,.F.,.F.)
B_SPLINE_SURFACE_WITH_KNOTS((6,1,1,1,1,1,1,1,1,1,1,1,1,1,1,1,1,1,1,1,1,
1,1,1,1,1,1,1,1,1,1,1,1,1,1,1,1,1,1,1,1,1,1,1,1,1,1,1,1,1,1,1,1,1,1,1,1,
1,1,1,1,1,1,1,1,6),(2,2),(-1.,-0.984615384615383,-0.969230769230768,-0.953846153846152,
-0.938461538461537,-0.923076923076922,-0.907692307692306,-0.892307692307691,
-0.876923076923076,-0.86153846153846,-0.846153846153845,-0.83076923076923,
-0.815384615384614,-0.799999999999999,-0.784615384615384,-0.769230769230768,
-0.753846153846153,-0.738461538461538,-0.723076923076922,-0.707692307692307,
-0.692307692307692,-0.676923076923076,-0.661538461538461,-0.646153846153846,
-0.63076923076923,-0.615384615384615,-0.6,-0.584615384615384,-0.569230769230769,
-0.553846153846154,-0.538461538461538,-0.523076923076923,-0.507692307692308,
-0.492307692307692,-0.476923076923077,-0.461538461538462,-0.446153846153846,
-0.430769230769231,-0.415384615384615,-0.4,-0.384615384615385,-0.369230769230769,
-0.353846153846154,-0.338461538461538,-0.323076923076923,-0.307692307692308,
-0.292307692307692,-0.276923076923077,-0.261538461538462,-0.246153846153846,
-0.230769230769231,-0.215384615384615,-0.2,-0.184615384615385,-0.169230769230769,
-0.153846153846154,-0.138461538461538,-0.123076923076923,-0.107692307692308,
-0.0923076923076923,-0.0769230769230769,-0.0615384615384615,-0.0461538461538462,
-0.0307692307692308,-0.0153846153846154,0.),(-1.,1.),.UNSPECIFIED.)
GEOMETRIC_REPRESENTATION_ITEM()
RATIONAL_B_SPLINE_SURFACE(((1.,1.),(1.,1.),(1.,1.),(1.,1.),(1.,1.),(1.,
1.),(1.,1.),(1.,1.),(1.,1.),(1.,1.),(1.,1.),(1.,1.),(1.,1.),(1.,1.),(1.,
1.),(1.,1.),(1.,1.),(1.,1.),(1.,1.),(1.,1.),(1.,1.),(1.,1.),(1.,1.),(1.,
1.),(1.,1.),(1.,1.),(1.,1.),(1.,1.),(1.,1.),(1.,1.),(1.,1.),(1.,1.),(1.,
1.),(1.,1.),(1.,1.),(1.,1.),(1.,1.),(1.,1.),(1.,1.),(1.,1.),(1.,1.),(1.,
1.),(1.,1.),(1.,1.),(1.,1.),(1.,1.),(1.,1.),(1.,1.),(1.,1.),(1.,1.),(1.,
1.),(1.,1.),(1.,1.),(1.,1.),(1.,1.),(1.,1.),(1.,1.),(1.,1.),(1.,1.),(1.,
1.),(1.,1.),(1.,1.),(1.,1.),(1.,1.),(1.,1.),(1.,1.),(1.,1.),(1.,1.),(1.,
1.),(1.,1.)))
REPRESENTATION_ITEM('')
SURFACE()
);
#159=(
BOUNDED_SURFACE()
B_SPLINE_SURFACE(5,1,((#70513,#70514),(#70515,#70516),(#70517,#70518),(#70519,
#70520),(#70521,#70522),(#70523,#70524),(#70525,#70526),(#70527,#70528),
(#70529,#70530),(#70531,#70532),(#70533,#70534),(#70535,#70536),(#70537,
#70538),(#70539,#70540),(#70541,#70542),(#70543,#70544),(#70545,#70546),
(#70547,#70548),(#70549,#70550),(#70551,#70552),(#70553,#70554),(#70555,
#70556),(#70557,#70558),(#70559,#70560),(#70561,#70562),(#70563,#70564),
(#70565,#70566),(#70567,#70568),(#70569,#70570),(#70571,#70572),(#70573,
#70574),(#70575,#70576),(#70577,#70578),(#70579,#70580),(#70581,#70582),
(#70583,#70584),(#70585,#70586),(#70587,#70588),(#70589,#70590),(#70591,
#70592),(#70593,#70594),(#70595,#70596),(#70597,#70598),(#70599,#70600),
(#70601,#70602),(#70603,#70604),(#70605,#70606),(#70607,#70608),(#70609,
#70610),(#70611,#70612),(#70613,#70614),(#70615,#70616),(#70617,#70618),
(#70619,#70620),(#70621,#70622),(#70623,#70624),(#70625,#70626),(#70627,
#70628),(#70629,#70630),(#70631,#70632),(#70633,#70634),(#70635,#70636),
(#70637,#70638),(#70639,#70640),(#70641,#70642),(#70643,#70644),(#70645,
#70646),(#70647,#70648),(#70649,#70650),(#70651,#70652)),.UNSPECIFIED.,
 .F.,.F.,.F.)
B_SPLINE_SURFACE_WITH_KNOTS((6,1,1,1,1,1,1,1,1,1,1,1,1,1,1,1,1,1,1,1,1,
1,1,1,1,1,1,1,1,1,1,1,1,1,1,1,1,1,1,1,1,1,1,1,1,1,1,1,1,1,1,1,1,1,1,1,1,
1,1,1,1,1,1,1,1,6),(2,2),(-1.,-0.984615384615383,-0.969230769230768,-0.953846153846152,
-0.938461538461537,-0.923076923076922,-0.907692307692306,-0.892307692307691,
-0.876923076923076,-0.86153846153846,-0.846153846153845,-0.83076923076923,
-0.815384615384614,-0.799999999999999,-0.784615384615384,-0.769230769230768,
-0.753846153846153,-0.738461538461538,-0.723076923076922,-0.707692307692307,
-0.692307692307692,-0.676923076923076,-0.661538461538461,-0.646153846153846,
-0.63076923076923,-0.615384615384615,-0.6,-0.584615384615384,-0.569230769230769,
-0.553846153846154,-0.538461538461538,-0.523076923076923,-0.507692307692308,
-0.492307692307692,-0.476923076923077,-0.461538461538462,-0.446153846153846,
-0.430769230769231,-0.415384615384615,-0.4,-0.384615384615385,-0.369230769230769,
-0.353846153846154,-0.338461538461538,-0.323076923076923,-0.307692307692308,
-0.292307692307692,-0.276923076923077,-0.261538461538462,-0.246153846153846,
-0.230769230769231,-0.215384615384615,-0.2,-0.184615384615385,-0.169230769230769,
-0.153846153846154,-0.138461538461538,-0.123076923076923,-0.107692307692308,
-0.0923076923076923,-0.0769230769230769,-0.0615384615384615,-0.0461538461538462,
-0.0307692307692308,-0.0153846153846154,0.),(-1.,1.),.UNSPECIFIED.)
GEOMETRIC_REPRESENTATION_ITEM()
RATIONAL_B_SPLINE_SURFACE(((1.,1.),(1.,1.),(1.,1.),(1.,1.),(1.,1.),(1.,
1.),(1.,1.),(1.,1.),(1.,1.),(1.,1.),(1.,1.),(1.,1.),(1.,1.),(1.,1.),(1.,
1.),(1.,1.),(1.,1.),(1.,1.),(1.,1.),(1.,1.),(1.,1.),(1.,1.),(1.,1.),(1.,
1.),(1.,1.),(1.,1.),(1.,1.),(1.,1.),(1.,1.),(1.,1.),(1.,1.),(1.,1.),(1.,
1.),(1.,1.),(1.,1.),(1.,1.),(1.,1.),(1.,1.),(1.,1.),(1.,1.),(1.,1.),(1.,
1.),(1.,1.),(1.,1.),(1.,1.),(1.,1.),(1.,1.),(1.,1.),(1.,1.),(1.,1.),(1.,
1.),(1.,1.),(1.,1.),(1.,1.),(1.,1.),(1.,1.),(1.,1.),(1.,1.),(1.,1.),(1.,
1.),(1.,1.),(1.,1.),(1.,1.),(1.,1.),(1.,1.),(1.,1.),(1.,1.),(1.,1.),(1.,
1.),(1.,1.)))
REPRESENTATION_ITEM('')
SURFACE()
);
#160=(
BOUNDED_SURFACE()
B_SPLINE_SURFACE(5,1,((#70725,#70726),(#70727,#70728),(#70729,#70730),(#70731,
#70732),(#70733,#70734),(#70735,#70736),(#70737,#70738),(#70739,#70740),
(#70741,#70742),(#70743,#70744),(#70745,#70746),(#70747,#70748),(#70749,
#70750),(#70751,#70752),(#70753,#70754),(#70755,#70756),(#70757,#70758),
(#70759,#70760),(#70761,#70762),(#70763,#70764),(#70765,#70766),(#70767,
#70768),(#70769,#70770),(#70771,#70772),(#70773,#70774),(#70775,#70776),
(#70777,#70778),(#70779,#70780),(#70781,#70782),(#70783,#70784),(#70785,
#70786),(#70787,#70788),(#70789,#70790),(#70791,#70792),(#70793,#70794),
(#70795,#70796),(#70797,#70798),(#70799,#70800),(#70801,#70802),(#70803,
#70804),(#70805,#70806),(#70807,#70808),(#70809,#70810),(#70811,#70812),
(#70813,#70814),(#70815,#70816),(#70817,#70818),(#70819,#70820),(#70821,
#70822),(#70823,#70824),(#70825,#70826),(#70827,#70828),(#70829,#70830),
(#70831,#70832),(#70833,#70834),(#70835,#70836),(#70837,#70838),(#70839,
#70840),(#70841,#70842),(#70843,#70844),(#70845,#70846),(#70847,#70848),
(#70849,#70850),(#70851,#70852),(#70853,#70854),(#70855,#70856),(#70857,
#70858),(#70859,#70860),(#70861,#70862),(#70863,#70864)),.UNSPECIFIED.,
 .F.,.F.,.F.)
B_SPLINE_SURFACE_WITH_KNOTS((6,1,1,1,1,1,1,1,1,1,1,1,1,1,1,1,1,1,1,1,1,
1,1,1,1,1,1,1,1,1,1,1,1,1,1,1,1,1,1,1,1,1,1,1,1,1,1,1,1,1,1,1,1,1,1,1,1,
1,1,1,1,1,1,1,1,6),(2,2),(-1.,-0.984615384615383,-0.969230769230768,-0.953846153846152,
-0.938461538461537,-0.923076923076922,-0.907692307692306,-0.892307692307691,
-0.876923076923076,-0.86153846153846,-0.846153846153845,-0.83076923076923,
-0.815384615384614,-0.799999999999999,-0.784615384615384,-0.769230769230768,
-0.753846153846153,-0.738461538461538,-0.723076923076922,-0.707692307692307,
-0.692307692307692,-0.676923076923076,-0.661538461538461,-0.646153846153846,
-0.63076923076923,-0.615384615384615,-0.6,-0.584615384615384,-0.569230769230769,
-0.553846153846154,-0.538461538461538,-0.523076923076923,-0.507692307692308,
-0.492307692307692,-0.476923076923077,-0.461538461538462,-0.446153846153846,
-0.430769230769231,-0.415384615384615,-0.4,-0.384615384615385,-0.369230769230769,
-0.353846153846154,-0.338461538461538,-0.323076923076923,-0.307692307692308,
-0.292307692307692,-0.276923076923077,-0.261538461538462,-0.246153846153846,
-0.230769230769231,-0.215384615384615,-0.2,-0.184615384615385,-0.169230769230769,
-0.153846153846154,-0.138461538461538,-0.123076923076923,-0.107692307692308,
-0.0923076923076923,-0.0769230769230769,-0.0615384615384615,-0.0461538461538462,
-0.0307692307692308,-0.0153846153846154,0.),(-1.,1.),.UNSPECIFIED.)
GEOMETRIC_REPRESENTATION_ITEM()
RATIONAL_B_SPLINE_SURFACE(((1.,1.),(1.,1.),(1.,1.),(1.,1.),(1.,1.),(1.,
1.),(1.,1.),(1.,1.),(1.,1.),(1.,1.),(1.,1.),(1.,1.),(1.,1.),(1.,1.),(1.,
1.),(1.,1.),(1.,1.),(1.,1.),(1.,1.),(1.,1.),(1.,1.),(1.,1.),(1.,1.),(1.,
1.),(1.,1.),(1.,1.),(1.,1.),(1.,1.),(1.,1.),(1.,1.),(1.,1.),(1.,1.),(1.,
1.),(1.,1.),(1.,1.),(1.,1.),(1.,1.),(1.,1.),(1.,1.),(1.,1.),(1.,1.),(1.,
1.),(1.,1.),(1.,1.),(1.,1.),(1.,1.),(1.,1.),(1.,1.),(1.,1.),(1.,1.),(1.,
1.),(1.,1.),(1.,1.),(1.,1.),(1.,1.),(1.,1.),(1.,1.),(1.,1.),(1.,1.),(1.,
1.),(1.,1.),(1.,1.),(1.,1.),(1.,1.),(1.,1.),(1.,1.),(1.,1.),(1.,1.),(1.,
1.),(1.,1.)))
REPRESENTATION_ITEM('')
SURFACE()
);
#161=(
BOUNDED_SURFACE()
B_SPLINE_SURFACE(5,1,((#70955,#70956),(#70957,#70958),(#70959,#70960),(#70961,
#70962),(#70963,#70964),(#70965,#70966),(#70967,#70968),(#70969,#70970),
(#70971,#70972),(#70973,#70974),(#70975,#70976),(#70977,#70978),(#70979,
#70980),(#70981,#70982),(#70983,#70984),(#70985,#70986),(#70987,#70988),
(#70989,#70990),(#70991,#70992),(#70993,#70994),(#70995,#70996),(#70997,
#70998),(#70999,#71000),(#71001,#71002),(#71003,#71004),(#71005,#71006),
(#71007,#71008),(#71009,#71010),(#71011,#71012),(#71013,#71014),(#71015,
#71016),(#71017,#71018),(#71019,#71020),(#71021,#71022),(#71023,#71024),
(#71025,#71026),(#71027,#71028),(#71029,#71030),(#71031,#71032),(#71033,
#71034),(#71035,#71036),(#71037,#71038),(#71039,#71040),(#71041,#71042),
(#71043,#71044),(#71045,#71046),(#71047,#71048),(#71049,#71050),(#71051,
#71052),(#71053,#71054),(#71055,#71056),(#71057,#71058),(#71059,#71060),
(#71061,#71062),(#71063,#71064),(#71065,#71066),(#71067,#71068),(#71069,
#71070),(#71071,#71072),(#71073,#71074),(#71075,#71076),(#71077,#71078),
(#71079,#71080),(#71081,#71082),(#71083,#71084),(#71085,#71086),(#71087,
#71088),(#71089,#71090),(#71091,#71092),(#71093,#71094)),.UNSPECIFIED.,
 .F.,.F.,.F.)
B_SPLINE_SURFACE_WITH_KNOTS((6,1,1,1,1,1,1,1,1,1,1,1,1,1,1,1,1,1,1,1,1,
1,1,1,1,1,1,1,1,1,1,1,1,1,1,1,1,1,1,1,1,1,1,1,1,1,1,1,1,1,1,1,1,1,1,1,1,
1,1,1,1,1,1,1,1,6),(2,2),(-1.,-0.984615384615383,-0.969230769230768,-0.953846153846152,
-0.938461538461537,-0.923076923076922,-0.907692307692306,-0.892307692307691,
-0.876923076923076,-0.86153846153846,-0.846153846153845,-0.83076923076923,
-0.815384615384614,-0.799999999999999,-0.784615384615384,-0.769230769230768,
-0.753846153846153,-0.738461538461538,-0.723076923076922,-0.707692307692307,
-0.692307692307692,-0.676923076923076,-0.661538461538461,-0.646153846153846,
-0.63076923076923,-0.615384615384615,-0.6,-0.584615384615384,-0.569230769230769,
-0.553846153846154,-0.538461538461538,-0.523076923076923,-0.507692307692308,
-0.492307692307692,-0.476923076923077,-0.461538461538462,-0.446153846153846,
-0.430769230769231,-0.415384615384615,-0.4,-0.384615384615385,-0.369230769230769,
-0.353846153846154,-0.338461538461538,-0.323076923076923,-0.307692307692308,
-0.292307692307692,-0.276923076923077,-0.261538461538462,-0.246153846153846,
-0.230769230769231,-0.215384615384615,-0.2,-0.184615384615385,-0.169230769230769,
-0.153846153846154,-0.138461538461538,-0.123076923076923,-0.107692307692308,
-0.0923076923076923,-0.0769230769230769,-0.0615384615384615,-0.0461538461538462,
-0.0307692307692308,-0.0153846153846154,0.),(-1.,1.),.UNSPECIFIED.)
GEOMETRIC_REPRESENTATION_ITEM()
RATIONAL_B_SPLINE_SURFACE(((1.,1.),(1.,1.),(1.,1.),(1.,1.),(1.,1.),(1.,
1.),(1.,1.),(1.,1.),(1.,1.),(1.,1.),(1.,1.),(1.,1.),(1.,1.),(1.,1.),(1.,
1.),(1.,1.),(1.,1.),(1.,1.),(1.,1.),(1.,1.),(1.,1.),(1.,1.),(1.,1.),(1.,
1.),(1.,1.),(1.,1.),(1.,1.),(1.,1.),(1.,1.),(1.,1.),(1.,1.),(1.,1.),(1.,
1.),(1.,1.),(1.,1.),(1.,1.),(1.,1.),(1.,1.),(1.,1.),(1.,1.),(1.,1.),(1.,
1.),(1.,1.),(1.,1.),(1.,1.),(1.,1.),(1.,1.),(1.,1.),(1.,1.),(1.,1.),(1.,
1.),(1.,1.),(1.,1.),(1.,1.),(1.,1.),(1.,1.),(1.,1.),(1.,1.),(1.,1.),(1.,
1.),(1.,1.),(1.,1.),(1.,1.),(1.,1.),(1.,1.),(1.,1.),(1.,1.),(1.,1.),(1.,
1.),(1.,1.)))
REPRESENTATION_ITEM('')
SURFACE()
);
#162=(
BOUNDED_SURFACE()
B_SPLINE_SURFACE(5,1,((#71167,#71168),(#71169,#71170),(#71171,#71172),(#71173,
#71174),(#71175,#71176),(#71177,#71178),(#71179,#71180),(#71181,#71182),
(#71183,#71184),(#71185,#71186),(#71187,#71188),(#71189,#71190),(#71191,
#71192),(#71193,#71194),(#71195,#71196),(#71197,#71198),(#71199,#71200),
(#71201,#71202),(#71203,#71204),(#71205,#71206),(#71207,#71208),(#71209,
#71210),(#71211,#71212),(#71213,#71214),(#71215,#71216),(#71217,#71218),
(#71219,#71220),(#71221,#71222),(#71223,#71224),(#71225,#71226),(#71227,
#71228),(#71229,#71230),(#71231,#71232),(#71233,#71234),(#71235,#71236),
(#71237,#71238),(#71239,#71240),(#71241,#71242),(#71243,#71244),(#71245,
#71246),(#71247,#71248),(#71249,#71250),(#71251,#71252),(#71253,#71254),
(#71255,#71256),(#71257,#71258),(#71259,#71260),(#71261,#71262),(#71263,
#71264),(#71265,#71266),(#71267,#71268),(#71269,#71270),(#71271,#71272),
(#71273,#71274),(#71275,#71276),(#71277,#71278),(#71279,#71280),(#71281,
#71282),(#71283,#71284),(#71285,#71286),(#71287,#71288),(#71289,#71290),
(#71291,#71292),(#71293,#71294),(#71295,#71296),(#71297,#71298),(#71299,
#71300),(#71301,#71302),(#71303,#71304),(#71305,#71306)),.UNSPECIFIED.,
 .F.,.F.,.F.)
B_SPLINE_SURFACE_WITH_KNOTS((6,1,1,1,1,1,1,1,1,1,1,1,1,1,1,1,1,1,1,1,1,
1,1,1,1,1,1,1,1,1,1,1,1,1,1,1,1,1,1,1,1,1,1,1,1,1,1,1,1,1,1,1,1,1,1,1,1,
1,1,1,1,1,1,1,1,6),(2,2),(-1.,-0.984615384615383,-0.969230769230768,-0.953846153846152,
-0.938461538461537,-0.923076923076922,-0.907692307692306,-0.892307692307691,
-0.876923076923076,-0.86153846153846,-0.846153846153845,-0.83076923076923,
-0.815384615384614,-0.799999999999999,-0.784615384615384,-0.769230769230768,
-0.753846153846153,-0.738461538461538,-0.723076923076922,-0.707692307692307,
-0.692307692307692,-0.676923076923076,-0.661538461538461,-0.646153846153846,
-0.63076923076923,-0.615384615384615,-0.6,-0.584615384615384,-0.569230769230769,
-0.553846153846154,-0.538461538461538,-0.523076923076923,-0.507692307692308,
-0.492307692307692,-0.476923076923077,-0.461538461538462,-0.446153846153846,
-0.430769230769231,-0.415384615384615,-0.4,-0.384615384615385,-0.369230769230769,
-0.353846153846154,-0.338461538461538,-0.323076923076923,-0.307692307692308,
-0.292307692307692,-0.276923076923077,-0.261538461538462,-0.246153846153846,
-0.230769230769231,-0.215384615384615,-0.2,-0.184615384615385,-0.169230769230769,
-0.153846153846154,-0.138461538461538,-0.123076923076923,-0.107692307692308,
-0.0923076923076923,-0.0769230769230769,-0.0615384615384615,-0.0461538461538462,
-0.0307692307692308,-0.0153846153846154,0.),(-1.,1.),.UNSPECIFIED.)
GEOMETRIC_REPRESENTATION_ITEM()
RATIONAL_B_SPLINE_SURFACE(((1.,1.),(1.,1.),(1.,1.),(1.,1.),(1.,1.),(1.,
1.),(1.,1.),(1.,1.),(1.,1.),(1.,1.),(1.,1.),(1.,1.),(1.,1.),(1.,1.),(1.,
1.),(1.,1.),(1.,1.),(1.,1.),(1.,1.),(1.,1.),(1.,1.),(1.,1.),(1.,1.),(1.,
1.),(1.,1.),(1.,1.),(1.,1.),(1.,1.),(1.,1.),(1.,1.),(1.,1.),(1.,1.),(1.,
1.),(1.,1.),(1.,1.),(1.,1.),(1.,1.),(1.,1.),(1.,1.),(1.,1.),(1.,1.),(1.,
1.),(1.,1.),(1.,1.),(1.,1.),(1.,1.),(1.,1.),(1.,1.),(1.,1.),(1.,1.),(1.,
1.),(1.,1.),(1.,1.),(1.,1.),(1.,1.),(1.,1.),(1.,1.),(1.,1.),(1.,1.),(1.,
1.),(1.,1.),(1.,1.),(1.,1.),(1.,1.),(1.,1.),(1.,1.),(1.,1.),(1.,1.),(1.,
1.),(1.,1.)))
REPRESENTATION_ITEM('')
SURFACE()
);
#163=(
BOUNDED_SURFACE()
B_SPLINE_SURFACE(5,1,((#71397,#71398),(#71399,#71400),(#71401,#71402),(#71403,
#71404),(#71405,#71406),(#71407,#71408),(#71409,#71410),(#71411,#71412),
(#71413,#71414),(#71415,#71416),(#71417,#71418),(#71419,#71420),(#71421,
#71422),(#71423,#71424),(#71425,#71426),(#71427,#71428),(#71429,#71430),
(#71431,#71432),(#71433,#71434),(#71435,#71436),(#71437,#71438),(#71439,
#71440),(#71441,#71442),(#71443,#71444),(#71445,#71446),(#71447,#71448),
(#71449,#71450),(#71451,#71452),(#71453,#71454),(#71455,#71456),(#71457,
#71458),(#71459,#71460),(#71461,#71462),(#71463,#71464),(#71465,#71466),
(#71467,#71468),(#71469,#71470),(#71471,#71472),(#71473,#71474),(#71475,
#71476),(#71477,#71478),(#71479,#71480),(#71481,#71482),(#71483,#71484),
(#71485,#71486),(#71487,#71488),(#71489,#71490),(#71491,#71492),(#71493,
#71494),(#71495,#71496),(#71497,#71498),(#71499,#71500),(#71501,#71502),
(#71503,#71504),(#71505,#71506),(#71507,#71508),(#71509,#71510),(#71511,
#71512),(#71513,#71514),(#71515,#71516),(#71517,#71518),(#71519,#71520),
(#71521,#71522),(#71523,#71524),(#71525,#71526),(#71527,#71528),(#71529,
#71530),(#71531,#71532),(#71533,#71534),(#71535,#71536)),.UNSPECIFIED.,
 .F.,.F.,.F.)
B_SPLINE_SURFACE_WITH_KNOTS((6,1,1,1,1,1,1,1,1,1,1,1,1,1,1,1,1,1,1,1,1,
1,1,1,1,1,1,1,1,1,1,1,1,1,1,1,1,1,1,1,1,1,1,1,1,1,1,1,1,1,1,1,1,1,1,1,1,
1,1,1,1,1,1,1,1,6),(2,2),(-1.,-0.984615384615383,-0.969230769230768,-0.953846153846152,
-0.938461538461537,-0.923076923076922,-0.907692307692306,-0.892307692307691,
-0.876923076923076,-0.86153846153846,-0.846153846153845,-0.83076923076923,
-0.815384615384614,-0.799999999999999,-0.784615384615384,-0.769230769230768,
-0.753846153846153,-0.738461538461538,-0.723076923076922,-0.707692307692307,
-0.692307692307692,-0.676923076923076,-0.661538461538461,-0.646153846153846,
-0.63076923076923,-0.615384615384615,-0.6,-0.584615384615384,-0.569230769230769,
-0.553846153846154,-0.538461538461538,-0.523076923076923,-0.507692307692308,
-0.492307692307692,-0.476923076923077,-0.461538461538462,-0.446153846153846,
-0.430769230769231,-0.415384615384615,-0.4,-0.384615384615385,-0.369230769230769,
-0.353846153846154,-0.338461538461538,-0.323076923076923,-0.307692307692308,
-0.292307692307692,-0.276923076923077,-0.261538461538462,-0.246153846153846,
-0.230769230769231,-0.215384615384615,-0.2,-0.184615384615385,-0.169230769230769,
-0.153846153846154,-0.138461538461538,-0.123076923076923,-0.107692307692308,
-0.0923076923076923,-0.0769230769230769,-0.0615384615384615,-0.0461538461538462,
-0.0307692307692308,-0.0153846153846154,0.),(-1.,1.),.UNSPECIFIED.)
GEOMETRIC_REPRESENTATION_ITEM()
RATIONAL_B_SPLINE_SURFACE(((1.,1.),(1.,1.),(1.,1.),(1.,1.),(1.,1.),(1.,
1.),(1.,1.),(1.,1.),(1.,1.),(1.,1.),(1.,1.),(1.,1.),(1.,1.),(1.,1.),(1.,
1.),(1.,1.),(1.,1.),(1.,1.),(1.,1.),(1.,1.),(1.,1.),(1.,1.),(1.,1.),(1.,
1.),(1.,1.),(1.,1.),(1.,1.),(1.,1.),(1.,1.),(1.,1.),(1.,1.),(1.,1.),(1.,
1.),(1.,1.),(1.,1.),(1.,1.),(1.,1.),(1.,1.),(1.,1.),(1.,1.),(1.,1.),(1.,
1.),(1.,1.),(1.,1.),(1.,1.),(1.,1.),(1.,1.),(1.,1.),(1.,1.),(1.,1.),(1.,
1.),(1.,1.),(1.,1.),(1.,1.),(1.,1.),(1.,1.),(1.,1.),(1.,1.),(1.,1.),(1.,
1.),(1.,1.),(1.,1.),(1.,1.),(1.,1.),(1.,1.),(1.,1.),(1.,1.),(1.,1.),(1.,
1.),(1.,1.)))
REPRESENTATION_ITEM('')
SURFACE()
);
#164=(
BOUNDED_SURFACE()
B_SPLINE_SURFACE(5,1,((#71609,#71610),(#71611,#71612),(#71613,#71614),(#71615,
#71616),(#71617,#71618),(#71619,#71620),(#71621,#71622),(#71623,#71624),
(#71625,#71626),(#71627,#71628),(#71629,#71630),(#71631,#71632),(#71633,
#71634),(#71635,#71636),(#71637,#71638),(#71639,#71640),(#71641,#71642),
(#71643,#71644),(#71645,#71646),(#71647,#71648),(#71649,#71650),(#71651,
#71652),(#71653,#71654),(#71655,#71656),(#71657,#71658),(#71659,#71660),
(#71661,#71662),(#71663,#71664),(#71665,#71666),(#71667,#71668),(#71669,
#71670),(#71671,#71672),(#71673,#71674),(#71675,#71676),(#71677,#71678),
(#71679,#71680),(#71681,#71682),(#71683,#71684),(#71685,#71686),(#71687,
#71688),(#71689,#71690),(#71691,#71692),(#71693,#71694),(#71695,#71696),
(#71697,#71698),(#71699,#71700),(#71701,#71702),(#71703,#71704),(#71705,
#71706),(#71707,#71708),(#71709,#71710),(#71711,#71712),(#71713,#71714),
(#71715,#71716),(#71717,#71718),(#71719,#71720),(#71721,#71722),(#71723,
#71724),(#71725,#71726),(#71727,#71728),(#71729,#71730),(#71731,#71732),
(#71733,#71734),(#71735,#71736),(#71737,#71738),(#71739,#71740),(#71741,
#71742),(#71743,#71744),(#71745,#71746),(#71747,#71748)),.UNSPECIFIED.,
 .F.,.F.,.F.)
B_SPLINE_SURFACE_WITH_KNOTS((6,1,1,1,1,1,1,1,1,1,1,1,1,1,1,1,1,1,1,1,1,
1,1,1,1,1,1,1,1,1,1,1,1,1,1,1,1,1,1,1,1,1,1,1,1,1,1,1,1,1,1,1,1,1,1,1,1,
1,1,1,1,1,1,1,1,6),(2,2),(-1.,-0.984615384615383,-0.969230769230768,-0.953846153846152,
-0.938461538461537,-0.923076923076922,-0.907692307692306,-0.892307692307691,
-0.876923076923076,-0.86153846153846,-0.846153846153845,-0.83076923076923,
-0.815384615384614,-0.799999999999999,-0.784615384615384,-0.769230769230768,
-0.753846153846153,-0.738461538461538,-0.723076923076922,-0.707692307692307,
-0.692307692307692,-0.676923076923076,-0.661538461538461,-0.646153846153846,
-0.63076923076923,-0.615384615384615,-0.6,-0.584615384615384,-0.569230769230769,
-0.553846153846154,-0.538461538461538,-0.523076923076923,-0.507692307692308,
-0.492307692307692,-0.476923076923077,-0.461538461538462,-0.446153846153846,
-0.430769230769231,-0.415384615384615,-0.4,-0.384615384615385,-0.369230769230769,
-0.353846153846154,-0.338461538461538,-0.323076923076923,-0.307692307692308,
-0.292307692307692,-0.276923076923077,-0.261538461538462,-0.246153846153846,
-0.230769230769231,-0.215384615384615,-0.2,-0.184615384615385,-0.169230769230769,
-0.153846153846154,-0.138461538461538,-0.123076923076923,-0.107692307692308,
-0.0923076923076923,-0.0769230769230769,-0.0615384615384615,-0.0461538461538462,
-0.0307692307692308,-0.0153846153846154,0.),(-1.,1.),.UNSPECIFIED.)
GEOMETRIC_REPRESENTATION_ITEM()
RATIONAL_B_SPLINE_SURFACE(((1.,1.),(1.,1.),(1.,1.),(1.,1.),(1.,1.),(1.,
1.),(1.,1.),(1.,1.),(1.,1.),(1.,1.),(1.,1.),(1.,1.),(1.,1.),(1.,1.),(1.,
1.),(1.,1.),(1.,1.),(1.,1.),(1.,1.),(1.,1.),(1.,1.),(1.,1.),(1.,1.),(1.,
1.),(1.,1.),(1.,1.),(1.,1.),(1.,1.),(1.,1.),(1.,1.),(1.,1.),(1.,1.),(1.,
1.),(1.,1.),(1.,1.),(1.,1.),(1.,1.),(1.,1.),(1.,1.),(1.,1.),(1.,1.),(1.,
1.),(1.,1.),(1.,1.),(1.,1.),(1.,1.),(1.,1.),(1.,1.),(1.,1.),(1.,1.),(1.,
1.),(1.,1.),(1.,1.),(1.,1.),(1.,1.),(1.,1.),(1.,1.),(1.,1.),(1.,1.),(1.,
1.),(1.,1.),(1.,1.),(1.,1.),(1.,1.),(1.,1.),(1.,1.),(1.,1.),(1.,1.),(1.,
1.),(1.,1.)))
REPRESENTATION_ITEM('')
SURFACE()
);
#165=(
BOUNDED_SURFACE()
B_SPLINE_SURFACE(5,1,((#71839,#71840),(#71841,#71842),(#71843,#71844),(#71845,
#71846),(#71847,#71848),(#71849,#71850),(#71851,#71852),(#71853,#71854),
(#71855,#71856),(#71857,#71858),(#71859,#71860),(#71861,#71862),(#71863,
#71864),(#71865,#71866),(#71867,#71868),(#71869,#71870),(#71871,#71872),
(#71873,#71874),(#71875,#71876),(#71877,#71878),(#71879,#71880),(#71881,
#71882),(#71883,#71884),(#71885,#71886),(#71887,#71888),(#71889,#71890),
(#71891,#71892),(#71893,#71894),(#71895,#71896),(#71897,#71898),(#71899,
#71900),(#71901,#71902),(#71903,#71904),(#71905,#71906),(#71907,#71908),
(#71909,#71910),(#71911,#71912),(#71913,#71914),(#71915,#71916),(#71917,
#71918),(#71919,#71920),(#71921,#71922),(#71923,#71924),(#71925,#71926),
(#71927,#71928),(#71929,#71930),(#71931,#71932),(#71933,#71934),(#71935,
#71936),(#71937,#71938),(#71939,#71940),(#71941,#71942),(#71943,#71944),
(#71945,#71946),(#71947,#71948),(#71949,#71950),(#71951,#71952),(#71953,
#71954),(#71955,#71956),(#71957,#71958),(#71959,#71960),(#71961,#71962),
(#71963,#71964),(#71965,#71966),(#71967,#71968),(#71969,#71970),(#71971,
#71972),(#71973,#71974),(#71975,#71976),(#71977,#71978)),.UNSPECIFIED.,
 .F.,.F.,.F.)
B_SPLINE_SURFACE_WITH_KNOTS((6,1,1,1,1,1,1,1,1,1,1,1,1,1,1,1,1,1,1,1,1,
1,1,1,1,1,1,1,1,1,1,1,1,1,1,1,1,1,1,1,1,1,1,1,1,1,1,1,1,1,1,1,1,1,1,1,1,
1,1,1,1,1,1,1,1,6),(2,2),(-1.,-0.984615384615383,-0.969230769230768,-0.953846153846152,
-0.938461538461537,-0.923076923076922,-0.907692307692306,-0.892307692307691,
-0.876923076923076,-0.86153846153846,-0.846153846153845,-0.83076923076923,
-0.815384615384614,-0.799999999999999,-0.784615384615384,-0.769230769230768,
-0.753846153846153,-0.738461538461538,-0.723076923076922,-0.707692307692307,
-0.692307692307692,-0.676923076923076,-0.661538461538461,-0.646153846153846,
-0.63076923076923,-0.615384615384615,-0.6,-0.584615384615384,-0.569230769230769,
-0.553846153846154,-0.538461538461538,-0.523076923076923,-0.507692307692308,
-0.492307692307692,-0.476923076923077,-0.461538461538462,-0.446153846153846,
-0.430769230769231,-0.415384615384615,-0.4,-0.384615384615385,-0.369230769230769,
-0.353846153846154,-0.338461538461538,-0.323076923076923,-0.307692307692308,
-0.292307692307692,-0.276923076923077,-0.261538461538462,-0.246153846153846,
-0.230769230769231,-0.215384615384615,-0.2,-0.184615384615385,-0.169230769230769,
-0.153846153846154,-0.138461538461538,-0.123076923076923,-0.107692307692308,
-0.0923076923076923,-0.0769230769230769,-0.0615384615384615,-0.0461538461538462,
-0.0307692307692308,-0.0153846153846154,0.),(-1.,1.),.UNSPECIFIED.)
GEOMETRIC_REPRESENTATION_ITEM()
RATIONAL_B_SPLINE_SURFACE(((1.,1.),(1.,1.),(1.,1.),(1.,1.),(1.,1.),(1.,
1.),(1.,1.),(1.,1.),(1.,1.),(1.,1.),(1.,1.),(1.,1.),(1.,1.),(1.,1.),(1.,
1.),(1.,1.),(1.,1.),(1.,1.),(1.,1.),(1.,1.),(1.,1.),(1.,1.),(1.,1.),(1.,
1.),(1.,1.),(1.,1.),(1.,1.),(1.,1.),(1.,1.),(1.,1.),(1.,1.),(1.,1.),(1.,
1.),(1.,1.),(1.,1.),(1.,1.),(1.,1.),(1.,1.),(1.,1.),(1.,1.),(1.,1.),(1.,
1.),(1.,1.),(1.,1.),(1.,1.),(1.,1.),(1.,1.),(1.,1.),(1.,1.),(1.,1.),(1.,
1.),(1.,1.),(1.,1.),(1.,1.),(1.,1.),(1.,1.),(1.,1.),(1.,1.),(1.,1.),(1.,
1.),(1.,1.),(1.,1.),(1.,1.),(1.,1.),(1.,1.),(1.,1.),(1.,1.),(1.,1.),(1.,
1.),(1.,1.)))
REPRESENTATION_ITEM('')
SURFACE()
);
#166=(
BOUNDED_SURFACE()
B_SPLINE_SURFACE(5,1,((#72051,#72052),(#72053,#72054),(#72055,#72056),(#72057,
#72058),(#72059,#72060),(#72061,#72062),(#72063,#72064),(#72065,#72066),
(#72067,#72068),(#72069,#72070),(#72071,#72072),(#72073,#72074),(#72075,
#72076),(#72077,#72078),(#72079,#72080),(#72081,#72082),(#72083,#72084),
(#72085,#72086),(#72087,#72088),(#72089,#72090),(#72091,#72092),(#72093,
#72094),(#72095,#72096),(#72097,#72098),(#72099,#72100),(#72101,#72102),
(#72103,#72104),(#72105,#72106),(#72107,#72108),(#72109,#72110),(#72111,
#72112),(#72113,#72114),(#72115,#72116),(#72117,#72118),(#72119,#72120),
(#72121,#72122),(#72123,#72124),(#72125,#72126),(#72127,#72128),(#72129,
#72130),(#72131,#72132),(#72133,#72134),(#72135,#72136),(#72137,#72138),
(#72139,#72140),(#72141,#72142),(#72143,#72144),(#72145,#72146),(#72147,
#72148),(#72149,#72150),(#72151,#72152),(#72153,#72154),(#72155,#72156),
(#72157,#72158),(#72159,#72160),(#72161,#72162),(#72163,#72164),(#72165,
#72166),(#72167,#72168),(#72169,#72170),(#72171,#72172),(#72173,#72174),
(#72175,#72176),(#72177,#72178),(#72179,#72180),(#72181,#72182),(#72183,
#72184),(#72185,#72186),(#72187,#72188),(#72189,#72190)),.UNSPECIFIED.,
 .F.,.F.,.F.)
B_SPLINE_SURFACE_WITH_KNOTS((6,1,1,1,1,1,1,1,1,1,1,1,1,1,1,1,1,1,1,1,1,
1,1,1,1,1,1,1,1,1,1,1,1,1,1,1,1,1,1,1,1,1,1,1,1,1,1,1,1,1,1,1,1,1,1,1,1,
1,1,1,1,1,1,1,1,6),(2,2),(-1.,-0.984615384615383,-0.969230769230768,-0.953846153846152,
-0.938461538461537,-0.923076923076922,-0.907692307692306,-0.892307692307691,
-0.876923076923076,-0.86153846153846,-0.846153846153845,-0.83076923076923,
-0.815384615384614,-0.799999999999999,-0.784615384615384,-0.769230769230768,
-0.753846153846153,-0.738461538461538,-0.723076923076922,-0.707692307692307,
-0.692307692307692,-0.676923076923076,-0.661538461538461,-0.646153846153846,
-0.63076923076923,-0.615384615384615,-0.6,-0.584615384615384,-0.569230769230769,
-0.553846153846154,-0.538461538461538,-0.523076923076923,-0.507692307692308,
-0.492307692307692,-0.476923076923077,-0.461538461538462,-0.446153846153846,
-0.430769230769231,-0.415384615384615,-0.4,-0.384615384615385,-0.369230769230769,
-0.353846153846154,-0.338461538461538,-0.323076923076923,-0.307692307692308,
-0.292307692307692,-0.276923076923077,-0.261538461538462,-0.246153846153846,
-0.230769230769231,-0.215384615384615,-0.2,-0.184615384615385,-0.169230769230769,
-0.153846153846154,-0.138461538461538,-0.123076923076923,-0.107692307692308,
-0.0923076923076923,-0.0769230769230769,-0.0615384615384615,-0.0461538461538462,
-0.0307692307692308,-0.0153846153846154,0.),(-1.,1.),.UNSPECIFIED.)
GEOMETRIC_REPRESENTATION_ITEM()
RATIONAL_B_SPLINE_SURFACE(((1.,1.),(1.,1.),(1.,1.),(1.,1.),(1.,1.),(1.,
1.),(1.,1.),(1.,1.),(1.,1.),(1.,1.),(1.,1.),(1.,1.),(1.,1.),(1.,1.),(1.,
1.),(1.,1.),(1.,1.),(1.,1.),(1.,1.),(1.,1.),(1.,1.),(1.,1.),(1.,1.),(1.,
1.),(1.,1.),(1.,1.),(1.,1.),(1.,1.),(1.,1.),(1.,1.),(1.,1.),(1.,1.),(1.,
1.),(1.,1.),(1.,1.),(1.,1.),(1.,1.),(1.,1.),(1.,1.),(1.,1.),(1.,1.),(1.,
1.),(1.,1.),(1.,1.),(1.,1.),(1.,1.),(1.,1.),(1.,1.),(1.,1.),(1.,1.),(1.,
1.),(1.,1.),(1.,1.),(1.,1.),(1.,1.),(1.,1.),(1.,1.),(1.,1.),(1.,1.),(1.,
1.),(1.,1.),(1.,1.),(1.,1.),(1.,1.),(1.,1.),(1.,1.),(1.,1.),(1.,1.),(1.,
1.),(1.,1.)))
REPRESENTATION_ITEM('')
SURFACE()
);
#167=(
BOUNDED_SURFACE()
B_SPLINE_SURFACE(5,1,((#72281,#72282),(#72283,#72284),(#72285,#72286),(#72287,
#72288),(#72289,#72290),(#72291,#72292),(#72293,#72294),(#72295,#72296),
(#72297,#72298),(#72299,#72300),(#72301,#72302),(#72303,#72304),(#72305,
#72306),(#72307,#72308),(#72309,#72310),(#72311,#72312),(#72313,#72314),
(#72315,#72316),(#72317,#72318),(#72319,#72320),(#72321,#72322),(#72323,
#72324),(#72325,#72326),(#72327,#72328),(#72329,#72330),(#72331,#72332),
(#72333,#72334),(#72335,#72336),(#72337,#72338),(#72339,#72340),(#72341,
#72342),(#72343,#72344),(#72345,#72346),(#72347,#72348),(#72349,#72350),
(#72351,#72352),(#72353,#72354),(#72355,#72356),(#72357,#72358),(#72359,
#72360),(#72361,#72362),(#72363,#72364),(#72365,#72366),(#72367,#72368),
(#72369,#72370),(#72371,#72372),(#72373,#72374),(#72375,#72376),(#72377,
#72378),(#72379,#72380),(#72381,#72382),(#72383,#72384),(#72385,#72386),
(#72387,#72388),(#72389,#72390),(#72391,#72392),(#72393,#72394),(#72395,
#72396),(#72397,#72398),(#72399,#72400),(#72401,#72402),(#72403,#72404),
(#72405,#72406),(#72407,#72408),(#72409,#72410),(#72411,#72412),(#72413,
#72414),(#72415,#72416),(#72417,#72418),(#72419,#72420)),.UNSPECIFIED.,
 .F.,.F.,.F.)
B_SPLINE_SURFACE_WITH_KNOTS((6,1,1,1,1,1,1,1,1,1,1,1,1,1,1,1,1,1,1,1,1,
1,1,1,1,1,1,1,1,1,1,1,1,1,1,1,1,1,1,1,1,1,1,1,1,1,1,1,1,1,1,1,1,1,1,1,1,
1,1,1,1,1,1,1,1,6),(2,2),(-1.,-0.984615384615383,-0.969230769230768,-0.953846153846152,
-0.938461538461537,-0.923076923076922,-0.907692307692306,-0.892307692307691,
-0.876923076923076,-0.86153846153846,-0.846153846153845,-0.83076923076923,
-0.815384615384614,-0.799999999999999,-0.784615384615384,-0.769230769230768,
-0.753846153846153,-0.738461538461538,-0.723076923076922,-0.707692307692307,
-0.692307692307692,-0.676923076923076,-0.661538461538461,-0.646153846153846,
-0.63076923076923,-0.615384615384615,-0.6,-0.584615384615384,-0.569230769230769,
-0.553846153846154,-0.538461538461538,-0.523076923076923,-0.507692307692308,
-0.492307692307692,-0.476923076923077,-0.461538461538462,-0.446153846153846,
-0.430769230769231,-0.415384615384615,-0.4,-0.384615384615385,-0.369230769230769,
-0.353846153846154,-0.338461538461538,-0.323076923076923,-0.307692307692308,
-0.292307692307692,-0.276923076923077,-0.261538461538462,-0.246153846153846,
-0.230769230769231,-0.215384615384615,-0.2,-0.184615384615385,-0.169230769230769,
-0.153846153846154,-0.138461538461538,-0.123076923076923,-0.107692307692308,
-0.0923076923076923,-0.0769230769230769,-0.0615384615384615,-0.0461538461538462,
-0.0307692307692308,-0.0153846153846154,0.),(-1.,1.),.UNSPECIFIED.)
GEOMETRIC_REPRESENTATION_ITEM()
RATIONAL_B_SPLINE_SURFACE(((1.,1.),(1.,1.),(1.,1.),(1.,1.),(1.,1.),(1.,
1.),(1.,1.),(1.,1.),(1.,1.),(1.,1.),(1.,1.),(1.,1.),(1.,1.),(1.,1.),(1.,
1.),(1.,1.),(1.,1.),(1.,1.),(1.,1.),(1.,1.),(1.,1.),(1.,1.),(1.,1.),(1.,
1.),(1.,1.),(1.,1.),(1.,1.),(1.,1.),(1.,1.),(1.,1.),(1.,1.),(1.,1.),(1.,
1.),(1.,1.),(1.,1.),(1.,1.),(1.,1.),(1.,1.),(1.,1.),(1.,1.),(1.,1.),(1.,
1.),(1.,1.),(1.,1.),(1.,1.),(1.,1.),(1.,1.),(1.,1.),(1.,1.),(1.,1.),(1.,
1.),(1.,1.),(1.,1.),(1.,1.),(1.,1.),(1.,1.),(1.,1.),(1.,1.),(1.,1.),(1.,
1.),(1.,1.),(1.,1.),(1.,1.),(1.,1.),(1.,1.),(1.,1.),(1.,1.),(1.,1.),(1.,
1.),(1.,1.)))
REPRESENTATION_ITEM('')
SURFACE()
);
#168=(
BOUNDED_SURFACE()
B_SPLINE_SURFACE(5,1,((#72497,#72498),(#72499,#72500),(#72501,#72502),(#72503,
#72504),(#72505,#72506),(#72507,#72508),(#72509,#72510),(#72511,#72512),
(#72513,#72514),(#72515,#72516),(#72517,#72518),(#72519,#72520),(#72521,
#72522),(#72523,#72524),(#72525,#72526),(#72527,#72528),(#72529,#72530),
(#72531,#72532),(#72533,#72534),(#72535,#72536),(#72537,#72538),(#72539,
#72540),(#72541,#72542),(#72543,#72544),(#72545,#72546),(#72547,#72548),
(#72549,#72550),(#72551,#72552),(#72553,#72554),(#72555,#72556),(#72557,
#72558),(#72559,#72560),(#72561,#72562),(#72563,#72564),(#72565,#72566),
(#72567,#72568),(#72569,#72570),(#72571,#72572),(#72573,#72574),(#72575,
#72576),(#72577,#72578),(#72579,#72580),(#72581,#72582),(#72583,#72584),
(#72585,#72586),(#72587,#72588),(#72589,#72590),(#72591,#72592),(#72593,
#72594),(#72595,#72596),(#72597,#72598),(#72599,#72600),(#72601,#72602),
(#72603,#72604),(#72605,#72606),(#72607,#72608),(#72609,#72610),(#72611,
#72612),(#72613,#72614),(#72615,#72616),(#72617,#72618),(#72619,#72620),
(#72621,#72622),(#72623,#72624),(#72625,#72626),(#72627,#72628),(#72629,
#72630),(#72631,#72632),(#72633,#72634),(#72635,#72636)),.UNSPECIFIED.,
 .F.,.F.,.F.)
B_SPLINE_SURFACE_WITH_KNOTS((6,1,1,1,1,1,1,1,1,1,1,1,1,1,1,1,1,1,1,1,1,
1,1,1,1,1,1,1,1,1,1,1,1,1,1,1,1,1,1,1,1,1,1,1,1,1,1,1,1,1,1,1,1,1,1,1,1,
1,1,1,1,1,1,1,1,6),(2,2),(-1.,-0.984615384615383,-0.969230769230768,-0.953846153846152,
-0.938461538461537,-0.923076923076922,-0.907692307692306,-0.892307692307691,
-0.876923076923076,-0.86153846153846,-0.846153846153845,-0.83076923076923,
-0.815384615384614,-0.799999999999999,-0.784615384615384,-0.769230769230768,
-0.753846153846153,-0.738461538461538,-0.723076923076922,-0.707692307692307,
-0.692307692307692,-0.676923076923076,-0.661538461538461,-0.646153846153846,
-0.63076923076923,-0.615384615384615,-0.6,-0.584615384615384,-0.569230769230769,
-0.553846153846154,-0.538461538461538,-0.523076923076923,-0.507692307692308,
-0.492307692307692,-0.476923076923077,-0.461538461538462,-0.446153846153846,
-0.430769230769231,-0.415384615384615,-0.4,-0.384615384615385,-0.369230769230769,
-0.353846153846154,-0.338461538461538,-0.323076923076923,-0.307692307692308,
-0.292307692307692,-0.276923076923077,-0.261538461538462,-0.246153846153846,
-0.230769230769231,-0.215384615384615,-0.2,-0.184615384615385,-0.169230769230769,
-0.153846153846154,-0.138461538461538,-0.123076923076923,-0.107692307692308,
-0.0923076923076923,-0.0769230769230769,-0.0615384615384615,-0.0461538461538462,
-0.0307692307692308,-0.0153846153846154,0.),(-1.,1.),.UNSPECIFIED.)
GEOMETRIC_REPRESENTATION_ITEM()
RATIONAL_B_SPLINE_SURFACE(((1.,1.),(1.,1.),(1.,1.),(1.,1.),(1.,1.),(1.,
1.),(1.,1.),(1.,1.),(1.,1.),(1.,1.),(1.,1.),(1.,1.),(1.,1.),(1.,1.),(1.,
1.),(1.,1.),(1.,1.),(1.,1.),(1.,1.),(1.,1.),(1.,1.),(1.,1.),(1.,1.),(1.,
1.),(1.,1.),(1.,1.),(1.,1.),(1.,1.),(1.,1.),(1.,1.),(1.,1.),(1.,1.),(1.,
1.),(1.,1.),(1.,1.),(1.,1.),(1.,1.),(1.,1.),(1.,1.),(1.,1.),(1.,1.),(1.,
1.),(1.,1.),(1.,1.),(1.,1.),(1.,1.),(1.,1.),(1.,1.),(1.,1.),(1.,1.),(1.,
1.),(1.,1.),(1.,1.),(1.,1.),(1.,1.),(1.,1.),(1.,1.),(1.,1.),(1.,1.),(1.,
1.),(1.,1.),(1.,1.),(1.,1.),(1.,1.),(1.,1.),(1.,1.),(1.,1.),(1.,1.),(1.,
1.),(1.,1.)))
REPRESENTATION_ITEM('')
SURFACE()
);
#169=(
BOUNDED_SURFACE()
B_SPLINE_SURFACE(5,1,((#72723,#72724),(#72725,#72726),(#72727,#72728),(#72729,
#72730),(#72731,#72732),(#72733,#72734),(#72735,#72736),(#72737,#72738),
(#72739,#72740),(#72741,#72742),(#72743,#72744),(#72745,#72746),(#72747,
#72748),(#72749,#72750),(#72751,#72752),(#72753,#72754),(#72755,#72756),
(#72757,#72758),(#72759,#72760),(#72761,#72762),(#72763,#72764),(#72765,
#72766),(#72767,#72768),(#72769,#72770),(#72771,#72772),(#72773,#72774),
(#72775,#72776),(#72777,#72778),(#72779,#72780),(#72781,#72782),(#72783,
#72784),(#72785,#72786),(#72787,#72788),(#72789,#72790),(#72791,#72792),
(#72793,#72794),(#72795,#72796),(#72797,#72798),(#72799,#72800),(#72801,
#72802),(#72803,#72804),(#72805,#72806),(#72807,#72808),(#72809,#72810),
(#72811,#72812),(#72813,#72814),(#72815,#72816),(#72817,#72818),(#72819,
#72820),(#72821,#72822),(#72823,#72824),(#72825,#72826),(#72827,#72828),
(#72829,#72830),(#72831,#72832),(#72833,#72834),(#72835,#72836),(#72837,
#72838),(#72839,#72840),(#72841,#72842),(#72843,#72844),(#72845,#72846),
(#72847,#72848),(#72849,#72850),(#72851,#72852),(#72853,#72854),(#72855,
#72856),(#72857,#72858),(#72859,#72860),(#72861,#72862)),.UNSPECIFIED.,
 .F.,.F.,.F.)
B_SPLINE_SURFACE_WITH_KNOTS((6,1,1,1,1,1,1,1,1,1,1,1,1,1,1,1,1,1,1,1,1,
1,1,1,1,1,1,1,1,1,1,1,1,1,1,1,1,1,1,1,1,1,1,1,1,1,1,1,1,1,1,1,1,1,1,1,1,
1,1,1,1,1,1,1,1,6),(2,2),(-1.,-0.984615384615383,-0.969230769230768,-0.953846153846152,
-0.938461538461537,-0.923076923076922,-0.907692307692306,-0.892307692307691,
-0.876923076923076,-0.86153846153846,-0.846153846153845,-0.83076923076923,
-0.815384615384614,-0.799999999999999,-0.784615384615384,-0.769230769230768,
-0.753846153846153,-0.738461538461538,-0.723076923076922,-0.707692307692307,
-0.692307692307692,-0.676923076923076,-0.661538461538461,-0.646153846153846,
-0.63076923076923,-0.615384615384615,-0.6,-0.584615384615384,-0.569230769230769,
-0.553846153846154,-0.538461538461538,-0.523076923076923,-0.507692307692308,
-0.492307692307692,-0.476923076923077,-0.461538461538462,-0.446153846153846,
-0.430769230769231,-0.415384615384615,-0.4,-0.384615384615385,-0.369230769230769,
-0.353846153846154,-0.338461538461538,-0.323076923076923,-0.307692307692308,
-0.292307692307692,-0.276923076923077,-0.261538461538462,-0.246153846153846,
-0.230769230769231,-0.215384615384615,-0.2,-0.184615384615385,-0.169230769230769,
-0.153846153846154,-0.138461538461538,-0.123076923076923,-0.107692307692308,
-0.0923076923076923,-0.0769230769230769,-0.0615384615384615,-0.0461538461538462,
-0.0307692307692308,-0.0153846153846154,0.),(-1.,1.),.UNSPECIFIED.)
GEOMETRIC_REPRESENTATION_ITEM()
RATIONAL_B_SPLINE_SURFACE(((1.,1.),(1.,1.),(1.,1.),(1.,1.),(1.,1.),(1.,
1.),(1.,1.),(1.,1.),(1.,1.),(1.,1.),(1.,1.),(1.,1.),(1.,1.),(1.,1.),(1.,
1.),(1.,1.),(1.,1.),(1.,1.),(1.,1.),(1.,1.),(1.,1.),(1.,1.),(1.,1.),(1.,
1.),(1.,1.),(1.,1.),(1.,1.),(1.,1.),(1.,1.),(1.,1.),(1.,1.),(1.,1.),(1.,
1.),(1.,1.),(1.,1.),(1.,1.),(1.,1.),(1.,1.),(1.,1.),(1.,1.),(1.,1.),(1.,
1.),(1.,1.),(1.,1.),(1.,1.),(1.,1.),(1.,1.),(1.,1.),(1.,1.),(1.,1.),(1.,
1.),(1.,1.),(1.,1.),(1.,1.),(1.,1.),(1.,1.),(1.,1.),(1.,1.),(1.,1.),(1.,
1.),(1.,1.),(1.,1.),(1.,1.),(1.,1.),(1.,1.),(1.,1.),(1.,1.),(1.,1.),(1.,
1.),(1.,1.)))
REPRESENTATION_ITEM('')
SURFACE()
);
#170=(
BOUNDED_SURFACE()
B_SPLINE_SURFACE(5,1,((#72942,#72943),(#72944,#72945),(#72946,#72947),(#72948,
#72949),(#72950,#72951),(#72952,#72953),(#72954,#72955),(#72956,#72957),
(#72958,#72959),(#72960,#72961),(#72962,#72963),(#72964,#72965),(#72966,
#72967),(#72968,#72969),(#72970,#72971),(#72972,#72973),(#72974,#72975),
(#72976,#72977),(#72978,#72979),(#72980,#72981),(#72982,#72983),(#72984,
#72985),(#72986,#72987),(#72988,#72989),(#72990,#72991),(#72992,#72993),
(#72994,#72995),(#72996,#72997),(#72998,#72999),(#73000,#73001),(#73002,
#73003),(#73004,#73005),(#73006,#73007),(#73008,#73009),(#73010,#73011),
(#73012,#73013),(#73014,#73015),(#73016,#73017),(#73018,#73019),(#73020,
#73021),(#73022,#73023),(#73024,#73025),(#73026,#73027),(#73028,#73029),
(#73030,#73031),(#73032,#73033),(#73034,#73035),(#73036,#73037),(#73038,
#73039),(#73040,#73041),(#73042,#73043),(#73044,#73045),(#73046,#73047),
(#73048,#73049),(#73050,#73051),(#73052,#73053),(#73054,#73055),(#73056,
#73057),(#73058,#73059),(#73060,#73061),(#73062,#73063),(#73064,#73065),
(#73066,#73067),(#73068,#73069),(#73070,#73071),(#73072,#73073),(#73074,
#73075),(#73076,#73077),(#73078,#73079),(#73080,#73081)),.UNSPECIFIED.,
 .F.,.F.,.F.)
B_SPLINE_SURFACE_WITH_KNOTS((6,1,1,1,1,1,1,1,1,1,1,1,1,1,1,1,1,1,1,1,1,
1,1,1,1,1,1,1,1,1,1,1,1,1,1,1,1,1,1,1,1,1,1,1,1,1,1,1,1,1,1,1,1,1,1,1,1,
1,1,1,1,1,1,1,1,6),(2,2),(-1.,-0.984615384615383,-0.969230769230768,-0.953846153846152,
-0.938461538461537,-0.923076923076922,-0.907692307692306,-0.892307692307691,
-0.876923076923076,-0.86153846153846,-0.846153846153845,-0.83076923076923,
-0.815384615384614,-0.799999999999999,-0.784615384615384,-0.769230769230768,
-0.753846153846153,-0.738461538461538,-0.723076923076922,-0.707692307692307,
-0.692307692307692,-0.676923076923076,-0.661538461538461,-0.646153846153846,
-0.63076923076923,-0.615384615384615,-0.6,-0.584615384615384,-0.569230769230769,
-0.553846153846154,-0.538461538461538,-0.523076923076923,-0.507692307692308,
-0.492307692307692,-0.476923076923077,-0.461538461538462,-0.446153846153846,
-0.430769230769231,-0.415384615384615,-0.4,-0.384615384615385,-0.369230769230769,
-0.353846153846154,-0.338461538461538,-0.323076923076923,-0.307692307692308,
-0.292307692307692,-0.276923076923077,-0.261538461538462,-0.246153846153846,
-0.230769230769231,-0.215384615384615,-0.2,-0.184615384615385,-0.169230769230769,
-0.153846153846154,-0.138461538461538,-0.123076923076923,-0.107692307692308,
-0.0923076923076923,-0.0769230769230769,-0.0615384615384615,-0.0461538461538462,
-0.0307692307692308,-0.0153846153846154,0.),(-1.,1.),.UNSPECIFIED.)
GEOMETRIC_REPRESENTATION_ITEM()
RATIONAL_B_SPLINE_SURFACE(((1.,1.),(1.,1.),(1.,1.),(1.,1.),(1.,1.),(1.,
1.),(1.,1.),(1.,1.),(1.,1.),(1.,1.),(1.,1.),(1.,1.),(1.,1.),(1.,1.),(1.,
1.),(1.,1.),(1.,1.),(1.,1.),(1.,1.),(1.,1.),(1.,1.),(1.,1.),(1.,1.),(1.,
1.),(1.,1.),(1.,1.),(1.,1.),(1.,1.),(1.,1.),(1.,1.),(1.,1.),(1.,1.),(1.,
1.),(1.,1.),(1.,1.),(1.,1.),(1.,1.),(1.,1.),(1.,1.),(1.,1.),(1.,1.),(1.,
1.),(1.,1.),(1.,1.),(1.,1.),(1.,1.),(1.,1.),(1.,1.),(1.,1.),(1.,1.),(1.,
1.),(1.,1.),(1.,1.),(1.,1.),(1.,1.),(1.,1.),(1.,1.),(1.,1.),(1.,1.),(1.,
1.),(1.,1.),(1.,1.),(1.,1.),(1.,1.),(1.,1.),(1.,1.),(1.,1.),(1.,1.),(1.,
1.),(1.,1.)))
REPRESENTATION_ITEM('')
SURFACE()
);
#171=(
BOUNDED_CURVE()
B_SPLINE_CURVE(5,(#25718,#25719,#25720,#25721,#25722,#25723,#25724,#25725,
#25726,#25727,#25728,#25729,#25730,#25731,#25732,#25733,#25734,#25735,#25736,
#25737,#25738,#25739,#25740,#25741,#25742,#25743,#25744,#25745,#25746,#25747,
#25748,#25749,#25750,#25751,#25752,#25753,#25754,#25755,#25756,#25757,#25758,
#25759,#25760,#25761,#25762,#25763,#25764,#25765,#25766,#25767,#25768,#25769,
#25770,#25771,#25772,#25773,#25774,#25775,#25776,#25777,#25778,#25779,#25780,
#25781,#25782,#25783,#25784,#25785,#25786,#25787),.UNSPECIFIED.,.F.,.F.)
B_SPLINE_CURVE_WITH_KNOTS((6,1,1,1,1,1,1,1,1,1,1,1,1,1,1,1,1,1,1,1,1,1,
1,1,1,1,1,1,1,1,1,1,1,1,1,1,1,1,1,1,1,1,1,1,1,1,1,1,1,1,1,1,1,1,1,1,1,1,
1,1,1,1,1,1,1,6),(0.,0.0153846153846154,0.0307692307692308,0.0461538461538462,
0.0615384615384615,0.0769230769230769,0.0923076923076923,0.107692307692308,
0.123076923076923,0.138461538461538,0.153846153846154,0.169230769230769,
0.184615384615385,0.2,0.215384615384615,0.230769230769231,0.246153846153846,
0.261538461538462,0.276923076923077,0.292307692307692,0.307692307692308,
0.323076923076923,0.338461538461538,0.353846153846154,0.369230769230769,
0.384615384615385,0.4,0.415384615384615,0.430769230769231,0.446153846153846,
0.461538461538462,0.476923076923077,0.492307692307692,0.507692307692308,
0.523076923076923,0.538461538461538,0.553846153846154,0.569230769230769,
0.584615384615384,0.6,0.615384615384615,0.63076923076923,0.646153846153846,
0.661538461538461,0.676923076923076,0.692307692307692,0.707692307692307,
0.723076923076922,0.738461538461538,0.753846153846153,0.769230769230768,
0.784615384615384,0.799999999999999,0.815384615384614,0.83076923076923,
0.846153846153845,0.86153846153846,0.876923076923076,0.892307692307691,
0.907692307692306,0.923076923076922,0.938461538461537,0.953846153846152,
0.969230769230768,0.984615384615383,1.),.UNSPECIFIED.)
CURVE()
GEOMETRIC_REPRESENTATION_ITEM()
RATIONAL_B_SPLINE_CURVE((1.,1.,1.,1.,1.,1.,1.,1.,1.,1.,1.,1.,1.,1.,1.,1.,
1.,1.,1.,1.,1.,1.,1.,1.,1.,1.,1.,1.,1.,1.,1.,1.,1.,1.,1.,1.,1.,1.,1.,1.,
1.,1.,1.,1.,1.,1.,1.,1.,1.,1.,1.,1.,1.,1.,1.,1.,1.,1.,1.,1.,1.,1.,1.,1.,
1.,1.,1.,1.,1.,1.))
REPRESENTATION_ITEM('')
);
#172=(
BOUNDED_CURVE()
B_SPLINE_CURVE(5,(#25791,#25792,#25793,#25794,#25795,#25796,#25797,#25798,
#25799,#25800,#25801,#25802,#25803,#25804,#25805,#25806,#25807,#25808,#25809,
#25810,#25811,#25812,#25813,#25814,#25815,#25816,#25817,#25818,#25819,#25820,
#25821,#25822,#25823,#25824,#25825,#25826,#25827,#25828,#25829,#25830,#25831,
#25832,#25833,#25834,#25835,#25836,#25837,#25838,#25839,#25840,#25841,#25842,
#25843,#25844,#25845,#25846,#25847,#25848,#25849,#25850,#25851,#25852,#25853,
#25854,#25855,#25856,#25857,#25858,#25859,#25860),.UNSPECIFIED.,.F.,.F.)
B_SPLINE_CURVE_WITH_KNOTS((6,1,1,1,1,1,1,1,1,1,1,1,1,1,1,1,1,1,1,1,1,1,
1,1,1,1,1,1,1,1,1,1,1,1,1,1,1,1,1,1,1,1,1,1,1,1,1,1,1,1,1,1,1,1,1,1,1,1,
1,1,1,1,1,1,1,6),(0.,0.0153846153846154,0.0307692307692308,0.0461538461538462,
0.0615384615384615,0.0769230769230769,0.0923076923076923,0.107692307692308,
0.123076923076923,0.138461538461538,0.153846153846154,0.169230769230769,
0.184615384615385,0.2,0.215384615384615,0.230769230769231,0.246153846153846,
0.261538461538462,0.276923076923077,0.292307692307692,0.307692307692308,
0.323076923076923,0.338461538461538,0.353846153846154,0.369230769230769,
0.384615384615385,0.4,0.415384615384615,0.430769230769231,0.446153846153846,
0.461538461538462,0.476923076923077,0.492307692307692,0.507692307692308,
0.523076923076923,0.538461538461538,0.553846153846154,0.569230769230769,
0.584615384615384,0.6,0.615384615384615,0.63076923076923,0.646153846153846,
0.661538461538461,0.676923076923076,0.692307692307692,0.707692307692307,
0.723076923076922,0.738461538461538,0.753846153846153,0.769230769230768,
0.784615384615384,0.799999999999999,0.815384615384614,0.83076923076923,
0.846153846153845,0.86153846153846,0.876923076923076,0.892307692307691,
0.907692307692306,0.923076923076922,0.938461538461537,0.953846153846152,
0.969230769230768,0.984615384615383,1.),.UNSPECIFIED.)
CURVE()
GEOMETRIC_REPRESENTATION_ITEM()
RATIONAL_B_SPLINE_CURVE((1.,1.,1.,1.,1.,1.,1.,1.,1.,1.,1.,1.,1.,1.,1.,1.,
1.,1.,1.,1.,1.,1.,1.,1.,1.,1.,1.,1.,1.,1.,1.,1.,1.,1.,1.,1.,1.,1.,1.,1.,
1.,1.,1.,1.,1.,1.,1.,1.,1.,1.,1.,1.,1.,1.,1.,1.,1.,1.,1.,1.,1.,1.,1.,1.,
1.,1.,1.,1.,1.,1.))
REPRESENTATION_ITEM('')
);
#173=(
BOUNDED_CURVE()
B_SPLINE_CURVE(5,(#25864,#25865,#25866,#25867,#25868,#25869,#25870,#25871,
#25872,#25873,#25874,#25875,#25876,#25877,#25878,#25879,#25880,#25881,#25882,
#25883,#25884,#25885,#25886,#25887,#25888,#25889,#25890,#25891,#25892,#25893,
#25894,#25895,#25896,#25897,#25898,#25899,#25900,#25901,#25902,#25903,#25904,
#25905,#25906,#25907,#25908,#25909,#25910,#25911,#25912,#25913,#25914,#25915,
#25916,#25917,#25918,#25919,#25920,#25921,#25922,#25923,#25924,#25925,#25926,
#25927,#25928,#25929,#25930,#25931,#25932,#25933),.UNSPECIFIED.,.F.,.F.)
B_SPLINE_CURVE_WITH_KNOTS((6,1,1,1,1,1,1,1,1,1,1,1,1,1,1,1,1,1,1,1,1,1,
1,1,1,1,1,1,1,1,1,1,1,1,1,1,1,1,1,1,1,1,1,1,1,1,1,1,1,1,1,1,1,1,1,1,1,1,
1,1,1,1,1,1,1,6),(0.,0.0153846153846154,0.0307692307692308,0.0461538461538462,
0.0615384615384615,0.0769230769230769,0.0923076923076923,0.107692307692308,
0.123076923076923,0.138461538461538,0.153846153846154,0.169230769230769,
0.184615384615385,0.2,0.215384615384615,0.230769230769231,0.246153846153846,
0.261538461538462,0.276923076923077,0.292307692307692,0.307692307692308,
0.323076923076923,0.338461538461538,0.353846153846154,0.369230769230769,
0.384615384615385,0.4,0.415384615384615,0.430769230769231,0.446153846153846,
0.461538461538462,0.476923076923077,0.492307692307692,0.507692307692308,
0.523076923076923,0.538461538461538,0.553846153846154,0.569230769230769,
0.584615384615384,0.6,0.615384615384615,0.63076923076923,0.646153846153846,
0.661538461538461,0.676923076923076,0.692307692307692,0.707692307692307,
0.723076923076922,0.738461538461538,0.753846153846153,0.769230769230768,
0.784615384615384,0.799999999999999,0.815384615384614,0.83076923076923,
0.846153846153845,0.86153846153846,0.876923076923076,0.892307692307691,
0.907692307692306,0.923076923076922,0.938461538461537,0.953846153846152,
0.969230769230768,0.984615384615383,1.),.UNSPECIFIED.)
CURVE()
GEOMETRIC_REPRESENTATION_ITEM()
RATIONAL_B_SPLINE_CURVE((1.,1.,1.,1.,1.,1.,1.,1.,1.,1.,1.,1.,1.,1.,1.,1.,
1.,1.,1.,1.,1.,1.,1.,1.,1.,1.,1.,1.,1.,1.,1.,1.,1.,1.,1.,1.,1.,1.,1.,1.,
1.,1.,1.,1.,1.,1.,1.,1.,1.,1.,1.,1.,1.,1.,1.,1.,1.,1.,1.,1.,1.,1.,1.,1.,
1.,1.,1.,1.,1.,1.))
REPRESENTATION_ITEM('')
);
#174=(
BOUNDED_CURVE()
B_SPLINE_CURVE(5,(#25937,#25938,#25939,#25940,#25941,#25942,#25943,#25944,
#25945,#25946,#25947,#25948,#25949,#25950,#25951,#25952,#25953,#25954,#25955,
#25956,#25957,#25958,#25959,#25960,#25961,#25962,#25963,#25964,#25965,#25966,
#25967,#25968,#25969,#25970,#25971,#25972,#25973,#25974,#25975,#25976,#25977,
#25978,#25979,#25980,#25981,#25982,#25983,#25984,#25985,#25986,#25987,#25988,
#25989,#25990,#25991,#25992,#25993,#25994,#25995,#25996,#25997,#25998,#25999,
#26000,#26001,#26002,#26003,#26004,#26005,#26006),.UNSPECIFIED.,.F.,.F.)
B_SPLINE_CURVE_WITH_KNOTS((6,1,1,1,1,1,1,1,1,1,1,1,1,1,1,1,1,1,1,1,1,1,
1,1,1,1,1,1,1,1,1,1,1,1,1,1,1,1,1,1,1,1,1,1,1,1,1,1,1,1,1,1,1,1,1,1,1,1,
1,1,1,1,1,1,1,6),(0.,0.0153846153846154,0.0307692307692308,0.0461538461538462,
0.0615384615384615,0.0769230769230769,0.0923076923076923,0.107692307692308,
0.123076923076923,0.138461538461538,0.153846153846154,0.169230769230769,
0.184615384615385,0.2,0.215384615384615,0.230769230769231,0.246153846153846,
0.261538461538462,0.276923076923077,0.292307692307692,0.307692307692308,
0.323076923076923,0.338461538461538,0.353846153846154,0.369230769230769,
0.384615384615385,0.4,0.415384615384615,0.430769230769231,0.446153846153846,
0.461538461538462,0.476923076923077,0.492307692307692,0.507692307692308,
0.523076923076923,0.538461538461538,0.553846153846154,0.569230769230769,
0.584615384615384,0.6,0.615384615384615,0.63076923076923,0.646153846153846,
0.661538461538461,0.676923076923076,0.692307692307692,0.707692307692307,
0.723076923076922,0.738461538461538,0.753846153846153,0.769230769230768,
0.784615384615384,0.799999999999999,0.815384615384614,0.83076923076923,
0.846153846153845,0.86153846153846,0.876923076923076,0.892307692307691,
0.907692307692306,0.923076923076922,0.938461538461537,0.953846153846152,
0.969230769230768,0.984615384615383,1.),.UNSPECIFIED.)
CURVE()
GEOMETRIC_REPRESENTATION_ITEM()
RATIONAL_B_SPLINE_CURVE((1.,1.,1.,1.,1.,1.,1.,1.,1.,1.,1.,1.,1.,1.,1.,1.,
1.,1.,1.,1.,1.,1.,1.,1.,1.,1.,1.,1.,1.,1.,1.,1.,1.,1.,1.,1.,1.,1.,1.,1.,
1.,1.,1.,1.,1.,1.,1.,1.,1.,1.,1.,1.,1.,1.,1.,1.,1.,1.,1.,1.,1.,1.,1.,1.,
1.,1.,1.,1.,1.,1.))
REPRESENTATION_ITEM('')
);
#175=(
BOUNDED_CURVE()
B_SPLINE_CURVE(5,(#26010,#26011,#26012,#26013,#26014,#26015,#26016,#26017,
#26018,#26019,#26020,#26021,#26022,#26023,#26024,#26025,#26026,#26027,#26028,
#26029,#26030,#26031,#26032,#26033,#26034,#26035,#26036,#26037,#26038,#26039,
#26040,#26041,#26042,#26043,#26044,#26045,#26046,#26047,#26048,#26049,#26050,
#26051,#26052,#26053,#26054,#26055,#26056,#26057,#26058,#26059,#26060,#26061,
#26062,#26063,#26064,#26065,#26066,#26067,#26068,#26069,#26070,#26071,#26072,
#26073,#26074,#26075,#26076,#26077,#26078,#26079),.UNSPECIFIED.,.F.,.F.)
B_SPLINE_CURVE_WITH_KNOTS((6,1,1,1,1,1,1,1,1,1,1,1,1,1,1,1,1,1,1,1,1,1,
1,1,1,1,1,1,1,1,1,1,1,1,1,1,1,1,1,1,1,1,1,1,1,1,1,1,1,1,1,1,1,1,1,1,1,1,
1,1,1,1,1,1,1,6),(0.,0.0153846153846154,0.0307692307692308,0.0461538461538462,
0.0615384615384615,0.0769230769230769,0.0923076923076923,0.107692307692308,
0.123076923076923,0.138461538461538,0.153846153846154,0.169230769230769,
0.184615384615385,0.2,0.215384615384615,0.230769230769231,0.246153846153846,
0.261538461538462,0.276923076923077,0.292307692307692,0.307692307692308,
0.323076923076923,0.338461538461538,0.353846153846154,0.369230769230769,
0.384615384615385,0.4,0.415384615384615,0.430769230769231,0.446153846153846,
0.461538461538462,0.476923076923077,0.492307692307692,0.507692307692308,
0.523076923076923,0.538461538461538,0.553846153846154,0.569230769230769,
0.584615384615384,0.6,0.615384615384615,0.63076923076923,0.646153846153846,
0.661538461538461,0.676923076923076,0.692307692307692,0.707692307692307,
0.723076923076922,0.738461538461538,0.753846153846153,0.769230769230768,
0.784615384615384,0.799999999999999,0.815384615384614,0.83076923076923,
0.846153846153845,0.86153846153846,0.876923076923076,0.892307692307691,
0.907692307692306,0.923076923076922,0.938461538461537,0.953846153846152,
0.969230769230768,0.984615384615383,1.),.UNSPECIFIED.)
CURVE()
GEOMETRIC_REPRESENTATION_ITEM()
RATIONAL_B_SPLINE_CURVE((1.,1.,1.,1.,1.,1.,1.,1.,1.,1.,1.,1.,1.,1.,1.,1.,
1.,1.,1.,1.,1.,1.,1.,1.,1.,1.,1.,1.,1.,1.,1.,1.,1.,1.,1.,1.,1.,1.,1.,1.,
1.,1.,1.,1.,1.,1.,1.,1.,1.,1.,1.,1.,1.,1.,1.,1.,1.,1.,1.,1.,1.,1.,1.,1.,
1.,1.,1.,1.,1.,1.))
REPRESENTATION_ITEM('')
);
#176=(
BOUNDED_CURVE()
B_SPLINE_CURVE(5,(#26083,#26084,#26085,#26086,#26087,#26088,#26089,#26090,
#26091,#26092,#26093,#26094,#26095,#26096,#26097,#26098,#26099,#26100,#26101,
#26102,#26103,#26104,#26105,#26106,#26107,#26108,#26109,#26110,#26111,#26112,
#26113,#26114,#26115,#26116,#26117,#26118,#26119,#26120,#26121,#26122,#26123,
#26124,#26125,#26126,#26127,#26128,#26129,#26130,#26131,#26132,#26133,#26134,
#26135,#26136,#26137,#26138,#26139,#26140,#26141,#26142,#26143,#26144,#26145,
#26146,#26147,#26148,#26149,#26150,#26151,#26152),.UNSPECIFIED.,.F.,.F.)
B_SPLINE_CURVE_WITH_KNOTS((6,1,1,1,1,1,1,1,1,1,1,1,1,1,1,1,1,1,1,1,1,1,
1,1,1,1,1,1,1,1,1,1,1,1,1,1,1,1,1,1,1,1,1,1,1,1,1,1,1,1,1,1,1,1,1,1,1,1,
1,1,1,1,1,1,1,6),(0.,0.0153846153846154,0.0307692307692308,0.0461538461538462,
0.0615384615384615,0.0769230769230769,0.0923076923076923,0.107692307692308,
0.123076923076923,0.138461538461538,0.153846153846154,0.169230769230769,
0.184615384615385,0.2,0.215384615384615,0.230769230769231,0.246153846153846,
0.261538461538462,0.276923076923077,0.292307692307692,0.307692307692308,
0.323076923076923,0.338461538461538,0.353846153846154,0.369230769230769,
0.384615384615385,0.4,0.415384615384615,0.430769230769231,0.446153846153846,
0.461538461538462,0.476923076923077,0.492307692307692,0.507692307692308,
0.523076923076923,0.538461538461538,0.553846153846154,0.569230769230769,
0.584615384615384,0.6,0.615384615384615,0.63076923076923,0.646153846153846,
0.661538461538461,0.676923076923076,0.692307692307692,0.707692307692307,
0.723076923076922,0.738461538461538,0.753846153846153,0.769230769230768,
0.784615384615384,0.799999999999999,0.815384615384614,0.83076923076923,
0.846153846153845,0.86153846153846,0.876923076923076,0.892307692307691,
0.907692307692306,0.923076923076922,0.938461538461537,0.953846153846152,
0.969230769230768,0.984615384615383,1.),.UNSPECIFIED.)
CURVE()
GEOMETRIC_REPRESENTATION_ITEM()
RATIONAL_B_SPLINE_CURVE((1.,1.,1.,1.,1.,1.,1.,1.,1.,1.,1.,1.,1.,1.,1.,1.,
1.,1.,1.,1.,1.,1.,1.,1.,1.,1.,1.,1.,1.,1.,1.,1.,1.,1.,1.,1.,1.,1.,1.,1.,
1.,1.,1.,1.,1.,1.,1.,1.,1.,1.,1.,1.,1.,1.,1.,1.,1.,1.,1.,1.,1.,1.,1.,1.,
1.,1.,1.,1.,1.,1.))
REPRESENTATION_ITEM('')
);
#177=(
BOUNDED_CURVE()
B_SPLINE_CURVE(5,(#26156,#26157,#26158,#26159,#26160,#26161,#26162,#26163,
#26164,#26165,#26166,#26167,#26168,#26169,#26170,#26171,#26172,#26173,#26174,
#26175,#26176,#26177,#26178,#26179,#26180,#26181,#26182,#26183,#26184,#26185,
#26186,#26187,#26188,#26189,#26190,#26191,#26192,#26193,#26194,#26195,#26196,
#26197,#26198,#26199,#26200,#26201,#26202,#26203,#26204,#26205,#26206,#26207,
#26208,#26209,#26210,#26211,#26212,#26213,#26214,#26215,#26216,#26217,#26218,
#26219,#26220,#26221,#26222,#26223,#26224,#26225),.UNSPECIFIED.,.F.,.F.)
B_SPLINE_CURVE_WITH_KNOTS((6,1,1,1,1,1,1,1,1,1,1,1,1,1,1,1,1,1,1,1,1,1,
1,1,1,1,1,1,1,1,1,1,1,1,1,1,1,1,1,1,1,1,1,1,1,1,1,1,1,1,1,1,1,1,1,1,1,1,
1,1,1,1,1,1,1,6),(0.,0.0153846153846154,0.0307692307692308,0.0461538461538462,
0.0615384615384615,0.0769230769230769,0.0923076923076923,0.107692307692308,
0.123076923076923,0.138461538461538,0.153846153846154,0.169230769230769,
0.184615384615385,0.2,0.215384615384615,0.230769230769231,0.246153846153846,
0.261538461538462,0.276923076923077,0.292307692307692,0.307692307692308,
0.323076923076923,0.338461538461538,0.353846153846154,0.369230769230769,
0.384615384615385,0.4,0.415384615384615,0.430769230769231,0.446153846153846,
0.461538461538462,0.476923076923077,0.492307692307692,0.507692307692308,
0.523076923076923,0.538461538461538,0.553846153846154,0.569230769230769,
0.584615384615384,0.6,0.615384615384615,0.63076923076923,0.646153846153846,
0.661538461538461,0.676923076923076,0.692307692307692,0.707692307692307,
0.723076923076922,0.738461538461538,0.753846153846153,0.769230769230768,
0.784615384615384,0.799999999999999,0.815384615384614,0.83076923076923,
0.846153846153845,0.86153846153846,0.876923076923076,0.892307692307691,
0.907692307692306,0.923076923076922,0.938461538461537,0.953846153846152,
0.969230769230768,0.984615384615383,1.),.UNSPECIFIED.)
CURVE()
GEOMETRIC_REPRESENTATION_ITEM()
RATIONAL_B_SPLINE_CURVE((1.,1.,1.,1.,1.,1.,1.,1.,1.,1.,1.,1.,1.,1.,1.,1.,
1.,1.,1.,1.,1.,1.,1.,1.,1.,1.,1.,1.,1.,1.,1.,1.,1.,1.,1.,1.,1.,1.,1.,1.,
1.,1.,1.,1.,1.,1.,1.,1.,1.,1.,1.,1.,1.,1.,1.,1.,1.,1.,1.,1.,1.,1.,1.,1.,
1.,1.,1.,1.,1.,1.))
REPRESENTATION_ITEM('')
);
#178=(
BOUNDED_CURVE()
B_SPLINE_CURVE(5,(#26229,#26230,#26231,#26232,#26233,#26234,#26235,#26236,
#26237,#26238,#26239,#26240,#26241,#26242,#26243,#26244,#26245,#26246,#26247,
#26248,#26249,#26250,#26251,#26252,#26253,#26254,#26255,#26256,#26257,#26258,
#26259,#26260,#26261,#26262,#26263,#26264,#26265,#26266,#26267,#26268,#26269,
#26270,#26271,#26272,#26273,#26274,#26275,#26276,#26277,#26278,#26279,#26280,
#26281,#26282,#26283,#26284,#26285,#26286,#26287,#26288,#26289,#26290,#26291,
#26292,#26293,#26294,#26295,#26296,#26297,#26298),.UNSPECIFIED.,.F.,.F.)
B_SPLINE_CURVE_WITH_KNOTS((6,1,1,1,1,1,1,1,1,1,1,1,1,1,1,1,1,1,1,1,1,1,
1,1,1,1,1,1,1,1,1,1,1,1,1,1,1,1,1,1,1,1,1,1,1,1,1,1,1,1,1,1,1,1,1,1,1,1,
1,1,1,1,1,1,1,6),(0.,0.0153846153846154,0.0307692307692308,0.0461538461538462,
0.0615384615384615,0.0769230769230769,0.0923076923076923,0.107692307692308,
0.123076923076923,0.138461538461538,0.153846153846154,0.169230769230769,
0.184615384615385,0.2,0.215384615384615,0.230769230769231,0.246153846153846,
0.261538461538462,0.276923076923077,0.292307692307692,0.307692307692308,
0.323076923076923,0.338461538461538,0.353846153846154,0.369230769230769,
0.384615384615385,0.4,0.415384615384615,0.430769230769231,0.446153846153846,
0.461538461538462,0.476923076923077,0.492307692307692,0.507692307692308,
0.523076923076923,0.538461538461538,0.553846153846154,0.569230769230769,
0.584615384615384,0.6,0.615384615384615,0.63076923076923,0.646153846153846,
0.661538461538461,0.676923076923076,0.692307692307692,0.707692307692307,
0.723076923076922,0.738461538461538,0.753846153846153,0.769230769230768,
0.784615384615384,0.799999999999999,0.815384615384614,0.83076923076923,
0.846153846153845,0.86153846153846,0.876923076923076,0.892307692307691,
0.907692307692306,0.923076923076922,0.938461538461537,0.953846153846152,
0.969230769230768,0.984615384615383,1.),.UNSPECIFIED.)
CURVE()
GEOMETRIC_REPRESENTATION_ITEM()
RATIONAL_B_SPLINE_CURVE((1.,1.,1.,1.,1.,1.,1.,1.,1.,1.,1.,1.,1.,1.,1.,1.,
1.,1.,1.,1.,1.,1.,1.,1.,1.,1.,1.,1.,1.,1.,1.,1.,1.,1.,1.,1.,1.,1.,1.,1.,
1.,1.,1.,1.,1.,1.,1.,1.,1.,1.,1.,1.,1.,1.,1.,1.,1.,1.,1.,1.,1.,1.,1.,1.,
1.,1.,1.,1.,1.,1.))
REPRESENTATION_ITEM('')
);
#179=(
BOUNDED_CURVE()
B_SPLINE_CURVE(5,(#26302,#26303,#26304,#26305,#26306,#26307,#26308,#26309,
#26310,#26311,#26312,#26313,#26314,#26315,#26316,#26317,#26318,#26319,#26320,
#26321,#26322,#26323,#26324,#26325,#26326,#26327,#26328,#26329,#26330,#26331,
#26332,#26333,#26334,#26335,#26336,#26337,#26338,#26339,#26340,#26341,#26342,
#26343,#26344,#26345,#26346,#26347,#26348,#26349,#26350,#26351,#26352,#26353,
#26354,#26355,#26356,#26357,#26358,#26359,#26360,#26361,#26362,#26363,#26364,
#26365,#26366,#26367,#26368,#26369,#26370,#26371),.UNSPECIFIED.,.F.,.F.)
B_SPLINE_CURVE_WITH_KNOTS((6,1,1,1,1,1,1,1,1,1,1,1,1,1,1,1,1,1,1,1,1,1,
1,1,1,1,1,1,1,1,1,1,1,1,1,1,1,1,1,1,1,1,1,1,1,1,1,1,1,1,1,1,1,1,1,1,1,1,
1,1,1,1,1,1,1,6),(0.,0.0153846153846154,0.0307692307692308,0.0461538461538462,
0.0615384615384615,0.0769230769230769,0.0923076923076923,0.107692307692308,
0.123076923076923,0.138461538461538,0.153846153846154,0.169230769230769,
0.184615384615385,0.2,0.215384615384615,0.230769230769231,0.246153846153846,
0.261538461538462,0.276923076923077,0.292307692307692,0.307692307692308,
0.323076923076923,0.338461538461538,0.353846153846154,0.369230769230769,
0.384615384615385,0.4,0.415384615384615,0.430769230769231,0.446153846153846,
0.461538461538462,0.476923076923077,0.492307692307692,0.507692307692308,
0.523076923076923,0.538461538461538,0.553846153846154,0.569230769230769,
0.584615384615384,0.6,0.615384615384615,0.63076923076923,0.646153846153846,
0.661538461538461,0.676923076923076,0.692307692307692,0.707692307692307,
0.723076923076922,0.738461538461538,0.753846153846153,0.769230769230768,
0.784615384615384,0.799999999999999,0.815384615384614,0.83076923076923,
0.846153846153845,0.86153846153846,0.876923076923076,0.892307692307691,
0.907692307692306,0.923076923076922,0.938461538461537,0.953846153846152,
0.969230769230768,0.984615384615383,1.),.UNSPECIFIED.)
CURVE()
GEOMETRIC_REPRESENTATION_ITEM()
RATIONAL_B_SPLINE_CURVE((1.,1.,1.,1.,1.,1.,1.,1.,1.,1.,1.,1.,1.,1.,1.,1.,
1.,1.,1.,1.,1.,1.,1.,1.,1.,1.,1.,1.,1.,1.,1.,1.,1.,1.,1.,1.,1.,1.,1.,1.,
1.,1.,1.,1.,1.,1.,1.,1.,1.,1.,1.,1.,1.,1.,1.,1.,1.,1.,1.,1.,1.,1.,1.,1.,
1.,1.,1.,1.,1.,1.))
REPRESENTATION_ITEM('')
);
#180=(
BOUNDED_CURVE()
B_SPLINE_CURVE(5,(#26375,#26376,#26377,#26378,#26379,#26380,#26381,#26382,
#26383,#26384,#26385,#26386,#26387,#26388,#26389,#26390,#26391,#26392,#26393,
#26394,#26395,#26396,#26397,#26398,#26399,#26400,#26401,#26402,#26403,#26404,
#26405,#26406,#26407,#26408,#26409,#26410,#26411,#26412,#26413,#26414,#26415,
#26416,#26417,#26418,#26419,#26420,#26421,#26422,#26423,#26424,#26425,#26426,
#26427,#26428,#26429,#26430,#26431,#26432,#26433,#26434,#26435,#26436,#26437,
#26438,#26439,#26440,#26441,#26442,#26443,#26444),.UNSPECIFIED.,.F.,.F.)
B_SPLINE_CURVE_WITH_KNOTS((6,1,1,1,1,1,1,1,1,1,1,1,1,1,1,1,1,1,1,1,1,1,
1,1,1,1,1,1,1,1,1,1,1,1,1,1,1,1,1,1,1,1,1,1,1,1,1,1,1,1,1,1,1,1,1,1,1,1,
1,1,1,1,1,1,1,6),(0.,0.0153846153846154,0.0307692307692308,0.0461538461538462,
0.0615384615384615,0.0769230769230769,0.0923076923076923,0.107692307692308,
0.123076923076923,0.138461538461538,0.153846153846154,0.169230769230769,
0.184615384615385,0.2,0.215384615384615,0.230769230769231,0.246153846153846,
0.261538461538462,0.276923076923077,0.292307692307692,0.307692307692308,
0.323076923076923,0.338461538461538,0.353846153846154,0.369230769230769,
0.384615384615385,0.4,0.415384615384615,0.430769230769231,0.446153846153846,
0.461538461538462,0.476923076923077,0.492307692307692,0.507692307692308,
0.523076923076923,0.538461538461538,0.553846153846154,0.569230769230769,
0.584615384615384,0.6,0.615384615384615,0.63076923076923,0.646153846153846,
0.661538461538461,0.676923076923076,0.692307692307692,0.707692307692307,
0.723076923076922,0.738461538461538,0.753846153846153,0.769230769230768,
0.784615384615384,0.799999999999999,0.815384615384614,0.83076923076923,
0.846153846153845,0.86153846153846,0.876923076923076,0.892307692307691,
0.907692307692306,0.923076923076922,0.938461538461537,0.953846153846152,
0.969230769230768,0.984615384615383,1.),.UNSPECIFIED.)
CURVE()
GEOMETRIC_REPRESENTATION_ITEM()
RATIONAL_B_SPLINE_CURVE((1.,1.,1.,1.,1.,1.,1.,1.,1.,1.,1.,1.,1.,1.,1.,1.,
1.,1.,1.,1.,1.,1.,1.,1.,1.,1.,1.,1.,1.,1.,1.,1.,1.,1.,1.,1.,1.,1.,1.,1.,
1.,1.,1.,1.,1.,1.,1.,1.,1.,1.,1.,1.,1.,1.,1.,1.,1.,1.,1.,1.,1.,1.,1.,1.,
1.,1.,1.,1.,1.,1.))
REPRESENTATION_ITEM('')
);
#181=(
BOUNDED_CURVE()
B_SPLINE_CURVE(5,(#26448,#26449,#26450,#26451,#26452,#26453,#26454,#26455,
#26456,#26457,#26458,#26459,#26460,#26461,#26462,#26463,#26464,#26465,#26466,
#26467,#26468,#26469,#26470,#26471,#26472,#26473,#26474,#26475,#26476,#26477,
#26478,#26479,#26480,#26481,#26482,#26483,#26484,#26485,#26486,#26487,#26488,
#26489,#26490,#26491,#26492,#26493,#26494,#26495,#26496,#26497,#26498,#26499,
#26500,#26501,#26502,#26503,#26504,#26505,#26506,#26507,#26508,#26509,#26510,
#26511,#26512,#26513,#26514,#26515,#26516,#26517),.UNSPECIFIED.,.F.,.F.)
B_SPLINE_CURVE_WITH_KNOTS((6,1,1,1,1,1,1,1,1,1,1,1,1,1,1,1,1,1,1,1,1,1,
1,1,1,1,1,1,1,1,1,1,1,1,1,1,1,1,1,1,1,1,1,1,1,1,1,1,1,1,1,1,1,1,1,1,1,1,
1,1,1,1,1,1,1,6),(0.,0.0153846153846154,0.0307692307692308,0.0461538461538462,
0.0615384615384615,0.0769230769230769,0.0923076923076923,0.107692307692308,
0.123076923076923,0.138461538461538,0.153846153846154,0.169230769230769,
0.184615384615385,0.2,0.215384615384615,0.230769230769231,0.246153846153846,
0.261538461538462,0.276923076923077,0.292307692307692,0.307692307692308,
0.323076923076923,0.338461538461538,0.353846153846154,0.369230769230769,
0.384615384615385,0.4,0.415384615384615,0.430769230769231,0.446153846153846,
0.461538461538462,0.476923076923077,0.492307692307692,0.507692307692308,
0.523076923076923,0.538461538461538,0.553846153846154,0.569230769230769,
0.584615384615384,0.6,0.615384615384615,0.63076923076923,0.646153846153846,
0.661538461538461,0.676923076923076,0.692307692307692,0.707692307692307,
0.723076923076922,0.738461538461538,0.753846153846153,0.769230769230768,
0.784615384615384,0.799999999999999,0.815384615384614,0.83076923076923,
0.846153846153845,0.86153846153846,0.876923076923076,0.892307692307691,
0.907692307692306,0.923076923076922,0.938461538461537,0.953846153846152,
0.969230769230768,0.984615384615383,1.),.UNSPECIFIED.)
CURVE()
GEOMETRIC_REPRESENTATION_ITEM()
RATIONAL_B_SPLINE_CURVE((1.,1.,1.,1.,1.,1.,1.,1.,1.,1.,1.,1.,1.,1.,1.,1.,
1.,1.,1.,1.,1.,1.,1.,1.,1.,1.,1.,1.,1.,1.,1.,1.,1.,1.,1.,1.,1.,1.,1.,1.,
1.,1.,1.,1.,1.,1.,1.,1.,1.,1.,1.,1.,1.,1.,1.,1.,1.,1.,1.,1.,1.,1.,1.,1.,
1.,1.,1.,1.,1.,1.))
REPRESENTATION_ITEM('')
);
#182=(
BOUNDED_CURVE()
B_SPLINE_CURVE(5,(#26521,#26522,#26523,#26524,#26525,#26526,#26527,#26528,
#26529,#26530,#26531,#26532,#26533,#26534,#26535,#26536,#26537,#26538,#26539,
#26540,#26541,#26542,#26543,#26544,#26545,#26546,#26547,#26548,#26549,#26550,
#26551,#26552,#26553,#26554,#26555,#26556,#26557,#26558,#26559,#26560,#26561,
#26562,#26563,#26564,#26565,#26566,#26567,#26568,#26569,#26570,#26571,#26572,
#26573,#26574,#26575,#26576,#26577,#26578,#26579,#26580,#26581,#26582,#26583,
#26584,#26585,#26586,#26587,#26588,#26589,#26590),.UNSPECIFIED.,.F.,.F.)
B_SPLINE_CURVE_WITH_KNOTS((6,1,1,1,1,1,1,1,1,1,1,1,1,1,1,1,1,1,1,1,1,1,
1,1,1,1,1,1,1,1,1,1,1,1,1,1,1,1,1,1,1,1,1,1,1,1,1,1,1,1,1,1,1,1,1,1,1,1,
1,1,1,1,1,1,1,6),(0.,0.0153846153846154,0.0307692307692308,0.0461538461538462,
0.0615384615384615,0.0769230769230769,0.0923076923076923,0.107692307692308,
0.123076923076923,0.138461538461538,0.153846153846154,0.169230769230769,
0.184615384615385,0.2,0.215384615384615,0.230769230769231,0.246153846153846,
0.261538461538462,0.276923076923077,0.292307692307692,0.307692307692308,
0.323076923076923,0.338461538461538,0.353846153846154,0.369230769230769,
0.384615384615385,0.4,0.415384615384615,0.430769230769231,0.446153846153846,
0.461538461538462,0.476923076923077,0.492307692307692,0.507692307692308,
0.523076923076923,0.538461538461538,0.553846153846154,0.569230769230769,
0.584615384615384,0.6,0.615384615384615,0.63076923076923,0.646153846153846,
0.661538461538461,0.676923076923076,0.692307692307692,0.707692307692307,
0.723076923076922,0.738461538461538,0.753846153846153,0.769230769230768,
0.784615384615384,0.799999999999999,0.815384615384614,0.83076923076923,
0.846153846153845,0.86153846153846,0.876923076923076,0.892307692307691,
0.907692307692306,0.923076923076922,0.938461538461537,0.953846153846152,
0.969230769230768,0.984615384615383,1.),.UNSPECIFIED.)
CURVE()
GEOMETRIC_REPRESENTATION_ITEM()
RATIONAL_B_SPLINE_CURVE((1.,1.,1.,1.,1.,1.,1.,1.,1.,1.,1.,1.,1.,1.,1.,1.,
1.,1.,1.,1.,1.,1.,1.,1.,1.,1.,1.,1.,1.,1.,1.,1.,1.,1.,1.,1.,1.,1.,1.,1.,
1.,1.,1.,1.,1.,1.,1.,1.,1.,1.,1.,1.,1.,1.,1.,1.,1.,1.,1.,1.,1.,1.,1.,1.,
1.,1.,1.,1.,1.,1.))
REPRESENTATION_ITEM('')
);
#183=(
BOUNDED_CURVE()
B_SPLINE_CURVE(5,(#26594,#26595,#26596,#26597,#26598,#26599,#26600,#26601,
#26602,#26603,#26604,#26605,#26606,#26607,#26608,#26609,#26610,#26611,#26612,
#26613,#26614,#26615,#26616,#26617,#26618,#26619,#26620,#26621,#26622,#26623,
#26624,#26625,#26626,#26627,#26628,#26629,#26630,#26631,#26632,#26633,#26634,
#26635,#26636,#26637,#26638,#26639,#26640,#26641,#26642,#26643,#26644,#26645,
#26646,#26647,#26648,#26649,#26650,#26651,#26652,#26653,#26654,#26655,#26656,
#26657,#26658,#26659,#26660,#26661,#26662,#26663),.UNSPECIFIED.,.F.,.F.)
B_SPLINE_CURVE_WITH_KNOTS((6,1,1,1,1,1,1,1,1,1,1,1,1,1,1,1,1,1,1,1,1,1,
1,1,1,1,1,1,1,1,1,1,1,1,1,1,1,1,1,1,1,1,1,1,1,1,1,1,1,1,1,1,1,1,1,1,1,1,
1,1,1,1,1,1,1,6),(0.,0.0153846153846154,0.0307692307692308,0.0461538461538462,
0.0615384615384615,0.0769230769230769,0.0923076923076923,0.107692307692308,
0.123076923076923,0.138461538461538,0.153846153846154,0.169230769230769,
0.184615384615385,0.2,0.215384615384615,0.230769230769231,0.246153846153846,
0.261538461538462,0.276923076923077,0.292307692307692,0.307692307692308,
0.323076923076923,0.338461538461538,0.353846153846154,0.369230769230769,
0.384615384615385,0.4,0.415384615384615,0.430769230769231,0.446153846153846,
0.461538461538462,0.476923076923077,0.492307692307692,0.507692307692308,
0.523076923076923,0.538461538461538,0.553846153846154,0.569230769230769,
0.584615384615384,0.6,0.615384615384615,0.63076923076923,0.646153846153846,
0.661538461538461,0.676923076923076,0.692307692307692,0.707692307692307,
0.723076923076922,0.738461538461538,0.753846153846153,0.769230769230768,
0.784615384615384,0.799999999999999,0.815384615384614,0.83076923076923,
0.846153846153845,0.86153846153846,0.876923076923076,0.892307692307691,
0.907692307692306,0.923076923076922,0.938461538461537,0.953846153846152,
0.969230769230768,0.984615384615383,1.),.UNSPECIFIED.)
CURVE()
GEOMETRIC_REPRESENTATION_ITEM()
RATIONAL_B_SPLINE_CURVE((1.,1.,1.,1.,1.,1.,1.,1.,1.,1.,1.,1.,1.,1.,1.,1.,
1.,1.,1.,1.,1.,1.,1.,1.,1.,1.,1.,1.,1.,1.,1.,1.,1.,1.,1.,1.,1.,1.,1.,1.,
1.,1.,1.,1.,1.,1.,1.,1.,1.,1.,1.,1.,1.,1.,1.,1.,1.,1.,1.,1.,1.,1.,1.,1.,
1.,1.,1.,1.,1.,1.))
REPRESENTATION_ITEM('')
);
#184=(
BOUNDED_CURVE()
B_SPLINE_CURVE(5,(#26667,#26668,#26669,#26670,#26671,#26672,#26673,#26674,
#26675,#26676,#26677,#26678,#26679,#26680,#26681,#26682,#26683,#26684,#26685,
#26686,#26687,#26688,#26689,#26690,#26691,#26692,#26693,#26694,#26695,#26696,
#26697,#26698,#26699,#26700,#26701,#26702,#26703,#26704,#26705,#26706,#26707,
#26708,#26709,#26710,#26711,#26712,#26713,#26714,#26715,#26716,#26717,#26718,
#26719,#26720,#26721,#26722,#26723,#26724,#26725,#26726,#26727,#26728,#26729,
#26730,#26731,#26732,#26733,#26734,#26735,#26736),.UNSPECIFIED.,.F.,.F.)
B_SPLINE_CURVE_WITH_KNOTS((6,1,1,1,1,1,1,1,1,1,1,1,1,1,1,1,1,1,1,1,1,1,
1,1,1,1,1,1,1,1,1,1,1,1,1,1,1,1,1,1,1,1,1,1,1,1,1,1,1,1,1,1,1,1,1,1,1,1,
1,1,1,1,1,1,1,6),(0.,0.0153846153846154,0.0307692307692308,0.0461538461538462,
0.0615384615384615,0.0769230769230769,0.0923076923076923,0.107692307692308,
0.123076923076923,0.138461538461538,0.153846153846154,0.169230769230769,
0.184615384615385,0.2,0.215384615384615,0.230769230769231,0.246153846153846,
0.261538461538462,0.276923076923077,0.292307692307692,0.307692307692308,
0.323076923076923,0.338461538461538,0.353846153846154,0.369230769230769,
0.384615384615385,0.4,0.415384615384615,0.430769230769231,0.446153846153846,
0.461538461538462,0.476923076923077,0.492307692307692,0.507692307692308,
0.523076923076923,0.538461538461538,0.553846153846154,0.569230769230769,
0.584615384615384,0.6,0.615384615384615,0.63076923076923,0.646153846153846,
0.661538461538461,0.676923076923076,0.692307692307692,0.707692307692307,
0.723076923076922,0.738461538461538,0.753846153846153,0.769230769230768,
0.784615384615384,0.799999999999999,0.815384615384614,0.83076923076923,
0.846153846153845,0.86153846153846,0.876923076923076,0.892307692307691,
0.907692307692306,0.923076923076922,0.938461538461537,0.953846153846152,
0.969230769230768,0.984615384615383,1.),.UNSPECIFIED.)
CURVE()
GEOMETRIC_REPRESENTATION_ITEM()
RATIONAL_B_SPLINE_CURVE((1.,1.,1.,1.,1.,1.,1.,1.,1.,1.,1.,1.,1.,1.,1.,1.,
1.,1.,1.,1.,1.,1.,1.,1.,1.,1.,1.,1.,1.,1.,1.,1.,1.,1.,1.,1.,1.,1.,1.,1.,
1.,1.,1.,1.,1.,1.,1.,1.,1.,1.,1.,1.,1.,1.,1.,1.,1.,1.,1.,1.,1.,1.,1.,1.,
1.,1.,1.,1.,1.,1.))
REPRESENTATION_ITEM('')
);
#185=(
BOUNDED_CURVE()
B_SPLINE_CURVE(5,(#26740,#26741,#26742,#26743,#26744,#26745,#26746,#26747,
#26748,#26749,#26750,#26751,#26752,#26753,#26754,#26755,#26756,#26757,#26758,
#26759,#26760,#26761,#26762,#26763,#26764,#26765,#26766,#26767,#26768,#26769,
#26770,#26771,#26772,#26773,#26774,#26775,#26776,#26777,#26778,#26779,#26780,
#26781,#26782,#26783,#26784,#26785,#26786,#26787,#26788,#26789,#26790,#26791,
#26792,#26793,#26794,#26795,#26796,#26797,#26798,#26799,#26800,#26801,#26802,
#26803,#26804,#26805,#26806,#26807,#26808,#26809),.UNSPECIFIED.,.F.,.F.)
B_SPLINE_CURVE_WITH_KNOTS((6,1,1,1,1,1,1,1,1,1,1,1,1,1,1,1,1,1,1,1,1,1,
1,1,1,1,1,1,1,1,1,1,1,1,1,1,1,1,1,1,1,1,1,1,1,1,1,1,1,1,1,1,1,1,1,1,1,1,
1,1,1,1,1,1,1,6),(0.,0.0153846153846154,0.0307692307692308,0.0461538461538462,
0.0615384615384615,0.0769230769230769,0.0923076923076923,0.107692307692308,
0.123076923076923,0.138461538461538,0.153846153846154,0.169230769230769,
0.184615384615385,0.2,0.215384615384615,0.230769230769231,0.246153846153846,
0.261538461538462,0.276923076923077,0.292307692307692,0.307692307692308,
0.323076923076923,0.338461538461538,0.353846153846154,0.369230769230769,
0.384615384615385,0.4,0.415384615384615,0.430769230769231,0.446153846153846,
0.461538461538462,0.476923076923077,0.492307692307692,0.507692307692308,
0.523076923076923,0.538461538461538,0.553846153846154,0.569230769230769,
0.584615384615384,0.6,0.615384615384615,0.63076923076923,0.646153846153846,
0.661538461538461,0.676923076923076,0.692307692307692,0.707692307692307,
0.723076923076922,0.738461538461538,0.753846153846153,0.769230769230768,
0.784615384615384,0.799999999999999,0.815384615384614,0.83076923076923,
0.846153846153845,0.86153846153846,0.876923076923076,0.892307692307691,
0.907692307692306,0.923076923076922,0.938461538461537,0.953846153846152,
0.969230769230768,0.984615384615383,1.),.UNSPECIFIED.)
CURVE()
GEOMETRIC_REPRESENTATION_ITEM()
RATIONAL_B_SPLINE_CURVE((1.,1.,1.,1.,1.,1.,1.,1.,1.,1.,1.,1.,1.,1.,1.,1.,
1.,1.,1.,1.,1.,1.,1.,1.,1.,1.,1.,1.,1.,1.,1.,1.,1.,1.,1.,1.,1.,1.,1.,1.,
1.,1.,1.,1.,1.,1.,1.,1.,1.,1.,1.,1.,1.,1.,1.,1.,1.,1.,1.,1.,1.,1.,1.,1.,
1.,1.,1.,1.,1.,1.))
REPRESENTATION_ITEM('')
);
#186=(
BOUNDED_CURVE()
B_SPLINE_CURVE(5,(#26813,#26814,#26815,#26816,#26817,#26818,#26819,#26820,
#26821,#26822,#26823,#26824,#26825,#26826,#26827,#26828,#26829,#26830,#26831,
#26832,#26833,#26834,#26835,#26836,#26837,#26838,#26839,#26840,#26841,#26842,
#26843,#26844,#26845,#26846,#26847,#26848,#26849,#26850,#26851,#26852,#26853,
#26854,#26855,#26856,#26857,#26858,#26859,#26860,#26861,#26862,#26863,#26864,
#26865,#26866,#26867,#26868,#26869,#26870,#26871,#26872,#26873,#26874,#26875,
#26876,#26877,#26878,#26879,#26880,#26881,#26882),.UNSPECIFIED.,.F.,.F.)
B_SPLINE_CURVE_WITH_KNOTS((6,1,1,1,1,1,1,1,1,1,1,1,1,1,1,1,1,1,1,1,1,1,
1,1,1,1,1,1,1,1,1,1,1,1,1,1,1,1,1,1,1,1,1,1,1,1,1,1,1,1,1,1,1,1,1,1,1,1,
1,1,1,1,1,1,1,6),(0.,0.0153846153846154,0.0307692307692308,0.0461538461538462,
0.0615384615384615,0.0769230769230769,0.0923076923076923,0.107692307692308,
0.123076923076923,0.138461538461538,0.153846153846154,0.169230769230769,
0.184615384615385,0.2,0.215384615384615,0.230769230769231,0.246153846153846,
0.261538461538462,0.276923076923077,0.292307692307692,0.307692307692308,
0.323076923076923,0.338461538461538,0.353846153846154,0.369230769230769,
0.384615384615385,0.4,0.415384615384615,0.430769230769231,0.446153846153846,
0.461538461538462,0.476923076923077,0.492307692307692,0.507692307692308,
0.523076923076923,0.538461538461538,0.553846153846154,0.569230769230769,
0.584615384615384,0.6,0.615384615384615,0.63076923076923,0.646153846153846,
0.661538461538461,0.676923076923076,0.692307692307692,0.707692307692307,
0.723076923076922,0.738461538461538,0.753846153846153,0.769230769230768,
0.784615384615384,0.799999999999999,0.815384615384614,0.83076923076923,
0.846153846153845,0.86153846153846,0.876923076923076,0.892307692307691,
0.907692307692306,0.923076923076922,0.938461538461537,0.953846153846152,
0.969230769230768,0.984615384615383,1.),.UNSPECIFIED.)
CURVE()
GEOMETRIC_REPRESENTATION_ITEM()
RATIONAL_B_SPLINE_CURVE((1.,1.,1.,1.,1.,1.,1.,1.,1.,1.,1.,1.,1.,1.,1.,1.,
1.,1.,1.,1.,1.,1.,1.,1.,1.,1.,1.,1.,1.,1.,1.,1.,1.,1.,1.,1.,1.,1.,1.,1.,
1.,1.,1.,1.,1.,1.,1.,1.,1.,1.,1.,1.,1.,1.,1.,1.,1.,1.,1.,1.,1.,1.,1.,1.,
1.,1.,1.,1.,1.,1.))
REPRESENTATION_ITEM('')
);
#187=(
BOUNDED_CURVE()
B_SPLINE_CURVE(5,(#26886,#26887,#26888,#26889,#26890,#26891,#26892,#26893,
#26894,#26895,#26896,#26897,#26898,#26899,#26900,#26901,#26902,#26903,#26904,
#26905,#26906,#26907,#26908,#26909,#26910,#26911,#26912,#26913,#26914,#26915,
#26916,#26917,#26918,#26919,#26920,#26921,#26922,#26923,#26924,#26925,#26926,
#26927,#26928,#26929,#26930,#26931,#26932,#26933,#26934,#26935,#26936,#26937,
#26938,#26939,#26940,#26941,#26942,#26943,#26944,#26945,#26946,#26947,#26948,
#26949,#26950,#26951,#26952,#26953,#26954,#26955),.UNSPECIFIED.,.F.,.F.)
B_SPLINE_CURVE_WITH_KNOTS((6,1,1,1,1,1,1,1,1,1,1,1,1,1,1,1,1,1,1,1,1,1,
1,1,1,1,1,1,1,1,1,1,1,1,1,1,1,1,1,1,1,1,1,1,1,1,1,1,1,1,1,1,1,1,1,1,1,1,
1,1,1,1,1,1,1,6),(0.,0.0153846153846154,0.0307692307692308,0.0461538461538462,
0.0615384615384615,0.0769230769230769,0.0923076923076923,0.107692307692308,
0.123076923076923,0.138461538461538,0.153846153846154,0.169230769230769,
0.184615384615385,0.2,0.215384615384615,0.230769230769231,0.246153846153846,
0.261538461538462,0.276923076923077,0.292307692307692,0.307692307692308,
0.323076923076923,0.338461538461538,0.353846153846154,0.369230769230769,
0.384615384615385,0.4,0.415384615384615,0.430769230769231,0.446153846153846,
0.461538461538462,0.476923076923077,0.492307692307692,0.507692307692308,
0.523076923076923,0.538461538461538,0.553846153846154,0.569230769230769,
0.584615384615384,0.6,0.615384615384615,0.63076923076923,0.646153846153846,
0.661538461538461,0.676923076923076,0.692307692307692,0.707692307692307,
0.723076923076922,0.738461538461538,0.753846153846153,0.769230769230768,
0.784615384615384,0.799999999999999,0.815384615384614,0.83076923076923,
0.846153846153845,0.86153846153846,0.876923076923076,0.892307692307691,
0.907692307692306,0.923076923076922,0.938461538461537,0.953846153846152,
0.969230769230768,0.984615384615383,1.),.UNSPECIFIED.)
CURVE()
GEOMETRIC_REPRESENTATION_ITEM()
RATIONAL_B_SPLINE_CURVE((1.,1.,1.,1.,1.,1.,1.,1.,1.,1.,1.,1.,1.,1.,1.,1.,
1.,1.,1.,1.,1.,1.,1.,1.,1.,1.,1.,1.,1.,1.,1.,1.,1.,1.,1.,1.,1.,1.,1.,1.,
1.,1.,1.,1.,1.,1.,1.,1.,1.,1.,1.,1.,1.,1.,1.,1.,1.,1.,1.,1.,1.,1.,1.,1.,
1.,1.,1.,1.,1.,1.))
REPRESENTATION_ITEM('')
);
#188=(
BOUNDED_CURVE()
B_SPLINE_CURVE(5,(#26959,#26960,#26961,#26962,#26963,#26964,#26965,#26966,
#26967,#26968,#26969,#26970,#26971,#26972,#26973,#26974,#26975,#26976,#26977,
#26978,#26979,#26980,#26981,#26982,#26983,#26984,#26985,#26986,#26987,#26988,
#26989,#26990,#26991,#26992,#26993,#26994,#26995,#26996,#26997,#26998,#26999,
#27000,#27001,#27002,#27003,#27004,#27005,#27006,#27007,#27008,#27009,#27010,
#27011,#27012,#27013,#27014,#27015,#27016,#27017,#27018,#27019,#27020,#27021,
#27022,#27023,#27024,#27025,#27026,#27027,#27028),.UNSPECIFIED.,.F.,.F.)
B_SPLINE_CURVE_WITH_KNOTS((6,1,1,1,1,1,1,1,1,1,1,1,1,1,1,1,1,1,1,1,1,1,
1,1,1,1,1,1,1,1,1,1,1,1,1,1,1,1,1,1,1,1,1,1,1,1,1,1,1,1,1,1,1,1,1,1,1,1,
1,1,1,1,1,1,1,6),(0.,0.0153846153846154,0.0307692307692308,0.0461538461538462,
0.0615384615384615,0.0769230769230769,0.0923076923076923,0.107692307692308,
0.123076923076923,0.138461538461538,0.153846153846154,0.169230769230769,
0.184615384615385,0.2,0.215384615384615,0.230769230769231,0.246153846153846,
0.261538461538462,0.276923076923077,0.292307692307692,0.307692307692308,
0.323076923076923,0.338461538461538,0.353846153846154,0.369230769230769,
0.384615384615385,0.4,0.415384615384615,0.430769230769231,0.446153846153846,
0.461538461538462,0.476923076923077,0.492307692307692,0.507692307692308,
0.523076923076923,0.538461538461538,0.553846153846154,0.569230769230769,
0.584615384615384,0.6,0.615384615384615,0.63076923076923,0.646153846153846,
0.661538461538461,0.676923076923076,0.692307692307692,0.707692307692307,
0.723076923076922,0.738461538461538,0.753846153846153,0.769230769230768,
0.784615384615384,0.799999999999999,0.815384615384614,0.83076923076923,
0.846153846153845,0.86153846153846,0.876923076923076,0.892307692307691,
0.907692307692306,0.923076923076922,0.938461538461537,0.953846153846152,
0.969230769230768,0.984615384615383,1.),.UNSPECIFIED.)
CURVE()
GEOMETRIC_REPRESENTATION_ITEM()
RATIONAL_B_SPLINE_CURVE((1.,1.,1.,1.,1.,1.,1.,1.,1.,1.,1.,1.,1.,1.,1.,1.,
1.,1.,1.,1.,1.,1.,1.,1.,1.,1.,1.,1.,1.,1.,1.,1.,1.,1.,1.,1.,1.,1.,1.,1.,
1.,1.,1.,1.,1.,1.,1.,1.,1.,1.,1.,1.,1.,1.,1.,1.,1.,1.,1.,1.,1.,1.,1.,1.,
1.,1.,1.,1.,1.,1.))
REPRESENTATION_ITEM('')
);
#189=(
BOUNDED_CURVE()
B_SPLINE_CURVE(5,(#27032,#27033,#27034,#27035,#27036,#27037,#27038,#27039,
#27040,#27041,#27042,#27043,#27044,#27045,#27046,#27047,#27048,#27049,#27050,
#27051,#27052,#27053,#27054,#27055,#27056,#27057,#27058,#27059,#27060,#27061,
#27062,#27063,#27064,#27065,#27066,#27067,#27068,#27069,#27070,#27071,#27072,
#27073,#27074,#27075,#27076,#27077,#27078,#27079,#27080,#27081,#27082,#27083,
#27084,#27085,#27086,#27087,#27088,#27089,#27090,#27091,#27092,#27093,#27094,
#27095,#27096,#27097,#27098,#27099,#27100,#27101),.UNSPECIFIED.,.F.,.F.)
B_SPLINE_CURVE_WITH_KNOTS((6,1,1,1,1,1,1,1,1,1,1,1,1,1,1,1,1,1,1,1,1,1,
1,1,1,1,1,1,1,1,1,1,1,1,1,1,1,1,1,1,1,1,1,1,1,1,1,1,1,1,1,1,1,1,1,1,1,1,
1,1,1,1,1,1,1,6),(0.,0.0153846153846154,0.0307692307692308,0.0461538461538462,
0.0615384615384615,0.0769230769230769,0.0923076923076923,0.107692307692308,
0.123076923076923,0.138461538461538,0.153846153846154,0.169230769230769,
0.184615384615385,0.2,0.215384615384615,0.230769230769231,0.246153846153846,
0.261538461538462,0.276923076923077,0.292307692307692,0.307692307692308,
0.323076923076923,0.338461538461538,0.353846153846154,0.369230769230769,
0.384615384615385,0.4,0.415384615384615,0.430769230769231,0.446153846153846,
0.461538461538462,0.476923076923077,0.492307692307692,0.507692307692308,
0.523076923076923,0.538461538461538,0.553846153846154,0.569230769230769,
0.584615384615384,0.6,0.615384615384615,0.63076923076923,0.646153846153846,
0.661538461538461,0.676923076923076,0.692307692307692,0.707692307692307,
0.723076923076922,0.738461538461538,0.753846153846153,0.769230769230768,
0.784615384615384,0.799999999999999,0.815384615384614,0.83076923076923,
0.846153846153845,0.86153846153846,0.876923076923076,0.892307692307691,
0.907692307692306,0.923076923076922,0.938461538461537,0.953846153846152,
0.969230769230768,0.984615384615383,1.),.UNSPECIFIED.)
CURVE()
GEOMETRIC_REPRESENTATION_ITEM()
RATIONAL_B_SPLINE_CURVE((1.,1.,1.,1.,1.,1.,1.,1.,1.,1.,1.,1.,1.,1.,1.,1.,
1.,1.,1.,1.,1.,1.,1.,1.,1.,1.,1.,1.,1.,1.,1.,1.,1.,1.,1.,1.,1.,1.,1.,1.,
1.,1.,1.,1.,1.,1.,1.,1.,1.,1.,1.,1.,1.,1.,1.,1.,1.,1.,1.,1.,1.,1.,1.,1.,
1.,1.,1.,1.,1.,1.))
REPRESENTATION_ITEM('')
);
#190=(
BOUNDED_CURVE()
B_SPLINE_CURVE(5,(#27105,#27106,#27107,#27108,#27109,#27110,#27111,#27112,
#27113,#27114,#27115,#27116,#27117,#27118,#27119,#27120,#27121,#27122,#27123,
#27124,#27125,#27126,#27127,#27128,#27129,#27130,#27131,#27132,#27133,#27134,
#27135,#27136,#27137,#27138,#27139,#27140,#27141,#27142,#27143,#27144,#27145,
#27146,#27147,#27148,#27149,#27150,#27151,#27152,#27153,#27154,#27155,#27156,
#27157,#27158,#27159,#27160,#27161,#27162,#27163,#27164,#27165,#27166,#27167,
#27168,#27169,#27170,#27171,#27172,#27173,#27174),.UNSPECIFIED.,.F.,.F.)
B_SPLINE_CURVE_WITH_KNOTS((6,1,1,1,1,1,1,1,1,1,1,1,1,1,1,1,1,1,1,1,1,1,
1,1,1,1,1,1,1,1,1,1,1,1,1,1,1,1,1,1,1,1,1,1,1,1,1,1,1,1,1,1,1,1,1,1,1,1,
1,1,1,1,1,1,1,6),(0.,0.0153846153846154,0.0307692307692308,0.0461538461538462,
0.0615384615384615,0.0769230769230769,0.0923076923076923,0.107692307692308,
0.123076923076923,0.138461538461538,0.153846153846154,0.169230769230769,
0.184615384615385,0.2,0.215384615384615,0.230769230769231,0.246153846153846,
0.261538461538462,0.276923076923077,0.292307692307692,0.307692307692308,
0.323076923076923,0.338461538461538,0.353846153846154,0.369230769230769,
0.384615384615385,0.4,0.415384615384615,0.430769230769231,0.446153846153846,
0.461538461538462,0.476923076923077,0.492307692307692,0.507692307692308,
0.523076923076923,0.538461538461538,0.553846153846154,0.569230769230769,
0.584615384615384,0.6,0.615384615384615,0.63076923076923,0.646153846153846,
0.661538461538461,0.676923076923076,0.692307692307692,0.707692307692307,
0.723076923076922,0.738461538461538,0.753846153846153,0.769230769230768,
0.784615384615384,0.799999999999999,0.815384615384614,0.83076923076923,
0.846153846153845,0.86153846153846,0.876923076923076,0.892307692307691,
0.907692307692306,0.923076923076922,0.938461538461537,0.953846153846152,
0.969230769230768,0.984615384615383,1.),.UNSPECIFIED.)
CURVE()
GEOMETRIC_REPRESENTATION_ITEM()
RATIONAL_B_SPLINE_CURVE((1.,1.,1.,1.,1.,1.,1.,1.,1.,1.,1.,1.,1.,1.,1.,1.,
1.,1.,1.,1.,1.,1.,1.,1.,1.,1.,1.,1.,1.,1.,1.,1.,1.,1.,1.,1.,1.,1.,1.,1.,
1.,1.,1.,1.,1.,1.,1.,1.,1.,1.,1.,1.,1.,1.,1.,1.,1.,1.,1.,1.,1.,1.,1.,1.,
1.,1.,1.,1.,1.,1.))
REPRESENTATION_ITEM('')
);
#191=(
BOUNDED_CURVE()
B_SPLINE_CURVE(5,(#27178,#27179,#27180,#27181,#27182,#27183,#27184,#27185,
#27186,#27187,#27188,#27189,#27190,#27191,#27192,#27193,#27194,#27195,#27196,
#27197,#27198,#27199,#27200,#27201,#27202,#27203,#27204,#27205,#27206,#27207,
#27208,#27209,#27210,#27211,#27212,#27213,#27214,#27215,#27216,#27217,#27218,
#27219,#27220,#27221,#27222,#27223,#27224,#27225,#27226,#27227,#27228,#27229,
#27230,#27231,#27232,#27233,#27234,#27235,#27236,#27237,#27238,#27239,#27240,
#27241,#27242,#27243,#27244,#27245,#27246,#27247),.UNSPECIFIED.,.F.,.F.)
B_SPLINE_CURVE_WITH_KNOTS((6,1,1,1,1,1,1,1,1,1,1,1,1,1,1,1,1,1,1,1,1,1,
1,1,1,1,1,1,1,1,1,1,1,1,1,1,1,1,1,1,1,1,1,1,1,1,1,1,1,1,1,1,1,1,1,1,1,1,
1,1,1,1,1,1,1,6),(0.,0.0153846153846154,0.0307692307692308,0.0461538461538462,
0.0615384615384615,0.0769230769230769,0.0923076923076923,0.107692307692308,
0.123076923076923,0.138461538461538,0.153846153846154,0.169230769230769,
0.184615384615385,0.2,0.215384615384615,0.230769230769231,0.246153846153846,
0.261538461538462,0.276923076923077,0.292307692307692,0.307692307692308,
0.323076923076923,0.338461538461538,0.353846153846154,0.369230769230769,
0.384615384615385,0.4,0.415384615384615,0.430769230769231,0.446153846153846,
0.461538461538462,0.476923076923077,0.492307692307692,0.507692307692308,
0.523076923076923,0.538461538461538,0.553846153846154,0.569230769230769,
0.584615384615384,0.6,0.615384615384615,0.63076923076923,0.646153846153846,
0.661538461538461,0.676923076923076,0.692307692307692,0.707692307692307,
0.723076923076922,0.738461538461538,0.753846153846153,0.769230769230768,
0.784615384615384,0.799999999999999,0.815384615384614,0.83076923076923,
0.846153846153845,0.86153846153846,0.876923076923076,0.892307692307691,
0.907692307692306,0.923076923076922,0.938461538461537,0.953846153846152,
0.969230769230768,0.984615384615383,1.),.UNSPECIFIED.)
CURVE()
GEOMETRIC_REPRESENTATION_ITEM()
RATIONAL_B_SPLINE_CURVE((1.,1.,1.,1.,1.,1.,1.,1.,1.,1.,1.,1.,1.,1.,1.,1.,
1.,1.,1.,1.,1.,1.,1.,1.,1.,1.,1.,1.,1.,1.,1.,1.,1.,1.,1.,1.,1.,1.,1.,1.,
1.,1.,1.,1.,1.,1.,1.,1.,1.,1.,1.,1.,1.,1.,1.,1.,1.,1.,1.,1.,1.,1.,1.,1.,
1.,1.,1.,1.,1.,1.))
REPRESENTATION_ITEM('')
);
#192=(
BOUNDED_CURVE()
B_SPLINE_CURVE(5,(#27251,#27252,#27253,#27254,#27255,#27256,#27257,#27258,
#27259,#27260,#27261,#27262,#27263,#27264,#27265,#27266,#27267,#27268,#27269,
#27270,#27271,#27272,#27273,#27274,#27275,#27276,#27277,#27278,#27279,#27280,
#27281,#27282,#27283,#27284,#27285,#27286,#27287,#27288,#27289,#27290,#27291,
#27292,#27293,#27294,#27295,#27296,#27297,#27298,#27299,#27300,#27301,#27302,
#27303,#27304,#27305,#27306,#27307,#27308,#27309,#27310,#27311,#27312,#27313,
#27314,#27315,#27316,#27317,#27318,#27319,#27320),.UNSPECIFIED.,.F.,.F.)
B_SPLINE_CURVE_WITH_KNOTS((6,1,1,1,1,1,1,1,1,1,1,1,1,1,1,1,1,1,1,1,1,1,
1,1,1,1,1,1,1,1,1,1,1,1,1,1,1,1,1,1,1,1,1,1,1,1,1,1,1,1,1,1,1,1,1,1,1,1,
1,1,1,1,1,1,1,6),(0.,0.0153846153846154,0.0307692307692308,0.0461538461538462,
0.0615384615384615,0.0769230769230769,0.0923076923076923,0.107692307692308,
0.123076923076923,0.138461538461538,0.153846153846154,0.169230769230769,
0.184615384615385,0.2,0.215384615384615,0.230769230769231,0.246153846153846,
0.261538461538462,0.276923076923077,0.292307692307692,0.307692307692308,
0.323076923076923,0.338461538461538,0.353846153846154,0.369230769230769,
0.384615384615385,0.4,0.415384615384615,0.430769230769231,0.446153846153846,
0.461538461538462,0.476923076923077,0.492307692307692,0.507692307692308,
0.523076923076923,0.538461538461538,0.553846153846154,0.569230769230769,
0.584615384615384,0.6,0.615384615384615,0.63076923076923,0.646153846153846,
0.661538461538461,0.676923076923076,0.692307692307692,0.707692307692307,
0.723076923076922,0.738461538461538,0.753846153846153,0.769230769230768,
0.784615384615384,0.799999999999999,0.815384615384614,0.83076923076923,
0.846153846153845,0.86153846153846,0.876923076923076,0.892307692307691,
0.907692307692306,0.923076923076922,0.938461538461537,0.953846153846152,
0.969230769230768,0.984615384615383,1.),.UNSPECIFIED.)
CURVE()
GEOMETRIC_REPRESENTATION_ITEM()
RATIONAL_B_SPLINE_CURVE((1.,1.,1.,1.,1.,1.,1.,1.,1.,1.,1.,1.,1.,1.,1.,1.,
1.,1.,1.,1.,1.,1.,1.,1.,1.,1.,1.,1.,1.,1.,1.,1.,1.,1.,1.,1.,1.,1.,1.,1.,
1.,1.,1.,1.,1.,1.,1.,1.,1.,1.,1.,1.,1.,1.,1.,1.,1.,1.,1.,1.,1.,1.,1.,1.,
1.,1.,1.,1.,1.,1.))
REPRESENTATION_ITEM('')
);
#193=(
BOUNDED_CURVE()
B_SPLINE_CURVE(5,(#27324,#27325,#27326,#27327,#27328,#27329,#27330,#27331,
#27332,#27333,#27334,#27335,#27336,#27337,#27338,#27339,#27340,#27341,#27342,
#27343,#27344,#27345,#27346,#27347,#27348,#27349,#27350,#27351,#27352,#27353,
#27354,#27355,#27356,#27357,#27358,#27359,#27360,#27361,#27362,#27363,#27364,
#27365,#27366,#27367,#27368,#27369,#27370,#27371,#27372,#27373,#27374,#27375,
#27376,#27377,#27378,#27379,#27380,#27381,#27382,#27383,#27384,#27385,#27386,
#27387,#27388,#27389,#27390,#27391,#27392,#27393),.UNSPECIFIED.,.F.,.F.)
B_SPLINE_CURVE_WITH_KNOTS((6,1,1,1,1,1,1,1,1,1,1,1,1,1,1,1,1,1,1,1,1,1,
1,1,1,1,1,1,1,1,1,1,1,1,1,1,1,1,1,1,1,1,1,1,1,1,1,1,1,1,1,1,1,1,1,1,1,1,
1,1,1,1,1,1,1,6),(0.,0.0153846153846154,0.0307692307692308,0.0461538461538462,
0.0615384615384615,0.0769230769230769,0.0923076923076923,0.107692307692308,
0.123076923076923,0.138461538461538,0.153846153846154,0.169230769230769,
0.184615384615385,0.2,0.215384615384615,0.230769230769231,0.246153846153846,
0.261538461538462,0.276923076923077,0.292307692307692,0.307692307692308,
0.323076923076923,0.338461538461538,0.353846153846154,0.369230769230769,
0.384615384615385,0.4,0.415384615384615,0.430769230769231,0.446153846153846,
0.461538461538462,0.476923076923077,0.492307692307692,0.507692307692308,
0.523076923076923,0.538461538461538,0.553846153846154,0.569230769230769,
0.584615384615384,0.6,0.615384615384615,0.63076923076923,0.646153846153846,
0.661538461538461,0.676923076923076,0.692307692307692,0.707692307692307,
0.723076923076922,0.738461538461538,0.753846153846153,0.769230769230768,
0.784615384615384,0.799999999999999,0.815384615384614,0.83076923076923,
0.846153846153845,0.86153846153846,0.876923076923076,0.892307692307691,
0.907692307692306,0.923076923076922,0.938461538461537,0.953846153846152,
0.969230769230768,0.984615384615383,1.),.UNSPECIFIED.)
CURVE()
GEOMETRIC_REPRESENTATION_ITEM()
RATIONAL_B_SPLINE_CURVE((1.,1.,1.,1.,1.,1.,1.,1.,1.,1.,1.,1.,1.,1.,1.,1.,
1.,1.,1.,1.,1.,1.,1.,1.,1.,1.,1.,1.,1.,1.,1.,1.,1.,1.,1.,1.,1.,1.,1.,1.,
1.,1.,1.,1.,1.,1.,1.,1.,1.,1.,1.,1.,1.,1.,1.,1.,1.,1.,1.,1.,1.,1.,1.,1.,
1.,1.,1.,1.,1.,1.))
REPRESENTATION_ITEM('')
);
#194=(
BOUNDED_CURVE()
B_SPLINE_CURVE(5,(#27397,#27398,#27399,#27400,#27401,#27402,#27403,#27404,
#27405,#27406,#27407,#27408,#27409,#27410,#27411,#27412,#27413,#27414,#27415,
#27416,#27417,#27418,#27419,#27420,#27421,#27422,#27423,#27424,#27425,#27426,
#27427,#27428,#27429,#27430,#27431,#27432,#27433,#27434,#27435,#27436,#27437,
#27438,#27439,#27440,#27441,#27442,#27443,#27444,#27445,#27446,#27447,#27448,
#27449,#27450,#27451,#27452,#27453,#27454,#27455,#27456,#27457,#27458,#27459,
#27460,#27461,#27462,#27463,#27464,#27465,#27466),.UNSPECIFIED.,.F.,.F.)
B_SPLINE_CURVE_WITH_KNOTS((6,1,1,1,1,1,1,1,1,1,1,1,1,1,1,1,1,1,1,1,1,1,
1,1,1,1,1,1,1,1,1,1,1,1,1,1,1,1,1,1,1,1,1,1,1,1,1,1,1,1,1,1,1,1,1,1,1,1,
1,1,1,1,1,1,1,6),(0.,0.0153846153846154,0.0307692307692308,0.0461538461538462,
0.0615384615384615,0.0769230769230769,0.0923076923076923,0.107692307692308,
0.123076923076923,0.138461538461538,0.153846153846154,0.169230769230769,
0.184615384615385,0.2,0.215384615384615,0.230769230769231,0.246153846153846,
0.261538461538462,0.276923076923077,0.292307692307692,0.307692307692308,
0.323076923076923,0.338461538461538,0.353846153846154,0.369230769230769,
0.384615384615385,0.4,0.415384615384615,0.430769230769231,0.446153846153846,
0.461538461538462,0.476923076923077,0.492307692307692,0.507692307692308,
0.523076923076923,0.538461538461538,0.553846153846154,0.569230769230769,
0.584615384615384,0.6,0.615384615384615,0.63076923076923,0.646153846153846,
0.661538461538461,0.676923076923076,0.692307692307692,0.707692307692307,
0.723076923076922,0.738461538461538,0.753846153846153,0.769230769230768,
0.784615384615384,0.799999999999999,0.815384615384614,0.83076923076923,
0.846153846153845,0.86153846153846,0.876923076923076,0.892307692307691,
0.907692307692306,0.923076923076922,0.938461538461537,0.953846153846152,
0.969230769230768,0.984615384615383,1.),.UNSPECIFIED.)
CURVE()
GEOMETRIC_REPRESENTATION_ITEM()
RATIONAL_B_SPLINE_CURVE((1.,1.,1.,1.,1.,1.,1.,1.,1.,1.,1.,1.,1.,1.,1.,1.,
1.,1.,1.,1.,1.,1.,1.,1.,1.,1.,1.,1.,1.,1.,1.,1.,1.,1.,1.,1.,1.,1.,1.,1.,
1.,1.,1.,1.,1.,1.,1.,1.,1.,1.,1.,1.,1.,1.,1.,1.,1.,1.,1.,1.,1.,1.,1.,1.,
1.,1.,1.,1.,1.,1.))
REPRESENTATION_ITEM('')
);
#195=(
BOUNDED_CURVE()
B_SPLINE_CURVE(5,(#27470,#27471,#27472,#27473,#27474,#27475,#27476,#27477,
#27478,#27479,#27480,#27481,#27482,#27483,#27484,#27485,#27486,#27487,#27488,
#27489,#27490,#27491,#27492,#27493,#27494,#27495,#27496,#27497,#27498,#27499,
#27500,#27501,#27502,#27503,#27504,#27505,#27506,#27507,#27508,#27509,#27510,
#27511,#27512,#27513,#27514,#27515,#27516,#27517,#27518,#27519,#27520,#27521,
#27522,#27523,#27524,#27525,#27526,#27527,#27528,#27529,#27530,#27531,#27532,
#27533,#27534,#27535,#27536,#27537,#27538,#27539),.UNSPECIFIED.,.F.,.F.)
B_SPLINE_CURVE_WITH_KNOTS((6,1,1,1,1,1,1,1,1,1,1,1,1,1,1,1,1,1,1,1,1,1,
1,1,1,1,1,1,1,1,1,1,1,1,1,1,1,1,1,1,1,1,1,1,1,1,1,1,1,1,1,1,1,1,1,1,1,1,
1,1,1,1,1,1,1,6),(0.,0.0153846153846154,0.0307692307692308,0.0461538461538462,
0.0615384615384615,0.0769230769230769,0.0923076923076923,0.107692307692308,
0.123076923076923,0.138461538461538,0.153846153846154,0.169230769230769,
0.184615384615385,0.2,0.215384615384615,0.230769230769231,0.246153846153846,
0.261538461538462,0.276923076923077,0.292307692307692,0.307692307692308,
0.323076923076923,0.338461538461538,0.353846153846154,0.369230769230769,
0.384615384615385,0.4,0.415384615384615,0.430769230769231,0.446153846153846,
0.461538461538462,0.476923076923077,0.492307692307692,0.507692307692308,
0.523076923076923,0.538461538461538,0.553846153846154,0.569230769230769,
0.584615384615384,0.6,0.615384615384615,0.63076923076923,0.646153846153846,
0.661538461538461,0.676923076923076,0.692307692307692,0.707692307692307,
0.723076923076922,0.738461538461538,0.753846153846153,0.769230769230768,
0.784615384615384,0.799999999999999,0.815384615384614,0.83076923076923,
0.846153846153845,0.86153846153846,0.876923076923076,0.892307692307691,
0.907692307692306,0.923076923076922,0.938461538461537,0.953846153846152,
0.969230769230768,0.984615384615383,1.),.UNSPECIFIED.)
CURVE()
GEOMETRIC_REPRESENTATION_ITEM()
RATIONAL_B_SPLINE_CURVE((1.,1.,1.,1.,1.,1.,1.,1.,1.,1.,1.,1.,1.,1.,1.,1.,
1.,1.,1.,1.,1.,1.,1.,1.,1.,1.,1.,1.,1.,1.,1.,1.,1.,1.,1.,1.,1.,1.,1.,1.,
1.,1.,1.,1.,1.,1.,1.,1.,1.,1.,1.,1.,1.,1.,1.,1.,1.,1.,1.,1.,1.,1.,1.,1.,
1.,1.,1.,1.,1.,1.))
REPRESENTATION_ITEM('')
);
#196=(
BOUNDED_CURVE()
B_SPLINE_CURVE(5,(#27543,#27544,#27545,#27546,#27547,#27548,#27549,#27550,
#27551,#27552,#27553,#27554,#27555,#27556,#27557,#27558,#27559,#27560,#27561,
#27562,#27563,#27564,#27565,#27566,#27567,#27568,#27569,#27570,#27571,#27572,
#27573,#27574,#27575,#27576,#27577,#27578,#27579,#27580,#27581,#27582,#27583,
#27584,#27585,#27586,#27587,#27588,#27589,#27590,#27591,#27592,#27593,#27594,
#27595,#27596,#27597,#27598,#27599,#27600,#27601,#27602,#27603,#27604,#27605,
#27606,#27607,#27608,#27609,#27610,#27611,#27612),.UNSPECIFIED.,.F.,.F.)
B_SPLINE_CURVE_WITH_KNOTS((6,1,1,1,1,1,1,1,1,1,1,1,1,1,1,1,1,1,1,1,1,1,
1,1,1,1,1,1,1,1,1,1,1,1,1,1,1,1,1,1,1,1,1,1,1,1,1,1,1,1,1,1,1,1,1,1,1,1,
1,1,1,1,1,1,1,6),(0.,0.0153846153846154,0.0307692307692308,0.0461538461538462,
0.0615384615384615,0.0769230769230769,0.0923076923076923,0.107692307692308,
0.123076923076923,0.138461538461538,0.153846153846154,0.169230769230769,
0.184615384615385,0.2,0.215384615384615,0.230769230769231,0.246153846153846,
0.261538461538462,0.276923076923077,0.292307692307692,0.307692307692308,
0.323076923076923,0.338461538461538,0.353846153846154,0.369230769230769,
0.384615384615385,0.4,0.415384615384615,0.430769230769231,0.446153846153846,
0.461538461538462,0.476923076923077,0.492307692307692,0.507692307692308,
0.523076923076923,0.538461538461538,0.553846153846154,0.569230769230769,
0.584615384615384,0.6,0.615384615384615,0.63076923076923,0.646153846153846,
0.661538461538461,0.676923076923076,0.692307692307692,0.707692307692307,
0.723076923076922,0.738461538461538,0.753846153846153,0.769230769230768,
0.784615384615384,0.799999999999999,0.815384615384614,0.83076923076923,
0.846153846153845,0.86153846153846,0.876923076923076,0.892307692307691,
0.907692307692306,0.923076923076922,0.938461538461537,0.953846153846152,
0.969230769230768,0.984615384615383,1.),.UNSPECIFIED.)
CURVE()
GEOMETRIC_REPRESENTATION_ITEM()
RATIONAL_B_SPLINE_CURVE((1.,1.,1.,1.,1.,1.,1.,1.,1.,1.,1.,1.,1.,1.,1.,1.,
1.,1.,1.,1.,1.,1.,1.,1.,1.,1.,1.,1.,1.,1.,1.,1.,1.,1.,1.,1.,1.,1.,1.,1.,
1.,1.,1.,1.,1.,1.,1.,1.,1.,1.,1.,1.,1.,1.,1.,1.,1.,1.,1.,1.,1.,1.,1.,1.,
1.,1.,1.,1.,1.,1.))
REPRESENTATION_ITEM('')
);
#197=(
BOUNDED_CURVE()
B_SPLINE_CURVE(5,(#27616,#27617,#27618,#27619,#27620,#27621,#27622,#27623,
#27624,#27625,#27626,#27627,#27628,#27629,#27630,#27631,#27632,#27633,#27634,
#27635,#27636,#27637,#27638,#27639,#27640,#27641,#27642,#27643,#27644,#27645,
#27646,#27647,#27648,#27649,#27650,#27651,#27652,#27653,#27654,#27655,#27656,
#27657,#27658,#27659,#27660,#27661,#27662,#27663,#27664,#27665,#27666,#27667,
#27668,#27669,#27670,#27671,#27672,#27673,#27674,#27675,#27676,#27677,#27678,
#27679,#27680,#27681,#27682,#27683,#27684,#27685),.UNSPECIFIED.,.F.,.F.)
B_SPLINE_CURVE_WITH_KNOTS((6,1,1,1,1,1,1,1,1,1,1,1,1,1,1,1,1,1,1,1,1,1,
1,1,1,1,1,1,1,1,1,1,1,1,1,1,1,1,1,1,1,1,1,1,1,1,1,1,1,1,1,1,1,1,1,1,1,1,
1,1,1,1,1,1,1,6),(0.,0.0153846153846154,0.0307692307692308,0.0461538461538462,
0.0615384615384615,0.0769230769230769,0.0923076923076923,0.107692307692308,
0.123076923076923,0.138461538461538,0.153846153846154,0.169230769230769,
0.184615384615385,0.2,0.215384615384615,0.230769230769231,0.246153846153846,
0.261538461538462,0.276923076923077,0.292307692307692,0.307692307692308,
0.323076923076923,0.338461538461538,0.353846153846154,0.369230769230769,
0.384615384615385,0.4,0.415384615384615,0.430769230769231,0.446153846153846,
0.461538461538462,0.476923076923077,0.492307692307692,0.507692307692308,
0.523076923076923,0.538461538461538,0.553846153846154,0.569230769230769,
0.584615384615384,0.6,0.615384615384615,0.63076923076923,0.646153846153846,
0.661538461538461,0.676923076923076,0.692307692307692,0.707692307692307,
0.723076923076922,0.738461538461538,0.753846153846153,0.769230769230768,
0.784615384615384,0.799999999999999,0.815384615384614,0.83076923076923,
0.846153846153845,0.86153846153846,0.876923076923076,0.892307692307691,
0.907692307692306,0.923076923076922,0.938461538461537,0.953846153846152,
0.969230769230768,0.984615384615383,1.),.UNSPECIFIED.)
CURVE()
GEOMETRIC_REPRESENTATION_ITEM()
RATIONAL_B_SPLINE_CURVE((1.,1.,1.,1.,1.,1.,1.,1.,1.,1.,1.,1.,1.,1.,1.,1.,
1.,1.,1.,1.,1.,1.,1.,1.,1.,1.,1.,1.,1.,1.,1.,1.,1.,1.,1.,1.,1.,1.,1.,1.,
1.,1.,1.,1.,1.,1.,1.,1.,1.,1.,1.,1.,1.,1.,1.,1.,1.,1.,1.,1.,1.,1.,1.,1.,
1.,1.,1.,1.,1.,1.))
REPRESENTATION_ITEM('')
);
#198=(
BOUNDED_CURVE()
B_SPLINE_CURVE(5,(#27689,#27690,#27691,#27692,#27693,#27694,#27695,#27696,
#27697,#27698,#27699,#27700,#27701,#27702,#27703,#27704,#27705,#27706,#27707,
#27708,#27709,#27710,#27711,#27712,#27713,#27714,#27715,#27716,#27717,#27718,
#27719,#27720,#27721,#27722,#27723,#27724,#27725,#27726,#27727,#27728,#27729,
#27730,#27731,#27732,#27733,#27734,#27735,#27736,#27737,#27738,#27739,#27740,
#27741,#27742,#27743,#27744,#27745,#27746,#27747,#27748,#27749,#27750,#27751,
#27752,#27753,#27754,#27755,#27756,#27757,#27758),.UNSPECIFIED.,.F.,.F.)
B_SPLINE_CURVE_WITH_KNOTS((6,1,1,1,1,1,1,1,1,1,1,1,1,1,1,1,1,1,1,1,1,1,
1,1,1,1,1,1,1,1,1,1,1,1,1,1,1,1,1,1,1,1,1,1,1,1,1,1,1,1,1,1,1,1,1,1,1,1,
1,1,1,1,1,1,1,6),(0.,0.0153846153846154,0.0307692307692308,0.0461538461538462,
0.0615384615384615,0.0769230769230769,0.0923076923076923,0.107692307692308,
0.123076923076923,0.138461538461538,0.153846153846154,0.169230769230769,
0.184615384615385,0.2,0.215384615384615,0.230769230769231,0.246153846153846,
0.261538461538462,0.276923076923077,0.292307692307692,0.307692307692308,
0.323076923076923,0.338461538461538,0.353846153846154,0.369230769230769,
0.384615384615385,0.4,0.415384615384615,0.430769230769231,0.446153846153846,
0.461538461538462,0.476923076923077,0.492307692307692,0.507692307692308,
0.523076923076923,0.538461538461538,0.553846153846154,0.569230769230769,
0.584615384615384,0.6,0.615384615384615,0.63076923076923,0.646153846153846,
0.661538461538461,0.676923076923076,0.692307692307692,0.707692307692307,
0.723076923076922,0.738461538461538,0.753846153846153,0.769230769230768,
0.784615384615384,0.799999999999999,0.815384615384614,0.83076923076923,
0.846153846153845,0.86153846153846,0.876923076923076,0.892307692307691,
0.907692307692306,0.923076923076922,0.938461538461537,0.953846153846152,
0.969230769230768,0.984615384615383,1.),.UNSPECIFIED.)
CURVE()
GEOMETRIC_REPRESENTATION_ITEM()
RATIONAL_B_SPLINE_CURVE((1.,1.,1.,1.,1.,1.,1.,1.,1.,1.,1.,1.,1.,1.,1.,1.,
1.,1.,1.,1.,1.,1.,1.,1.,1.,1.,1.,1.,1.,1.,1.,1.,1.,1.,1.,1.,1.,1.,1.,1.,
1.,1.,1.,1.,1.,1.,1.,1.,1.,1.,1.,1.,1.,1.,1.,1.,1.,1.,1.,1.,1.,1.,1.,1.,
1.,1.,1.,1.,1.,1.))
REPRESENTATION_ITEM('')
);
#199=(
BOUNDED_CURVE()
B_SPLINE_CURVE(5,(#27762,#27763,#27764,#27765,#27766,#27767,#27768,#27769,
#27770,#27771,#27772,#27773,#27774,#27775,#27776,#27777,#27778,#27779,#27780,
#27781,#27782,#27783,#27784,#27785,#27786,#27787,#27788,#27789,#27790,#27791,
#27792,#27793,#27794,#27795,#27796,#27797,#27798,#27799,#27800,#27801,#27802,
#27803,#27804,#27805,#27806,#27807,#27808,#27809,#27810,#27811,#27812,#27813,
#27814,#27815,#27816,#27817,#27818,#27819,#27820,#27821,#27822,#27823,#27824,
#27825,#27826,#27827,#27828,#27829,#27830,#27831),.UNSPECIFIED.,.F.,.F.)
B_SPLINE_CURVE_WITH_KNOTS((6,1,1,1,1,1,1,1,1,1,1,1,1,1,1,1,1,1,1,1,1,1,
1,1,1,1,1,1,1,1,1,1,1,1,1,1,1,1,1,1,1,1,1,1,1,1,1,1,1,1,1,1,1,1,1,1,1,1,
1,1,1,1,1,1,1,6),(0.,0.0153846153846154,0.0307692307692308,0.0461538461538462,
0.0615384615384615,0.0769230769230769,0.0923076923076923,0.107692307692308,
0.123076923076923,0.138461538461538,0.153846153846154,0.169230769230769,
0.184615384615385,0.2,0.215384615384615,0.230769230769231,0.246153846153846,
0.261538461538462,0.276923076923077,0.292307692307692,0.307692307692308,
0.323076923076923,0.338461538461538,0.353846153846154,0.369230769230769,
0.384615384615385,0.4,0.415384615384615,0.430769230769231,0.446153846153846,
0.461538461538462,0.476923076923077,0.492307692307692,0.507692307692308,
0.523076923076923,0.538461538461538,0.553846153846154,0.569230769230769,
0.584615384615384,0.6,0.615384615384615,0.63076923076923,0.646153846153846,
0.661538461538461,0.676923076923076,0.692307692307692,0.707692307692307,
0.723076923076922,0.738461538461538,0.753846153846153,0.769230769230768,
0.784615384615384,0.799999999999999,0.815384615384614,0.83076923076923,
0.846153846153845,0.86153846153846,0.876923076923076,0.892307692307691,
0.907692307692306,0.923076923076922,0.938461538461537,0.953846153846152,
0.969230769230768,0.984615384615383,1.),.UNSPECIFIED.)
CURVE()
GEOMETRIC_REPRESENTATION_ITEM()
RATIONAL_B_SPLINE_CURVE((1.,1.,1.,1.,1.,1.,1.,1.,1.,1.,1.,1.,1.,1.,1.,1.,
1.,1.,1.,1.,1.,1.,1.,1.,1.,1.,1.,1.,1.,1.,1.,1.,1.,1.,1.,1.,1.,1.,1.,1.,
1.,1.,1.,1.,1.,1.,1.,1.,1.,1.,1.,1.,1.,1.,1.,1.,1.,1.,1.,1.,1.,1.,1.,1.,
1.,1.,1.,1.,1.,1.))
REPRESENTATION_ITEM('')
);
#200=(
BOUNDED_CURVE()
B_SPLINE_CURVE(5,(#27835,#27836,#27837,#27838,#27839,#27840,#27841,#27842,
#27843,#27844,#27845,#27846,#27847,#27848,#27849,#27850,#27851,#27852,#27853,
#27854,#27855,#27856,#27857,#27858,#27859,#27860,#27861,#27862,#27863,#27864,
#27865,#27866,#27867,#27868,#27869,#27870,#27871,#27872,#27873,#27874,#27875,
#27876,#27877,#27878,#27879,#27880,#27881,#27882,#27883,#27884,#27885,#27886,
#27887,#27888,#27889,#27890,#27891,#27892,#27893,#27894,#27895,#27896,#27897,
#27898,#27899,#27900,#27901,#27902,#27903,#27904),.UNSPECIFIED.,.F.,.F.)
B_SPLINE_CURVE_WITH_KNOTS((6,1,1,1,1,1,1,1,1,1,1,1,1,1,1,1,1,1,1,1,1,1,
1,1,1,1,1,1,1,1,1,1,1,1,1,1,1,1,1,1,1,1,1,1,1,1,1,1,1,1,1,1,1,1,1,1,1,1,
1,1,1,1,1,1,1,6),(0.,0.0153846153846154,0.0307692307692308,0.0461538461538462,
0.0615384615384615,0.0769230769230769,0.0923076923076923,0.107692307692308,
0.123076923076923,0.138461538461538,0.153846153846154,0.169230769230769,
0.184615384615385,0.2,0.215384615384615,0.230769230769231,0.246153846153846,
0.261538461538462,0.276923076923077,0.292307692307692,0.307692307692308,
0.323076923076923,0.338461538461538,0.353846153846154,0.369230769230769,
0.384615384615385,0.4,0.415384615384615,0.430769230769231,0.446153846153846,
0.461538461538462,0.476923076923077,0.492307692307692,0.507692307692308,
0.523076923076923,0.538461538461538,0.553846153846154,0.569230769230769,
0.584615384615384,0.6,0.615384615384615,0.63076923076923,0.646153846153846,
0.661538461538461,0.676923076923076,0.692307692307692,0.707692307692307,
0.723076923076922,0.738461538461538,0.753846153846153,0.769230769230768,
0.784615384615384,0.799999999999999,0.815384615384614,0.83076923076923,
0.846153846153845,0.86153846153846,0.876923076923076,0.892307692307691,
0.907692307692306,0.923076923076922,0.938461538461537,0.953846153846152,
0.969230769230768,0.984615384615383,1.),.UNSPECIFIED.)
CURVE()
GEOMETRIC_REPRESENTATION_ITEM()
RATIONAL_B_SPLINE_CURVE((1.,1.,1.,1.,1.,1.,1.,1.,1.,1.,1.,1.,1.,1.,1.,1.,
1.,1.,1.,1.,1.,1.,1.,1.,1.,1.,1.,1.,1.,1.,1.,1.,1.,1.,1.,1.,1.,1.,1.,1.,
1.,1.,1.,1.,1.,1.,1.,1.,1.,1.,1.,1.,1.,1.,1.,1.,1.,1.,1.,1.,1.,1.,1.,1.,
1.,1.,1.,1.,1.,1.))
REPRESENTATION_ITEM('')
);
#201=(
BOUNDED_CURVE()
B_SPLINE_CURVE(5,(#27908,#27909,#27910,#27911,#27912,#27913,#27914,#27915,
#27916,#27917,#27918,#27919,#27920,#27921,#27922,#27923,#27924,#27925,#27926,
#27927,#27928,#27929,#27930,#27931,#27932,#27933,#27934,#27935,#27936,#27937,
#27938,#27939,#27940,#27941,#27942,#27943,#27944,#27945,#27946,#27947,#27948,
#27949,#27950,#27951,#27952,#27953,#27954,#27955,#27956,#27957,#27958,#27959,
#27960,#27961,#27962,#27963,#27964,#27965,#27966,#27967,#27968,#27969,#27970,
#27971,#27972,#27973,#27974,#27975,#27976,#27977),.UNSPECIFIED.,.F.,.F.)
B_SPLINE_CURVE_WITH_KNOTS((6,1,1,1,1,1,1,1,1,1,1,1,1,1,1,1,1,1,1,1,1,1,
1,1,1,1,1,1,1,1,1,1,1,1,1,1,1,1,1,1,1,1,1,1,1,1,1,1,1,1,1,1,1,1,1,1,1,1,
1,1,1,1,1,1,1,6),(0.,0.0153846153846154,0.0307692307692308,0.0461538461538462,
0.0615384615384615,0.0769230769230769,0.0923076923076923,0.107692307692308,
0.123076923076923,0.138461538461538,0.153846153846154,0.169230769230769,
0.184615384615385,0.2,0.215384615384615,0.230769230769231,0.246153846153846,
0.261538461538462,0.276923076923077,0.292307692307692,0.307692307692308,
0.323076923076923,0.338461538461538,0.353846153846154,0.369230769230769,
0.384615384615385,0.4,0.415384615384615,0.430769230769231,0.446153846153846,
0.461538461538462,0.476923076923077,0.492307692307692,0.507692307692308,
0.523076923076923,0.538461538461538,0.553846153846154,0.569230769230769,
0.584615384615384,0.6,0.615384615384615,0.63076923076923,0.646153846153846,
0.661538461538461,0.676923076923076,0.692307692307692,0.707692307692307,
0.723076923076922,0.738461538461538,0.753846153846153,0.769230769230768,
0.784615384615384,0.799999999999999,0.815384615384614,0.83076923076923,
0.846153846153845,0.86153846153846,0.876923076923076,0.892307692307691,
0.907692307692306,0.923076923076922,0.938461538461537,0.953846153846152,
0.969230769230768,0.984615384615383,1.),.UNSPECIFIED.)
CURVE()
GEOMETRIC_REPRESENTATION_ITEM()
RATIONAL_B_SPLINE_CURVE((1.,1.,1.,1.,1.,1.,1.,1.,1.,1.,1.,1.,1.,1.,1.,1.,
1.,1.,1.,1.,1.,1.,1.,1.,1.,1.,1.,1.,1.,1.,1.,1.,1.,1.,1.,1.,1.,1.,1.,1.,
1.,1.,1.,1.,1.,1.,1.,1.,1.,1.,1.,1.,1.,1.,1.,1.,1.,1.,1.,1.,1.,1.,1.,1.,
1.,1.,1.,1.,1.,1.))
REPRESENTATION_ITEM('')
);
#202=(
BOUNDED_CURVE()
B_SPLINE_CURVE(5,(#27981,#27982,#27983,#27984,#27985,#27986,#27987,#27988,
#27989,#27990,#27991,#27992,#27993,#27994,#27995,#27996,#27997,#27998,#27999,
#28000,#28001,#28002,#28003,#28004,#28005,#28006,#28007,#28008,#28009,#28010,
#28011,#28012,#28013,#28014,#28015,#28016,#28017,#28018,#28019,#28020,#28021,
#28022,#28023,#28024,#28025,#28026,#28027,#28028,#28029,#28030,#28031,#28032,
#28033,#28034,#28035,#28036,#28037,#28038,#28039,#28040,#28041,#28042,#28043,
#28044,#28045,#28046,#28047,#28048,#28049,#28050),.UNSPECIFIED.,.F.,.F.)
B_SPLINE_CURVE_WITH_KNOTS((6,1,1,1,1,1,1,1,1,1,1,1,1,1,1,1,1,1,1,1,1,1,
1,1,1,1,1,1,1,1,1,1,1,1,1,1,1,1,1,1,1,1,1,1,1,1,1,1,1,1,1,1,1,1,1,1,1,1,
1,1,1,1,1,1,1,6),(0.,0.0153846153846154,0.0307692307692308,0.0461538461538462,
0.0615384615384615,0.0769230769230769,0.0923076923076923,0.107692307692308,
0.123076923076923,0.138461538461538,0.153846153846154,0.169230769230769,
0.184615384615385,0.2,0.215384615384615,0.230769230769231,0.246153846153846,
0.261538461538462,0.276923076923077,0.292307692307692,0.307692307692308,
0.323076923076923,0.338461538461538,0.353846153846154,0.369230769230769,
0.384615384615385,0.4,0.415384615384615,0.430769230769231,0.446153846153846,
0.461538461538462,0.476923076923077,0.492307692307692,0.507692307692308,
0.523076923076923,0.538461538461538,0.553846153846154,0.569230769230769,
0.584615384615384,0.6,0.615384615384615,0.63076923076923,0.646153846153846,
0.661538461538461,0.676923076923076,0.692307692307692,0.707692307692307,
0.723076923076922,0.738461538461538,0.753846153846153,0.769230769230768,
0.784615384615384,0.799999999999999,0.815384615384614,0.83076923076923,
0.846153846153845,0.86153846153846,0.876923076923076,0.892307692307691,
0.907692307692306,0.923076923076922,0.938461538461537,0.953846153846152,
0.969230769230768,0.984615384615383,1.),.UNSPECIFIED.)
CURVE()
GEOMETRIC_REPRESENTATION_ITEM()
RATIONAL_B_SPLINE_CURVE((1.,1.,1.,1.,1.,1.,1.,1.,1.,1.,1.,1.,1.,1.,1.,1.,
1.,1.,1.,1.,1.,1.,1.,1.,1.,1.,1.,1.,1.,1.,1.,1.,1.,1.,1.,1.,1.,1.,1.,1.,
1.,1.,1.,1.,1.,1.,1.,1.,1.,1.,1.,1.,1.,1.,1.,1.,1.,1.,1.,1.,1.,1.,1.,1.,
1.,1.,1.,1.,1.,1.))
REPRESENTATION_ITEM('')
);
#203=(
BOUNDED_CURVE()
B_SPLINE_CURVE(5,(#28054,#28055,#28056,#28057,#28058,#28059,#28060,#28061,
#28062,#28063,#28064,#28065,#28066,#28067,#28068,#28069,#28070,#28071,#28072,
#28073,#28074,#28075,#28076,#28077,#28078,#28079,#28080,#28081,#28082,#28083,
#28084,#28085,#28086,#28087,#28088,#28089,#28090,#28091,#28092,#28093,#28094,
#28095,#28096,#28097,#28098,#28099,#28100,#28101,#28102,#28103,#28104,#28105,
#28106,#28107,#28108,#28109,#28110,#28111,#28112,#28113,#28114,#28115,#28116,
#28117,#28118,#28119,#28120,#28121,#28122,#28123),.UNSPECIFIED.,.F.,.F.)
B_SPLINE_CURVE_WITH_KNOTS((6,1,1,1,1,1,1,1,1,1,1,1,1,1,1,1,1,1,1,1,1,1,
1,1,1,1,1,1,1,1,1,1,1,1,1,1,1,1,1,1,1,1,1,1,1,1,1,1,1,1,1,1,1,1,1,1,1,1,
1,1,1,1,1,1,1,6),(0.,0.0153846153846154,0.0307692307692308,0.0461538461538462,
0.0615384615384615,0.0769230769230769,0.0923076923076923,0.107692307692308,
0.123076923076923,0.138461538461538,0.153846153846154,0.169230769230769,
0.184615384615385,0.2,0.215384615384615,0.230769230769231,0.246153846153846,
0.261538461538462,0.276923076923077,0.292307692307692,0.307692307692308,
0.323076923076923,0.338461538461538,0.353846153846154,0.369230769230769,
0.384615384615385,0.4,0.415384615384615,0.430769230769231,0.446153846153846,
0.461538461538462,0.476923076923077,0.492307692307692,0.507692307692308,
0.523076923076923,0.538461538461538,0.553846153846154,0.569230769230769,
0.584615384615384,0.6,0.615384615384615,0.63076923076923,0.646153846153846,
0.661538461538461,0.676923076923076,0.692307692307692,0.707692307692307,
0.723076923076922,0.738461538461538,0.753846153846153,0.769230769230768,
0.784615384615384,0.799999999999999,0.815384615384614,0.83076923076923,
0.846153846153845,0.86153846153846,0.876923076923076,0.892307692307691,
0.907692307692306,0.923076923076922,0.938461538461537,0.953846153846152,
0.969230769230768,0.984615384615383,1.),.UNSPECIFIED.)
CURVE()
GEOMETRIC_REPRESENTATION_ITEM()
RATIONAL_B_SPLINE_CURVE((1.,1.,1.,1.,1.,1.,1.,1.,1.,1.,1.,1.,1.,1.,1.,1.,
1.,1.,1.,1.,1.,1.,1.,1.,1.,1.,1.,1.,1.,1.,1.,1.,1.,1.,1.,1.,1.,1.,1.,1.,
1.,1.,1.,1.,1.,1.,1.,1.,1.,1.,1.,1.,1.,1.,1.,1.,1.,1.,1.,1.,1.,1.,1.,1.,
1.,1.,1.,1.,1.,1.))
REPRESENTATION_ITEM('')
);
#204=(
BOUNDED_CURVE()
B_SPLINE_CURVE(5,(#28127,#28128,#28129,#28130,#28131,#28132,#28133,#28134,
#28135,#28136,#28137,#28138,#28139,#28140,#28141,#28142,#28143,#28144,#28145,
#28146,#28147,#28148,#28149,#28150,#28151,#28152,#28153,#28154,#28155,#28156,
#28157,#28158,#28159,#28160,#28161,#28162,#28163,#28164,#28165,#28166,#28167,
#28168,#28169,#28170,#28171,#28172,#28173,#28174,#28175,#28176,#28177,#28178,
#28179,#28180,#28181,#28182,#28183,#28184,#28185,#28186,#28187,#28188,#28189,
#28190,#28191,#28192,#28193,#28194,#28195,#28196),.UNSPECIFIED.,.F.,.F.)
B_SPLINE_CURVE_WITH_KNOTS((6,1,1,1,1,1,1,1,1,1,1,1,1,1,1,1,1,1,1,1,1,1,
1,1,1,1,1,1,1,1,1,1,1,1,1,1,1,1,1,1,1,1,1,1,1,1,1,1,1,1,1,1,1,1,1,1,1,1,
1,1,1,1,1,1,1,6),(0.,0.0153846153846154,0.0307692307692308,0.0461538461538462,
0.0615384615384615,0.0769230769230769,0.0923076923076923,0.107692307692308,
0.123076923076923,0.138461538461538,0.153846153846154,0.169230769230769,
0.184615384615385,0.2,0.215384615384615,0.230769230769231,0.246153846153846,
0.261538461538462,0.276923076923077,0.292307692307692,0.307692307692308,
0.323076923076923,0.338461538461538,0.353846153846154,0.369230769230769,
0.384615384615385,0.4,0.415384615384615,0.430769230769231,0.446153846153846,
0.461538461538462,0.476923076923077,0.492307692307692,0.507692307692308,
0.523076923076923,0.538461538461538,0.553846153846154,0.569230769230769,
0.584615384615384,0.6,0.615384615384615,0.63076923076923,0.646153846153846,
0.661538461538461,0.676923076923076,0.692307692307692,0.707692307692307,
0.723076923076922,0.738461538461538,0.753846153846153,0.769230769230768,
0.784615384615384,0.799999999999999,0.815384615384614,0.83076923076923,
0.846153846153845,0.86153846153846,0.876923076923076,0.892307692307691,
0.907692307692306,0.923076923076922,0.938461538461537,0.953846153846152,
0.969230769230768,0.984615384615383,1.),.UNSPECIFIED.)
CURVE()
GEOMETRIC_REPRESENTATION_ITEM()
RATIONAL_B_SPLINE_CURVE((1.,1.,1.,1.,1.,1.,1.,1.,1.,1.,1.,1.,1.,1.,1.,1.,
1.,1.,1.,1.,1.,1.,1.,1.,1.,1.,1.,1.,1.,1.,1.,1.,1.,1.,1.,1.,1.,1.,1.,1.,
1.,1.,1.,1.,1.,1.,1.,1.,1.,1.,1.,1.,1.,1.,1.,1.,1.,1.,1.,1.,1.,1.,1.,1.,
1.,1.,1.,1.,1.,1.))
REPRESENTATION_ITEM('')
);
#205=(
BOUNDED_CURVE()
B_SPLINE_CURVE(5,(#28200,#28201,#28202,#28203,#28204,#28205,#28206,#28207,
#28208,#28209,#28210,#28211,#28212,#28213,#28214,#28215,#28216,#28217,#28218,
#28219,#28220,#28221,#28222,#28223,#28224,#28225,#28226,#28227,#28228,#28229,
#28230,#28231,#28232,#28233,#28234,#28235,#28236,#28237,#28238,#28239,#28240,
#28241,#28242,#28243,#28244,#28245,#28246,#28247,#28248,#28249,#28250,#28251,
#28252,#28253,#28254,#28255,#28256,#28257,#28258,#28259,#28260,#28261,#28262,
#28263,#28264,#28265,#28266,#28267,#28268,#28269),.UNSPECIFIED.,.F.,.F.)
B_SPLINE_CURVE_WITH_KNOTS((6,1,1,1,1,1,1,1,1,1,1,1,1,1,1,1,1,1,1,1,1,1,
1,1,1,1,1,1,1,1,1,1,1,1,1,1,1,1,1,1,1,1,1,1,1,1,1,1,1,1,1,1,1,1,1,1,1,1,
1,1,1,1,1,1,1,6),(0.,0.0153846153846154,0.0307692307692308,0.0461538461538462,
0.0615384615384615,0.0769230769230769,0.0923076923076923,0.107692307692308,
0.123076923076923,0.138461538461538,0.153846153846154,0.169230769230769,
0.184615384615385,0.2,0.215384615384615,0.230769230769231,0.246153846153846,
0.261538461538462,0.276923076923077,0.292307692307692,0.307692307692308,
0.323076923076923,0.338461538461538,0.353846153846154,0.369230769230769,
0.384615384615385,0.4,0.415384615384615,0.430769230769231,0.446153846153846,
0.461538461538462,0.476923076923077,0.492307692307692,0.507692307692308,
0.523076923076923,0.538461538461538,0.553846153846154,0.569230769230769,
0.584615384615384,0.6,0.615384615384615,0.63076923076923,0.646153846153846,
0.661538461538461,0.676923076923076,0.692307692307692,0.707692307692307,
0.723076923076922,0.738461538461538,0.753846153846153,0.769230769230768,
0.784615384615384,0.799999999999999,0.815384615384614,0.83076923076923,
0.846153846153845,0.86153846153846,0.876923076923076,0.892307692307691,
0.907692307692306,0.923076923076922,0.938461538461537,0.953846153846152,
0.969230769230768,0.984615384615383,1.),.UNSPECIFIED.)
CURVE()
GEOMETRIC_REPRESENTATION_ITEM()
RATIONAL_B_SPLINE_CURVE((1.,1.,1.,1.,1.,1.,1.,1.,1.,1.,1.,1.,1.,1.,1.,1.,
1.,1.,1.,1.,1.,1.,1.,1.,1.,1.,1.,1.,1.,1.,1.,1.,1.,1.,1.,1.,1.,1.,1.,1.,
1.,1.,1.,1.,1.,1.,1.,1.,1.,1.,1.,1.,1.,1.,1.,1.,1.,1.,1.,1.,1.,1.,1.,1.,
1.,1.,1.,1.,1.,1.))
REPRESENTATION_ITEM('')
);
#206=(
BOUNDED_CURVE()
B_SPLINE_CURVE(5,(#28273,#28274,#28275,#28276,#28277,#28278,#28279,#28280,
#28281,#28282,#28283,#28284,#28285,#28286,#28287,#28288,#28289,#28290,#28291,
#28292,#28293,#28294,#28295,#28296,#28297,#28298,#28299,#28300,#28301,#28302,
#28303,#28304,#28305,#28306,#28307,#28308,#28309,#28310,#28311,#28312,#28313,
#28314,#28315,#28316,#28317,#28318,#28319,#28320,#28321,#28322,#28323,#28324,
#28325,#28326,#28327,#28328,#28329,#28330,#28331,#28332,#28333,#28334,#28335,
#28336,#28337,#28338,#28339,#28340,#28341,#28342),.UNSPECIFIED.,.F.,.F.)
B_SPLINE_CURVE_WITH_KNOTS((6,1,1,1,1,1,1,1,1,1,1,1,1,1,1,1,1,1,1,1,1,1,
1,1,1,1,1,1,1,1,1,1,1,1,1,1,1,1,1,1,1,1,1,1,1,1,1,1,1,1,1,1,1,1,1,1,1,1,
1,1,1,1,1,1,1,6),(0.,0.0153846153846154,0.0307692307692308,0.0461538461538462,
0.0615384615384615,0.0769230769230769,0.0923076923076923,0.107692307692308,
0.123076923076923,0.138461538461538,0.153846153846154,0.169230769230769,
0.184615384615385,0.2,0.215384615384615,0.230769230769231,0.246153846153846,
0.261538461538462,0.276923076923077,0.292307692307692,0.307692307692308,
0.323076923076923,0.338461538461538,0.353846153846154,0.369230769230769,
0.384615384615385,0.4,0.415384615384615,0.430769230769231,0.446153846153846,
0.461538461538462,0.476923076923077,0.492307692307692,0.507692307692308,
0.523076923076923,0.538461538461538,0.553846153846154,0.569230769230769,
0.584615384615384,0.6,0.615384615384615,0.63076923076923,0.646153846153846,
0.661538461538461,0.676923076923076,0.692307692307692,0.707692307692307,
0.723076923076922,0.738461538461538,0.753846153846153,0.769230769230768,
0.784615384615384,0.799999999999999,0.815384615384614,0.83076923076923,
0.846153846153845,0.86153846153846,0.876923076923076,0.892307692307691,
0.907692307692306,0.923076923076922,0.938461538461537,0.953846153846152,
0.969230769230768,0.984615384615383,1.),.UNSPECIFIED.)
CURVE()
GEOMETRIC_REPRESENTATION_ITEM()
RATIONAL_B_SPLINE_CURVE((1.,1.,1.,1.,1.,1.,1.,1.,1.,1.,1.,1.,1.,1.,1.,1.,
1.,1.,1.,1.,1.,1.,1.,1.,1.,1.,1.,1.,1.,1.,1.,1.,1.,1.,1.,1.,1.,1.,1.,1.,
1.,1.,1.,1.,1.,1.,1.,1.,1.,1.,1.,1.,1.,1.,1.,1.,1.,1.,1.,1.,1.,1.,1.,1.,
1.,1.,1.,1.,1.,1.))
REPRESENTATION_ITEM('')
);
#207=(
BOUNDED_CURVE()
B_SPLINE_CURVE(5,(#28346,#28347,#28348,#28349,#28350,#28351,#28352,#28353,
#28354,#28355,#28356,#28357,#28358,#28359,#28360,#28361,#28362,#28363,#28364,
#28365,#28366,#28367,#28368,#28369,#28370,#28371,#28372,#28373,#28374,#28375,
#28376,#28377,#28378,#28379,#28380,#28381,#28382,#28383,#28384,#28385,#28386,
#28387,#28388,#28389,#28390,#28391,#28392,#28393,#28394,#28395,#28396,#28397,
#28398,#28399,#28400,#28401,#28402,#28403,#28404,#28405,#28406,#28407,#28408,
#28409,#28410,#28411,#28412,#28413,#28414,#28415),.UNSPECIFIED.,.F.,.F.)
B_SPLINE_CURVE_WITH_KNOTS((6,1,1,1,1,1,1,1,1,1,1,1,1,1,1,1,1,1,1,1,1,1,
1,1,1,1,1,1,1,1,1,1,1,1,1,1,1,1,1,1,1,1,1,1,1,1,1,1,1,1,1,1,1,1,1,1,1,1,
1,1,1,1,1,1,1,6),(0.,0.0153846153846154,0.0307692307692308,0.0461538461538462,
0.0615384615384615,0.0769230769230769,0.0923076923076923,0.107692307692308,
0.123076923076923,0.138461538461538,0.153846153846154,0.169230769230769,
0.184615384615385,0.2,0.215384615384615,0.230769230769231,0.246153846153846,
0.261538461538462,0.276923076923077,0.292307692307692,0.307692307692308,
0.323076923076923,0.338461538461538,0.353846153846154,0.369230769230769,
0.384615384615385,0.4,0.415384615384615,0.430769230769231,0.446153846153846,
0.461538461538462,0.476923076923077,0.492307692307692,0.507692307692308,
0.523076923076923,0.538461538461538,0.553846153846154,0.569230769230769,
0.584615384615384,0.6,0.615384615384615,0.63076923076923,0.646153846153846,
0.661538461538461,0.676923076923076,0.692307692307692,0.707692307692307,
0.723076923076922,0.738461538461538,0.753846153846153,0.769230769230768,
0.784615384615384,0.799999999999999,0.815384615384614,0.83076923076923,
0.846153846153845,0.86153846153846,0.876923076923076,0.892307692307691,
0.907692307692306,0.923076923076922,0.938461538461537,0.953846153846152,
0.969230769230768,0.984615384615383,1.),.UNSPECIFIED.)
CURVE()
GEOMETRIC_REPRESENTATION_ITEM()
RATIONAL_B_SPLINE_CURVE((1.,1.,1.,1.,1.,1.,1.,1.,1.,1.,1.,1.,1.,1.,1.,1.,
1.,1.,1.,1.,1.,1.,1.,1.,1.,1.,1.,1.,1.,1.,1.,1.,1.,1.,1.,1.,1.,1.,1.,1.,
1.,1.,1.,1.,1.,1.,1.,1.,1.,1.,1.,1.,1.,1.,1.,1.,1.,1.,1.,1.,1.,1.,1.,1.,
1.,1.,1.,1.,1.,1.))
REPRESENTATION_ITEM('')
);
#208=(
BOUNDED_CURVE()
B_SPLINE_CURVE(5,(#28419,#28420,#28421,#28422,#28423,#28424,#28425,#28426,
#28427,#28428,#28429,#28430,#28431,#28432,#28433,#28434,#28435,#28436,#28437,
#28438,#28439,#28440,#28441,#28442,#28443,#28444,#28445,#28446,#28447,#28448,
#28449,#28450,#28451,#28452,#28453,#28454,#28455,#28456,#28457,#28458,#28459,
#28460,#28461,#28462,#28463,#28464,#28465,#28466,#28467,#28468,#28469,#28470,
#28471,#28472,#28473,#28474,#28475,#28476,#28477,#28478,#28479,#28480,#28481,
#28482,#28483,#28484,#28485,#28486,#28487,#28488),.UNSPECIFIED.,.F.,.F.)
B_SPLINE_CURVE_WITH_KNOTS((6,1,1,1,1,1,1,1,1,1,1,1,1,1,1,1,1,1,1,1,1,1,
1,1,1,1,1,1,1,1,1,1,1,1,1,1,1,1,1,1,1,1,1,1,1,1,1,1,1,1,1,1,1,1,1,1,1,1,
1,1,1,1,1,1,1,6),(0.,0.0153846153846154,0.0307692307692308,0.0461538461538462,
0.0615384615384615,0.0769230769230769,0.0923076923076923,0.107692307692308,
0.123076923076923,0.138461538461538,0.153846153846154,0.169230769230769,
0.184615384615385,0.2,0.215384615384615,0.230769230769231,0.246153846153846,
0.261538461538462,0.276923076923077,0.292307692307692,0.307692307692308,
0.323076923076923,0.338461538461538,0.353846153846154,0.369230769230769,
0.384615384615385,0.4,0.415384615384615,0.430769230769231,0.446153846153846,
0.461538461538462,0.476923076923077,0.492307692307692,0.507692307692308,
0.523076923076923,0.538461538461538,0.553846153846154,0.569230769230769,
0.584615384615384,0.6,0.615384615384615,0.63076923076923,0.646153846153846,
0.661538461538461,0.676923076923076,0.692307692307692,0.707692307692307,
0.723076923076922,0.738461538461538,0.753846153846153,0.769230769230768,
0.784615384615384,0.799999999999999,0.815384615384614,0.83076923076923,
0.846153846153845,0.86153846153846,0.876923076923076,0.892307692307691,
0.907692307692306,0.923076923076922,0.938461538461537,0.953846153846152,
0.969230769230768,0.984615384615383,1.),.UNSPECIFIED.)
CURVE()
GEOMETRIC_REPRESENTATION_ITEM()
RATIONAL_B_SPLINE_CURVE((1.,1.,1.,1.,1.,1.,1.,1.,1.,1.,1.,1.,1.,1.,1.,1.,
1.,1.,1.,1.,1.,1.,1.,1.,1.,1.,1.,1.,1.,1.,1.,1.,1.,1.,1.,1.,1.,1.,1.,1.,
1.,1.,1.,1.,1.,1.,1.,1.,1.,1.,1.,1.,1.,1.,1.,1.,1.,1.,1.,1.,1.,1.,1.,1.,
1.,1.,1.,1.,1.,1.))
REPRESENTATION_ITEM('')
);
#209=(
BOUNDED_CURVE()
B_SPLINE_CURVE(5,(#28492,#28493,#28494,#28495,#28496,#28497,#28498,#28499,
#28500,#28501,#28502,#28503,#28504,#28505,#28506,#28507,#28508,#28509,#28510,
#28511,#28512,#28513,#28514,#28515,#28516,#28517,#28518,#28519,#28520,#28521,
#28522,#28523,#28524,#28525,#28526,#28527,#28528,#28529,#28530,#28531,#28532,
#28533,#28534,#28535,#28536,#28537,#28538,#28539,#28540,#28541,#28542,#28543,
#28544,#28545,#28546,#28547,#28548,#28549,#28550,#28551,#28552,#28553,#28554,
#28555,#28556,#28557,#28558,#28559,#28560,#28561),.UNSPECIFIED.,.F.,.F.)
B_SPLINE_CURVE_WITH_KNOTS((6,1,1,1,1,1,1,1,1,1,1,1,1,1,1,1,1,1,1,1,1,1,
1,1,1,1,1,1,1,1,1,1,1,1,1,1,1,1,1,1,1,1,1,1,1,1,1,1,1,1,1,1,1,1,1,1,1,1,
1,1,1,1,1,1,1,6),(0.,0.0153846153846154,0.0307692307692308,0.0461538461538462,
0.0615384615384615,0.0769230769230769,0.0923076923076923,0.107692307692308,
0.123076923076923,0.138461538461538,0.153846153846154,0.169230769230769,
0.184615384615385,0.2,0.215384615384615,0.230769230769231,0.246153846153846,
0.261538461538462,0.276923076923077,0.292307692307692,0.307692307692308,
0.323076923076923,0.338461538461538,0.353846153846154,0.369230769230769,
0.384615384615385,0.4,0.415384615384615,0.430769230769231,0.446153846153846,
0.461538461538462,0.476923076923077,0.492307692307692,0.507692307692308,
0.523076923076923,0.538461538461538,0.553846153846154,0.569230769230769,
0.584615384615384,0.6,0.615384615384615,0.63076923076923,0.646153846153846,
0.661538461538461,0.676923076923076,0.692307692307692,0.707692307692307,
0.723076923076922,0.738461538461538,0.753846153846153,0.769230769230768,
0.784615384615384,0.799999999999999,0.815384615384614,0.83076923076923,
0.846153846153845,0.86153846153846,0.876923076923076,0.892307692307691,
0.907692307692306,0.923076923076922,0.938461538461537,0.953846153846152,
0.969230769230768,0.984615384615383,1.),.UNSPECIFIED.)
CURVE()
GEOMETRIC_REPRESENTATION_ITEM()
RATIONAL_B_SPLINE_CURVE((1.,1.,1.,1.,1.,1.,1.,1.,1.,1.,1.,1.,1.,1.,1.,1.,
1.,1.,1.,1.,1.,1.,1.,1.,1.,1.,1.,1.,1.,1.,1.,1.,1.,1.,1.,1.,1.,1.,1.,1.,
1.,1.,1.,1.,1.,1.,1.,1.,1.,1.,1.,1.,1.,1.,1.,1.,1.,1.,1.,1.,1.,1.,1.,1.,
1.,1.,1.,1.,1.,1.))
REPRESENTATION_ITEM('')
);
#210=(
BOUNDED_CURVE()
B_SPLINE_CURVE(5,(#28564,#28565,#28566,#28567,#28568,#28569,#28570,#28571,
#28572,#28573,#28574,#28575,#28576,#28577,#28578,#28579,#28580,#28581,#28582,
#28583,#28584,#28585,#28586,#28587,#28588,#28589,#28590,#28591,#28592,#28593,
#28594,#28595,#28596,#28597,#28598,#28599,#28600,#28601,#28602,#28603,#28604,
#28605,#28606,#28607,#28608,#28609,#28610,#28611,#28612,#28613,#28614,#28615,
#28616,#28617,#28618,#28619,#28620,#28621,#28622,#28623,#28624,#28625,#28626,
#28627,#28628,#28629,#28630,#28631,#28632,#28633),.UNSPECIFIED.,.F.,.F.)
B_SPLINE_CURVE_WITH_KNOTS((6,1,1,1,1,1,1,1,1,1,1,1,1,1,1,1,1,1,1,1,1,1,
1,1,1,1,1,1,1,1,1,1,1,1,1,1,1,1,1,1,1,1,1,1,1,1,1,1,1,1,1,1,1,1,1,1,1,1,
1,1,1,1,1,1,1,6),(0.,0.0153846153846154,0.0307692307692308,0.0461538461538462,
0.0615384615384615,0.0769230769230769,0.0923076923076923,0.107692307692308,
0.123076923076923,0.138461538461538,0.153846153846154,0.169230769230769,
0.184615384615385,0.2,0.215384615384615,0.230769230769231,0.246153846153846,
0.261538461538462,0.276923076923077,0.292307692307692,0.307692307692308,
0.323076923076923,0.338461538461538,0.353846153846154,0.369230769230769,
0.384615384615385,0.4,0.415384615384615,0.430769230769231,0.446153846153846,
0.461538461538462,0.476923076923077,0.492307692307692,0.507692307692308,
0.523076923076923,0.538461538461538,0.553846153846154,0.569230769230769,
0.584615384615384,0.6,0.615384615384615,0.63076923076923,0.646153846153846,
0.661538461538461,0.676923076923076,0.692307692307692,0.707692307692307,
0.723076923076922,0.738461538461538,0.753846153846153,0.769230769230768,
0.784615384615384,0.799999999999999,0.815384615384614,0.83076923076923,
0.846153846153845,0.86153846153846,0.876923076923076,0.892307692307691,
0.907692307692306,0.923076923076922,0.938461538461537,0.953846153846152,
0.969230769230768,0.984615384615383,1.),.UNSPECIFIED.)
CURVE()
GEOMETRIC_REPRESENTATION_ITEM()
RATIONAL_B_SPLINE_CURVE((1.,1.,1.,1.,1.,1.,1.,1.,1.,1.,1.,1.,1.,1.,1.,1.,
1.,1.,1.,1.,1.,1.,1.,1.,1.,1.,1.,1.,1.,1.,1.,1.,1.,1.,1.,1.,1.,1.,1.,1.,
1.,1.,1.,1.,1.,1.,1.,1.,1.,1.,1.,1.,1.,1.,1.,1.,1.,1.,1.,1.,1.,1.,1.,1.,
1.,1.,1.,1.,1.,1.))
REPRESENTATION_ITEM('')
);
#211=(
BOUNDED_CURVE()
B_SPLINE_CURVE(5,(#28787,#28788,#28789,#28790,#28791,#28792,#28793,#28794,
#28795,#28796,#28797,#28798,#28799,#28800,#28801,#28802,#28803,#28804,#28805,
#28806,#28807,#28808,#28809,#28810,#28811,#28812,#28813,#28814,#28815,#28816,
#28817,#28818,#28819,#28820,#28821,#28822,#28823,#28824,#28825,#28826,#28827,
#28828,#28829,#28830,#28831,#28832,#28833,#28834,#28835,#28836,#28837,#28838,
#28839,#28840,#28841,#28842,#28843,#28844,#28845,#28846,#28847,#28848,#28849,
#28850,#28851,#28852,#28853,#28854,#28855,#28856),.UNSPECIFIED.,.F.,.F.)
B_SPLINE_CURVE_WITH_KNOTS((6,1,1,1,1,1,1,1,1,1,1,1,1,1,1,1,1,1,1,1,1,1,
1,1,1,1,1,1,1,1,1,1,1,1,1,1,1,1,1,1,1,1,1,1,1,1,1,1,1,1,1,1,1,1,1,1,1,1,
1,1,1,1,1,1,1,6),(-1.,-0.984615384615383,-0.969230769230768,-0.953846153846152,
-0.938461538461537,-0.923076923076922,-0.907692307692306,-0.892307692307691,
-0.876923076923076,-0.86153846153846,-0.846153846153845,-0.83076923076923,
-0.815384615384614,-0.799999999999999,-0.784615384615384,-0.769230769230768,
-0.753846153846153,-0.738461538461538,-0.723076923076922,-0.707692307692307,
-0.692307692307692,-0.676923076923076,-0.661538461538461,-0.646153846153846,
-0.63076923076923,-0.615384615384615,-0.6,-0.584615384615384,-0.569230769230769,
-0.553846153846154,-0.538461538461538,-0.523076923076923,-0.507692307692308,
-0.492307692307692,-0.476923076923077,-0.461538461538462,-0.446153846153846,
-0.430769230769231,-0.415384615384615,-0.4,-0.384615384615385,-0.369230769230769,
-0.353846153846154,-0.338461538461538,-0.323076923076923,-0.307692307692308,
-0.292307692307692,-0.276923076923077,-0.261538461538462,-0.246153846153846,
-0.230769230769231,-0.215384615384615,-0.2,-0.184615384615385,-0.169230769230769,
-0.153846153846154,-0.138461538461538,-0.123076923076923,-0.107692307692308,
-0.0923076923076923,-0.0769230769230769,-0.0615384615384615,-0.0461538461538462,
-0.0307692307692308,-0.0153846153846154,0.),.UNSPECIFIED.)
CURVE()
GEOMETRIC_REPRESENTATION_ITEM()
RATIONAL_B_SPLINE_CURVE((1.,1.,1.,1.,1.,1.,1.,1.,1.,1.,1.,1.,1.,1.,1.,1.,
1.,1.,1.,1.,1.,1.,1.,1.,1.,1.,1.,1.,1.,1.,1.,1.,1.,1.,1.,1.,1.,1.,1.,1.,
1.,1.,1.,1.,1.,1.,1.,1.,1.,1.,1.,1.,1.,1.,1.,1.,1.,1.,1.,1.,1.,1.,1.,1.,
1.,1.,1.,1.,1.,1.))
REPRESENTATION_ITEM('')
);
#212=(
BOUNDED_CURVE()
B_SPLINE_CURVE(5,(#29003,#29004,#29005,#29006,#29007,#29008,#29009,#29010,
#29011,#29012,#29013,#29014,#29015,#29016,#29017,#29018,#29019,#29020,#29021,
#29022,#29023,#29024,#29025,#29026,#29027,#29028,#29029,#29030,#29031,#29032,
#29033,#29034,#29035,#29036,#29037,#29038,#29039,#29040,#29041,#29042,#29043,
#29044,#29045,#29046,#29047,#29048,#29049,#29050,#29051,#29052,#29053,#29054,
#29055,#29056,#29057,#29058,#29059,#29060,#29061,#29062,#29063,#29064,#29065,
#29066,#29067,#29068,#29069,#29070,#29071,#29072),.UNSPECIFIED.,.F.,.F.)
B_SPLINE_CURVE_WITH_KNOTS((6,1,1,1,1,1,1,1,1,1,1,1,1,1,1,1,1,1,1,1,1,1,
1,1,1,1,1,1,1,1,1,1,1,1,1,1,1,1,1,1,1,1,1,1,1,1,1,1,1,1,1,1,1,1,1,1,1,1,
1,1,1,1,1,1,1,6),(-1.,-0.984615384615383,-0.969230769230768,-0.953846153846152,
-0.938461538461537,-0.923076923076922,-0.907692307692306,-0.892307692307691,
-0.876923076923076,-0.86153846153846,-0.846153846153845,-0.83076923076923,
-0.815384615384614,-0.799999999999999,-0.784615384615384,-0.769230769230768,
-0.753846153846153,-0.738461538461538,-0.723076923076922,-0.707692307692307,
-0.692307692307692,-0.676923076923076,-0.661538461538461,-0.646153846153846,
-0.63076923076923,-0.615384615384615,-0.6,-0.584615384615384,-0.569230769230769,
-0.553846153846154,-0.538461538461538,-0.523076923076923,-0.507692307692308,
-0.492307692307692,-0.476923076923077,-0.461538461538462,-0.446153846153846,
-0.430769230769231,-0.415384615384615,-0.4,-0.384615384615385,-0.369230769230769,
-0.353846153846154,-0.338461538461538,-0.323076923076923,-0.307692307692308,
-0.292307692307692,-0.276923076923077,-0.261538461538462,-0.246153846153846,
-0.230769230769231,-0.215384615384615,-0.2,-0.184615384615385,-0.169230769230769,
-0.153846153846154,-0.138461538461538,-0.123076923076923,-0.107692307692308,
-0.0923076923076923,-0.0769230769230769,-0.0615384615384615,-0.0461538461538462,
-0.0307692307692308,-0.0153846153846154,0.),.UNSPECIFIED.)
CURVE()
GEOMETRIC_REPRESENTATION_ITEM()
RATIONAL_B_SPLINE_CURVE((1.,1.,1.,1.,1.,1.,1.,1.,1.,1.,1.,1.,1.,1.,1.,1.,
1.,1.,1.,1.,1.,1.,1.,1.,1.,1.,1.,1.,1.,1.,1.,1.,1.,1.,1.,1.,1.,1.,1.,1.,
1.,1.,1.,1.,1.,1.,1.,1.,1.,1.,1.,1.,1.,1.,1.,1.,1.,1.,1.,1.,1.,1.,1.,1.,
1.,1.,1.,1.,1.,1.))
REPRESENTATION_ITEM('')
);
#213=(
BOUNDED_CURVE()
B_SPLINE_CURVE(5,(#29219,#29220,#29221,#29222,#29223,#29224,#29225,#29226,
#29227,#29228,#29229,#29230,#29231,#29232,#29233,#29234,#29235,#29236,#29237,
#29238,#29239,#29240,#29241,#29242,#29243,#29244,#29245,#29246,#29247,#29248,
#29249,#29250,#29251,#29252,#29253,#29254,#29255,#29256,#29257,#29258,#29259,
#29260,#29261,#29262,#29263,#29264,#29265,#29266,#29267,#29268,#29269,#29270,
#29271,#29272,#29273,#29274,#29275,#29276,#29277,#29278,#29279,#29280,#29281,
#29282,#29283,#29284,#29285,#29286,#29287,#29288),.UNSPECIFIED.,.F.,.F.)
B_SPLINE_CURVE_WITH_KNOTS((6,1,1,1,1,1,1,1,1,1,1,1,1,1,1,1,1,1,1,1,1,1,
1,1,1,1,1,1,1,1,1,1,1,1,1,1,1,1,1,1,1,1,1,1,1,1,1,1,1,1,1,1,1,1,1,1,1,1,
1,1,1,1,1,1,1,6),(-1.,-0.984615384615383,-0.969230769230768,-0.953846153846152,
-0.938461538461537,-0.923076923076922,-0.907692307692306,-0.892307692307691,
-0.876923076923076,-0.86153846153846,-0.846153846153845,-0.83076923076923,
-0.815384615384614,-0.799999999999999,-0.784615384615384,-0.769230769230768,
-0.753846153846153,-0.738461538461538,-0.723076923076922,-0.707692307692307,
-0.692307692307692,-0.676923076923076,-0.661538461538461,-0.646153846153846,
-0.63076923076923,-0.615384615384615,-0.6,-0.584615384615384,-0.569230769230769,
-0.553846153846154,-0.538461538461538,-0.523076923076923,-0.507692307692308,
-0.492307692307692,-0.476923076923077,-0.461538461538462,-0.446153846153846,
-0.430769230769231,-0.415384615384615,-0.4,-0.384615384615385,-0.369230769230769,
-0.353846153846154,-0.338461538461538,-0.323076923076923,-0.307692307692308,
-0.292307692307692,-0.276923076923077,-0.261538461538462,-0.246153846153846,
-0.230769230769231,-0.215384615384615,-0.2,-0.184615384615385,-0.169230769230769,
-0.153846153846154,-0.138461538461538,-0.123076923076923,-0.107692307692308,
-0.0923076923076923,-0.0769230769230769,-0.0615384615384615,-0.0461538461538462,
-0.0307692307692308,-0.0153846153846154,0.),.UNSPECIFIED.)
CURVE()
GEOMETRIC_REPRESENTATION_ITEM()
RATIONAL_B_SPLINE_CURVE((1.,1.,1.,1.,1.,1.,1.,1.,1.,1.,1.,1.,1.,1.,1.,1.,
1.,1.,1.,1.,1.,1.,1.,1.,1.,1.,1.,1.,1.,1.,1.,1.,1.,1.,1.,1.,1.,1.,1.,1.,
1.,1.,1.,1.,1.,1.,1.,1.,1.,1.,1.,1.,1.,1.,1.,1.,1.,1.,1.,1.,1.,1.,1.,1.,
1.,1.,1.,1.,1.,1.))
REPRESENTATION_ITEM('')
);
#214=(
BOUNDED_CURVE()
B_SPLINE_CURVE(5,(#29435,#29436,#29437,#29438,#29439,#29440,#29441,#29442,
#29443,#29444,#29445,#29446,#29447,#29448,#29449,#29450,#29451,#29452,#29453,
#29454,#29455,#29456,#29457,#29458,#29459,#29460,#29461,#29462,#29463,#29464,
#29465,#29466,#29467,#29468,#29469,#29470,#29471,#29472,#29473,#29474,#29475,
#29476,#29477,#29478,#29479,#29480,#29481,#29482,#29483,#29484,#29485,#29486,
#29487,#29488,#29489,#29490,#29491,#29492,#29493,#29494,#29495,#29496,#29497,
#29498,#29499,#29500,#29501,#29502,#29503,#29504),.UNSPECIFIED.,.F.,.F.)
B_SPLINE_CURVE_WITH_KNOTS((6,1,1,1,1,1,1,1,1,1,1,1,1,1,1,1,1,1,1,1,1,1,
1,1,1,1,1,1,1,1,1,1,1,1,1,1,1,1,1,1,1,1,1,1,1,1,1,1,1,1,1,1,1,1,1,1,1,1,
1,1,1,1,1,1,1,6),(-1.,-0.984615384615383,-0.969230769230768,-0.953846153846152,
-0.938461538461537,-0.923076923076922,-0.907692307692306,-0.892307692307691,
-0.876923076923076,-0.86153846153846,-0.846153846153845,-0.83076923076923,
-0.815384615384614,-0.799999999999999,-0.784615384615384,-0.769230769230768,
-0.753846153846153,-0.738461538461538,-0.723076923076922,-0.707692307692307,
-0.692307692307692,-0.676923076923076,-0.661538461538461,-0.646153846153846,
-0.63076923076923,-0.615384615384615,-0.6,-0.584615384615384,-0.569230769230769,
-0.553846153846154,-0.538461538461538,-0.523076923076923,-0.507692307692308,
-0.492307692307692,-0.476923076923077,-0.461538461538462,-0.446153846153846,
-0.430769230769231,-0.415384615384615,-0.4,-0.384615384615385,-0.369230769230769,
-0.353846153846154,-0.338461538461538,-0.323076923076923,-0.307692307692308,
-0.292307692307692,-0.276923076923077,-0.261538461538462,-0.246153846153846,
-0.230769230769231,-0.215384615384615,-0.2,-0.184615384615385,-0.169230769230769,
-0.153846153846154,-0.138461538461538,-0.123076923076923,-0.107692307692308,
-0.0923076923076923,-0.0769230769230769,-0.0615384615384615,-0.0461538461538462,
-0.0307692307692308,-0.0153846153846154,0.),.UNSPECIFIED.)
CURVE()
GEOMETRIC_REPRESENTATION_ITEM()
RATIONAL_B_SPLINE_CURVE((1.,1.,1.,1.,1.,1.,1.,1.,1.,1.,1.,1.,1.,1.,1.,1.,
1.,1.,1.,1.,1.,1.,1.,1.,1.,1.,1.,1.,1.,1.,1.,1.,1.,1.,1.,1.,1.,1.,1.,1.,
1.,1.,1.,1.,1.,1.,1.,1.,1.,1.,1.,1.,1.,1.,1.,1.,1.,1.,1.,1.,1.,1.,1.,1.,
1.,1.,1.,1.,1.,1.))
REPRESENTATION_ITEM('')
);
#215=(
BOUNDED_CURVE()
B_SPLINE_CURVE(5,(#29651,#29652,#29653,#29654,#29655,#29656,#29657,#29658,
#29659,#29660,#29661,#29662,#29663,#29664,#29665,#29666,#29667,#29668,#29669,
#29670,#29671,#29672,#29673,#29674,#29675,#29676,#29677,#29678,#29679,#29680,
#29681,#29682,#29683,#29684,#29685,#29686,#29687,#29688,#29689,#29690,#29691,
#29692,#29693,#29694,#29695,#29696,#29697,#29698,#29699,#29700,#29701,#29702,
#29703,#29704,#29705,#29706,#29707,#29708,#29709,#29710,#29711,#29712,#29713,
#29714,#29715,#29716,#29717,#29718,#29719,#29720),.UNSPECIFIED.,.F.,.F.)
B_SPLINE_CURVE_WITH_KNOTS((6,1,1,1,1,1,1,1,1,1,1,1,1,1,1,1,1,1,1,1,1,1,
1,1,1,1,1,1,1,1,1,1,1,1,1,1,1,1,1,1,1,1,1,1,1,1,1,1,1,1,1,1,1,1,1,1,1,1,
1,1,1,1,1,1,1,6),(-1.,-0.984615384615383,-0.969230769230768,-0.953846153846152,
-0.938461538461537,-0.923076923076922,-0.907692307692306,-0.892307692307691,
-0.876923076923076,-0.86153846153846,-0.846153846153845,-0.83076923076923,
-0.815384615384614,-0.799999999999999,-0.784615384615384,-0.769230769230768,
-0.753846153846153,-0.738461538461538,-0.723076923076922,-0.707692307692307,
-0.692307692307692,-0.676923076923076,-0.661538461538461,-0.646153846153846,
-0.63076923076923,-0.615384615384615,-0.6,-0.584615384615384,-0.569230769230769,
-0.553846153846154,-0.538461538461538,-0.523076923076923,-0.507692307692308,
-0.492307692307692,-0.476923076923077,-0.461538461538462,-0.446153846153846,
-0.430769230769231,-0.415384615384615,-0.4,-0.384615384615385,-0.369230769230769,
-0.353846153846154,-0.338461538461538,-0.323076923076923,-0.307692307692308,
-0.292307692307692,-0.276923076923077,-0.261538461538462,-0.246153846153846,
-0.230769230769231,-0.215384615384615,-0.2,-0.184615384615385,-0.169230769230769,
-0.153846153846154,-0.138461538461538,-0.123076923076923,-0.107692307692308,
-0.0923076923076923,-0.0769230769230769,-0.0615384615384615,-0.0461538461538462,
-0.0307692307692308,-0.0153846153846154,0.),.UNSPECIFIED.)
CURVE()
GEOMETRIC_REPRESENTATION_ITEM()
RATIONAL_B_SPLINE_CURVE((1.,1.,1.,1.,1.,1.,1.,1.,1.,1.,1.,1.,1.,1.,1.,1.,
1.,1.,1.,1.,1.,1.,1.,1.,1.,1.,1.,1.,1.,1.,1.,1.,1.,1.,1.,1.,1.,1.,1.,1.,
1.,1.,1.,1.,1.,1.,1.,1.,1.,1.,1.,1.,1.,1.,1.,1.,1.,1.,1.,1.,1.,1.,1.,1.,
1.,1.,1.,1.,1.,1.))
REPRESENTATION_ITEM('')
);
#216=(
BOUNDED_CURVE()
B_SPLINE_CURVE(5,(#29867,#29868,#29869,#29870,#29871,#29872,#29873,#29874,
#29875,#29876,#29877,#29878,#29879,#29880,#29881,#29882,#29883,#29884,#29885,
#29886,#29887,#29888,#29889,#29890,#29891,#29892,#29893,#29894,#29895,#29896,
#29897,#29898,#29899,#29900,#29901,#29902,#29903,#29904,#29905,#29906,#29907,
#29908,#29909,#29910,#29911,#29912,#29913,#29914,#29915,#29916,#29917,#29918,
#29919,#29920,#29921,#29922,#29923,#29924,#29925,#29926,#29927,#29928,#29929,
#29930,#29931,#29932,#29933,#29934,#29935,#29936),.UNSPECIFIED.,.F.,.F.)
B_SPLINE_CURVE_WITH_KNOTS((6,1,1,1,1,1,1,1,1,1,1,1,1,1,1,1,1,1,1,1,1,1,
1,1,1,1,1,1,1,1,1,1,1,1,1,1,1,1,1,1,1,1,1,1,1,1,1,1,1,1,1,1,1,1,1,1,1,1,
1,1,1,1,1,1,1,6),(-1.,-0.984615384615383,-0.969230769230768,-0.953846153846152,
-0.938461538461537,-0.923076923076922,-0.907692307692306,-0.892307692307691,
-0.876923076923076,-0.86153846153846,-0.846153846153845,-0.83076923076923,
-0.815384615384614,-0.799999999999999,-0.784615384615384,-0.769230769230768,
-0.753846153846153,-0.738461538461538,-0.723076923076922,-0.707692307692307,
-0.692307692307692,-0.676923076923076,-0.661538461538461,-0.646153846153846,
-0.63076923076923,-0.615384615384615,-0.6,-0.584615384615384,-0.569230769230769,
-0.553846153846154,-0.538461538461538,-0.523076923076923,-0.507692307692308,
-0.492307692307692,-0.476923076923077,-0.461538461538462,-0.446153846153846,
-0.430769230769231,-0.415384615384615,-0.4,-0.384615384615385,-0.369230769230769,
-0.353846153846154,-0.338461538461538,-0.323076923076923,-0.307692307692308,
-0.292307692307692,-0.276923076923077,-0.261538461538462,-0.246153846153846,
-0.230769230769231,-0.215384615384615,-0.2,-0.184615384615385,-0.169230769230769,
-0.153846153846154,-0.138461538461538,-0.123076923076923,-0.107692307692308,
-0.0923076923076923,-0.0769230769230769,-0.0615384615384615,-0.0461538461538462,
-0.0307692307692308,-0.0153846153846154,0.),.UNSPECIFIED.)
CURVE()
GEOMETRIC_REPRESENTATION_ITEM()
RATIONAL_B_SPLINE_CURVE((1.,1.,1.,1.,1.,1.,1.,1.,1.,1.,1.,1.,1.,1.,1.,1.,
1.,1.,1.,1.,1.,1.,1.,1.,1.,1.,1.,1.,1.,1.,1.,1.,1.,1.,1.,1.,1.,1.,1.,1.,
1.,1.,1.,1.,1.,1.,1.,1.,1.,1.,1.,1.,1.,1.,1.,1.,1.,1.,1.,1.,1.,1.,1.,1.,
1.,1.,1.,1.,1.,1.))
REPRESENTATION_ITEM('')
);
#217=(
BOUNDED_CURVE()
B_SPLINE_CURVE(5,(#30083,#30084,#30085,#30086,#30087,#30088,#30089,#30090,
#30091,#30092,#30093,#30094,#30095,#30096,#30097,#30098,#30099,#30100,#30101,
#30102,#30103,#30104,#30105,#30106,#30107,#30108,#30109,#30110,#30111,#30112,
#30113,#30114,#30115,#30116,#30117,#30118,#30119,#30120,#30121,#30122,#30123,
#30124,#30125,#30126,#30127,#30128,#30129,#30130,#30131,#30132,#30133,#30134,
#30135,#30136,#30137,#30138,#30139,#30140,#30141,#30142,#30143,#30144,#30145,
#30146,#30147,#30148,#30149,#30150,#30151,#30152),.UNSPECIFIED.,.F.,.F.)
B_SPLINE_CURVE_WITH_KNOTS((6,1,1,1,1,1,1,1,1,1,1,1,1,1,1,1,1,1,1,1,1,1,
1,1,1,1,1,1,1,1,1,1,1,1,1,1,1,1,1,1,1,1,1,1,1,1,1,1,1,1,1,1,1,1,1,1,1,1,
1,1,1,1,1,1,1,6),(-1.,-0.984615384615383,-0.969230769230768,-0.953846153846152,
-0.938461538461537,-0.923076923076922,-0.907692307692306,-0.892307692307691,
-0.876923076923076,-0.86153846153846,-0.846153846153845,-0.83076923076923,
-0.815384615384614,-0.799999999999999,-0.784615384615384,-0.769230769230768,
-0.753846153846153,-0.738461538461538,-0.723076923076922,-0.707692307692307,
-0.692307692307692,-0.676923076923076,-0.661538461538461,-0.646153846153846,
-0.63076923076923,-0.615384615384615,-0.6,-0.584615384615384,-0.569230769230769,
-0.553846153846154,-0.538461538461538,-0.523076923076923,-0.507692307692308,
-0.492307692307692,-0.476923076923077,-0.461538461538462,-0.446153846153846,
-0.430769230769231,-0.415384615384615,-0.4,-0.384615384615385,-0.369230769230769,
-0.353846153846154,-0.338461538461538,-0.323076923076923,-0.307692307692308,
-0.292307692307692,-0.276923076923077,-0.261538461538462,-0.246153846153846,
-0.230769230769231,-0.215384615384615,-0.2,-0.184615384615385,-0.169230769230769,
-0.153846153846154,-0.138461538461538,-0.123076923076923,-0.107692307692308,
-0.0923076923076923,-0.0769230769230769,-0.0615384615384615,-0.0461538461538462,
-0.0307692307692308,-0.0153846153846154,0.),.UNSPECIFIED.)
CURVE()
GEOMETRIC_REPRESENTATION_ITEM()
RATIONAL_B_SPLINE_CURVE((1.,1.,1.,1.,1.,1.,1.,1.,1.,1.,1.,1.,1.,1.,1.,1.,
1.,1.,1.,1.,1.,1.,1.,1.,1.,1.,1.,1.,1.,1.,1.,1.,1.,1.,1.,1.,1.,1.,1.,1.,
1.,1.,1.,1.,1.,1.,1.,1.,1.,1.,1.,1.,1.,1.,1.,1.,1.,1.,1.,1.,1.,1.,1.,1.,
1.,1.,1.,1.,1.,1.))
REPRESENTATION_ITEM('')
);
#218=(
BOUNDED_CURVE()
B_SPLINE_CURVE(5,(#30299,#30300,#30301,#30302,#30303,#30304,#30305,#30306,
#30307,#30308,#30309,#30310,#30311,#30312,#30313,#30314,#30315,#30316,#30317,
#30318,#30319,#30320,#30321,#30322,#30323,#30324,#30325,#30326,#30327,#30328,
#30329,#30330,#30331,#30332,#30333,#30334,#30335,#30336,#30337,#30338,#30339,
#30340,#30341,#30342,#30343,#30344,#30345,#30346,#30347,#30348,#30349,#30350,
#30351,#30352,#30353,#30354,#30355,#30356,#30357,#30358,#30359,#30360,#30361,
#30362,#30363,#30364,#30365,#30366,#30367,#30368),.UNSPECIFIED.,.F.,.F.)
B_SPLINE_CURVE_WITH_KNOTS((6,1,1,1,1,1,1,1,1,1,1,1,1,1,1,1,1,1,1,1,1,1,
1,1,1,1,1,1,1,1,1,1,1,1,1,1,1,1,1,1,1,1,1,1,1,1,1,1,1,1,1,1,1,1,1,1,1,1,
1,1,1,1,1,1,1,6),(-1.,-0.984615384615383,-0.969230769230768,-0.953846153846152,
-0.938461538461537,-0.923076923076922,-0.907692307692306,-0.892307692307691,
-0.876923076923076,-0.86153846153846,-0.846153846153845,-0.83076923076923,
-0.815384615384614,-0.799999999999999,-0.784615384615384,-0.769230769230768,
-0.753846153846153,-0.738461538461538,-0.723076923076922,-0.707692307692307,
-0.692307692307692,-0.676923076923076,-0.661538461538461,-0.646153846153846,
-0.63076923076923,-0.615384615384615,-0.6,-0.584615384615384,-0.569230769230769,
-0.553846153846154,-0.538461538461538,-0.523076923076923,-0.507692307692308,
-0.492307692307692,-0.476923076923077,-0.461538461538462,-0.446153846153846,
-0.430769230769231,-0.415384615384615,-0.4,-0.384615384615385,-0.369230769230769,
-0.353846153846154,-0.338461538461538,-0.323076923076923,-0.307692307692308,
-0.292307692307692,-0.276923076923077,-0.261538461538462,-0.246153846153846,
-0.230769230769231,-0.215384615384615,-0.2,-0.184615384615385,-0.169230769230769,
-0.153846153846154,-0.138461538461538,-0.123076923076923,-0.107692307692308,
-0.0923076923076923,-0.0769230769230769,-0.0615384615384615,-0.0461538461538462,
-0.0307692307692308,-0.0153846153846154,0.),.UNSPECIFIED.)
CURVE()
GEOMETRIC_REPRESENTATION_ITEM()
RATIONAL_B_SPLINE_CURVE((1.,1.,1.,1.,1.,1.,1.,1.,1.,1.,1.,1.,1.,1.,1.,1.,
1.,1.,1.,1.,1.,1.,1.,1.,1.,1.,1.,1.,1.,1.,1.,1.,1.,1.,1.,1.,1.,1.,1.,1.,
1.,1.,1.,1.,1.,1.,1.,1.,1.,1.,1.,1.,1.,1.,1.,1.,1.,1.,1.,1.,1.,1.,1.,1.,
1.,1.,1.,1.,1.,1.))
REPRESENTATION_ITEM('')
);
#219=(
BOUNDED_CURVE()
B_SPLINE_CURVE(5,(#30515,#30516,#30517,#30518,#30519,#30520,#30521,#30522,
#30523,#30524,#30525,#30526,#30527,#30528,#30529,#30530,#30531,#30532,#30533,
#30534,#30535,#30536,#30537,#30538,#30539,#30540,#30541,#30542,#30543,#30544,
#30545,#30546,#30547,#30548,#30549,#30550,#30551,#30552,#30553,#30554,#30555,
#30556,#30557,#30558,#30559,#30560,#30561,#30562,#30563,#30564,#30565,#30566,
#30567,#30568,#30569,#30570,#30571,#30572,#30573,#30574,#30575,#30576,#30577,
#30578,#30579,#30580,#30581,#30582,#30583,#30584),.UNSPECIFIED.,.F.,.F.)
B_SPLINE_CURVE_WITH_KNOTS((6,1,1,1,1,1,1,1,1,1,1,1,1,1,1,1,1,1,1,1,1,1,
1,1,1,1,1,1,1,1,1,1,1,1,1,1,1,1,1,1,1,1,1,1,1,1,1,1,1,1,1,1,1,1,1,1,1,1,
1,1,1,1,1,1,1,6),(-1.,-0.984615384615383,-0.969230769230768,-0.953846153846152,
-0.938461538461537,-0.923076923076922,-0.907692307692306,-0.892307692307691,
-0.876923076923076,-0.86153846153846,-0.846153846153845,-0.83076923076923,
-0.815384615384614,-0.799999999999999,-0.784615384615384,-0.769230769230768,
-0.753846153846153,-0.738461538461538,-0.723076923076922,-0.707692307692307,
-0.692307692307692,-0.676923076923076,-0.661538461538461,-0.646153846153846,
-0.63076923076923,-0.615384615384615,-0.6,-0.584615384615384,-0.569230769230769,
-0.553846153846154,-0.538461538461538,-0.523076923076923,-0.507692307692308,
-0.492307692307692,-0.476923076923077,-0.461538461538462,-0.446153846153846,
-0.430769230769231,-0.415384615384615,-0.4,-0.384615384615385,-0.369230769230769,
-0.353846153846154,-0.338461538461538,-0.323076923076923,-0.307692307692308,
-0.292307692307692,-0.276923076923077,-0.261538461538462,-0.246153846153846,
-0.230769230769231,-0.215384615384615,-0.2,-0.184615384615385,-0.169230769230769,
-0.153846153846154,-0.138461538461538,-0.123076923076923,-0.107692307692308,
-0.0923076923076923,-0.0769230769230769,-0.0615384615384615,-0.0461538461538462,
-0.0307692307692308,-0.0153846153846154,0.),.UNSPECIFIED.)
CURVE()
GEOMETRIC_REPRESENTATION_ITEM()
RATIONAL_B_SPLINE_CURVE((1.,1.,1.,1.,1.,1.,1.,1.,1.,1.,1.,1.,1.,1.,1.,1.,
1.,1.,1.,1.,1.,1.,1.,1.,1.,1.,1.,1.,1.,1.,1.,1.,1.,1.,1.,1.,1.,1.,1.,1.,
1.,1.,1.,1.,1.,1.,1.,1.,1.,1.,1.,1.,1.,1.,1.,1.,1.,1.,1.,1.,1.,1.,1.,1.,
1.,1.,1.,1.,1.,1.))
REPRESENTATION_ITEM('')
);
#220=(
BOUNDED_CURVE()
B_SPLINE_CURVE(5,(#30731,#30732,#30733,#30734,#30735,#30736,#30737,#30738,
#30739,#30740,#30741,#30742,#30743,#30744,#30745,#30746,#30747,#30748,#30749,
#30750,#30751,#30752,#30753,#30754,#30755,#30756,#30757,#30758,#30759,#30760,
#30761,#30762,#30763,#30764,#30765,#30766,#30767,#30768,#30769,#30770,#30771,
#30772,#30773,#30774,#30775,#30776,#30777,#30778,#30779,#30780,#30781,#30782,
#30783,#30784,#30785,#30786,#30787,#30788,#30789,#30790,#30791,#30792,#30793,
#30794,#30795,#30796,#30797,#30798,#30799,#30800),.UNSPECIFIED.,.F.,.F.)
B_SPLINE_CURVE_WITH_KNOTS((6,1,1,1,1,1,1,1,1,1,1,1,1,1,1,1,1,1,1,1,1,1,
1,1,1,1,1,1,1,1,1,1,1,1,1,1,1,1,1,1,1,1,1,1,1,1,1,1,1,1,1,1,1,1,1,1,1,1,
1,1,1,1,1,1,1,6),(-1.,-0.984615384615383,-0.969230769230768,-0.953846153846152,
-0.938461538461537,-0.923076923076922,-0.907692307692306,-0.892307692307691,
-0.876923076923076,-0.86153846153846,-0.846153846153845,-0.83076923076923,
-0.815384615384614,-0.799999999999999,-0.784615384615384,-0.769230769230768,
-0.753846153846153,-0.738461538461538,-0.723076923076922,-0.707692307692307,
-0.692307692307692,-0.676923076923076,-0.661538461538461,-0.646153846153846,
-0.63076923076923,-0.615384615384615,-0.6,-0.584615384615384,-0.569230769230769,
-0.553846153846154,-0.538461538461538,-0.523076923076923,-0.507692307692308,
-0.492307692307692,-0.476923076923077,-0.461538461538462,-0.446153846153846,
-0.430769230769231,-0.415384615384615,-0.4,-0.384615384615385,-0.369230769230769,
-0.353846153846154,-0.338461538461538,-0.323076923076923,-0.307692307692308,
-0.292307692307692,-0.276923076923077,-0.261538461538462,-0.246153846153846,
-0.230769230769231,-0.215384615384615,-0.2,-0.184615384615385,-0.169230769230769,
-0.153846153846154,-0.138461538461538,-0.123076923076923,-0.107692307692308,
-0.0923076923076923,-0.0769230769230769,-0.0615384615384615,-0.0461538461538462,
-0.0307692307692308,-0.0153846153846154,0.),.UNSPECIFIED.)
CURVE()
GEOMETRIC_REPRESENTATION_ITEM()
RATIONAL_B_SPLINE_CURVE((1.,1.,1.,1.,1.,1.,1.,1.,1.,1.,1.,1.,1.,1.,1.,1.,
1.,1.,1.,1.,1.,1.,1.,1.,1.,1.,1.,1.,1.,1.,1.,1.,1.,1.,1.,1.,1.,1.,1.,1.,
1.,1.,1.,1.,1.,1.,1.,1.,1.,1.,1.,1.,1.,1.,1.,1.,1.,1.,1.,1.,1.,1.,1.,1.,
1.,1.,1.,1.,1.,1.))
REPRESENTATION_ITEM('')
);
#221=(
BOUNDED_CURVE()
B_SPLINE_CURVE(5,(#30947,#30948,#30949,#30950,#30951,#30952,#30953,#30954,
#30955,#30956,#30957,#30958,#30959,#30960,#30961,#30962,#30963,#30964,#30965,
#30966,#30967,#30968,#30969,#30970,#30971,#30972,#30973,#30974,#30975,#30976,
#30977,#30978,#30979,#30980,#30981,#30982,#30983,#30984,#30985,#30986,#30987,
#30988,#30989,#30990,#30991,#30992,#30993,#30994,#30995,#30996,#30997,#30998,
#30999,#31000,#31001,#31002,#31003,#31004,#31005,#31006,#31007,#31008,#31009,
#31010,#31011,#31012,#31013,#31014,#31015,#31016),.UNSPECIFIED.,.F.,.F.)
B_SPLINE_CURVE_WITH_KNOTS((6,1,1,1,1,1,1,1,1,1,1,1,1,1,1,1,1,1,1,1,1,1,
1,1,1,1,1,1,1,1,1,1,1,1,1,1,1,1,1,1,1,1,1,1,1,1,1,1,1,1,1,1,1,1,1,1,1,1,
1,1,1,1,1,1,1,6),(-1.,-0.984615384615383,-0.969230769230768,-0.953846153846152,
-0.938461538461537,-0.923076923076922,-0.907692307692306,-0.892307692307691,
-0.876923076923076,-0.86153846153846,-0.846153846153845,-0.83076923076923,
-0.815384615384614,-0.799999999999999,-0.784615384615384,-0.769230769230768,
-0.753846153846153,-0.738461538461538,-0.723076923076922,-0.707692307692307,
-0.692307692307692,-0.676923076923076,-0.661538461538461,-0.646153846153846,
-0.63076923076923,-0.615384615384615,-0.6,-0.584615384615384,-0.569230769230769,
-0.553846153846154,-0.538461538461538,-0.523076923076923,-0.507692307692308,
-0.492307692307692,-0.476923076923077,-0.461538461538462,-0.446153846153846,
-0.430769230769231,-0.415384615384615,-0.4,-0.384615384615385,-0.369230769230769,
-0.353846153846154,-0.338461538461538,-0.323076923076923,-0.307692307692308,
-0.292307692307692,-0.276923076923077,-0.261538461538462,-0.246153846153846,
-0.230769230769231,-0.215384615384615,-0.2,-0.184615384615385,-0.169230769230769,
-0.153846153846154,-0.138461538461538,-0.123076923076923,-0.107692307692308,
-0.0923076923076923,-0.0769230769230769,-0.0615384615384615,-0.0461538461538462,
-0.0307692307692308,-0.0153846153846154,0.),.UNSPECIFIED.)
CURVE()
GEOMETRIC_REPRESENTATION_ITEM()
RATIONAL_B_SPLINE_CURVE((1.,1.,1.,1.,1.,1.,1.,1.,1.,1.,1.,1.,1.,1.,1.,1.,
1.,1.,1.,1.,1.,1.,1.,1.,1.,1.,1.,1.,1.,1.,1.,1.,1.,1.,1.,1.,1.,1.,1.,1.,
1.,1.,1.,1.,1.,1.,1.,1.,1.,1.,1.,1.,1.,1.,1.,1.,1.,1.,1.,1.,1.,1.,1.,1.,
1.,1.,1.,1.,1.,1.))
REPRESENTATION_ITEM('')
);
#222=(
BOUNDED_CURVE()
B_SPLINE_CURVE(5,(#31163,#31164,#31165,#31166,#31167,#31168,#31169,#31170,
#31171,#31172,#31173,#31174,#31175,#31176,#31177,#31178,#31179,#31180,#31181,
#31182,#31183,#31184,#31185,#31186,#31187,#31188,#31189,#31190,#31191,#31192,
#31193,#31194,#31195,#31196,#31197,#31198,#31199,#31200,#31201,#31202,#31203,
#31204,#31205,#31206,#31207,#31208,#31209,#31210,#31211,#31212,#31213,#31214,
#31215,#31216,#31217,#31218,#31219,#31220,#31221,#31222,#31223,#31224,#31225,
#31226,#31227,#31228,#31229,#31230,#31231,#31232),.UNSPECIFIED.,.F.,.F.)
B_SPLINE_CURVE_WITH_KNOTS((6,1,1,1,1,1,1,1,1,1,1,1,1,1,1,1,1,1,1,1,1,1,
1,1,1,1,1,1,1,1,1,1,1,1,1,1,1,1,1,1,1,1,1,1,1,1,1,1,1,1,1,1,1,1,1,1,1,1,
1,1,1,1,1,1,1,6),(-1.,-0.984615384615383,-0.969230769230768,-0.953846153846152,
-0.938461538461537,-0.923076923076922,-0.907692307692306,-0.892307692307691,
-0.876923076923076,-0.86153846153846,-0.846153846153845,-0.83076923076923,
-0.815384615384614,-0.799999999999999,-0.784615384615384,-0.769230769230768,
-0.753846153846153,-0.738461538461538,-0.723076923076922,-0.707692307692307,
-0.692307692307692,-0.676923076923076,-0.661538461538461,-0.646153846153846,
-0.63076923076923,-0.615384615384615,-0.6,-0.584615384615384,-0.569230769230769,
-0.553846153846154,-0.538461538461538,-0.523076923076923,-0.507692307692308,
-0.492307692307692,-0.476923076923077,-0.461538461538462,-0.446153846153846,
-0.430769230769231,-0.415384615384615,-0.4,-0.384615384615385,-0.369230769230769,
-0.353846153846154,-0.338461538461538,-0.323076923076923,-0.307692307692308,
-0.292307692307692,-0.276923076923077,-0.261538461538462,-0.246153846153846,
-0.230769230769231,-0.215384615384615,-0.2,-0.184615384615385,-0.169230769230769,
-0.153846153846154,-0.138461538461538,-0.123076923076923,-0.107692307692308,
-0.0923076923076923,-0.0769230769230769,-0.0615384615384615,-0.0461538461538462,
-0.0307692307692308,-0.0153846153846154,0.),.UNSPECIFIED.)
CURVE()
GEOMETRIC_REPRESENTATION_ITEM()
RATIONAL_B_SPLINE_CURVE((1.,1.,1.,1.,1.,1.,1.,1.,1.,1.,1.,1.,1.,1.,1.,1.,
1.,1.,1.,1.,1.,1.,1.,1.,1.,1.,1.,1.,1.,1.,1.,1.,1.,1.,1.,1.,1.,1.,1.,1.,
1.,1.,1.,1.,1.,1.,1.,1.,1.,1.,1.,1.,1.,1.,1.,1.,1.,1.,1.,1.,1.,1.,1.,1.,
1.,1.,1.,1.,1.,1.))
REPRESENTATION_ITEM('')
);
#223=(
BOUNDED_CURVE()
B_SPLINE_CURVE(5,(#31379,#31380,#31381,#31382,#31383,#31384,#31385,#31386,
#31387,#31388,#31389,#31390,#31391,#31392,#31393,#31394,#31395,#31396,#31397,
#31398,#31399,#31400,#31401,#31402,#31403,#31404,#31405,#31406,#31407,#31408,
#31409,#31410,#31411,#31412,#31413,#31414,#31415,#31416,#31417,#31418,#31419,
#31420,#31421,#31422,#31423,#31424,#31425,#31426,#31427,#31428,#31429,#31430,
#31431,#31432,#31433,#31434,#31435,#31436,#31437,#31438,#31439,#31440,#31441,
#31442,#31443,#31444,#31445,#31446,#31447,#31448),.UNSPECIFIED.,.F.,.F.)
B_SPLINE_CURVE_WITH_KNOTS((6,1,1,1,1,1,1,1,1,1,1,1,1,1,1,1,1,1,1,1,1,1,
1,1,1,1,1,1,1,1,1,1,1,1,1,1,1,1,1,1,1,1,1,1,1,1,1,1,1,1,1,1,1,1,1,1,1,1,
1,1,1,1,1,1,1,6),(-1.,-0.984615384615383,-0.969230769230768,-0.953846153846152,
-0.938461538461537,-0.923076923076922,-0.907692307692306,-0.892307692307691,
-0.876923076923076,-0.86153846153846,-0.846153846153845,-0.83076923076923,
-0.815384615384614,-0.799999999999999,-0.784615384615384,-0.769230769230768,
-0.753846153846153,-0.738461538461538,-0.723076923076922,-0.707692307692307,
-0.692307692307692,-0.676923076923076,-0.661538461538461,-0.646153846153846,
-0.63076923076923,-0.615384615384615,-0.6,-0.584615384615384,-0.569230769230769,
-0.553846153846154,-0.538461538461538,-0.523076923076923,-0.507692307692308,
-0.492307692307692,-0.476923076923077,-0.461538461538462,-0.446153846153846,
-0.430769230769231,-0.415384615384615,-0.4,-0.384615384615385,-0.369230769230769,
-0.353846153846154,-0.338461538461538,-0.323076923076923,-0.307692307692308,
-0.292307692307692,-0.276923076923077,-0.261538461538462,-0.246153846153846,
-0.230769230769231,-0.215384615384615,-0.2,-0.184615384615385,-0.169230769230769,
-0.153846153846154,-0.138461538461538,-0.123076923076923,-0.107692307692308,
-0.0923076923076923,-0.0769230769230769,-0.0615384615384615,-0.0461538461538462,
-0.0307692307692308,-0.0153846153846154,0.),.UNSPECIFIED.)
CURVE()
GEOMETRIC_REPRESENTATION_ITEM()
RATIONAL_B_SPLINE_CURVE((1.,1.,1.,1.,1.,1.,1.,1.,1.,1.,1.,1.,1.,1.,1.,1.,
1.,1.,1.,1.,1.,1.,1.,1.,1.,1.,1.,1.,1.,1.,1.,1.,1.,1.,1.,1.,1.,1.,1.,1.,
1.,1.,1.,1.,1.,1.,1.,1.,1.,1.,1.,1.,1.,1.,1.,1.,1.,1.,1.,1.,1.,1.,1.,1.,
1.,1.,1.,1.,1.,1.))
REPRESENTATION_ITEM('')
);
#224=(
BOUNDED_CURVE()
B_SPLINE_CURVE(5,(#31595,#31596,#31597,#31598,#31599,#31600,#31601,#31602,
#31603,#31604,#31605,#31606,#31607,#31608,#31609,#31610,#31611,#31612,#31613,
#31614,#31615,#31616,#31617,#31618,#31619,#31620,#31621,#31622,#31623,#31624,
#31625,#31626,#31627,#31628,#31629,#31630,#31631,#31632,#31633,#31634,#31635,
#31636,#31637,#31638,#31639,#31640,#31641,#31642,#31643,#31644,#31645,#31646,
#31647,#31648,#31649,#31650,#31651,#31652,#31653,#31654,#31655,#31656,#31657,
#31658,#31659,#31660,#31661,#31662,#31663,#31664),.UNSPECIFIED.,.F.,.F.)
B_SPLINE_CURVE_WITH_KNOTS((6,1,1,1,1,1,1,1,1,1,1,1,1,1,1,1,1,1,1,1,1,1,
1,1,1,1,1,1,1,1,1,1,1,1,1,1,1,1,1,1,1,1,1,1,1,1,1,1,1,1,1,1,1,1,1,1,1,1,
1,1,1,1,1,1,1,6),(-1.,-0.984615384615383,-0.969230769230768,-0.953846153846152,
-0.938461538461537,-0.923076923076922,-0.907692307692306,-0.892307692307691,
-0.876923076923076,-0.86153846153846,-0.846153846153845,-0.83076923076923,
-0.815384615384614,-0.799999999999999,-0.784615384615384,-0.769230769230768,
-0.753846153846153,-0.738461538461538,-0.723076923076922,-0.707692307692307,
-0.692307692307692,-0.676923076923076,-0.661538461538461,-0.646153846153846,
-0.63076923076923,-0.615384615384615,-0.6,-0.584615384615384,-0.569230769230769,
-0.553846153846154,-0.538461538461538,-0.523076923076923,-0.507692307692308,
-0.492307692307692,-0.476923076923077,-0.461538461538462,-0.446153846153846,
-0.430769230769231,-0.415384615384615,-0.4,-0.384615384615385,-0.369230769230769,
-0.353846153846154,-0.338461538461538,-0.323076923076923,-0.307692307692308,
-0.292307692307692,-0.276923076923077,-0.261538461538462,-0.246153846153846,
-0.230769230769231,-0.215384615384615,-0.2,-0.184615384615385,-0.169230769230769,
-0.153846153846154,-0.138461538461538,-0.123076923076923,-0.107692307692308,
-0.0923076923076923,-0.0769230769230769,-0.0615384615384615,-0.0461538461538462,
-0.0307692307692308,-0.0153846153846154,0.),.UNSPECIFIED.)
CURVE()
GEOMETRIC_REPRESENTATION_ITEM()
RATIONAL_B_SPLINE_CURVE((1.,1.,1.,1.,1.,1.,1.,1.,1.,1.,1.,1.,1.,1.,1.,1.,
1.,1.,1.,1.,1.,1.,1.,1.,1.,1.,1.,1.,1.,1.,1.,1.,1.,1.,1.,1.,1.,1.,1.,1.,
1.,1.,1.,1.,1.,1.,1.,1.,1.,1.,1.,1.,1.,1.,1.,1.,1.,1.,1.,1.,1.,1.,1.,1.,
1.,1.,1.,1.,1.,1.))
REPRESENTATION_ITEM('')
);
#225=(
BOUNDED_CURVE()
B_SPLINE_CURVE(5,(#31811,#31812,#31813,#31814,#31815,#31816,#31817,#31818,
#31819,#31820,#31821,#31822,#31823,#31824,#31825,#31826,#31827,#31828,#31829,
#31830,#31831,#31832,#31833,#31834,#31835,#31836,#31837,#31838,#31839,#31840,
#31841,#31842,#31843,#31844,#31845,#31846,#31847,#31848,#31849,#31850,#31851,
#31852,#31853,#31854,#31855,#31856,#31857,#31858,#31859,#31860,#31861,#31862,
#31863,#31864,#31865,#31866,#31867,#31868,#31869,#31870,#31871,#31872,#31873,
#31874,#31875,#31876,#31877,#31878,#31879,#31880),.UNSPECIFIED.,.F.,.F.)
B_SPLINE_CURVE_WITH_KNOTS((6,1,1,1,1,1,1,1,1,1,1,1,1,1,1,1,1,1,1,1,1,1,
1,1,1,1,1,1,1,1,1,1,1,1,1,1,1,1,1,1,1,1,1,1,1,1,1,1,1,1,1,1,1,1,1,1,1,1,
1,1,1,1,1,1,1,6),(-1.,-0.984615384615383,-0.969230769230768,-0.953846153846152,
-0.938461538461537,-0.923076923076922,-0.907692307692306,-0.892307692307691,
-0.876923076923076,-0.86153846153846,-0.846153846153845,-0.83076923076923,
-0.815384615384614,-0.799999999999999,-0.784615384615384,-0.769230769230768,
-0.753846153846153,-0.738461538461538,-0.723076923076922,-0.707692307692307,
-0.692307692307692,-0.676923076923076,-0.661538461538461,-0.646153846153846,
-0.63076923076923,-0.615384615384615,-0.6,-0.584615384615384,-0.569230769230769,
-0.553846153846154,-0.538461538461538,-0.523076923076923,-0.507692307692308,
-0.492307692307692,-0.476923076923077,-0.461538461538462,-0.446153846153846,
-0.430769230769231,-0.415384615384615,-0.4,-0.384615384615385,-0.369230769230769,
-0.353846153846154,-0.338461538461538,-0.323076923076923,-0.307692307692308,
-0.292307692307692,-0.276923076923077,-0.261538461538462,-0.246153846153846,
-0.230769230769231,-0.215384615384615,-0.2,-0.184615384615385,-0.169230769230769,
-0.153846153846154,-0.138461538461538,-0.123076923076923,-0.107692307692308,
-0.0923076923076923,-0.0769230769230769,-0.0615384615384615,-0.0461538461538462,
-0.0307692307692308,-0.0153846153846154,0.),.UNSPECIFIED.)
CURVE()
GEOMETRIC_REPRESENTATION_ITEM()
RATIONAL_B_SPLINE_CURVE((1.,1.,1.,1.,1.,1.,1.,1.,1.,1.,1.,1.,1.,1.,1.,1.,
1.,1.,1.,1.,1.,1.,1.,1.,1.,1.,1.,1.,1.,1.,1.,1.,1.,1.,1.,1.,1.,1.,1.,1.,
1.,1.,1.,1.,1.,1.,1.,1.,1.,1.,1.,1.,1.,1.,1.,1.,1.,1.,1.,1.,1.,1.,1.,1.,
1.,1.,1.,1.,1.,1.))
REPRESENTATION_ITEM('')
);
#226=(
BOUNDED_CURVE()
B_SPLINE_CURVE(5,(#32027,#32028,#32029,#32030,#32031,#32032,#32033,#32034,
#32035,#32036,#32037,#32038,#32039,#32040,#32041,#32042,#32043,#32044,#32045,
#32046,#32047,#32048,#32049,#32050,#32051,#32052,#32053,#32054,#32055,#32056,
#32057,#32058,#32059,#32060,#32061,#32062,#32063,#32064,#32065,#32066,#32067,
#32068,#32069,#32070,#32071,#32072,#32073,#32074,#32075,#32076,#32077,#32078,
#32079,#32080,#32081,#32082,#32083,#32084,#32085,#32086,#32087,#32088,#32089,
#32090,#32091,#32092,#32093,#32094,#32095,#32096),.UNSPECIFIED.,.F.,.F.)
B_SPLINE_CURVE_WITH_KNOTS((6,1,1,1,1,1,1,1,1,1,1,1,1,1,1,1,1,1,1,1,1,1,
1,1,1,1,1,1,1,1,1,1,1,1,1,1,1,1,1,1,1,1,1,1,1,1,1,1,1,1,1,1,1,1,1,1,1,1,
1,1,1,1,1,1,1,6),(-1.,-0.984615384615383,-0.969230769230768,-0.953846153846152,
-0.938461538461537,-0.923076923076922,-0.907692307692306,-0.892307692307691,
-0.876923076923076,-0.86153846153846,-0.846153846153845,-0.83076923076923,
-0.815384615384614,-0.799999999999999,-0.784615384615384,-0.769230769230768,
-0.753846153846153,-0.738461538461538,-0.723076923076922,-0.707692307692307,
-0.692307692307692,-0.676923076923076,-0.661538461538461,-0.646153846153846,
-0.63076923076923,-0.615384615384615,-0.6,-0.584615384615384,-0.569230769230769,
-0.553846153846154,-0.538461538461538,-0.523076923076923,-0.507692307692308,
-0.492307692307692,-0.476923076923077,-0.461538461538462,-0.446153846153846,
-0.430769230769231,-0.415384615384615,-0.4,-0.384615384615385,-0.369230769230769,
-0.353846153846154,-0.338461538461538,-0.323076923076923,-0.307692307692308,
-0.292307692307692,-0.276923076923077,-0.261538461538462,-0.246153846153846,
-0.230769230769231,-0.215384615384615,-0.2,-0.184615384615385,-0.169230769230769,
-0.153846153846154,-0.138461538461538,-0.123076923076923,-0.107692307692308,
-0.0923076923076923,-0.0769230769230769,-0.0615384615384615,-0.0461538461538462,
-0.0307692307692308,-0.0153846153846154,0.),.UNSPECIFIED.)
CURVE()
GEOMETRIC_REPRESENTATION_ITEM()
RATIONAL_B_SPLINE_CURVE((1.,1.,1.,1.,1.,1.,1.,1.,1.,1.,1.,1.,1.,1.,1.,1.,
1.,1.,1.,1.,1.,1.,1.,1.,1.,1.,1.,1.,1.,1.,1.,1.,1.,1.,1.,1.,1.,1.,1.,1.,
1.,1.,1.,1.,1.,1.,1.,1.,1.,1.,1.,1.,1.,1.,1.,1.,1.,1.,1.,1.,1.,1.,1.,1.,
1.,1.,1.,1.,1.,1.))
REPRESENTATION_ITEM('')
);
#227=(
BOUNDED_CURVE()
B_SPLINE_CURVE(5,(#32243,#32244,#32245,#32246,#32247,#32248,#32249,#32250,
#32251,#32252,#32253,#32254,#32255,#32256,#32257,#32258,#32259,#32260,#32261,
#32262,#32263,#32264,#32265,#32266,#32267,#32268,#32269,#32270,#32271,#32272,
#32273,#32274,#32275,#32276,#32277,#32278,#32279,#32280,#32281,#32282,#32283,
#32284,#32285,#32286,#32287,#32288,#32289,#32290,#32291,#32292,#32293,#32294,
#32295,#32296,#32297,#32298,#32299,#32300,#32301,#32302,#32303,#32304,#32305,
#32306,#32307,#32308,#32309,#32310,#32311,#32312),.UNSPECIFIED.,.F.,.F.)
B_SPLINE_CURVE_WITH_KNOTS((6,1,1,1,1,1,1,1,1,1,1,1,1,1,1,1,1,1,1,1,1,1,
1,1,1,1,1,1,1,1,1,1,1,1,1,1,1,1,1,1,1,1,1,1,1,1,1,1,1,1,1,1,1,1,1,1,1,1,
1,1,1,1,1,1,1,6),(-1.,-0.984615384615383,-0.969230769230768,-0.953846153846152,
-0.938461538461537,-0.923076923076922,-0.907692307692306,-0.892307692307691,
-0.876923076923076,-0.86153846153846,-0.846153846153845,-0.83076923076923,
-0.815384615384614,-0.799999999999999,-0.784615384615384,-0.769230769230768,
-0.753846153846153,-0.738461538461538,-0.723076923076922,-0.707692307692307,
-0.692307692307692,-0.676923076923076,-0.661538461538461,-0.646153846153846,
-0.63076923076923,-0.615384615384615,-0.6,-0.584615384615384,-0.569230769230769,
-0.553846153846154,-0.538461538461538,-0.523076923076923,-0.507692307692308,
-0.492307692307692,-0.476923076923077,-0.461538461538462,-0.446153846153846,
-0.430769230769231,-0.415384615384615,-0.4,-0.384615384615385,-0.369230769230769,
-0.353846153846154,-0.338461538461538,-0.323076923076923,-0.307692307692308,
-0.292307692307692,-0.276923076923077,-0.261538461538462,-0.246153846153846,
-0.230769230769231,-0.215384615384615,-0.2,-0.184615384615385,-0.169230769230769,
-0.153846153846154,-0.138461538461538,-0.123076923076923,-0.107692307692308,
-0.0923076923076923,-0.0769230769230769,-0.0615384615384615,-0.0461538461538462,
-0.0307692307692308,-0.0153846153846154,0.),.UNSPECIFIED.)
CURVE()
GEOMETRIC_REPRESENTATION_ITEM()
RATIONAL_B_SPLINE_CURVE((1.,1.,1.,1.,1.,1.,1.,1.,1.,1.,1.,1.,1.,1.,1.,1.,
1.,1.,1.,1.,1.,1.,1.,1.,1.,1.,1.,1.,1.,1.,1.,1.,1.,1.,1.,1.,1.,1.,1.,1.,
1.,1.,1.,1.,1.,1.,1.,1.,1.,1.,1.,1.,1.,1.,1.,1.,1.,1.,1.,1.,1.,1.,1.,1.,
1.,1.,1.,1.,1.,1.))
REPRESENTATION_ITEM('')
);
#228=(
BOUNDED_CURVE()
B_SPLINE_CURVE(5,(#32459,#32460,#32461,#32462,#32463,#32464,#32465,#32466,
#32467,#32468,#32469,#32470,#32471,#32472,#32473,#32474,#32475,#32476,#32477,
#32478,#32479,#32480,#32481,#32482,#32483,#32484,#32485,#32486,#32487,#32488,
#32489,#32490,#32491,#32492,#32493,#32494,#32495,#32496,#32497,#32498,#32499,
#32500,#32501,#32502,#32503,#32504,#32505,#32506,#32507,#32508,#32509,#32510,
#32511,#32512,#32513,#32514,#32515,#32516,#32517,#32518,#32519,#32520,#32521,
#32522,#32523,#32524,#32525,#32526,#32527,#32528),.UNSPECIFIED.,.F.,.F.)
B_SPLINE_CURVE_WITH_KNOTS((6,1,1,1,1,1,1,1,1,1,1,1,1,1,1,1,1,1,1,1,1,1,
1,1,1,1,1,1,1,1,1,1,1,1,1,1,1,1,1,1,1,1,1,1,1,1,1,1,1,1,1,1,1,1,1,1,1,1,
1,1,1,1,1,1,1,6),(-1.,-0.984615384615383,-0.969230769230768,-0.953846153846152,
-0.938461538461537,-0.923076923076922,-0.907692307692306,-0.892307692307691,
-0.876923076923076,-0.86153846153846,-0.846153846153845,-0.83076923076923,
-0.815384615384614,-0.799999999999999,-0.784615384615384,-0.769230769230768,
-0.753846153846153,-0.738461538461538,-0.723076923076922,-0.707692307692307,
-0.692307692307692,-0.676923076923076,-0.661538461538461,-0.646153846153846,
-0.63076923076923,-0.615384615384615,-0.6,-0.584615384615384,-0.569230769230769,
-0.553846153846154,-0.538461538461538,-0.523076923076923,-0.507692307692308,
-0.492307692307692,-0.476923076923077,-0.461538461538462,-0.446153846153846,
-0.430769230769231,-0.415384615384615,-0.4,-0.384615384615385,-0.369230769230769,
-0.353846153846154,-0.338461538461538,-0.323076923076923,-0.307692307692308,
-0.292307692307692,-0.276923076923077,-0.261538461538462,-0.246153846153846,
-0.230769230769231,-0.215384615384615,-0.2,-0.184615384615385,-0.169230769230769,
-0.153846153846154,-0.138461538461538,-0.123076923076923,-0.107692307692308,
-0.0923076923076923,-0.0769230769230769,-0.0615384615384615,-0.0461538461538462,
-0.0307692307692308,-0.0153846153846154,0.),.UNSPECIFIED.)
CURVE()
GEOMETRIC_REPRESENTATION_ITEM()
RATIONAL_B_SPLINE_CURVE((1.,1.,1.,1.,1.,1.,1.,1.,1.,1.,1.,1.,1.,1.,1.,1.,
1.,1.,1.,1.,1.,1.,1.,1.,1.,1.,1.,1.,1.,1.,1.,1.,1.,1.,1.,1.,1.,1.,1.,1.,
1.,1.,1.,1.,1.,1.,1.,1.,1.,1.,1.,1.,1.,1.,1.,1.,1.,1.,1.,1.,1.,1.,1.,1.,
1.,1.,1.,1.,1.,1.))
REPRESENTATION_ITEM('')
);
#229=(
BOUNDED_CURVE()
B_SPLINE_CURVE(5,(#32675,#32676,#32677,#32678,#32679,#32680,#32681,#32682,
#32683,#32684,#32685,#32686,#32687,#32688,#32689,#32690,#32691,#32692,#32693,
#32694,#32695,#32696,#32697,#32698,#32699,#32700,#32701,#32702,#32703,#32704,
#32705,#32706,#32707,#32708,#32709,#32710,#32711,#32712,#32713,#32714,#32715,
#32716,#32717,#32718,#32719,#32720,#32721,#32722,#32723,#32724,#32725,#32726,
#32727,#32728,#32729,#32730,#32731,#32732,#32733,#32734,#32735,#32736,#32737,
#32738,#32739,#32740,#32741,#32742,#32743,#32744),.UNSPECIFIED.,.F.,.F.)
B_SPLINE_CURVE_WITH_KNOTS((6,1,1,1,1,1,1,1,1,1,1,1,1,1,1,1,1,1,1,1,1,1,
1,1,1,1,1,1,1,1,1,1,1,1,1,1,1,1,1,1,1,1,1,1,1,1,1,1,1,1,1,1,1,1,1,1,1,1,
1,1,1,1,1,1,1,6),(-1.,-0.984615384615383,-0.969230769230768,-0.953846153846152,
-0.938461538461537,-0.923076923076922,-0.907692307692306,-0.892307692307691,
-0.876923076923076,-0.86153846153846,-0.846153846153845,-0.83076923076923,
-0.815384615384614,-0.799999999999999,-0.784615384615384,-0.769230769230768,
-0.753846153846153,-0.738461538461538,-0.723076923076922,-0.707692307692307,
-0.692307692307692,-0.676923076923076,-0.661538461538461,-0.646153846153846,
-0.63076923076923,-0.615384615384615,-0.6,-0.584615384615384,-0.569230769230769,
-0.553846153846154,-0.538461538461538,-0.523076923076923,-0.507692307692308,
-0.492307692307692,-0.476923076923077,-0.461538461538462,-0.446153846153846,
-0.430769230769231,-0.415384615384615,-0.4,-0.384615384615385,-0.369230769230769,
-0.353846153846154,-0.338461538461538,-0.323076923076923,-0.307692307692308,
-0.292307692307692,-0.276923076923077,-0.261538461538462,-0.246153846153846,
-0.230769230769231,-0.215384615384615,-0.2,-0.184615384615385,-0.169230769230769,
-0.153846153846154,-0.138461538461538,-0.123076923076923,-0.107692307692308,
-0.0923076923076923,-0.0769230769230769,-0.0615384615384615,-0.0461538461538462,
-0.0307692307692308,-0.0153846153846154,0.),.UNSPECIFIED.)
CURVE()
GEOMETRIC_REPRESENTATION_ITEM()
RATIONAL_B_SPLINE_CURVE((1.,1.,1.,1.,1.,1.,1.,1.,1.,1.,1.,1.,1.,1.,1.,1.,
1.,1.,1.,1.,1.,1.,1.,1.,1.,1.,1.,1.,1.,1.,1.,1.,1.,1.,1.,1.,1.,1.,1.,1.,
1.,1.,1.,1.,1.,1.,1.,1.,1.,1.,1.,1.,1.,1.,1.,1.,1.,1.,1.,1.,1.,1.,1.,1.,
1.,1.,1.,1.,1.,1.))
REPRESENTATION_ITEM('')
);
#230=(
BOUNDED_CURVE()
B_SPLINE_CURVE(5,(#32891,#32892,#32893,#32894,#32895,#32896,#32897,#32898,
#32899,#32900,#32901,#32902,#32903,#32904,#32905,#32906,#32907,#32908,#32909,
#32910,#32911,#32912,#32913,#32914,#32915,#32916,#32917,#32918,#32919,#32920,
#32921,#32922,#32923,#32924,#32925,#32926,#32927,#32928,#32929,#32930,#32931,
#32932,#32933,#32934,#32935,#32936,#32937,#32938,#32939,#32940,#32941,#32942,
#32943,#32944,#32945,#32946,#32947,#32948,#32949,#32950,#32951,#32952,#32953,
#32954,#32955,#32956,#32957,#32958,#32959,#32960),.UNSPECIFIED.,.F.,.F.)
B_SPLINE_CURVE_WITH_KNOTS((6,1,1,1,1,1,1,1,1,1,1,1,1,1,1,1,1,1,1,1,1,1,
1,1,1,1,1,1,1,1,1,1,1,1,1,1,1,1,1,1,1,1,1,1,1,1,1,1,1,1,1,1,1,1,1,1,1,1,
1,1,1,1,1,1,1,6),(-1.,-0.984615384615383,-0.969230769230768,-0.953846153846152,
-0.938461538461537,-0.923076923076922,-0.907692307692306,-0.892307692307691,
-0.876923076923076,-0.86153846153846,-0.846153846153845,-0.83076923076923,
-0.815384615384614,-0.799999999999999,-0.784615384615384,-0.769230769230768,
-0.753846153846153,-0.738461538461538,-0.723076923076922,-0.707692307692307,
-0.692307692307692,-0.676923076923076,-0.661538461538461,-0.646153846153846,
-0.63076923076923,-0.615384615384615,-0.6,-0.584615384615384,-0.569230769230769,
-0.553846153846154,-0.538461538461538,-0.523076923076923,-0.507692307692308,
-0.492307692307692,-0.476923076923077,-0.461538461538462,-0.446153846153846,
-0.430769230769231,-0.415384615384615,-0.4,-0.384615384615385,-0.369230769230769,
-0.353846153846154,-0.338461538461538,-0.323076923076923,-0.307692307692308,
-0.292307692307692,-0.276923076923077,-0.261538461538462,-0.246153846153846,
-0.230769230769231,-0.215384615384615,-0.2,-0.184615384615385,-0.169230769230769,
-0.153846153846154,-0.138461538461538,-0.123076923076923,-0.107692307692308,
-0.0923076923076923,-0.0769230769230769,-0.0615384615384615,-0.0461538461538462,
-0.0307692307692308,-0.0153846153846154,0.),.UNSPECIFIED.)
CURVE()
GEOMETRIC_REPRESENTATION_ITEM()
RATIONAL_B_SPLINE_CURVE((1.,1.,1.,1.,1.,1.,1.,1.,1.,1.,1.,1.,1.,1.,1.,1.,
1.,1.,1.,1.,1.,1.,1.,1.,1.,1.,1.,1.,1.,1.,1.,1.,1.,1.,1.,1.,1.,1.,1.,1.,
1.,1.,1.,1.,1.,1.,1.,1.,1.,1.,1.,1.,1.,1.,1.,1.,1.,1.,1.,1.,1.,1.,1.,1.,
1.,1.,1.,1.,1.,1.))
REPRESENTATION_ITEM('')
);
#231=(
BOUNDED_CURVE()
B_SPLINE_CURVE(5,(#33107,#33108,#33109,#33110,#33111,#33112,#33113,#33114,
#33115,#33116,#33117,#33118,#33119,#33120,#33121,#33122,#33123,#33124,#33125,
#33126,#33127,#33128,#33129,#33130,#33131,#33132,#33133,#33134,#33135,#33136,
#33137,#33138,#33139,#33140,#33141,#33142,#33143,#33144,#33145,#33146,#33147,
#33148,#33149,#33150,#33151,#33152,#33153,#33154,#33155,#33156,#33157,#33158,
#33159,#33160,#33161,#33162,#33163,#33164,#33165,#33166,#33167,#33168,#33169,
#33170,#33171,#33172,#33173,#33174,#33175,#33176),.UNSPECIFIED.,.F.,.F.)
B_SPLINE_CURVE_WITH_KNOTS((6,1,1,1,1,1,1,1,1,1,1,1,1,1,1,1,1,1,1,1,1,1,
1,1,1,1,1,1,1,1,1,1,1,1,1,1,1,1,1,1,1,1,1,1,1,1,1,1,1,1,1,1,1,1,1,1,1,1,
1,1,1,1,1,1,1,6),(-1.,-0.984615384615383,-0.969230769230768,-0.953846153846152,
-0.938461538461537,-0.923076923076922,-0.907692307692306,-0.892307692307691,
-0.876923076923076,-0.86153846153846,-0.846153846153845,-0.83076923076923,
-0.815384615384614,-0.799999999999999,-0.784615384615384,-0.769230769230768,
-0.753846153846153,-0.738461538461538,-0.723076923076922,-0.707692307692307,
-0.692307692307692,-0.676923076923076,-0.661538461538461,-0.646153846153846,
-0.63076923076923,-0.615384615384615,-0.6,-0.584615384615384,-0.569230769230769,
-0.553846153846154,-0.538461538461538,-0.523076923076923,-0.507692307692308,
-0.492307692307692,-0.476923076923077,-0.461538461538462,-0.446153846153846,
-0.430769230769231,-0.415384615384615,-0.4,-0.384615384615385,-0.369230769230769,
-0.353846153846154,-0.338461538461538,-0.323076923076923,-0.307692307692308,
-0.292307692307692,-0.276923076923077,-0.261538461538462,-0.246153846153846,
-0.230769230769231,-0.215384615384615,-0.2,-0.184615384615385,-0.169230769230769,
-0.153846153846154,-0.138461538461538,-0.123076923076923,-0.107692307692308,
-0.0923076923076923,-0.0769230769230769,-0.0615384615384615,-0.0461538461538462,
-0.0307692307692308,-0.0153846153846154,0.),.UNSPECIFIED.)
CURVE()
GEOMETRIC_REPRESENTATION_ITEM()
RATIONAL_B_SPLINE_CURVE((1.,1.,1.,1.,1.,1.,1.,1.,1.,1.,1.,1.,1.,1.,1.,1.,
1.,1.,1.,1.,1.,1.,1.,1.,1.,1.,1.,1.,1.,1.,1.,1.,1.,1.,1.,1.,1.,1.,1.,1.,
1.,1.,1.,1.,1.,1.,1.,1.,1.,1.,1.,1.,1.,1.,1.,1.,1.,1.,1.,1.,1.,1.,1.,1.,
1.,1.,1.,1.,1.,1.))
REPRESENTATION_ITEM('')
);
#232=(
BOUNDED_CURVE()
B_SPLINE_CURVE(5,(#33323,#33324,#33325,#33326,#33327,#33328,#33329,#33330,
#33331,#33332,#33333,#33334,#33335,#33336,#33337,#33338,#33339,#33340,#33341,
#33342,#33343,#33344,#33345,#33346,#33347,#33348,#33349,#33350,#33351,#33352,
#33353,#33354,#33355,#33356,#33357,#33358,#33359,#33360,#33361,#33362,#33363,
#33364,#33365,#33366,#33367,#33368,#33369,#33370,#33371,#33372,#33373,#33374,
#33375,#33376,#33377,#33378,#33379,#33380,#33381,#33382,#33383,#33384,#33385,
#33386,#33387,#33388,#33389,#33390,#33391,#33392),.UNSPECIFIED.,.F.,.F.)
B_SPLINE_CURVE_WITH_KNOTS((6,1,1,1,1,1,1,1,1,1,1,1,1,1,1,1,1,1,1,1,1,1,
1,1,1,1,1,1,1,1,1,1,1,1,1,1,1,1,1,1,1,1,1,1,1,1,1,1,1,1,1,1,1,1,1,1,1,1,
1,1,1,1,1,1,1,6),(-1.,-0.984615384615383,-0.969230769230768,-0.953846153846152,
-0.938461538461537,-0.923076923076922,-0.907692307692306,-0.892307692307691,
-0.876923076923076,-0.86153846153846,-0.846153846153845,-0.83076923076923,
-0.815384615384614,-0.799999999999999,-0.784615384615384,-0.769230769230768,
-0.753846153846153,-0.738461538461538,-0.723076923076922,-0.707692307692307,
-0.692307692307692,-0.676923076923076,-0.661538461538461,-0.646153846153846,
-0.63076923076923,-0.615384615384615,-0.6,-0.584615384615384,-0.569230769230769,
-0.553846153846154,-0.538461538461538,-0.523076923076923,-0.507692307692308,
-0.492307692307692,-0.476923076923077,-0.461538461538462,-0.446153846153846,
-0.430769230769231,-0.415384615384615,-0.4,-0.384615384615385,-0.369230769230769,
-0.353846153846154,-0.338461538461538,-0.323076923076923,-0.307692307692308,
-0.292307692307692,-0.276923076923077,-0.261538461538462,-0.246153846153846,
-0.230769230769231,-0.215384615384615,-0.2,-0.184615384615385,-0.169230769230769,
-0.153846153846154,-0.138461538461538,-0.123076923076923,-0.107692307692308,
-0.0923076923076923,-0.0769230769230769,-0.0615384615384615,-0.0461538461538462,
-0.0307692307692308,-0.0153846153846154,0.),.UNSPECIFIED.)
CURVE()
GEOMETRIC_REPRESENTATION_ITEM()
RATIONAL_B_SPLINE_CURVE((1.,1.,1.,1.,1.,1.,1.,1.,1.,1.,1.,1.,1.,1.,1.,1.,
1.,1.,1.,1.,1.,1.,1.,1.,1.,1.,1.,1.,1.,1.,1.,1.,1.,1.,1.,1.,1.,1.,1.,1.,
1.,1.,1.,1.,1.,1.,1.,1.,1.,1.,1.,1.,1.,1.,1.,1.,1.,1.,1.,1.,1.,1.,1.,1.,
1.,1.,1.,1.,1.,1.))
REPRESENTATION_ITEM('')
);
#233=(
BOUNDED_CURVE()
B_SPLINE_CURVE(5,(#33539,#33540,#33541,#33542,#33543,#33544,#33545,#33546,
#33547,#33548,#33549,#33550,#33551,#33552,#33553,#33554,#33555,#33556,#33557,
#33558,#33559,#33560,#33561,#33562,#33563,#33564,#33565,#33566,#33567,#33568,
#33569,#33570,#33571,#33572,#33573,#33574,#33575,#33576,#33577,#33578,#33579,
#33580,#33581,#33582,#33583,#33584,#33585,#33586,#33587,#33588,#33589,#33590,
#33591,#33592,#33593,#33594,#33595,#33596,#33597,#33598,#33599,#33600,#33601,
#33602,#33603,#33604,#33605,#33606,#33607,#33608),.UNSPECIFIED.,.F.,.F.)
B_SPLINE_CURVE_WITH_KNOTS((6,1,1,1,1,1,1,1,1,1,1,1,1,1,1,1,1,1,1,1,1,1,
1,1,1,1,1,1,1,1,1,1,1,1,1,1,1,1,1,1,1,1,1,1,1,1,1,1,1,1,1,1,1,1,1,1,1,1,
1,1,1,1,1,1,1,6),(-1.,-0.984615384615383,-0.969230769230768,-0.953846153846152,
-0.938461538461537,-0.923076923076922,-0.907692307692306,-0.892307692307691,
-0.876923076923076,-0.86153846153846,-0.846153846153845,-0.83076923076923,
-0.815384615384614,-0.799999999999999,-0.784615384615384,-0.769230769230768,
-0.753846153846153,-0.738461538461538,-0.723076923076922,-0.707692307692307,
-0.692307692307692,-0.676923076923076,-0.661538461538461,-0.646153846153846,
-0.63076923076923,-0.615384615384615,-0.6,-0.584615384615384,-0.569230769230769,
-0.553846153846154,-0.538461538461538,-0.523076923076923,-0.507692307692308,
-0.492307692307692,-0.476923076923077,-0.461538461538462,-0.446153846153846,
-0.430769230769231,-0.415384615384615,-0.4,-0.384615384615385,-0.369230769230769,
-0.353846153846154,-0.338461538461538,-0.323076923076923,-0.307692307692308,
-0.292307692307692,-0.276923076923077,-0.261538461538462,-0.246153846153846,
-0.230769230769231,-0.215384615384615,-0.2,-0.184615384615385,-0.169230769230769,
-0.153846153846154,-0.138461538461538,-0.123076923076923,-0.107692307692308,
-0.0923076923076923,-0.0769230769230769,-0.0615384615384615,-0.0461538461538462,
-0.0307692307692308,-0.0153846153846154,0.),.UNSPECIFIED.)
CURVE()
GEOMETRIC_REPRESENTATION_ITEM()
RATIONAL_B_SPLINE_CURVE((1.,1.,1.,1.,1.,1.,1.,1.,1.,1.,1.,1.,1.,1.,1.,1.,
1.,1.,1.,1.,1.,1.,1.,1.,1.,1.,1.,1.,1.,1.,1.,1.,1.,1.,1.,1.,1.,1.,1.,1.,
1.,1.,1.,1.,1.,1.,1.,1.,1.,1.,1.,1.,1.,1.,1.,1.,1.,1.,1.,1.,1.,1.,1.,1.,
1.,1.,1.,1.,1.,1.))
REPRESENTATION_ITEM('')
);
#234=(
BOUNDED_CURVE()
B_SPLINE_CURVE(5,(#33755,#33756,#33757,#33758,#33759,#33760,#33761,#33762,
#33763,#33764,#33765,#33766,#33767,#33768,#33769,#33770,#33771,#33772,#33773,
#33774,#33775,#33776,#33777,#33778,#33779,#33780,#33781,#33782,#33783,#33784,
#33785,#33786,#33787,#33788,#33789,#33790,#33791,#33792,#33793,#33794,#33795,
#33796,#33797,#33798,#33799,#33800,#33801,#33802,#33803,#33804,#33805,#33806,
#33807,#33808,#33809,#33810,#33811,#33812,#33813,#33814,#33815,#33816,#33817,
#33818,#33819,#33820,#33821,#33822,#33823,#33824),.UNSPECIFIED.,.F.,.F.)
B_SPLINE_CURVE_WITH_KNOTS((6,1,1,1,1,1,1,1,1,1,1,1,1,1,1,1,1,1,1,1,1,1,
1,1,1,1,1,1,1,1,1,1,1,1,1,1,1,1,1,1,1,1,1,1,1,1,1,1,1,1,1,1,1,1,1,1,1,1,
1,1,1,1,1,1,1,6),(-1.,-0.984615384615383,-0.969230769230768,-0.953846153846152,
-0.938461538461537,-0.923076923076922,-0.907692307692306,-0.892307692307691,
-0.876923076923076,-0.86153846153846,-0.846153846153845,-0.83076923076923,
-0.815384615384614,-0.799999999999999,-0.784615384615384,-0.769230769230768,
-0.753846153846153,-0.738461538461538,-0.723076923076922,-0.707692307692307,
-0.692307692307692,-0.676923076923076,-0.661538461538461,-0.646153846153846,
-0.63076923076923,-0.615384615384615,-0.6,-0.584615384615384,-0.569230769230769,
-0.553846153846154,-0.538461538461538,-0.523076923076923,-0.507692307692308,
-0.492307692307692,-0.476923076923077,-0.461538461538462,-0.446153846153846,
-0.430769230769231,-0.415384615384615,-0.4,-0.384615384615385,-0.369230769230769,
-0.353846153846154,-0.338461538461538,-0.323076923076923,-0.307692307692308,
-0.292307692307692,-0.276923076923077,-0.261538461538462,-0.246153846153846,
-0.230769230769231,-0.215384615384615,-0.2,-0.184615384615385,-0.169230769230769,
-0.153846153846154,-0.138461538461538,-0.123076923076923,-0.107692307692308,
-0.0923076923076923,-0.0769230769230769,-0.0615384615384615,-0.0461538461538462,
-0.0307692307692308,-0.0153846153846154,0.),.UNSPECIFIED.)
CURVE()
GEOMETRIC_REPRESENTATION_ITEM()
RATIONAL_B_SPLINE_CURVE((1.,1.,1.,1.,1.,1.,1.,1.,1.,1.,1.,1.,1.,1.,1.,1.,
1.,1.,1.,1.,1.,1.,1.,1.,1.,1.,1.,1.,1.,1.,1.,1.,1.,1.,1.,1.,1.,1.,1.,1.,
1.,1.,1.,1.,1.,1.,1.,1.,1.,1.,1.,1.,1.,1.,1.,1.,1.,1.,1.,1.,1.,1.,1.,1.,
1.,1.,1.,1.,1.,1.))
REPRESENTATION_ITEM('')
);
#235=(
BOUNDED_CURVE()
B_SPLINE_CURVE(5,(#33971,#33972,#33973,#33974,#33975,#33976,#33977,#33978,
#33979,#33980,#33981,#33982,#33983,#33984,#33985,#33986,#33987,#33988,#33989,
#33990,#33991,#33992,#33993,#33994,#33995,#33996,#33997,#33998,#33999,#34000,
#34001,#34002,#34003,#34004,#34005,#34006,#34007,#34008,#34009,#34010,#34011,
#34012,#34013,#34014,#34015,#34016,#34017,#34018,#34019,#34020,#34021,#34022,
#34023,#34024,#34025,#34026,#34027,#34028,#34029,#34030,#34031,#34032,#34033,
#34034,#34035,#34036,#34037,#34038,#34039,#34040),.UNSPECIFIED.,.F.,.F.)
B_SPLINE_CURVE_WITH_KNOTS((6,1,1,1,1,1,1,1,1,1,1,1,1,1,1,1,1,1,1,1,1,1,
1,1,1,1,1,1,1,1,1,1,1,1,1,1,1,1,1,1,1,1,1,1,1,1,1,1,1,1,1,1,1,1,1,1,1,1,
1,1,1,1,1,1,1,6),(-1.,-0.984615384615383,-0.969230769230768,-0.953846153846152,
-0.938461538461537,-0.923076923076922,-0.907692307692306,-0.892307692307691,
-0.876923076923076,-0.86153846153846,-0.846153846153845,-0.83076923076923,
-0.815384615384614,-0.799999999999999,-0.784615384615384,-0.769230769230768,
-0.753846153846153,-0.738461538461538,-0.723076923076922,-0.707692307692307,
-0.692307692307692,-0.676923076923076,-0.661538461538461,-0.646153846153846,
-0.63076923076923,-0.615384615384615,-0.6,-0.584615384615384,-0.569230769230769,
-0.553846153846154,-0.538461538461538,-0.523076923076923,-0.507692307692308,
-0.492307692307692,-0.476923076923077,-0.461538461538462,-0.446153846153846,
-0.430769230769231,-0.415384615384615,-0.4,-0.384615384615385,-0.369230769230769,
-0.353846153846154,-0.338461538461538,-0.323076923076923,-0.307692307692308,
-0.292307692307692,-0.276923076923077,-0.261538461538462,-0.246153846153846,
-0.230769230769231,-0.215384615384615,-0.2,-0.184615384615385,-0.169230769230769,
-0.153846153846154,-0.138461538461538,-0.123076923076923,-0.107692307692308,
-0.0923076923076923,-0.0769230769230769,-0.0615384615384615,-0.0461538461538462,
-0.0307692307692308,-0.0153846153846154,0.),.UNSPECIFIED.)
CURVE()
GEOMETRIC_REPRESENTATION_ITEM()
RATIONAL_B_SPLINE_CURVE((1.,1.,1.,1.,1.,1.,1.,1.,1.,1.,1.,1.,1.,1.,1.,1.,
1.,1.,1.,1.,1.,1.,1.,1.,1.,1.,1.,1.,1.,1.,1.,1.,1.,1.,1.,1.,1.,1.,1.,1.,
1.,1.,1.,1.,1.,1.,1.,1.,1.,1.,1.,1.,1.,1.,1.,1.,1.,1.,1.,1.,1.,1.,1.,1.,
1.,1.,1.,1.,1.,1.))
REPRESENTATION_ITEM('')
);
#236=(
BOUNDED_CURVE()
B_SPLINE_CURVE(5,(#34187,#34188,#34189,#34190,#34191,#34192,#34193,#34194,
#34195,#34196,#34197,#34198,#34199,#34200,#34201,#34202,#34203,#34204,#34205,
#34206,#34207,#34208,#34209,#34210,#34211,#34212,#34213,#34214,#34215,#34216,
#34217,#34218,#34219,#34220,#34221,#34222,#34223,#34224,#34225,#34226,#34227,
#34228,#34229,#34230,#34231,#34232,#34233,#34234,#34235,#34236,#34237,#34238,
#34239,#34240,#34241,#34242,#34243,#34244,#34245,#34246,#34247,#34248,#34249,
#34250,#34251,#34252,#34253,#34254,#34255,#34256),.UNSPECIFIED.,.F.,.F.)
B_SPLINE_CURVE_WITH_KNOTS((6,1,1,1,1,1,1,1,1,1,1,1,1,1,1,1,1,1,1,1,1,1,
1,1,1,1,1,1,1,1,1,1,1,1,1,1,1,1,1,1,1,1,1,1,1,1,1,1,1,1,1,1,1,1,1,1,1,1,
1,1,1,1,1,1,1,6),(-1.,-0.984615384615383,-0.969230769230768,-0.953846153846152,
-0.938461538461537,-0.923076923076922,-0.907692307692306,-0.892307692307691,
-0.876923076923076,-0.86153846153846,-0.846153846153845,-0.83076923076923,
-0.815384615384614,-0.799999999999999,-0.784615384615384,-0.769230769230768,
-0.753846153846153,-0.738461538461538,-0.723076923076922,-0.707692307692307,
-0.692307692307692,-0.676923076923076,-0.661538461538461,-0.646153846153846,
-0.63076923076923,-0.615384615384615,-0.6,-0.584615384615384,-0.569230769230769,
-0.553846153846154,-0.538461538461538,-0.523076923076923,-0.507692307692308,
-0.492307692307692,-0.476923076923077,-0.461538461538462,-0.446153846153846,
-0.430769230769231,-0.415384615384615,-0.4,-0.384615384615385,-0.369230769230769,
-0.353846153846154,-0.338461538461538,-0.323076923076923,-0.307692307692308,
-0.292307692307692,-0.276923076923077,-0.261538461538462,-0.246153846153846,
-0.230769230769231,-0.215384615384615,-0.2,-0.184615384615385,-0.169230769230769,
-0.153846153846154,-0.138461538461538,-0.123076923076923,-0.107692307692308,
-0.0923076923076923,-0.0769230769230769,-0.0615384615384615,-0.0461538461538462,
-0.0307692307692308,-0.0153846153846154,0.),.UNSPECIFIED.)
CURVE()
GEOMETRIC_REPRESENTATION_ITEM()
RATIONAL_B_SPLINE_CURVE((1.,1.,1.,1.,1.,1.,1.,1.,1.,1.,1.,1.,1.,1.,1.,1.,
1.,1.,1.,1.,1.,1.,1.,1.,1.,1.,1.,1.,1.,1.,1.,1.,1.,1.,1.,1.,1.,1.,1.,1.,
1.,1.,1.,1.,1.,1.,1.,1.,1.,1.,1.,1.,1.,1.,1.,1.,1.,1.,1.,1.,1.,1.,1.,1.,
1.,1.,1.,1.,1.,1.))
REPRESENTATION_ITEM('')
);
#237=(
BOUNDED_CURVE()
B_SPLINE_CURVE(5,(#34403,#34404,#34405,#34406,#34407,#34408,#34409,#34410,
#34411,#34412,#34413,#34414,#34415,#34416,#34417,#34418,#34419,#34420,#34421,
#34422,#34423,#34424,#34425,#34426,#34427,#34428,#34429,#34430,#34431,#34432,
#34433,#34434,#34435,#34436,#34437,#34438,#34439,#34440,#34441,#34442,#34443,
#34444,#34445,#34446,#34447,#34448,#34449,#34450,#34451,#34452,#34453,#34454,
#34455,#34456,#34457,#34458,#34459,#34460,#34461,#34462,#34463,#34464,#34465,
#34466,#34467,#34468,#34469,#34470,#34471,#34472),.UNSPECIFIED.,.F.,.F.)
B_SPLINE_CURVE_WITH_KNOTS((6,1,1,1,1,1,1,1,1,1,1,1,1,1,1,1,1,1,1,1,1,1,
1,1,1,1,1,1,1,1,1,1,1,1,1,1,1,1,1,1,1,1,1,1,1,1,1,1,1,1,1,1,1,1,1,1,1,1,
1,1,1,1,1,1,1,6),(-1.,-0.984615384615383,-0.969230769230768,-0.953846153846152,
-0.938461538461537,-0.923076923076922,-0.907692307692306,-0.892307692307691,
-0.876923076923076,-0.86153846153846,-0.846153846153845,-0.83076923076923,
-0.815384615384614,-0.799999999999999,-0.784615384615384,-0.769230769230768,
-0.753846153846153,-0.738461538461538,-0.723076923076922,-0.707692307692307,
-0.692307692307692,-0.676923076923076,-0.661538461538461,-0.646153846153846,
-0.63076923076923,-0.615384615384615,-0.6,-0.584615384615384,-0.569230769230769,
-0.553846153846154,-0.538461538461538,-0.523076923076923,-0.507692307692308,
-0.492307692307692,-0.476923076923077,-0.461538461538462,-0.446153846153846,
-0.430769230769231,-0.415384615384615,-0.4,-0.384615384615385,-0.369230769230769,
-0.353846153846154,-0.338461538461538,-0.323076923076923,-0.307692307692308,
-0.292307692307692,-0.276923076923077,-0.261538461538462,-0.246153846153846,
-0.230769230769231,-0.215384615384615,-0.2,-0.184615384615385,-0.169230769230769,
-0.153846153846154,-0.138461538461538,-0.123076923076923,-0.107692307692308,
-0.0923076923076923,-0.0769230769230769,-0.0615384615384615,-0.0461538461538462,
-0.0307692307692308,-0.0153846153846154,0.),.UNSPECIFIED.)
CURVE()
GEOMETRIC_REPRESENTATION_ITEM()
RATIONAL_B_SPLINE_CURVE((1.,1.,1.,1.,1.,1.,1.,1.,1.,1.,1.,1.,1.,1.,1.,1.,
1.,1.,1.,1.,1.,1.,1.,1.,1.,1.,1.,1.,1.,1.,1.,1.,1.,1.,1.,1.,1.,1.,1.,1.,
1.,1.,1.,1.,1.,1.,1.,1.,1.,1.,1.,1.,1.,1.,1.,1.,1.,1.,1.,1.,1.,1.,1.,1.,
1.,1.,1.,1.,1.,1.))
REPRESENTATION_ITEM('')
);
#238=(
BOUNDED_CURVE()
B_SPLINE_CURVE(5,(#34619,#34620,#34621,#34622,#34623,#34624,#34625,#34626,
#34627,#34628,#34629,#34630,#34631,#34632,#34633,#34634,#34635,#34636,#34637,
#34638,#34639,#34640,#34641,#34642,#34643,#34644,#34645,#34646,#34647,#34648,
#34649,#34650,#34651,#34652,#34653,#34654,#34655,#34656,#34657,#34658,#34659,
#34660,#34661,#34662,#34663,#34664,#34665,#34666,#34667,#34668,#34669,#34670,
#34671,#34672,#34673,#34674,#34675,#34676,#34677,#34678,#34679,#34680,#34681,
#34682,#34683,#34684,#34685,#34686,#34687,#34688),.UNSPECIFIED.,.F.,.F.)
B_SPLINE_CURVE_WITH_KNOTS((6,1,1,1,1,1,1,1,1,1,1,1,1,1,1,1,1,1,1,1,1,1,
1,1,1,1,1,1,1,1,1,1,1,1,1,1,1,1,1,1,1,1,1,1,1,1,1,1,1,1,1,1,1,1,1,1,1,1,
1,1,1,1,1,1,1,6),(-1.,-0.984615384615383,-0.969230769230768,-0.953846153846152,
-0.938461538461537,-0.923076923076922,-0.907692307692306,-0.892307692307691,
-0.876923076923076,-0.86153846153846,-0.846153846153845,-0.83076923076923,
-0.815384615384614,-0.799999999999999,-0.784615384615384,-0.769230769230768,
-0.753846153846153,-0.738461538461538,-0.723076923076922,-0.707692307692307,
-0.692307692307692,-0.676923076923076,-0.661538461538461,-0.646153846153846,
-0.63076923076923,-0.615384615384615,-0.6,-0.584615384615384,-0.569230769230769,
-0.553846153846154,-0.538461538461538,-0.523076923076923,-0.507692307692308,
-0.492307692307692,-0.476923076923077,-0.461538461538462,-0.446153846153846,
-0.430769230769231,-0.415384615384615,-0.4,-0.384615384615385,-0.369230769230769,
-0.353846153846154,-0.338461538461538,-0.323076923076923,-0.307692307692308,
-0.292307692307692,-0.276923076923077,-0.261538461538462,-0.246153846153846,
-0.230769230769231,-0.215384615384615,-0.2,-0.184615384615385,-0.169230769230769,
-0.153846153846154,-0.138461538461538,-0.123076923076923,-0.107692307692308,
-0.0923076923076923,-0.0769230769230769,-0.0615384615384615,-0.0461538461538462,
-0.0307692307692308,-0.0153846153846154,0.),.UNSPECIFIED.)
CURVE()
GEOMETRIC_REPRESENTATION_ITEM()
RATIONAL_B_SPLINE_CURVE((1.,1.,1.,1.,1.,1.,1.,1.,1.,1.,1.,1.,1.,1.,1.,1.,
1.,1.,1.,1.,1.,1.,1.,1.,1.,1.,1.,1.,1.,1.,1.,1.,1.,1.,1.,1.,1.,1.,1.,1.,
1.,1.,1.,1.,1.,1.,1.,1.,1.,1.,1.,1.,1.,1.,1.,1.,1.,1.,1.,1.,1.,1.,1.,1.,
1.,1.,1.,1.,1.,1.))
REPRESENTATION_ITEM('')
);
#239=(
BOUNDED_CURVE()
B_SPLINE_CURVE(5,(#34835,#34836,#34837,#34838,#34839,#34840,#34841,#34842,
#34843,#34844,#34845,#34846,#34847,#34848,#34849,#34850,#34851,#34852,#34853,
#34854,#34855,#34856,#34857,#34858,#34859,#34860,#34861,#34862,#34863,#34864,
#34865,#34866,#34867,#34868,#34869,#34870,#34871,#34872,#34873,#34874,#34875,
#34876,#34877,#34878,#34879,#34880,#34881,#34882,#34883,#34884,#34885,#34886,
#34887,#34888,#34889,#34890,#34891,#34892,#34893,#34894,#34895,#34896,#34897,
#34898,#34899,#34900,#34901,#34902,#34903,#34904),.UNSPECIFIED.,.F.,.F.)
B_SPLINE_CURVE_WITH_KNOTS((6,1,1,1,1,1,1,1,1,1,1,1,1,1,1,1,1,1,1,1,1,1,
1,1,1,1,1,1,1,1,1,1,1,1,1,1,1,1,1,1,1,1,1,1,1,1,1,1,1,1,1,1,1,1,1,1,1,1,
1,1,1,1,1,1,1,6),(-1.,-0.984615384615383,-0.969230769230768,-0.953846153846152,
-0.938461538461537,-0.923076923076922,-0.907692307692306,-0.892307692307691,
-0.876923076923076,-0.86153846153846,-0.846153846153845,-0.83076923076923,
-0.815384615384614,-0.799999999999999,-0.784615384615384,-0.769230769230768,
-0.753846153846153,-0.738461538461538,-0.723076923076922,-0.707692307692307,
-0.692307692307692,-0.676923076923076,-0.661538461538461,-0.646153846153846,
-0.63076923076923,-0.615384615384615,-0.6,-0.584615384615384,-0.569230769230769,
-0.553846153846154,-0.538461538461538,-0.523076923076923,-0.507692307692308,
-0.492307692307692,-0.476923076923077,-0.461538461538462,-0.446153846153846,
-0.430769230769231,-0.415384615384615,-0.4,-0.384615384615385,-0.369230769230769,
-0.353846153846154,-0.338461538461538,-0.323076923076923,-0.307692307692308,
-0.292307692307692,-0.276923076923077,-0.261538461538462,-0.246153846153846,
-0.230769230769231,-0.215384615384615,-0.2,-0.184615384615385,-0.169230769230769,
-0.153846153846154,-0.138461538461538,-0.123076923076923,-0.107692307692308,
-0.0923076923076923,-0.0769230769230769,-0.0615384615384615,-0.0461538461538462,
-0.0307692307692308,-0.0153846153846154,0.),.UNSPECIFIED.)
CURVE()
GEOMETRIC_REPRESENTATION_ITEM()
RATIONAL_B_SPLINE_CURVE((1.,1.,1.,1.,1.,1.,1.,1.,1.,1.,1.,1.,1.,1.,1.,1.,
1.,1.,1.,1.,1.,1.,1.,1.,1.,1.,1.,1.,1.,1.,1.,1.,1.,1.,1.,1.,1.,1.,1.,1.,
1.,1.,1.,1.,1.,1.,1.,1.,1.,1.,1.,1.,1.,1.,1.,1.,1.,1.,1.,1.,1.,1.,1.,1.,
1.,1.,1.,1.,1.,1.))
REPRESENTATION_ITEM('')
);
#240=(
BOUNDED_CURVE()
B_SPLINE_CURVE(5,(#35051,#35052,#35053,#35054,#35055,#35056,#35057,#35058,
#35059,#35060,#35061,#35062,#35063,#35064,#35065,#35066,#35067,#35068,#35069,
#35070,#35071,#35072,#35073,#35074,#35075,#35076,#35077,#35078,#35079,#35080,
#35081,#35082,#35083,#35084,#35085,#35086,#35087,#35088,#35089,#35090,#35091,
#35092,#35093,#35094,#35095,#35096,#35097,#35098,#35099,#35100,#35101,#35102,
#35103,#35104,#35105,#35106,#35107,#35108,#35109,#35110,#35111,#35112,#35113,
#35114,#35115,#35116,#35117,#35118,#35119,#35120),.UNSPECIFIED.,.F.,.F.)
B_SPLINE_CURVE_WITH_KNOTS((6,1,1,1,1,1,1,1,1,1,1,1,1,1,1,1,1,1,1,1,1,1,
1,1,1,1,1,1,1,1,1,1,1,1,1,1,1,1,1,1,1,1,1,1,1,1,1,1,1,1,1,1,1,1,1,1,1,1,
1,1,1,1,1,1,1,6),(-1.,-0.984615384615383,-0.969230769230768,-0.953846153846152,
-0.938461538461537,-0.923076923076922,-0.907692307692306,-0.892307692307691,
-0.876923076923076,-0.86153846153846,-0.846153846153845,-0.83076923076923,
-0.815384615384614,-0.799999999999999,-0.784615384615384,-0.769230769230768,
-0.753846153846153,-0.738461538461538,-0.723076923076922,-0.707692307692307,
-0.692307692307692,-0.676923076923076,-0.661538461538461,-0.646153846153846,
-0.63076923076923,-0.615384615384615,-0.6,-0.584615384615384,-0.569230769230769,
-0.553846153846154,-0.538461538461538,-0.523076923076923,-0.507692307692308,
-0.492307692307692,-0.476923076923077,-0.461538461538462,-0.446153846153846,
-0.430769230769231,-0.415384615384615,-0.4,-0.384615384615385,-0.369230769230769,
-0.353846153846154,-0.338461538461538,-0.323076923076923,-0.307692307692308,
-0.292307692307692,-0.276923076923077,-0.261538461538462,-0.246153846153846,
-0.230769230769231,-0.215384615384615,-0.2,-0.184615384615385,-0.169230769230769,
-0.153846153846154,-0.138461538461538,-0.123076923076923,-0.107692307692308,
-0.0923076923076923,-0.0769230769230769,-0.0615384615384615,-0.0461538461538462,
-0.0307692307692308,-0.0153846153846154,0.),.UNSPECIFIED.)
CURVE()
GEOMETRIC_REPRESENTATION_ITEM()
RATIONAL_B_SPLINE_CURVE((1.,1.,1.,1.,1.,1.,1.,1.,1.,1.,1.,1.,1.,1.,1.,1.,
1.,1.,1.,1.,1.,1.,1.,1.,1.,1.,1.,1.,1.,1.,1.,1.,1.,1.,1.,1.,1.,1.,1.,1.,
1.,1.,1.,1.,1.,1.,1.,1.,1.,1.,1.,1.,1.,1.,1.,1.,1.,1.,1.,1.,1.,1.,1.,1.,
1.,1.,1.,1.,1.,1.))
REPRESENTATION_ITEM('')
);
#241=(
BOUNDED_CURVE()
B_SPLINE_CURVE(5,(#35267,#35268,#35269,#35270,#35271,#35272,#35273,#35274,
#35275,#35276,#35277,#35278,#35279,#35280,#35281,#35282,#35283,#35284,#35285,
#35286,#35287,#35288,#35289,#35290,#35291,#35292,#35293,#35294,#35295,#35296,
#35297,#35298,#35299,#35300,#35301,#35302,#35303,#35304,#35305,#35306,#35307,
#35308,#35309,#35310,#35311,#35312,#35313,#35314,#35315,#35316,#35317,#35318,
#35319,#35320,#35321,#35322,#35323,#35324,#35325,#35326,#35327,#35328,#35329,
#35330,#35331,#35332,#35333,#35334,#35335,#35336),.UNSPECIFIED.,.F.,.F.)
B_SPLINE_CURVE_WITH_KNOTS((6,1,1,1,1,1,1,1,1,1,1,1,1,1,1,1,1,1,1,1,1,1,
1,1,1,1,1,1,1,1,1,1,1,1,1,1,1,1,1,1,1,1,1,1,1,1,1,1,1,1,1,1,1,1,1,1,1,1,
1,1,1,1,1,1,1,6),(-1.,-0.984615384615383,-0.969230769230768,-0.953846153846152,
-0.938461538461537,-0.923076923076922,-0.907692307692306,-0.892307692307691,
-0.876923076923076,-0.86153846153846,-0.846153846153845,-0.83076923076923,
-0.815384615384614,-0.799999999999999,-0.784615384615384,-0.769230769230768,
-0.753846153846153,-0.738461538461538,-0.723076923076922,-0.707692307692307,
-0.692307692307692,-0.676923076923076,-0.661538461538461,-0.646153846153846,
-0.63076923076923,-0.615384615384615,-0.6,-0.584615384615384,-0.569230769230769,
-0.553846153846154,-0.538461538461538,-0.523076923076923,-0.507692307692308,
-0.492307692307692,-0.476923076923077,-0.461538461538462,-0.446153846153846,
-0.430769230769231,-0.415384615384615,-0.4,-0.384615384615385,-0.369230769230769,
-0.353846153846154,-0.338461538461538,-0.323076923076923,-0.307692307692308,
-0.292307692307692,-0.276923076923077,-0.261538461538462,-0.246153846153846,
-0.230769230769231,-0.215384615384615,-0.2,-0.184615384615385,-0.169230769230769,
-0.153846153846154,-0.138461538461538,-0.123076923076923,-0.107692307692308,
-0.0923076923076923,-0.0769230769230769,-0.0615384615384615,-0.0461538461538462,
-0.0307692307692308,-0.0153846153846154,0.),.UNSPECIFIED.)
CURVE()
GEOMETRIC_REPRESENTATION_ITEM()
RATIONAL_B_SPLINE_CURVE((1.,1.,1.,1.,1.,1.,1.,1.,1.,1.,1.,1.,1.,1.,1.,1.,
1.,1.,1.,1.,1.,1.,1.,1.,1.,1.,1.,1.,1.,1.,1.,1.,1.,1.,1.,1.,1.,1.,1.,1.,
1.,1.,1.,1.,1.,1.,1.,1.,1.,1.,1.,1.,1.,1.,1.,1.,1.,1.,1.,1.,1.,1.,1.,1.,
1.,1.,1.,1.,1.,1.))
REPRESENTATION_ITEM('')
);
#242=(
BOUNDED_CURVE()
B_SPLINE_CURVE(5,(#35483,#35484,#35485,#35486,#35487,#35488,#35489,#35490,
#35491,#35492,#35493,#35494,#35495,#35496,#35497,#35498,#35499,#35500,#35501,
#35502,#35503,#35504,#35505,#35506,#35507,#35508,#35509,#35510,#35511,#35512,
#35513,#35514,#35515,#35516,#35517,#35518,#35519,#35520,#35521,#35522,#35523,
#35524,#35525,#35526,#35527,#35528,#35529,#35530,#35531,#35532,#35533,#35534,
#35535,#35536,#35537,#35538,#35539,#35540,#35541,#35542,#35543,#35544,#35545,
#35546,#35547,#35548,#35549,#35550,#35551,#35552),.UNSPECIFIED.,.F.,.F.)
B_SPLINE_CURVE_WITH_KNOTS((6,1,1,1,1,1,1,1,1,1,1,1,1,1,1,1,1,1,1,1,1,1,
1,1,1,1,1,1,1,1,1,1,1,1,1,1,1,1,1,1,1,1,1,1,1,1,1,1,1,1,1,1,1,1,1,1,1,1,
1,1,1,1,1,1,1,6),(-1.,-0.984615384615383,-0.969230769230768,-0.953846153846152,
-0.938461538461537,-0.923076923076922,-0.907692307692306,-0.892307692307691,
-0.876923076923076,-0.86153846153846,-0.846153846153845,-0.83076923076923,
-0.815384615384614,-0.799999999999999,-0.784615384615384,-0.769230769230768,
-0.753846153846153,-0.738461538461538,-0.723076923076922,-0.707692307692307,
-0.692307692307692,-0.676923076923076,-0.661538461538461,-0.646153846153846,
-0.63076923076923,-0.615384615384615,-0.6,-0.584615384615384,-0.569230769230769,
-0.553846153846154,-0.538461538461538,-0.523076923076923,-0.507692307692308,
-0.492307692307692,-0.476923076923077,-0.461538461538462,-0.446153846153846,
-0.430769230769231,-0.415384615384615,-0.4,-0.384615384615385,-0.369230769230769,
-0.353846153846154,-0.338461538461538,-0.323076923076923,-0.307692307692308,
-0.292307692307692,-0.276923076923077,-0.261538461538462,-0.246153846153846,
-0.230769230769231,-0.215384615384615,-0.2,-0.184615384615385,-0.169230769230769,
-0.153846153846154,-0.138461538461538,-0.123076923076923,-0.107692307692308,
-0.0923076923076923,-0.0769230769230769,-0.0615384615384615,-0.0461538461538462,
-0.0307692307692308,-0.0153846153846154,0.),.UNSPECIFIED.)
CURVE()
GEOMETRIC_REPRESENTATION_ITEM()
RATIONAL_B_SPLINE_CURVE((1.,1.,1.,1.,1.,1.,1.,1.,1.,1.,1.,1.,1.,1.,1.,1.,
1.,1.,1.,1.,1.,1.,1.,1.,1.,1.,1.,1.,1.,1.,1.,1.,1.,1.,1.,1.,1.,1.,1.,1.,
1.,1.,1.,1.,1.,1.,1.,1.,1.,1.,1.,1.,1.,1.,1.,1.,1.,1.,1.,1.,1.,1.,1.,1.,
1.,1.,1.,1.,1.,1.))
REPRESENTATION_ITEM('')
);
#243=(
BOUNDED_CURVE()
B_SPLINE_CURVE(5,(#35699,#35700,#35701,#35702,#35703,#35704,#35705,#35706,
#35707,#35708,#35709,#35710,#35711,#35712,#35713,#35714,#35715,#35716,#35717,
#35718,#35719,#35720,#35721,#35722,#35723,#35724,#35725,#35726,#35727,#35728,
#35729,#35730,#35731,#35732,#35733,#35734,#35735,#35736,#35737,#35738,#35739,
#35740,#35741,#35742,#35743,#35744,#35745,#35746,#35747,#35748,#35749,#35750,
#35751,#35752,#35753,#35754,#35755,#35756,#35757,#35758,#35759,#35760,#35761,
#35762,#35763,#35764,#35765,#35766,#35767,#35768),.UNSPECIFIED.,.F.,.F.)
B_SPLINE_CURVE_WITH_KNOTS((6,1,1,1,1,1,1,1,1,1,1,1,1,1,1,1,1,1,1,1,1,1,
1,1,1,1,1,1,1,1,1,1,1,1,1,1,1,1,1,1,1,1,1,1,1,1,1,1,1,1,1,1,1,1,1,1,1,1,
1,1,1,1,1,1,1,6),(-1.,-0.984615384615383,-0.969230769230768,-0.953846153846152,
-0.938461538461537,-0.923076923076922,-0.907692307692306,-0.892307692307691,
-0.876923076923076,-0.86153846153846,-0.846153846153845,-0.83076923076923,
-0.815384615384614,-0.799999999999999,-0.784615384615384,-0.769230769230768,
-0.753846153846153,-0.738461538461538,-0.723076923076922,-0.707692307692307,
-0.692307692307692,-0.676923076923076,-0.661538461538461,-0.646153846153846,
-0.63076923076923,-0.615384615384615,-0.6,-0.584615384615384,-0.569230769230769,
-0.553846153846154,-0.538461538461538,-0.523076923076923,-0.507692307692308,
-0.492307692307692,-0.476923076923077,-0.461538461538462,-0.446153846153846,
-0.430769230769231,-0.415384615384615,-0.4,-0.384615384615385,-0.369230769230769,
-0.353846153846154,-0.338461538461538,-0.323076923076923,-0.307692307692308,
-0.292307692307692,-0.276923076923077,-0.261538461538462,-0.246153846153846,
-0.230769230769231,-0.215384615384615,-0.2,-0.184615384615385,-0.169230769230769,
-0.153846153846154,-0.138461538461538,-0.123076923076923,-0.107692307692308,
-0.0923076923076923,-0.0769230769230769,-0.0615384615384615,-0.0461538461538462,
-0.0307692307692308,-0.0153846153846154,0.),.UNSPECIFIED.)
CURVE()
GEOMETRIC_REPRESENTATION_ITEM()
RATIONAL_B_SPLINE_CURVE((1.,1.,1.,1.,1.,1.,1.,1.,1.,1.,1.,1.,1.,1.,1.,1.,
1.,1.,1.,1.,1.,1.,1.,1.,1.,1.,1.,1.,1.,1.,1.,1.,1.,1.,1.,1.,1.,1.,1.,1.,
1.,1.,1.,1.,1.,1.,1.,1.,1.,1.,1.,1.,1.,1.,1.,1.,1.,1.,1.,1.,1.,1.,1.,1.,
1.,1.,1.,1.,1.,1.))
REPRESENTATION_ITEM('')
);
#244=(
BOUNDED_CURVE()
B_SPLINE_CURVE(5,(#35915,#35916,#35917,#35918,#35919,#35920,#35921,#35922,
#35923,#35924,#35925,#35926,#35927,#35928,#35929,#35930,#35931,#35932,#35933,
#35934,#35935,#35936,#35937,#35938,#35939,#35940,#35941,#35942,#35943,#35944,
#35945,#35946,#35947,#35948,#35949,#35950,#35951,#35952,#35953,#35954,#35955,
#35956,#35957,#35958,#35959,#35960,#35961,#35962,#35963,#35964,#35965,#35966,
#35967,#35968,#35969,#35970,#35971,#35972,#35973,#35974,#35975,#35976,#35977,
#35978,#35979,#35980,#35981,#35982,#35983,#35984),.UNSPECIFIED.,.F.,.F.)
B_SPLINE_CURVE_WITH_KNOTS((6,1,1,1,1,1,1,1,1,1,1,1,1,1,1,1,1,1,1,1,1,1,
1,1,1,1,1,1,1,1,1,1,1,1,1,1,1,1,1,1,1,1,1,1,1,1,1,1,1,1,1,1,1,1,1,1,1,1,
1,1,1,1,1,1,1,6),(-1.,-0.984615384615383,-0.969230769230768,-0.953846153846152,
-0.938461538461537,-0.923076923076922,-0.907692307692306,-0.892307692307691,
-0.876923076923076,-0.86153846153846,-0.846153846153845,-0.83076923076923,
-0.815384615384614,-0.799999999999999,-0.784615384615384,-0.769230769230768,
-0.753846153846153,-0.738461538461538,-0.723076923076922,-0.707692307692307,
-0.692307692307692,-0.676923076923076,-0.661538461538461,-0.646153846153846,
-0.63076923076923,-0.615384615384615,-0.6,-0.584615384615384,-0.569230769230769,
-0.553846153846154,-0.538461538461538,-0.523076923076923,-0.507692307692308,
-0.492307692307692,-0.476923076923077,-0.461538461538462,-0.446153846153846,
-0.430769230769231,-0.415384615384615,-0.4,-0.384615384615385,-0.369230769230769,
-0.353846153846154,-0.338461538461538,-0.323076923076923,-0.307692307692308,
-0.292307692307692,-0.276923076923077,-0.261538461538462,-0.246153846153846,
-0.230769230769231,-0.215384615384615,-0.2,-0.184615384615385,-0.169230769230769,
-0.153846153846154,-0.138461538461538,-0.123076923076923,-0.107692307692308,
-0.0923076923076923,-0.0769230769230769,-0.0615384615384615,-0.0461538461538462,
-0.0307692307692308,-0.0153846153846154,0.),.UNSPECIFIED.)
CURVE()
GEOMETRIC_REPRESENTATION_ITEM()
RATIONAL_B_SPLINE_CURVE((1.,1.,1.,1.,1.,1.,1.,1.,1.,1.,1.,1.,1.,1.,1.,1.,
1.,1.,1.,1.,1.,1.,1.,1.,1.,1.,1.,1.,1.,1.,1.,1.,1.,1.,1.,1.,1.,1.,1.,1.,
1.,1.,1.,1.,1.,1.,1.,1.,1.,1.,1.,1.,1.,1.,1.,1.,1.,1.,1.,1.,1.,1.,1.,1.,
1.,1.,1.,1.,1.,1.))
REPRESENTATION_ITEM('')
);
#245=(
BOUNDED_CURVE()
B_SPLINE_CURVE(5,(#36131,#36132,#36133,#36134,#36135,#36136,#36137,#36138,
#36139,#36140,#36141,#36142,#36143,#36144,#36145,#36146,#36147,#36148,#36149,
#36150,#36151,#36152,#36153,#36154,#36155,#36156,#36157,#36158,#36159,#36160,
#36161,#36162,#36163,#36164,#36165,#36166,#36167,#36168,#36169,#36170,#36171,
#36172,#36173,#36174,#36175,#36176,#36177,#36178,#36179,#36180,#36181,#36182,
#36183,#36184,#36185,#36186,#36187,#36188,#36189,#36190,#36191,#36192,#36193,
#36194,#36195,#36196,#36197,#36198,#36199,#36200),.UNSPECIFIED.,.F.,.F.)
B_SPLINE_CURVE_WITH_KNOTS((6,1,1,1,1,1,1,1,1,1,1,1,1,1,1,1,1,1,1,1,1,1,
1,1,1,1,1,1,1,1,1,1,1,1,1,1,1,1,1,1,1,1,1,1,1,1,1,1,1,1,1,1,1,1,1,1,1,1,
1,1,1,1,1,1,1,6),(-1.,-0.984615384615383,-0.969230769230768,-0.953846153846152,
-0.938461538461537,-0.923076923076922,-0.907692307692306,-0.892307692307691,
-0.876923076923076,-0.86153846153846,-0.846153846153845,-0.83076923076923,
-0.815384615384614,-0.799999999999999,-0.784615384615384,-0.769230769230768,
-0.753846153846153,-0.738461538461538,-0.723076923076922,-0.707692307692307,
-0.692307692307692,-0.676923076923076,-0.661538461538461,-0.646153846153846,
-0.63076923076923,-0.615384615384615,-0.6,-0.584615384615384,-0.569230769230769,
-0.553846153846154,-0.538461538461538,-0.523076923076923,-0.507692307692308,
-0.492307692307692,-0.476923076923077,-0.461538461538462,-0.446153846153846,
-0.430769230769231,-0.415384615384615,-0.4,-0.384615384615385,-0.369230769230769,
-0.353846153846154,-0.338461538461538,-0.323076923076923,-0.307692307692308,
-0.292307692307692,-0.276923076923077,-0.261538461538462,-0.246153846153846,
-0.230769230769231,-0.215384615384615,-0.2,-0.184615384615385,-0.169230769230769,
-0.153846153846154,-0.138461538461538,-0.123076923076923,-0.107692307692308,
-0.0923076923076923,-0.0769230769230769,-0.0615384615384615,-0.0461538461538462,
-0.0307692307692308,-0.0153846153846154,0.),.UNSPECIFIED.)
CURVE()
GEOMETRIC_REPRESENTATION_ITEM()
RATIONAL_B_SPLINE_CURVE((1.,1.,1.,1.,1.,1.,1.,1.,1.,1.,1.,1.,1.,1.,1.,1.,
1.,1.,1.,1.,1.,1.,1.,1.,1.,1.,1.,1.,1.,1.,1.,1.,1.,1.,1.,1.,1.,1.,1.,1.,
1.,1.,1.,1.,1.,1.,1.,1.,1.,1.,1.,1.,1.,1.,1.,1.,1.,1.,1.,1.,1.,1.,1.,1.,
1.,1.,1.,1.,1.,1.))
REPRESENTATION_ITEM('')
);
#246=(
BOUNDED_CURVE()
B_SPLINE_CURVE(5,(#36347,#36348,#36349,#36350,#36351,#36352,#36353,#36354,
#36355,#36356,#36357,#36358,#36359,#36360,#36361,#36362,#36363,#36364,#36365,
#36366,#36367,#36368,#36369,#36370,#36371,#36372,#36373,#36374,#36375,#36376,
#36377,#36378,#36379,#36380,#36381,#36382,#36383,#36384,#36385,#36386,#36387,
#36388,#36389,#36390,#36391,#36392,#36393,#36394,#36395,#36396,#36397,#36398,
#36399,#36400,#36401,#36402,#36403,#36404,#36405,#36406,#36407,#36408,#36409,
#36410,#36411,#36412,#36413,#36414,#36415,#36416),.UNSPECIFIED.,.F.,.F.)
B_SPLINE_CURVE_WITH_KNOTS((6,1,1,1,1,1,1,1,1,1,1,1,1,1,1,1,1,1,1,1,1,1,
1,1,1,1,1,1,1,1,1,1,1,1,1,1,1,1,1,1,1,1,1,1,1,1,1,1,1,1,1,1,1,1,1,1,1,1,
1,1,1,1,1,1,1,6),(-1.,-0.984615384615383,-0.969230769230768,-0.953846153846152,
-0.938461538461537,-0.923076923076922,-0.907692307692306,-0.892307692307691,
-0.876923076923076,-0.86153846153846,-0.846153846153845,-0.83076923076923,
-0.815384615384614,-0.799999999999999,-0.784615384615384,-0.769230769230768,
-0.753846153846153,-0.738461538461538,-0.723076923076922,-0.707692307692307,
-0.692307692307692,-0.676923076923076,-0.661538461538461,-0.646153846153846,
-0.63076923076923,-0.615384615384615,-0.6,-0.584615384615384,-0.569230769230769,
-0.553846153846154,-0.538461538461538,-0.523076923076923,-0.507692307692308,
-0.492307692307692,-0.476923076923077,-0.461538461538462,-0.446153846153846,
-0.430769230769231,-0.415384615384615,-0.4,-0.384615384615385,-0.369230769230769,
-0.353846153846154,-0.338461538461538,-0.323076923076923,-0.307692307692308,
-0.292307692307692,-0.276923076923077,-0.261538461538462,-0.246153846153846,
-0.230769230769231,-0.215384615384615,-0.2,-0.184615384615385,-0.169230769230769,
-0.153846153846154,-0.138461538461538,-0.123076923076923,-0.107692307692308,
-0.0923076923076923,-0.0769230769230769,-0.0615384615384615,-0.0461538461538462,
-0.0307692307692308,-0.0153846153846154,0.),.UNSPECIFIED.)
CURVE()
GEOMETRIC_REPRESENTATION_ITEM()
RATIONAL_B_SPLINE_CURVE((1.,1.,1.,1.,1.,1.,1.,1.,1.,1.,1.,1.,1.,1.,1.,1.,
1.,1.,1.,1.,1.,1.,1.,1.,1.,1.,1.,1.,1.,1.,1.,1.,1.,1.,1.,1.,1.,1.,1.,1.,
1.,1.,1.,1.,1.,1.,1.,1.,1.,1.,1.,1.,1.,1.,1.,1.,1.,1.,1.,1.,1.,1.,1.,1.,
1.,1.,1.,1.,1.,1.))
REPRESENTATION_ITEM('')
);
#247=(
BOUNDED_CURVE()
B_SPLINE_CURVE(5,(#36563,#36564,#36565,#36566,#36567,#36568,#36569,#36570,
#36571,#36572,#36573,#36574,#36575,#36576,#36577,#36578,#36579,#36580,#36581,
#36582,#36583,#36584,#36585,#36586,#36587,#36588,#36589,#36590,#36591,#36592,
#36593,#36594,#36595,#36596,#36597,#36598,#36599,#36600,#36601,#36602,#36603,
#36604,#36605,#36606,#36607,#36608,#36609,#36610,#36611,#36612,#36613,#36614,
#36615,#36616,#36617,#36618,#36619,#36620,#36621,#36622,#36623,#36624,#36625,
#36626,#36627,#36628,#36629,#36630,#36631,#36632),.UNSPECIFIED.,.F.,.F.)
B_SPLINE_CURVE_WITH_KNOTS((6,1,1,1,1,1,1,1,1,1,1,1,1,1,1,1,1,1,1,1,1,1,
1,1,1,1,1,1,1,1,1,1,1,1,1,1,1,1,1,1,1,1,1,1,1,1,1,1,1,1,1,1,1,1,1,1,1,1,
1,1,1,1,1,1,1,6),(-1.,-0.984615384615383,-0.969230769230768,-0.953846153846152,
-0.938461538461537,-0.923076923076922,-0.907692307692306,-0.892307692307691,
-0.876923076923076,-0.86153846153846,-0.846153846153845,-0.83076923076923,
-0.815384615384614,-0.799999999999999,-0.784615384615384,-0.769230769230768,
-0.753846153846153,-0.738461538461538,-0.723076923076922,-0.707692307692307,
-0.692307692307692,-0.676923076923076,-0.661538461538461,-0.646153846153846,
-0.63076923076923,-0.615384615384615,-0.6,-0.584615384615384,-0.569230769230769,
-0.553846153846154,-0.538461538461538,-0.523076923076923,-0.507692307692308,
-0.492307692307692,-0.476923076923077,-0.461538461538462,-0.446153846153846,
-0.430769230769231,-0.415384615384615,-0.4,-0.384615384615385,-0.369230769230769,
-0.353846153846154,-0.338461538461538,-0.323076923076923,-0.307692307692308,
-0.292307692307692,-0.276923076923077,-0.261538461538462,-0.246153846153846,
-0.230769230769231,-0.215384615384615,-0.2,-0.184615384615385,-0.169230769230769,
-0.153846153846154,-0.138461538461538,-0.123076923076923,-0.107692307692308,
-0.0923076923076923,-0.0769230769230769,-0.0615384615384615,-0.0461538461538462,
-0.0307692307692308,-0.0153846153846154,0.),.UNSPECIFIED.)
CURVE()
GEOMETRIC_REPRESENTATION_ITEM()
RATIONAL_B_SPLINE_CURVE((1.,1.,1.,1.,1.,1.,1.,1.,1.,1.,1.,1.,1.,1.,1.,1.,
1.,1.,1.,1.,1.,1.,1.,1.,1.,1.,1.,1.,1.,1.,1.,1.,1.,1.,1.,1.,1.,1.,1.,1.,
1.,1.,1.,1.,1.,1.,1.,1.,1.,1.,1.,1.,1.,1.,1.,1.,1.,1.,1.,1.,1.,1.,1.,1.,
1.,1.,1.,1.,1.,1.))
REPRESENTATION_ITEM('')
);
#248=(
BOUNDED_CURVE()
B_SPLINE_CURVE(5,(#36779,#36780,#36781,#36782,#36783,#36784,#36785,#36786,
#36787,#36788,#36789,#36790,#36791,#36792,#36793,#36794,#36795,#36796,#36797,
#36798,#36799,#36800,#36801,#36802,#36803,#36804,#36805,#36806,#36807,#36808,
#36809,#36810,#36811,#36812,#36813,#36814,#36815,#36816,#36817,#36818,#36819,
#36820,#36821,#36822,#36823,#36824,#36825,#36826,#36827,#36828,#36829,#36830,
#36831,#36832,#36833,#36834,#36835,#36836,#36837,#36838,#36839,#36840,#36841,
#36842,#36843,#36844,#36845,#36846,#36847,#36848),.UNSPECIFIED.,.F.,.F.)
B_SPLINE_CURVE_WITH_KNOTS((6,1,1,1,1,1,1,1,1,1,1,1,1,1,1,1,1,1,1,1,1,1,
1,1,1,1,1,1,1,1,1,1,1,1,1,1,1,1,1,1,1,1,1,1,1,1,1,1,1,1,1,1,1,1,1,1,1,1,
1,1,1,1,1,1,1,6),(-1.,-0.984615384615383,-0.969230769230768,-0.953846153846152,
-0.938461538461537,-0.923076923076922,-0.907692307692306,-0.892307692307691,
-0.876923076923076,-0.86153846153846,-0.846153846153845,-0.83076923076923,
-0.815384615384614,-0.799999999999999,-0.784615384615384,-0.769230769230768,
-0.753846153846153,-0.738461538461538,-0.723076923076922,-0.707692307692307,
-0.692307692307692,-0.676923076923076,-0.661538461538461,-0.646153846153846,
-0.63076923076923,-0.615384615384615,-0.6,-0.584615384615384,-0.569230769230769,
-0.553846153846154,-0.538461538461538,-0.523076923076923,-0.507692307692308,
-0.492307692307692,-0.476923076923077,-0.461538461538462,-0.446153846153846,
-0.430769230769231,-0.415384615384615,-0.4,-0.384615384615385,-0.369230769230769,
-0.353846153846154,-0.338461538461538,-0.323076923076923,-0.307692307692308,
-0.292307692307692,-0.276923076923077,-0.261538461538462,-0.246153846153846,
-0.230769230769231,-0.215384615384615,-0.2,-0.184615384615385,-0.169230769230769,
-0.153846153846154,-0.138461538461538,-0.123076923076923,-0.107692307692308,
-0.0923076923076923,-0.0769230769230769,-0.0615384615384615,-0.0461538461538462,
-0.0307692307692308,-0.0153846153846154,0.),.UNSPECIFIED.)
CURVE()
GEOMETRIC_REPRESENTATION_ITEM()
RATIONAL_B_SPLINE_CURVE((1.,1.,1.,1.,1.,1.,1.,1.,1.,1.,1.,1.,1.,1.,1.,1.,
1.,1.,1.,1.,1.,1.,1.,1.,1.,1.,1.,1.,1.,1.,1.,1.,1.,1.,1.,1.,1.,1.,1.,1.,
1.,1.,1.,1.,1.,1.,1.,1.,1.,1.,1.,1.,1.,1.,1.,1.,1.,1.,1.,1.,1.,1.,1.,1.,
1.,1.,1.,1.,1.,1.))
REPRESENTATION_ITEM('')
);
#249=(
BOUNDED_CURVE()
B_SPLINE_CURVE(5,(#36995,#36996,#36997,#36998,#36999,#37000,#37001,#37002,
#37003,#37004,#37005,#37006,#37007,#37008,#37009,#37010,#37011,#37012,#37013,
#37014,#37015,#37016,#37017,#37018,#37019,#37020,#37021,#37022,#37023,#37024,
#37025,#37026,#37027,#37028,#37029,#37030,#37031,#37032,#37033,#37034,#37035,
#37036,#37037,#37038,#37039,#37040,#37041,#37042,#37043,#37044,#37045,#37046,
#37047,#37048,#37049,#37050,#37051,#37052,#37053,#37054,#37055,#37056,#37057,
#37058,#37059,#37060,#37061,#37062,#37063,#37064),.UNSPECIFIED.,.F.,.F.)
B_SPLINE_CURVE_WITH_KNOTS((6,1,1,1,1,1,1,1,1,1,1,1,1,1,1,1,1,1,1,1,1,1,
1,1,1,1,1,1,1,1,1,1,1,1,1,1,1,1,1,1,1,1,1,1,1,1,1,1,1,1,1,1,1,1,1,1,1,1,
1,1,1,1,1,1,1,6),(-1.,-0.984615384615383,-0.969230769230768,-0.953846153846152,
-0.938461538461537,-0.923076923076922,-0.907692307692306,-0.892307692307691,
-0.876923076923076,-0.86153846153846,-0.846153846153845,-0.83076923076923,
-0.815384615384614,-0.799999999999999,-0.784615384615384,-0.769230769230768,
-0.753846153846153,-0.738461538461538,-0.723076923076922,-0.707692307692307,
-0.692307692307692,-0.676923076923076,-0.661538461538461,-0.646153846153846,
-0.63076923076923,-0.615384615384615,-0.6,-0.584615384615384,-0.569230769230769,
-0.553846153846154,-0.538461538461538,-0.523076923076923,-0.507692307692308,
-0.492307692307692,-0.476923076923077,-0.461538461538462,-0.446153846153846,
-0.430769230769231,-0.415384615384615,-0.4,-0.384615384615385,-0.369230769230769,
-0.353846153846154,-0.338461538461538,-0.323076923076923,-0.307692307692308,
-0.292307692307692,-0.276923076923077,-0.261538461538462,-0.246153846153846,
-0.230769230769231,-0.215384615384615,-0.2,-0.184615384615385,-0.169230769230769,
-0.153846153846154,-0.138461538461538,-0.123076923076923,-0.107692307692308,
-0.0923076923076923,-0.0769230769230769,-0.0615384615384615,-0.0461538461538462,
-0.0307692307692308,-0.0153846153846154,0.),.UNSPECIFIED.)
CURVE()
GEOMETRIC_REPRESENTATION_ITEM()
RATIONAL_B_SPLINE_CURVE((1.,1.,1.,1.,1.,1.,1.,1.,1.,1.,1.,1.,1.,1.,1.,1.,
1.,1.,1.,1.,1.,1.,1.,1.,1.,1.,1.,1.,1.,1.,1.,1.,1.,1.,1.,1.,1.,1.,1.,1.,
1.,1.,1.,1.,1.,1.,1.,1.,1.,1.,1.,1.,1.,1.,1.,1.,1.,1.,1.,1.,1.,1.,1.,1.,
1.,1.,1.,1.,1.,1.))
REPRESENTATION_ITEM('')
);
#250=(
BOUNDED_CURVE()
B_SPLINE_CURVE(5,(#37211,#37212,#37213,#37214,#37215,#37216,#37217,#37218,
#37219,#37220,#37221,#37222,#37223,#37224,#37225,#37226,#37227,#37228,#37229,
#37230,#37231,#37232,#37233,#37234,#37235,#37236,#37237,#37238,#37239,#37240,
#37241,#37242,#37243,#37244,#37245,#37246,#37247,#37248,#37249,#37250,#37251,
#37252,#37253,#37254,#37255,#37256,#37257,#37258,#37259,#37260,#37261,#37262,
#37263,#37264,#37265,#37266,#37267,#37268,#37269,#37270,#37271,#37272,#37273,
#37274,#37275,#37276,#37277,#37278,#37279,#37280),.UNSPECIFIED.,.F.,.F.)
B_SPLINE_CURVE_WITH_KNOTS((6,1,1,1,1,1,1,1,1,1,1,1,1,1,1,1,1,1,1,1,1,1,
1,1,1,1,1,1,1,1,1,1,1,1,1,1,1,1,1,1,1,1,1,1,1,1,1,1,1,1,1,1,1,1,1,1,1,1,
1,1,1,1,1,1,1,6),(-1.,-0.984615384615383,-0.969230769230768,-0.953846153846152,
-0.938461538461537,-0.923076923076922,-0.907692307692306,-0.892307692307691,
-0.876923076923076,-0.86153846153846,-0.846153846153845,-0.83076923076923,
-0.815384615384614,-0.799999999999999,-0.784615384615384,-0.769230769230768,
-0.753846153846153,-0.738461538461538,-0.723076923076922,-0.707692307692307,
-0.692307692307692,-0.676923076923076,-0.661538461538461,-0.646153846153846,
-0.63076923076923,-0.615384615384615,-0.6,-0.584615384615384,-0.569230769230769,
-0.553846153846154,-0.538461538461538,-0.523076923076923,-0.507692307692308,
-0.492307692307692,-0.476923076923077,-0.461538461538462,-0.446153846153846,
-0.430769230769231,-0.415384615384615,-0.4,-0.384615384615385,-0.369230769230769,
-0.353846153846154,-0.338461538461538,-0.323076923076923,-0.307692307692308,
-0.292307692307692,-0.276923076923077,-0.261538461538462,-0.246153846153846,
-0.230769230769231,-0.215384615384615,-0.2,-0.184615384615385,-0.169230769230769,
-0.153846153846154,-0.138461538461538,-0.123076923076923,-0.107692307692308,
-0.0923076923076923,-0.0769230769230769,-0.0615384615384615,-0.0461538461538462,
-0.0307692307692308,-0.0153846153846154,0.),.UNSPECIFIED.)
CURVE()
GEOMETRIC_REPRESENTATION_ITEM()
RATIONAL_B_SPLINE_CURVE((1.,1.,1.,1.,1.,1.,1.,1.,1.,1.,1.,1.,1.,1.,1.,1.,
1.,1.,1.,1.,1.,1.,1.,1.,1.,1.,1.,1.,1.,1.,1.,1.,1.,1.,1.,1.,1.,1.,1.,1.,
1.,1.,1.,1.,1.,1.,1.,1.,1.,1.,1.,1.,1.,1.,1.,1.,1.,1.,1.,1.,1.,1.,1.,1.,
1.,1.,1.,1.,1.,1.))
REPRESENTATION_ITEM('')
);
#251=(
BOUNDED_CURVE()
B_SPLINE_CURVE(5,(#37694,#37695,#37696,#37697,#37698,#37699,#37700,#37701,
#37702,#37703,#37704,#37705,#37706,#37707,#37708,#37709,#37710,#37711,#37712,
#37713,#37714,#37715,#37716,#37717,#37718,#37719,#37720,#37721,#37722,#37723,
#37724,#37725,#37726,#37727,#37728,#37729,#37730,#37731,#37732,#37733,#37734,
#37735,#37736,#37737,#37738,#37739,#37740,#37741,#37742,#37743,#37744,#37745,
#37746,#37747,#37748,#37749,#37750,#37751,#37752,#37753,#37754,#37755,#37756,
#37757,#37758,#37759,#37760,#37761,#37762,#37763),.UNSPECIFIED.,.F.,.F.)
B_SPLINE_CURVE_WITH_KNOTS((6,1,1,1,1,1,1,1,1,1,1,1,1,1,1,1,1,1,1,1,1,1,
1,1,1,1,1,1,1,1,1,1,1,1,1,1,1,1,1,1,1,1,1,1,1,1,1,1,1,1,1,1,1,1,1,1,1,1,
1,1,1,1,1,1,1,6),(0.,0.0153846153846154,0.0307692307692308,0.0461538461538462,
0.0615384615384615,0.0769230769230769,0.0923076923076923,0.107692307692308,
0.123076923076923,0.138461538461538,0.153846153846154,0.169230769230769,
0.184615384615385,0.2,0.215384615384615,0.230769230769231,0.246153846153846,
0.261538461538462,0.276923076923077,0.292307692307692,0.307692307692308,
0.323076923076923,0.338461538461538,0.353846153846154,0.369230769230769,
0.384615384615385,0.4,0.415384615384615,0.430769230769231,0.446153846153846,
0.461538461538462,0.476923076923077,0.492307692307692,0.507692307692308,
0.523076923076923,0.538461538461538,0.553846153846154,0.569230769230769,
0.584615384615384,0.6,0.615384615384615,0.63076923076923,0.646153846153846,
0.661538461538461,0.676923076923076,0.692307692307692,0.707692307692307,
0.723076923076922,0.738461538461538,0.753846153846153,0.769230769230768,
0.784615384615384,0.799999999999999,0.815384615384614,0.83076923076923,
0.846153846153845,0.86153846153846,0.876923076923076,0.892307692307691,
0.907692307692306,0.923076923076922,0.938461538461537,0.953846153846152,
0.969230769230768,0.984615384615383,1.),.UNSPECIFIED.)
CURVE()
GEOMETRIC_REPRESENTATION_ITEM()
RATIONAL_B_SPLINE_CURVE((1.,1.,1.,1.,1.,1.,1.,1.,1.,1.,1.,1.,1.,1.,1.,1.,
1.,1.,1.,1.,1.,1.,1.,1.,1.,1.,1.,1.,1.,1.,1.,1.,1.,1.,1.,1.,1.,1.,1.,1.,
1.,1.,1.,1.,1.,1.,1.,1.,1.,1.,1.,1.,1.,1.,1.,1.,1.,1.,1.,1.,1.,1.,1.,1.,
1.,1.,1.,1.,1.,1.))
REPRESENTATION_ITEM('')
);
#252=(
BOUNDED_CURVE()
B_SPLINE_CURVE(5,(#37767,#37768,#37769,#37770,#37771,#37772,#37773,#37774,
#37775,#37776,#37777,#37778,#37779,#37780,#37781,#37782,#37783,#37784,#37785,
#37786,#37787,#37788,#37789,#37790,#37791,#37792,#37793,#37794,#37795,#37796,
#37797,#37798,#37799,#37800,#37801,#37802,#37803,#37804,#37805,#37806,#37807,
#37808,#37809,#37810,#37811,#37812,#37813,#37814,#37815,#37816,#37817,#37818,
#37819,#37820,#37821,#37822,#37823,#37824,#37825,#37826,#37827,#37828,#37829,
#37830,#37831,#37832,#37833,#37834,#37835,#37836),.UNSPECIFIED.,.F.,.F.)
B_SPLINE_CURVE_WITH_KNOTS((6,1,1,1,1,1,1,1,1,1,1,1,1,1,1,1,1,1,1,1,1,1,
1,1,1,1,1,1,1,1,1,1,1,1,1,1,1,1,1,1,1,1,1,1,1,1,1,1,1,1,1,1,1,1,1,1,1,1,
1,1,1,1,1,1,1,6),(0.,0.0153846153846154,0.0307692307692308,0.0461538461538462,
0.0615384615384615,0.0769230769230769,0.0923076923076923,0.107692307692308,
0.123076923076923,0.138461538461538,0.153846153846154,0.169230769230769,
0.184615384615385,0.2,0.215384615384615,0.230769230769231,0.246153846153846,
0.261538461538462,0.276923076923077,0.292307692307692,0.307692307692308,
0.323076923076923,0.338461538461538,0.353846153846154,0.369230769230769,
0.384615384615385,0.4,0.415384615384615,0.430769230769231,0.446153846153846,
0.461538461538462,0.476923076923077,0.492307692307692,0.507692307692308,
0.523076923076923,0.538461538461538,0.553846153846154,0.569230769230769,
0.584615384615384,0.6,0.615384615384615,0.63076923076923,0.646153846153846,
0.661538461538461,0.676923076923076,0.692307692307692,0.707692307692307,
0.723076923076922,0.738461538461538,0.753846153846153,0.769230769230768,
0.784615384615384,0.799999999999999,0.815384615384614,0.83076923076923,
0.846153846153845,0.86153846153846,0.876923076923076,0.892307692307691,
0.907692307692306,0.923076923076922,0.938461538461537,0.953846153846152,
0.969230769230768,0.984615384615383,1.),.UNSPECIFIED.)
CURVE()
GEOMETRIC_REPRESENTATION_ITEM()
RATIONAL_B_SPLINE_CURVE((1.,1.,1.,1.,1.,1.,1.,1.,1.,1.,1.,1.,1.,1.,1.,1.,
1.,1.,1.,1.,1.,1.,1.,1.,1.,1.,1.,1.,1.,1.,1.,1.,1.,1.,1.,1.,1.,1.,1.,1.,
1.,1.,1.,1.,1.,1.,1.,1.,1.,1.,1.,1.,1.,1.,1.,1.,1.,1.,1.,1.,1.,1.,1.,1.,
1.,1.,1.,1.,1.,1.))
REPRESENTATION_ITEM('')
);
#253=(
BOUNDED_CURVE()
B_SPLINE_CURVE(5,(#37840,#37841,#37842,#37843,#37844,#37845,#37846,#37847,
#37848,#37849,#37850,#37851,#37852,#37853,#37854,#37855,#37856,#37857,#37858,
#37859,#37860,#37861,#37862,#37863,#37864,#37865,#37866,#37867,#37868,#37869,
#37870,#37871,#37872,#37873,#37874,#37875,#37876,#37877,#37878,#37879,#37880,
#37881,#37882,#37883,#37884,#37885,#37886,#37887,#37888,#37889,#37890,#37891,
#37892,#37893,#37894,#37895,#37896,#37897,#37898,#37899,#37900,#37901,#37902,
#37903,#37904,#37905,#37906,#37907,#37908,#37909),.UNSPECIFIED.,.F.,.F.)
B_SPLINE_CURVE_WITH_KNOTS((6,1,1,1,1,1,1,1,1,1,1,1,1,1,1,1,1,1,1,1,1,1,
1,1,1,1,1,1,1,1,1,1,1,1,1,1,1,1,1,1,1,1,1,1,1,1,1,1,1,1,1,1,1,1,1,1,1,1,
1,1,1,1,1,1,1,6),(0.,0.0153846153846154,0.0307692307692308,0.0461538461538462,
0.0615384615384615,0.0769230769230769,0.0923076923076923,0.107692307692308,
0.123076923076923,0.138461538461538,0.153846153846154,0.169230769230769,
0.184615384615385,0.2,0.215384615384615,0.230769230769231,0.246153846153846,
0.261538461538462,0.276923076923077,0.292307692307692,0.307692307692308,
0.323076923076923,0.338461538461538,0.353846153846154,0.369230769230769,
0.384615384615385,0.4,0.415384615384615,0.430769230769231,0.446153846153846,
0.461538461538462,0.476923076923077,0.492307692307692,0.507692307692308,
0.523076923076923,0.538461538461538,0.553846153846154,0.569230769230769,
0.584615384615384,0.6,0.615384615384615,0.63076923076923,0.646153846153846,
0.661538461538461,0.676923076923076,0.692307692307692,0.707692307692307,
0.723076923076922,0.738461538461538,0.753846153846153,0.769230769230768,
0.784615384615384,0.799999999999999,0.815384615384614,0.83076923076923,
0.846153846153845,0.86153846153846,0.876923076923076,0.892307692307691,
0.907692307692306,0.923076923076922,0.938461538461537,0.953846153846152,
0.969230769230768,0.984615384615383,1.),.UNSPECIFIED.)
CURVE()
GEOMETRIC_REPRESENTATION_ITEM()
RATIONAL_B_SPLINE_CURVE((1.,1.,1.,1.,1.,1.,1.,1.,1.,1.,1.,1.,1.,1.,1.,1.,
1.,1.,1.,1.,1.,1.,1.,1.,1.,1.,1.,1.,1.,1.,1.,1.,1.,1.,1.,1.,1.,1.,1.,1.,
1.,1.,1.,1.,1.,1.,1.,1.,1.,1.,1.,1.,1.,1.,1.,1.,1.,1.,1.,1.,1.,1.,1.,1.,
1.,1.,1.,1.,1.,1.))
REPRESENTATION_ITEM('')
);
#254=(
BOUNDED_CURVE()
B_SPLINE_CURVE(5,(#37913,#37914,#37915,#37916,#37917,#37918,#37919,#37920,
#37921,#37922,#37923,#37924,#37925,#37926,#37927,#37928,#37929,#37930,#37931,
#37932,#37933,#37934,#37935,#37936,#37937,#37938,#37939,#37940,#37941,#37942,
#37943,#37944,#37945,#37946,#37947,#37948,#37949,#37950,#37951,#37952,#37953,
#37954,#37955,#37956,#37957,#37958,#37959,#37960,#37961,#37962,#37963,#37964,
#37965,#37966,#37967,#37968,#37969,#37970,#37971,#37972,#37973,#37974,#37975,
#37976,#37977,#37978,#37979,#37980,#37981,#37982),.UNSPECIFIED.,.F.,.F.)
B_SPLINE_CURVE_WITH_KNOTS((6,1,1,1,1,1,1,1,1,1,1,1,1,1,1,1,1,1,1,1,1,1,
1,1,1,1,1,1,1,1,1,1,1,1,1,1,1,1,1,1,1,1,1,1,1,1,1,1,1,1,1,1,1,1,1,1,1,1,
1,1,1,1,1,1,1,6),(0.,0.0153846153846154,0.0307692307692308,0.0461538461538462,
0.0615384615384615,0.0769230769230769,0.0923076923076923,0.107692307692308,
0.123076923076923,0.138461538461538,0.153846153846154,0.169230769230769,
0.184615384615385,0.2,0.215384615384615,0.230769230769231,0.246153846153846,
0.261538461538462,0.276923076923077,0.292307692307692,0.307692307692308,
0.323076923076923,0.338461538461538,0.353846153846154,0.369230769230769,
0.384615384615385,0.4,0.415384615384615,0.430769230769231,0.446153846153846,
0.461538461538462,0.476923076923077,0.492307692307692,0.507692307692308,
0.523076923076923,0.538461538461538,0.553846153846154,0.569230769230769,
0.584615384615384,0.6,0.615384615384615,0.63076923076923,0.646153846153846,
0.661538461538461,0.676923076923076,0.692307692307692,0.707692307692307,
0.723076923076922,0.738461538461538,0.753846153846153,0.769230769230768,
0.784615384615384,0.799999999999999,0.815384615384614,0.83076923076923,
0.846153846153845,0.86153846153846,0.876923076923076,0.892307692307691,
0.907692307692306,0.923076923076922,0.938461538461537,0.953846153846152,
0.969230769230768,0.984615384615383,1.),.UNSPECIFIED.)
CURVE()
GEOMETRIC_REPRESENTATION_ITEM()
RATIONAL_B_SPLINE_CURVE((1.,1.,1.,1.,1.,1.,1.,1.,1.,1.,1.,1.,1.,1.,1.,1.,
1.,1.,1.,1.,1.,1.,1.,1.,1.,1.,1.,1.,1.,1.,1.,1.,1.,1.,1.,1.,1.,1.,1.,1.,
1.,1.,1.,1.,1.,1.,1.,1.,1.,1.,1.,1.,1.,1.,1.,1.,1.,1.,1.,1.,1.,1.,1.,1.,
1.,1.,1.,1.,1.,1.))
REPRESENTATION_ITEM('')
);
#255=(
BOUNDED_CURVE()
B_SPLINE_CURVE(5,(#37986,#37987,#37988,#37989,#37990,#37991,#37992,#37993,
#37994,#37995,#37996,#37997,#37998,#37999,#38000,#38001,#38002,#38003,#38004,
#38005,#38006,#38007,#38008,#38009,#38010,#38011,#38012,#38013,#38014,#38015,
#38016,#38017,#38018,#38019,#38020,#38021,#38022,#38023,#38024,#38025,#38026,
#38027,#38028,#38029,#38030,#38031,#38032,#38033,#38034,#38035,#38036,#38037,
#38038,#38039,#38040,#38041,#38042,#38043,#38044,#38045,#38046,#38047,#38048,
#38049,#38050,#38051,#38052,#38053,#38054,#38055),.UNSPECIFIED.,.F.,.F.)
B_SPLINE_CURVE_WITH_KNOTS((6,1,1,1,1,1,1,1,1,1,1,1,1,1,1,1,1,1,1,1,1,1,
1,1,1,1,1,1,1,1,1,1,1,1,1,1,1,1,1,1,1,1,1,1,1,1,1,1,1,1,1,1,1,1,1,1,1,1,
1,1,1,1,1,1,1,6),(0.,0.0153846153846154,0.0307692307692308,0.0461538461538462,
0.0615384615384615,0.0769230769230769,0.0923076923076923,0.107692307692308,
0.123076923076923,0.138461538461538,0.153846153846154,0.169230769230769,
0.184615384615385,0.2,0.215384615384615,0.230769230769231,0.246153846153846,
0.261538461538462,0.276923076923077,0.292307692307692,0.307692307692308,
0.323076923076923,0.338461538461538,0.353846153846154,0.369230769230769,
0.384615384615385,0.4,0.415384615384615,0.430769230769231,0.446153846153846,
0.461538461538462,0.476923076923077,0.492307692307692,0.507692307692308,
0.523076923076923,0.538461538461538,0.553846153846154,0.569230769230769,
0.584615384615384,0.6,0.615384615384615,0.63076923076923,0.646153846153846,
0.661538461538461,0.676923076923076,0.692307692307692,0.707692307692307,
0.723076923076922,0.738461538461538,0.753846153846153,0.769230769230768,
0.784615384615384,0.799999999999999,0.815384615384614,0.83076923076923,
0.846153846153845,0.86153846153846,0.876923076923076,0.892307692307691,
0.907692307692306,0.923076923076922,0.938461538461537,0.953846153846152,
0.969230769230768,0.984615384615383,1.),.UNSPECIFIED.)
CURVE()
GEOMETRIC_REPRESENTATION_ITEM()
RATIONAL_B_SPLINE_CURVE((1.,1.,1.,1.,1.,1.,1.,1.,1.,1.,1.,1.,1.,1.,1.,1.,
1.,1.,1.,1.,1.,1.,1.,1.,1.,1.,1.,1.,1.,1.,1.,1.,1.,1.,1.,1.,1.,1.,1.,1.,
1.,1.,1.,1.,1.,1.,1.,1.,1.,1.,1.,1.,1.,1.,1.,1.,1.,1.,1.,1.,1.,1.,1.,1.,
1.,1.,1.,1.,1.,1.))
REPRESENTATION_ITEM('')
);
#256=(
BOUNDED_CURVE()
B_SPLINE_CURVE(5,(#38059,#38060,#38061,#38062,#38063,#38064,#38065,#38066,
#38067,#38068,#38069,#38070,#38071,#38072,#38073,#38074,#38075,#38076,#38077,
#38078,#38079,#38080,#38081,#38082,#38083,#38084,#38085,#38086,#38087,#38088,
#38089,#38090,#38091,#38092,#38093,#38094,#38095,#38096,#38097,#38098,#38099,
#38100,#38101,#38102,#38103,#38104,#38105,#38106,#38107,#38108,#38109,#38110,
#38111,#38112,#38113,#38114,#38115,#38116,#38117,#38118,#38119,#38120,#38121,
#38122,#38123,#38124,#38125,#38126,#38127,#38128),.UNSPECIFIED.,.F.,.F.)
B_SPLINE_CURVE_WITH_KNOTS((6,1,1,1,1,1,1,1,1,1,1,1,1,1,1,1,1,1,1,1,1,1,
1,1,1,1,1,1,1,1,1,1,1,1,1,1,1,1,1,1,1,1,1,1,1,1,1,1,1,1,1,1,1,1,1,1,1,1,
1,1,1,1,1,1,1,6),(0.,0.0153846153846154,0.0307692307692308,0.0461538461538462,
0.0615384615384615,0.0769230769230769,0.0923076923076923,0.107692307692308,
0.123076923076923,0.138461538461538,0.153846153846154,0.169230769230769,
0.184615384615385,0.2,0.215384615384615,0.230769230769231,0.246153846153846,
0.261538461538462,0.276923076923077,0.292307692307692,0.307692307692308,
0.323076923076923,0.338461538461538,0.353846153846154,0.369230769230769,
0.384615384615385,0.4,0.415384615384615,0.430769230769231,0.446153846153846,
0.461538461538462,0.476923076923077,0.492307692307692,0.507692307692308,
0.523076923076923,0.538461538461538,0.553846153846154,0.569230769230769,
0.584615384615384,0.6,0.615384615384615,0.63076923076923,0.646153846153846,
0.661538461538461,0.676923076923076,0.692307692307692,0.707692307692307,
0.723076923076922,0.738461538461538,0.753846153846153,0.769230769230768,
0.784615384615384,0.799999999999999,0.815384615384614,0.83076923076923,
0.846153846153845,0.86153846153846,0.876923076923076,0.892307692307691,
0.907692307692306,0.923076923076922,0.938461538461537,0.953846153846152,
0.969230769230768,0.984615384615383,1.),.UNSPECIFIED.)
CURVE()
GEOMETRIC_REPRESENTATION_ITEM()
RATIONAL_B_SPLINE_CURVE((1.,1.,1.,1.,1.,1.,1.,1.,1.,1.,1.,1.,1.,1.,1.,1.,
1.,1.,1.,1.,1.,1.,1.,1.,1.,1.,1.,1.,1.,1.,1.,1.,1.,1.,1.,1.,1.,1.,1.,1.,
1.,1.,1.,1.,1.,1.,1.,1.,1.,1.,1.,1.,1.,1.,1.,1.,1.,1.,1.,1.,1.,1.,1.,1.,
1.,1.,1.,1.,1.,1.))
REPRESENTATION_ITEM('')
);
#257=(
BOUNDED_CURVE()
B_SPLINE_CURVE(5,(#38132,#38133,#38134,#38135,#38136,#38137,#38138,#38139,
#38140,#38141,#38142,#38143,#38144,#38145,#38146,#38147,#38148,#38149,#38150,
#38151,#38152,#38153,#38154,#38155,#38156,#38157,#38158,#38159,#38160,#38161,
#38162,#38163,#38164,#38165,#38166,#38167,#38168,#38169,#38170,#38171,#38172,
#38173,#38174,#38175,#38176,#38177,#38178,#38179,#38180,#38181,#38182,#38183,
#38184,#38185,#38186,#38187,#38188,#38189,#38190,#38191,#38192,#38193,#38194,
#38195,#38196,#38197,#38198,#38199,#38200,#38201),.UNSPECIFIED.,.F.,.F.)
B_SPLINE_CURVE_WITH_KNOTS((6,1,1,1,1,1,1,1,1,1,1,1,1,1,1,1,1,1,1,1,1,1,
1,1,1,1,1,1,1,1,1,1,1,1,1,1,1,1,1,1,1,1,1,1,1,1,1,1,1,1,1,1,1,1,1,1,1,1,
1,1,1,1,1,1,1,6),(0.,0.0153846153846154,0.0307692307692308,0.0461538461538462,
0.0615384615384615,0.0769230769230769,0.0923076923076923,0.107692307692308,
0.123076923076923,0.138461538461538,0.153846153846154,0.169230769230769,
0.184615384615385,0.2,0.215384615384615,0.230769230769231,0.246153846153846,
0.261538461538462,0.276923076923077,0.292307692307692,0.307692307692308,
0.323076923076923,0.338461538461538,0.353846153846154,0.369230769230769,
0.384615384615385,0.4,0.415384615384615,0.430769230769231,0.446153846153846,
0.461538461538462,0.476923076923077,0.492307692307692,0.507692307692308,
0.523076923076923,0.538461538461538,0.553846153846154,0.569230769230769,
0.584615384615384,0.6,0.615384615384615,0.63076923076923,0.646153846153846,
0.661538461538461,0.676923076923076,0.692307692307692,0.707692307692307,
0.723076923076922,0.738461538461538,0.753846153846153,0.769230769230768,
0.784615384615384,0.799999999999999,0.815384615384614,0.83076923076923,
0.846153846153845,0.86153846153846,0.876923076923076,0.892307692307691,
0.907692307692306,0.923076923076922,0.938461538461537,0.953846153846152,
0.969230769230768,0.984615384615383,1.),.UNSPECIFIED.)
CURVE()
GEOMETRIC_REPRESENTATION_ITEM()
RATIONAL_B_SPLINE_CURVE((1.,1.,1.,1.,1.,1.,1.,1.,1.,1.,1.,1.,1.,1.,1.,1.,
1.,1.,1.,1.,1.,1.,1.,1.,1.,1.,1.,1.,1.,1.,1.,1.,1.,1.,1.,1.,1.,1.,1.,1.,
1.,1.,1.,1.,1.,1.,1.,1.,1.,1.,1.,1.,1.,1.,1.,1.,1.,1.,1.,1.,1.,1.,1.,1.,
1.,1.,1.,1.,1.,1.))
REPRESENTATION_ITEM('')
);
#258=(
BOUNDED_CURVE()
B_SPLINE_CURVE(5,(#38205,#38206,#38207,#38208,#38209,#38210,#38211,#38212,
#38213,#38214,#38215,#38216,#38217,#38218,#38219,#38220,#38221,#38222,#38223,
#38224,#38225,#38226,#38227,#38228,#38229,#38230,#38231,#38232,#38233,#38234,
#38235,#38236,#38237,#38238,#38239,#38240,#38241,#38242,#38243,#38244,#38245,
#38246,#38247,#38248,#38249,#38250,#38251,#38252,#38253,#38254,#38255,#38256,
#38257,#38258,#38259,#38260,#38261,#38262,#38263,#38264,#38265,#38266,#38267,
#38268,#38269,#38270,#38271,#38272,#38273,#38274),.UNSPECIFIED.,.F.,.F.)
B_SPLINE_CURVE_WITH_KNOTS((6,1,1,1,1,1,1,1,1,1,1,1,1,1,1,1,1,1,1,1,1,1,
1,1,1,1,1,1,1,1,1,1,1,1,1,1,1,1,1,1,1,1,1,1,1,1,1,1,1,1,1,1,1,1,1,1,1,1,
1,1,1,1,1,1,1,6),(0.,0.0153846153846154,0.0307692307692308,0.0461538461538462,
0.0615384615384615,0.0769230769230769,0.0923076923076923,0.107692307692308,
0.123076923076923,0.138461538461538,0.153846153846154,0.169230769230769,
0.184615384615385,0.2,0.215384615384615,0.230769230769231,0.246153846153846,
0.261538461538462,0.276923076923077,0.292307692307692,0.307692307692308,
0.323076923076923,0.338461538461538,0.353846153846154,0.369230769230769,
0.384615384615385,0.4,0.415384615384615,0.430769230769231,0.446153846153846,
0.461538461538462,0.476923076923077,0.492307692307692,0.507692307692308,
0.523076923076923,0.538461538461538,0.553846153846154,0.569230769230769,
0.584615384615384,0.6,0.615384615384615,0.63076923076923,0.646153846153846,
0.661538461538461,0.676923076923076,0.692307692307692,0.707692307692307,
0.723076923076922,0.738461538461538,0.753846153846153,0.769230769230768,
0.784615384615384,0.799999999999999,0.815384615384614,0.83076923076923,
0.846153846153845,0.86153846153846,0.876923076923076,0.892307692307691,
0.907692307692306,0.923076923076922,0.938461538461537,0.953846153846152,
0.969230769230768,0.984615384615383,1.),.UNSPECIFIED.)
CURVE()
GEOMETRIC_REPRESENTATION_ITEM()
RATIONAL_B_SPLINE_CURVE((1.,1.,1.,1.,1.,1.,1.,1.,1.,1.,1.,1.,1.,1.,1.,1.,
1.,1.,1.,1.,1.,1.,1.,1.,1.,1.,1.,1.,1.,1.,1.,1.,1.,1.,1.,1.,1.,1.,1.,1.,
1.,1.,1.,1.,1.,1.,1.,1.,1.,1.,1.,1.,1.,1.,1.,1.,1.,1.,1.,1.,1.,1.,1.,1.,
1.,1.,1.,1.,1.,1.))
REPRESENTATION_ITEM('')
);
#259=(
BOUNDED_CURVE()
B_SPLINE_CURVE(5,(#38278,#38279,#38280,#38281,#38282,#38283,#38284,#38285,
#38286,#38287,#38288,#38289,#38290,#38291,#38292,#38293,#38294,#38295,#38296,
#38297,#38298,#38299,#38300,#38301,#38302,#38303,#38304,#38305,#38306,#38307,
#38308,#38309,#38310,#38311,#38312,#38313,#38314,#38315,#38316,#38317,#38318,
#38319,#38320,#38321,#38322,#38323,#38324,#38325,#38326,#38327,#38328,#38329,
#38330,#38331,#38332,#38333,#38334,#38335,#38336,#38337,#38338,#38339,#38340,
#38341,#38342,#38343,#38344,#38345,#38346,#38347),.UNSPECIFIED.,.F.,.F.)
B_SPLINE_CURVE_WITH_KNOTS((6,1,1,1,1,1,1,1,1,1,1,1,1,1,1,1,1,1,1,1,1,1,
1,1,1,1,1,1,1,1,1,1,1,1,1,1,1,1,1,1,1,1,1,1,1,1,1,1,1,1,1,1,1,1,1,1,1,1,
1,1,1,1,1,1,1,6),(0.,0.0153846153846154,0.0307692307692308,0.0461538461538462,
0.0615384615384615,0.0769230769230769,0.0923076923076923,0.107692307692308,
0.123076923076923,0.138461538461538,0.153846153846154,0.169230769230769,
0.184615384615385,0.2,0.215384615384615,0.230769230769231,0.246153846153846,
0.261538461538462,0.276923076923077,0.292307692307692,0.307692307692308,
0.323076923076923,0.338461538461538,0.353846153846154,0.369230769230769,
0.384615384615385,0.4,0.415384615384615,0.430769230769231,0.446153846153846,
0.461538461538462,0.476923076923077,0.492307692307692,0.507692307692308,
0.523076923076923,0.538461538461538,0.553846153846154,0.569230769230769,
0.584615384615384,0.6,0.615384615384615,0.63076923076923,0.646153846153846,
0.661538461538461,0.676923076923076,0.692307692307692,0.707692307692307,
0.723076923076922,0.738461538461538,0.753846153846153,0.769230769230768,
0.784615384615384,0.799999999999999,0.815384615384614,0.83076923076923,
0.846153846153845,0.86153846153846,0.876923076923076,0.892307692307691,
0.907692307692306,0.923076923076922,0.938461538461537,0.953846153846152,
0.969230769230768,0.984615384615383,1.),.UNSPECIFIED.)
CURVE()
GEOMETRIC_REPRESENTATION_ITEM()
RATIONAL_B_SPLINE_CURVE((1.,1.,1.,1.,1.,1.,1.,1.,1.,1.,1.,1.,1.,1.,1.,1.,
1.,1.,1.,1.,1.,1.,1.,1.,1.,1.,1.,1.,1.,1.,1.,1.,1.,1.,1.,1.,1.,1.,1.,1.,
1.,1.,1.,1.,1.,1.,1.,1.,1.,1.,1.,1.,1.,1.,1.,1.,1.,1.,1.,1.,1.,1.,1.,1.,
1.,1.,1.,1.,1.,1.))
REPRESENTATION_ITEM('')
);
#260=(
BOUNDED_CURVE()
B_SPLINE_CURVE(5,(#38351,#38352,#38353,#38354,#38355,#38356,#38357,#38358,
#38359,#38360,#38361,#38362,#38363,#38364,#38365,#38366,#38367,#38368,#38369,
#38370,#38371,#38372,#38373,#38374,#38375,#38376,#38377,#38378,#38379,#38380,
#38381,#38382,#38383,#38384,#38385,#38386,#38387,#38388,#38389,#38390,#38391,
#38392,#38393,#38394,#38395,#38396,#38397,#38398,#38399,#38400,#38401,#38402,
#38403,#38404,#38405,#38406,#38407,#38408,#38409,#38410,#38411,#38412,#38413,
#38414,#38415,#38416,#38417,#38418,#38419,#38420),.UNSPECIFIED.,.F.,.F.)
B_SPLINE_CURVE_WITH_KNOTS((6,1,1,1,1,1,1,1,1,1,1,1,1,1,1,1,1,1,1,1,1,1,
1,1,1,1,1,1,1,1,1,1,1,1,1,1,1,1,1,1,1,1,1,1,1,1,1,1,1,1,1,1,1,1,1,1,1,1,
1,1,1,1,1,1,1,6),(0.,0.0153846153846154,0.0307692307692308,0.0461538461538462,
0.0615384615384615,0.0769230769230769,0.0923076923076923,0.107692307692308,
0.123076923076923,0.138461538461538,0.153846153846154,0.169230769230769,
0.184615384615385,0.2,0.215384615384615,0.230769230769231,0.246153846153846,
0.261538461538462,0.276923076923077,0.292307692307692,0.307692307692308,
0.323076923076923,0.338461538461538,0.353846153846154,0.369230769230769,
0.384615384615385,0.4,0.415384615384615,0.430769230769231,0.446153846153846,
0.461538461538462,0.476923076923077,0.492307692307692,0.507692307692308,
0.523076923076923,0.538461538461538,0.553846153846154,0.569230769230769,
0.584615384615384,0.6,0.615384615384615,0.63076923076923,0.646153846153846,
0.661538461538461,0.676923076923076,0.692307692307692,0.707692307692307,
0.723076923076922,0.738461538461538,0.753846153846153,0.769230769230768,
0.784615384615384,0.799999999999999,0.815384615384614,0.83076923076923,
0.846153846153845,0.86153846153846,0.876923076923076,0.892307692307691,
0.907692307692306,0.923076923076922,0.938461538461537,0.953846153846152,
0.969230769230768,0.984615384615383,1.),.UNSPECIFIED.)
CURVE()
GEOMETRIC_REPRESENTATION_ITEM()
RATIONAL_B_SPLINE_CURVE((1.,1.,1.,1.,1.,1.,1.,1.,1.,1.,1.,1.,1.,1.,1.,1.,
1.,1.,1.,1.,1.,1.,1.,1.,1.,1.,1.,1.,1.,1.,1.,1.,1.,1.,1.,1.,1.,1.,1.,1.,
1.,1.,1.,1.,1.,1.,1.,1.,1.,1.,1.,1.,1.,1.,1.,1.,1.,1.,1.,1.,1.,1.,1.,1.,
1.,1.,1.,1.,1.,1.))
REPRESENTATION_ITEM('')
);
#261=(
BOUNDED_CURVE()
B_SPLINE_CURVE(5,(#38424,#38425,#38426,#38427,#38428,#38429,#38430,#38431,
#38432,#38433,#38434,#38435,#38436,#38437,#38438,#38439,#38440,#38441,#38442,
#38443,#38444,#38445,#38446,#38447,#38448,#38449,#38450,#38451,#38452,#38453,
#38454,#38455,#38456,#38457,#38458,#38459,#38460,#38461,#38462,#38463,#38464,
#38465,#38466,#38467,#38468,#38469,#38470,#38471,#38472,#38473,#38474,#38475,
#38476,#38477,#38478,#38479,#38480,#38481,#38482,#38483,#38484,#38485,#38486,
#38487,#38488,#38489,#38490,#38491,#38492,#38493),.UNSPECIFIED.,.F.,.F.)
B_SPLINE_CURVE_WITH_KNOTS((6,1,1,1,1,1,1,1,1,1,1,1,1,1,1,1,1,1,1,1,1,1,
1,1,1,1,1,1,1,1,1,1,1,1,1,1,1,1,1,1,1,1,1,1,1,1,1,1,1,1,1,1,1,1,1,1,1,1,
1,1,1,1,1,1,1,6),(0.,0.0153846153846154,0.0307692307692308,0.0461538461538462,
0.0615384615384615,0.0769230769230769,0.0923076923076923,0.107692307692308,
0.123076923076923,0.138461538461538,0.153846153846154,0.169230769230769,
0.184615384615385,0.2,0.215384615384615,0.230769230769231,0.246153846153846,
0.261538461538462,0.276923076923077,0.292307692307692,0.307692307692308,
0.323076923076923,0.338461538461538,0.353846153846154,0.369230769230769,
0.384615384615385,0.4,0.415384615384615,0.430769230769231,0.446153846153846,
0.461538461538462,0.476923076923077,0.492307692307692,0.507692307692308,
0.523076923076923,0.538461538461538,0.553846153846154,0.569230769230769,
0.584615384615384,0.6,0.615384615384615,0.63076923076923,0.646153846153846,
0.661538461538461,0.676923076923076,0.692307692307692,0.707692307692307,
0.723076923076922,0.738461538461538,0.753846153846153,0.769230769230768,
0.784615384615384,0.799999999999999,0.815384615384614,0.83076923076923,
0.846153846153845,0.86153846153846,0.876923076923076,0.892307692307691,
0.907692307692306,0.923076923076922,0.938461538461537,0.953846153846152,
0.969230769230768,0.984615384615383,1.),.UNSPECIFIED.)
CURVE()
GEOMETRIC_REPRESENTATION_ITEM()
RATIONAL_B_SPLINE_CURVE((1.,1.,1.,1.,1.,1.,1.,1.,1.,1.,1.,1.,1.,1.,1.,1.,
1.,1.,1.,1.,1.,1.,1.,1.,1.,1.,1.,1.,1.,1.,1.,1.,1.,1.,1.,1.,1.,1.,1.,1.,
1.,1.,1.,1.,1.,1.,1.,1.,1.,1.,1.,1.,1.,1.,1.,1.,1.,1.,1.,1.,1.,1.,1.,1.,
1.,1.,1.,1.,1.,1.))
REPRESENTATION_ITEM('')
);
#262=(
BOUNDED_CURVE()
B_SPLINE_CURVE(5,(#38497,#38498,#38499,#38500,#38501,#38502,#38503,#38504,
#38505,#38506,#38507,#38508,#38509,#38510,#38511,#38512,#38513,#38514,#38515,
#38516,#38517,#38518,#38519,#38520,#38521,#38522,#38523,#38524,#38525,#38526,
#38527,#38528,#38529,#38530,#38531,#38532,#38533,#38534,#38535,#38536,#38537,
#38538,#38539,#38540,#38541,#38542,#38543,#38544,#38545,#38546,#38547,#38548,
#38549,#38550,#38551,#38552,#38553,#38554,#38555,#38556,#38557,#38558,#38559,
#38560,#38561,#38562,#38563,#38564,#38565,#38566),.UNSPECIFIED.,.F.,.F.)
B_SPLINE_CURVE_WITH_KNOTS((6,1,1,1,1,1,1,1,1,1,1,1,1,1,1,1,1,1,1,1,1,1,
1,1,1,1,1,1,1,1,1,1,1,1,1,1,1,1,1,1,1,1,1,1,1,1,1,1,1,1,1,1,1,1,1,1,1,1,
1,1,1,1,1,1,1,6),(0.,0.0153846153846154,0.0307692307692308,0.0461538461538462,
0.0615384615384615,0.0769230769230769,0.0923076923076923,0.107692307692308,
0.123076923076923,0.138461538461538,0.153846153846154,0.169230769230769,
0.184615384615385,0.2,0.215384615384615,0.230769230769231,0.246153846153846,
0.261538461538462,0.276923076923077,0.292307692307692,0.307692307692308,
0.323076923076923,0.338461538461538,0.353846153846154,0.369230769230769,
0.384615384615385,0.4,0.415384615384615,0.430769230769231,0.446153846153846,
0.461538461538462,0.476923076923077,0.492307692307692,0.507692307692308,
0.523076923076923,0.538461538461538,0.553846153846154,0.569230769230769,
0.584615384615384,0.6,0.615384615384615,0.63076923076923,0.646153846153846,
0.661538461538461,0.676923076923076,0.692307692307692,0.707692307692307,
0.723076923076922,0.738461538461538,0.753846153846153,0.769230769230768,
0.784615384615384,0.799999999999999,0.815384615384614,0.83076923076923,
0.846153846153845,0.86153846153846,0.876923076923076,0.892307692307691,
0.907692307692306,0.923076923076922,0.938461538461537,0.953846153846152,
0.969230769230768,0.984615384615383,1.),.UNSPECIFIED.)
CURVE()
GEOMETRIC_REPRESENTATION_ITEM()
RATIONAL_B_SPLINE_CURVE((1.,1.,1.,1.,1.,1.,1.,1.,1.,1.,1.,1.,1.,1.,1.,1.,
1.,1.,1.,1.,1.,1.,1.,1.,1.,1.,1.,1.,1.,1.,1.,1.,1.,1.,1.,1.,1.,1.,1.,1.,
1.,1.,1.,1.,1.,1.,1.,1.,1.,1.,1.,1.,1.,1.,1.,1.,1.,1.,1.,1.,1.,1.,1.,1.,
1.,1.,1.,1.,1.,1.))
REPRESENTATION_ITEM('')
);
#263=(
BOUNDED_CURVE()
B_SPLINE_CURVE(5,(#38570,#38571,#38572,#38573,#38574,#38575,#38576,#38577,
#38578,#38579,#38580,#38581,#38582,#38583,#38584,#38585,#38586,#38587,#38588,
#38589,#38590,#38591,#38592,#38593,#38594,#38595,#38596,#38597,#38598,#38599,
#38600,#38601,#38602,#38603,#38604,#38605,#38606,#38607,#38608,#38609,#38610,
#38611,#38612,#38613,#38614,#38615,#38616,#38617,#38618,#38619,#38620,#38621,
#38622,#38623,#38624,#38625,#38626,#38627,#38628,#38629,#38630,#38631,#38632,
#38633,#38634,#38635,#38636,#38637,#38638,#38639),.UNSPECIFIED.,.F.,.F.)
B_SPLINE_CURVE_WITH_KNOTS((6,1,1,1,1,1,1,1,1,1,1,1,1,1,1,1,1,1,1,1,1,1,
1,1,1,1,1,1,1,1,1,1,1,1,1,1,1,1,1,1,1,1,1,1,1,1,1,1,1,1,1,1,1,1,1,1,1,1,
1,1,1,1,1,1,1,6),(0.,0.0153846153846154,0.0307692307692308,0.0461538461538462,
0.0615384615384615,0.0769230769230769,0.0923076923076923,0.107692307692308,
0.123076923076923,0.138461538461538,0.153846153846154,0.169230769230769,
0.184615384615385,0.2,0.215384615384615,0.230769230769231,0.246153846153846,
0.261538461538462,0.276923076923077,0.292307692307692,0.307692307692308,
0.323076923076923,0.338461538461538,0.353846153846154,0.369230769230769,
0.384615384615385,0.4,0.415384615384615,0.430769230769231,0.446153846153846,
0.461538461538462,0.476923076923077,0.492307692307692,0.507692307692308,
0.523076923076923,0.538461538461538,0.553846153846154,0.569230769230769,
0.584615384615384,0.6,0.615384615384615,0.63076923076923,0.646153846153846,
0.661538461538461,0.676923076923076,0.692307692307692,0.707692307692307,
0.723076923076922,0.738461538461538,0.753846153846153,0.769230769230768,
0.784615384615384,0.799999999999999,0.815384615384614,0.83076923076923,
0.846153846153845,0.86153846153846,0.876923076923076,0.892307692307691,
0.907692307692306,0.923076923076922,0.938461538461537,0.953846153846152,
0.969230769230768,0.984615384615383,1.),.UNSPECIFIED.)
CURVE()
GEOMETRIC_REPRESENTATION_ITEM()
RATIONAL_B_SPLINE_CURVE((1.,1.,1.,1.,1.,1.,1.,1.,1.,1.,1.,1.,1.,1.,1.,1.,
1.,1.,1.,1.,1.,1.,1.,1.,1.,1.,1.,1.,1.,1.,1.,1.,1.,1.,1.,1.,1.,1.,1.,1.,
1.,1.,1.,1.,1.,1.,1.,1.,1.,1.,1.,1.,1.,1.,1.,1.,1.,1.,1.,1.,1.,1.,1.,1.,
1.,1.,1.,1.,1.,1.))
REPRESENTATION_ITEM('')
);
#264=(
BOUNDED_CURVE()
B_SPLINE_CURVE(5,(#38643,#38644,#38645,#38646,#38647,#38648,#38649,#38650,
#38651,#38652,#38653,#38654,#38655,#38656,#38657,#38658,#38659,#38660,#38661,
#38662,#38663,#38664,#38665,#38666,#38667,#38668,#38669,#38670,#38671,#38672,
#38673,#38674,#38675,#38676,#38677,#38678,#38679,#38680,#38681,#38682,#38683,
#38684,#38685,#38686,#38687,#38688,#38689,#38690,#38691,#38692,#38693,#38694,
#38695,#38696,#38697,#38698,#38699,#38700,#38701,#38702,#38703,#38704,#38705,
#38706,#38707,#38708,#38709,#38710,#38711,#38712),.UNSPECIFIED.,.F.,.F.)
B_SPLINE_CURVE_WITH_KNOTS((6,1,1,1,1,1,1,1,1,1,1,1,1,1,1,1,1,1,1,1,1,1,
1,1,1,1,1,1,1,1,1,1,1,1,1,1,1,1,1,1,1,1,1,1,1,1,1,1,1,1,1,1,1,1,1,1,1,1,
1,1,1,1,1,1,1,6),(0.,0.0153846153846154,0.0307692307692308,0.0461538461538462,
0.0615384615384615,0.0769230769230769,0.0923076923076923,0.107692307692308,
0.123076923076923,0.138461538461538,0.153846153846154,0.169230769230769,
0.184615384615385,0.2,0.215384615384615,0.230769230769231,0.246153846153846,
0.261538461538462,0.276923076923077,0.292307692307692,0.307692307692308,
0.323076923076923,0.338461538461538,0.353846153846154,0.369230769230769,
0.384615384615385,0.4,0.415384615384615,0.430769230769231,0.446153846153846,
0.461538461538462,0.476923076923077,0.492307692307692,0.507692307692308,
0.523076923076923,0.538461538461538,0.553846153846154,0.569230769230769,
0.584615384615384,0.6,0.615384615384615,0.63076923076923,0.646153846153846,
0.661538461538461,0.676923076923076,0.692307692307692,0.707692307692307,
0.723076923076922,0.738461538461538,0.753846153846153,0.769230769230768,
0.784615384615384,0.799999999999999,0.815384615384614,0.83076923076923,
0.846153846153845,0.86153846153846,0.876923076923076,0.892307692307691,
0.907692307692306,0.923076923076922,0.938461538461537,0.953846153846152,
0.969230769230768,0.984615384615383,1.),.UNSPECIFIED.)
CURVE()
GEOMETRIC_REPRESENTATION_ITEM()
RATIONAL_B_SPLINE_CURVE((1.,1.,1.,1.,1.,1.,1.,1.,1.,1.,1.,1.,1.,1.,1.,1.,
1.,1.,1.,1.,1.,1.,1.,1.,1.,1.,1.,1.,1.,1.,1.,1.,1.,1.,1.,1.,1.,1.,1.,1.,
1.,1.,1.,1.,1.,1.,1.,1.,1.,1.,1.,1.,1.,1.,1.,1.,1.,1.,1.,1.,1.,1.,1.,1.,
1.,1.,1.,1.,1.,1.))
REPRESENTATION_ITEM('')
);
#265=(
BOUNDED_CURVE()
B_SPLINE_CURVE(5,(#38716,#38717,#38718,#38719,#38720,#38721,#38722,#38723,
#38724,#38725,#38726,#38727,#38728,#38729,#38730,#38731,#38732,#38733,#38734,
#38735,#38736,#38737,#38738,#38739,#38740,#38741,#38742,#38743,#38744,#38745,
#38746,#38747,#38748,#38749,#38750,#38751,#38752,#38753,#38754,#38755,#38756,
#38757,#38758,#38759,#38760,#38761,#38762,#38763,#38764,#38765,#38766,#38767,
#38768,#38769,#38770,#38771,#38772,#38773,#38774,#38775,#38776,#38777,#38778,
#38779,#38780,#38781,#38782,#38783,#38784,#38785),.UNSPECIFIED.,.F.,.F.)
B_SPLINE_CURVE_WITH_KNOTS((6,1,1,1,1,1,1,1,1,1,1,1,1,1,1,1,1,1,1,1,1,1,
1,1,1,1,1,1,1,1,1,1,1,1,1,1,1,1,1,1,1,1,1,1,1,1,1,1,1,1,1,1,1,1,1,1,1,1,
1,1,1,1,1,1,1,6),(0.,0.0153846153846154,0.0307692307692308,0.0461538461538462,
0.0615384615384615,0.0769230769230769,0.0923076923076923,0.107692307692308,
0.123076923076923,0.138461538461538,0.153846153846154,0.169230769230769,
0.184615384615385,0.2,0.215384615384615,0.230769230769231,0.246153846153846,
0.261538461538462,0.276923076923077,0.292307692307692,0.307692307692308,
0.323076923076923,0.338461538461538,0.353846153846154,0.369230769230769,
0.384615384615385,0.4,0.415384615384615,0.430769230769231,0.446153846153846,
0.461538461538462,0.476923076923077,0.492307692307692,0.507692307692308,
0.523076923076923,0.538461538461538,0.553846153846154,0.569230769230769,
0.584615384615384,0.6,0.615384615384615,0.63076923076923,0.646153846153846,
0.661538461538461,0.676923076923076,0.692307692307692,0.707692307692307,
0.723076923076922,0.738461538461538,0.753846153846153,0.769230769230768,
0.784615384615384,0.799999999999999,0.815384615384614,0.83076923076923,
0.846153846153845,0.86153846153846,0.876923076923076,0.892307692307691,
0.907692307692306,0.923076923076922,0.938461538461537,0.953846153846152,
0.969230769230768,0.984615384615383,1.),.UNSPECIFIED.)
CURVE()
GEOMETRIC_REPRESENTATION_ITEM()
RATIONAL_B_SPLINE_CURVE((1.,1.,1.,1.,1.,1.,1.,1.,1.,1.,1.,1.,1.,1.,1.,1.,
1.,1.,1.,1.,1.,1.,1.,1.,1.,1.,1.,1.,1.,1.,1.,1.,1.,1.,1.,1.,1.,1.,1.,1.,
1.,1.,1.,1.,1.,1.,1.,1.,1.,1.,1.,1.,1.,1.,1.,1.,1.,1.,1.,1.,1.,1.,1.,1.,
1.,1.,1.,1.,1.,1.))
REPRESENTATION_ITEM('')
);
#266=(
BOUNDED_CURVE()
B_SPLINE_CURVE(5,(#38789,#38790,#38791,#38792,#38793,#38794,#38795,#38796,
#38797,#38798,#38799,#38800,#38801,#38802,#38803,#38804,#38805,#38806,#38807,
#38808,#38809,#38810,#38811,#38812,#38813,#38814,#38815,#38816,#38817,#38818,
#38819,#38820,#38821,#38822,#38823,#38824,#38825,#38826,#38827,#38828,#38829,
#38830,#38831,#38832,#38833,#38834,#38835,#38836,#38837,#38838,#38839,#38840,
#38841,#38842,#38843,#38844,#38845,#38846,#38847,#38848,#38849,#38850,#38851,
#38852,#38853,#38854,#38855,#38856,#38857,#38858),.UNSPECIFIED.,.F.,.F.)
B_SPLINE_CURVE_WITH_KNOTS((6,1,1,1,1,1,1,1,1,1,1,1,1,1,1,1,1,1,1,1,1,1,
1,1,1,1,1,1,1,1,1,1,1,1,1,1,1,1,1,1,1,1,1,1,1,1,1,1,1,1,1,1,1,1,1,1,1,1,
1,1,1,1,1,1,1,6),(0.,0.0153846153846154,0.0307692307692308,0.0461538461538462,
0.0615384615384615,0.0769230769230769,0.0923076923076923,0.107692307692308,
0.123076923076923,0.138461538461538,0.153846153846154,0.169230769230769,
0.184615384615385,0.2,0.215384615384615,0.230769230769231,0.246153846153846,
0.261538461538462,0.276923076923077,0.292307692307692,0.307692307692308,
0.323076923076923,0.338461538461538,0.353846153846154,0.369230769230769,
0.384615384615385,0.4,0.415384615384615,0.430769230769231,0.446153846153846,
0.461538461538462,0.476923076923077,0.492307692307692,0.507692307692308,
0.523076923076923,0.538461538461538,0.553846153846154,0.569230769230769,
0.584615384615384,0.6,0.615384615384615,0.63076923076923,0.646153846153846,
0.661538461538461,0.676923076923076,0.692307692307692,0.707692307692307,
0.723076923076922,0.738461538461538,0.753846153846153,0.769230769230768,
0.784615384615384,0.799999999999999,0.815384615384614,0.83076923076923,
0.846153846153845,0.86153846153846,0.876923076923076,0.892307692307691,
0.907692307692306,0.923076923076922,0.938461538461537,0.953846153846152,
0.969230769230768,0.984615384615383,1.),.UNSPECIFIED.)
CURVE()
GEOMETRIC_REPRESENTATION_ITEM()
RATIONAL_B_SPLINE_CURVE((1.,1.,1.,1.,1.,1.,1.,1.,1.,1.,1.,1.,1.,1.,1.,1.,
1.,1.,1.,1.,1.,1.,1.,1.,1.,1.,1.,1.,1.,1.,1.,1.,1.,1.,1.,1.,1.,1.,1.,1.,
1.,1.,1.,1.,1.,1.,1.,1.,1.,1.,1.,1.,1.,1.,1.,1.,1.,1.,1.,1.,1.,1.,1.,1.,
1.,1.,1.,1.,1.,1.))
REPRESENTATION_ITEM('')
);
#267=(
BOUNDED_CURVE()
B_SPLINE_CURVE(5,(#38862,#38863,#38864,#38865,#38866,#38867,#38868,#38869,
#38870,#38871,#38872,#38873,#38874,#38875,#38876,#38877,#38878,#38879,#38880,
#38881,#38882,#38883,#38884,#38885,#38886,#38887,#38888,#38889,#38890,#38891,
#38892,#38893,#38894,#38895,#38896,#38897,#38898,#38899,#38900,#38901,#38902,
#38903,#38904,#38905,#38906,#38907,#38908,#38909,#38910,#38911,#38912,#38913,
#38914,#38915,#38916,#38917,#38918,#38919,#38920,#38921,#38922,#38923,#38924,
#38925,#38926,#38927,#38928,#38929,#38930,#38931),.UNSPECIFIED.,.F.,.F.)
B_SPLINE_CURVE_WITH_KNOTS((6,1,1,1,1,1,1,1,1,1,1,1,1,1,1,1,1,1,1,1,1,1,
1,1,1,1,1,1,1,1,1,1,1,1,1,1,1,1,1,1,1,1,1,1,1,1,1,1,1,1,1,1,1,1,1,1,1,1,
1,1,1,1,1,1,1,6),(0.,0.0153846153846154,0.0307692307692308,0.0461538461538462,
0.0615384615384615,0.0769230769230769,0.0923076923076923,0.107692307692308,
0.123076923076923,0.138461538461538,0.153846153846154,0.169230769230769,
0.184615384615385,0.2,0.215384615384615,0.230769230769231,0.246153846153846,
0.261538461538462,0.276923076923077,0.292307692307692,0.307692307692308,
0.323076923076923,0.338461538461538,0.353846153846154,0.369230769230769,
0.384615384615385,0.4,0.415384615384615,0.430769230769231,0.446153846153846,
0.461538461538462,0.476923076923077,0.492307692307692,0.507692307692308,
0.523076923076923,0.538461538461538,0.553846153846154,0.569230769230769,
0.584615384615384,0.6,0.615384615384615,0.63076923076923,0.646153846153846,
0.661538461538461,0.676923076923076,0.692307692307692,0.707692307692307,
0.723076923076922,0.738461538461538,0.753846153846153,0.769230769230768,
0.784615384615384,0.799999999999999,0.815384615384614,0.83076923076923,
0.846153846153845,0.86153846153846,0.876923076923076,0.892307692307691,
0.907692307692306,0.923076923076922,0.938461538461537,0.953846153846152,
0.969230769230768,0.984615384615383,1.),.UNSPECIFIED.)
CURVE()
GEOMETRIC_REPRESENTATION_ITEM()
RATIONAL_B_SPLINE_CURVE((1.,1.,1.,1.,1.,1.,1.,1.,1.,1.,1.,1.,1.,1.,1.,1.,
1.,1.,1.,1.,1.,1.,1.,1.,1.,1.,1.,1.,1.,1.,1.,1.,1.,1.,1.,1.,1.,1.,1.,1.,
1.,1.,1.,1.,1.,1.,1.,1.,1.,1.,1.,1.,1.,1.,1.,1.,1.,1.,1.,1.,1.,1.,1.,1.,
1.,1.,1.,1.,1.,1.))
REPRESENTATION_ITEM('')
);
#268=(
BOUNDED_CURVE()
B_SPLINE_CURVE(5,(#38935,#38936,#38937,#38938,#38939,#38940,#38941,#38942,
#38943,#38944,#38945,#38946,#38947,#38948,#38949,#38950,#38951,#38952,#38953,
#38954,#38955,#38956,#38957,#38958,#38959,#38960,#38961,#38962,#38963,#38964,
#38965,#38966,#38967,#38968,#38969,#38970,#38971,#38972,#38973,#38974,#38975,
#38976,#38977,#38978,#38979,#38980,#38981,#38982,#38983,#38984,#38985,#38986,
#38987,#38988,#38989,#38990,#38991,#38992,#38993,#38994,#38995,#38996,#38997,
#38998,#38999,#39000,#39001,#39002,#39003,#39004),.UNSPECIFIED.,.F.,.F.)
B_SPLINE_CURVE_WITH_KNOTS((6,1,1,1,1,1,1,1,1,1,1,1,1,1,1,1,1,1,1,1,1,1,
1,1,1,1,1,1,1,1,1,1,1,1,1,1,1,1,1,1,1,1,1,1,1,1,1,1,1,1,1,1,1,1,1,1,1,1,
1,1,1,1,1,1,1,6),(0.,0.0153846153846154,0.0307692307692308,0.0461538461538462,
0.0615384615384615,0.0769230769230769,0.0923076923076923,0.107692307692308,
0.123076923076923,0.138461538461538,0.153846153846154,0.169230769230769,
0.184615384615385,0.2,0.215384615384615,0.230769230769231,0.246153846153846,
0.261538461538462,0.276923076923077,0.292307692307692,0.307692307692308,
0.323076923076923,0.338461538461538,0.353846153846154,0.369230769230769,
0.384615384615385,0.4,0.415384615384615,0.430769230769231,0.446153846153846,
0.461538461538462,0.476923076923077,0.492307692307692,0.507692307692308,
0.523076923076923,0.538461538461538,0.553846153846154,0.569230769230769,
0.584615384615384,0.6,0.615384615384615,0.63076923076923,0.646153846153846,
0.661538461538461,0.676923076923076,0.692307692307692,0.707692307692307,
0.723076923076922,0.738461538461538,0.753846153846153,0.769230769230768,
0.784615384615384,0.799999999999999,0.815384615384614,0.83076923076923,
0.846153846153845,0.86153846153846,0.876923076923076,0.892307692307691,
0.907692307692306,0.923076923076922,0.938461538461537,0.953846153846152,
0.969230769230768,0.984615384615383,1.),.UNSPECIFIED.)
CURVE()
GEOMETRIC_REPRESENTATION_ITEM()
RATIONAL_B_SPLINE_CURVE((1.,1.,1.,1.,1.,1.,1.,1.,1.,1.,1.,1.,1.,1.,1.,1.,
1.,1.,1.,1.,1.,1.,1.,1.,1.,1.,1.,1.,1.,1.,1.,1.,1.,1.,1.,1.,1.,1.,1.,1.,
1.,1.,1.,1.,1.,1.,1.,1.,1.,1.,1.,1.,1.,1.,1.,1.,1.,1.,1.,1.,1.,1.,1.,1.,
1.,1.,1.,1.,1.,1.))
REPRESENTATION_ITEM('')
);
#269=(
BOUNDED_CURVE()
B_SPLINE_CURVE(5,(#39008,#39009,#39010,#39011,#39012,#39013,#39014,#39015,
#39016,#39017,#39018,#39019,#39020,#39021,#39022,#39023,#39024,#39025,#39026,
#39027,#39028,#39029,#39030,#39031,#39032,#39033,#39034,#39035,#39036,#39037,
#39038,#39039,#39040,#39041,#39042,#39043,#39044,#39045,#39046,#39047,#39048,
#39049,#39050,#39051,#39052,#39053,#39054,#39055,#39056,#39057,#39058,#39059,
#39060,#39061,#39062,#39063,#39064,#39065,#39066,#39067,#39068,#39069,#39070,
#39071,#39072,#39073,#39074,#39075,#39076,#39077),.UNSPECIFIED.,.F.,.F.)
B_SPLINE_CURVE_WITH_KNOTS((6,1,1,1,1,1,1,1,1,1,1,1,1,1,1,1,1,1,1,1,1,1,
1,1,1,1,1,1,1,1,1,1,1,1,1,1,1,1,1,1,1,1,1,1,1,1,1,1,1,1,1,1,1,1,1,1,1,1,
1,1,1,1,1,1,1,6),(0.,0.0153846153846154,0.0307692307692308,0.0461538461538462,
0.0615384615384615,0.0769230769230769,0.0923076923076923,0.107692307692308,
0.123076923076923,0.138461538461538,0.153846153846154,0.169230769230769,
0.184615384615385,0.2,0.215384615384615,0.230769230769231,0.246153846153846,
0.261538461538462,0.276923076923077,0.292307692307692,0.307692307692308,
0.323076923076923,0.338461538461538,0.353846153846154,0.369230769230769,
0.384615384615385,0.4,0.415384615384615,0.430769230769231,0.446153846153846,
0.461538461538462,0.476923076923077,0.492307692307692,0.507692307692308,
0.523076923076923,0.538461538461538,0.553846153846154,0.569230769230769,
0.584615384615384,0.6,0.615384615384615,0.63076923076923,0.646153846153846,
0.661538461538461,0.676923076923076,0.692307692307692,0.707692307692307,
0.723076923076922,0.738461538461538,0.753846153846153,0.769230769230768,
0.784615384615384,0.799999999999999,0.815384615384614,0.83076923076923,
0.846153846153845,0.86153846153846,0.876923076923076,0.892307692307691,
0.907692307692306,0.923076923076922,0.938461538461537,0.953846153846152,
0.969230769230768,0.984615384615383,1.),.UNSPECIFIED.)
CURVE()
GEOMETRIC_REPRESENTATION_ITEM()
RATIONAL_B_SPLINE_CURVE((1.,1.,1.,1.,1.,1.,1.,1.,1.,1.,1.,1.,1.,1.,1.,1.,
1.,1.,1.,1.,1.,1.,1.,1.,1.,1.,1.,1.,1.,1.,1.,1.,1.,1.,1.,1.,1.,1.,1.,1.,
1.,1.,1.,1.,1.,1.,1.,1.,1.,1.,1.,1.,1.,1.,1.,1.,1.,1.,1.,1.,1.,1.,1.,1.,
1.,1.,1.,1.,1.,1.))
REPRESENTATION_ITEM('')
);
#270=(
BOUNDED_CURVE()
B_SPLINE_CURVE(5,(#39081,#39082,#39083,#39084,#39085,#39086,#39087,#39088,
#39089,#39090,#39091,#39092,#39093,#39094,#39095,#39096,#39097,#39098,#39099,
#39100,#39101,#39102,#39103,#39104,#39105,#39106,#39107,#39108,#39109,#39110,
#39111,#39112,#39113,#39114,#39115,#39116,#39117,#39118,#39119,#39120,#39121,
#39122,#39123,#39124,#39125,#39126,#39127,#39128,#39129,#39130,#39131,#39132,
#39133,#39134,#39135,#39136,#39137,#39138,#39139,#39140,#39141,#39142,#39143,
#39144,#39145,#39146,#39147,#39148,#39149,#39150),.UNSPECIFIED.,.F.,.F.)
B_SPLINE_CURVE_WITH_KNOTS((6,1,1,1,1,1,1,1,1,1,1,1,1,1,1,1,1,1,1,1,1,1,
1,1,1,1,1,1,1,1,1,1,1,1,1,1,1,1,1,1,1,1,1,1,1,1,1,1,1,1,1,1,1,1,1,1,1,1,
1,1,1,1,1,1,1,6),(0.,0.0153846153846154,0.0307692307692308,0.0461538461538462,
0.0615384615384615,0.0769230769230769,0.0923076923076923,0.107692307692308,
0.123076923076923,0.138461538461538,0.153846153846154,0.169230769230769,
0.184615384615385,0.2,0.215384615384615,0.230769230769231,0.246153846153846,
0.261538461538462,0.276923076923077,0.292307692307692,0.307692307692308,
0.323076923076923,0.338461538461538,0.353846153846154,0.369230769230769,
0.384615384615385,0.4,0.415384615384615,0.430769230769231,0.446153846153846,
0.461538461538462,0.476923076923077,0.492307692307692,0.507692307692308,
0.523076923076923,0.538461538461538,0.553846153846154,0.569230769230769,
0.584615384615384,0.6,0.615384615384615,0.63076923076923,0.646153846153846,
0.661538461538461,0.676923076923076,0.692307692307692,0.707692307692307,
0.723076923076922,0.738461538461538,0.753846153846153,0.769230769230768,
0.784615384615384,0.799999999999999,0.815384615384614,0.83076923076923,
0.846153846153845,0.86153846153846,0.876923076923076,0.892307692307691,
0.907692307692306,0.923076923076922,0.938461538461537,0.953846153846152,
0.969230769230768,0.984615384615383,1.),.UNSPECIFIED.)
CURVE()
GEOMETRIC_REPRESENTATION_ITEM()
RATIONAL_B_SPLINE_CURVE((1.,1.,1.,1.,1.,1.,1.,1.,1.,1.,1.,1.,1.,1.,1.,1.,
1.,1.,1.,1.,1.,1.,1.,1.,1.,1.,1.,1.,1.,1.,1.,1.,1.,1.,1.,1.,1.,1.,1.,1.,
1.,1.,1.,1.,1.,1.,1.,1.,1.,1.,1.,1.,1.,1.,1.,1.,1.,1.,1.,1.,1.,1.,1.,1.,
1.,1.,1.,1.,1.,1.))
REPRESENTATION_ITEM('')
);
#271=(
BOUNDED_CURVE()
B_SPLINE_CURVE(5,(#39154,#39155,#39156,#39157,#39158,#39159,#39160,#39161,
#39162,#39163,#39164,#39165,#39166,#39167,#39168,#39169,#39170,#39171,#39172,
#39173,#39174,#39175,#39176,#39177,#39178,#39179,#39180,#39181,#39182,#39183,
#39184,#39185,#39186,#39187,#39188,#39189,#39190,#39191,#39192,#39193,#39194,
#39195,#39196,#39197,#39198,#39199,#39200,#39201,#39202,#39203,#39204,#39205,
#39206,#39207,#39208,#39209,#39210,#39211,#39212,#39213,#39214,#39215,#39216,
#39217,#39218,#39219,#39220,#39221,#39222,#39223),.UNSPECIFIED.,.F.,.F.)
B_SPLINE_CURVE_WITH_KNOTS((6,1,1,1,1,1,1,1,1,1,1,1,1,1,1,1,1,1,1,1,1,1,
1,1,1,1,1,1,1,1,1,1,1,1,1,1,1,1,1,1,1,1,1,1,1,1,1,1,1,1,1,1,1,1,1,1,1,1,
1,1,1,1,1,1,1,6),(0.,0.0153846153846154,0.0307692307692308,0.0461538461538462,
0.0615384615384615,0.0769230769230769,0.0923076923076923,0.107692307692308,
0.123076923076923,0.138461538461538,0.153846153846154,0.169230769230769,
0.184615384615385,0.2,0.215384615384615,0.230769230769231,0.246153846153846,
0.261538461538462,0.276923076923077,0.292307692307692,0.307692307692308,
0.323076923076923,0.338461538461538,0.353846153846154,0.369230769230769,
0.384615384615385,0.4,0.415384615384615,0.430769230769231,0.446153846153846,
0.461538461538462,0.476923076923077,0.492307692307692,0.507692307692308,
0.523076923076923,0.538461538461538,0.553846153846154,0.569230769230769,
0.584615384615384,0.6,0.615384615384615,0.63076923076923,0.646153846153846,
0.661538461538461,0.676923076923076,0.692307692307692,0.707692307692307,
0.723076923076922,0.738461538461538,0.753846153846153,0.769230769230768,
0.784615384615384,0.799999999999999,0.815384615384614,0.83076923076923,
0.846153846153845,0.86153846153846,0.876923076923076,0.892307692307691,
0.907692307692306,0.923076923076922,0.938461538461537,0.953846153846152,
0.969230769230768,0.984615384615383,1.),.UNSPECIFIED.)
CURVE()
GEOMETRIC_REPRESENTATION_ITEM()
RATIONAL_B_SPLINE_CURVE((1.,1.,1.,1.,1.,1.,1.,1.,1.,1.,1.,1.,1.,1.,1.,1.,
1.,1.,1.,1.,1.,1.,1.,1.,1.,1.,1.,1.,1.,1.,1.,1.,1.,1.,1.,1.,1.,1.,1.,1.,
1.,1.,1.,1.,1.,1.,1.,1.,1.,1.,1.,1.,1.,1.,1.,1.,1.,1.,1.,1.,1.,1.,1.,1.,
1.,1.,1.,1.,1.,1.))
REPRESENTATION_ITEM('')
);
#272=(
BOUNDED_CURVE()
B_SPLINE_CURVE(5,(#39227,#39228,#39229,#39230,#39231,#39232,#39233,#39234,
#39235,#39236,#39237,#39238,#39239,#39240,#39241,#39242,#39243,#39244,#39245,
#39246,#39247,#39248,#39249,#39250,#39251,#39252,#39253,#39254,#39255,#39256,
#39257,#39258,#39259,#39260,#39261,#39262,#39263,#39264,#39265,#39266,#39267,
#39268,#39269,#39270,#39271,#39272,#39273,#39274,#39275,#39276,#39277,#39278,
#39279,#39280,#39281,#39282,#39283,#39284,#39285,#39286,#39287,#39288,#39289,
#39290,#39291,#39292,#39293,#39294,#39295,#39296),.UNSPECIFIED.,.F.,.F.)
B_SPLINE_CURVE_WITH_KNOTS((6,1,1,1,1,1,1,1,1,1,1,1,1,1,1,1,1,1,1,1,1,1,
1,1,1,1,1,1,1,1,1,1,1,1,1,1,1,1,1,1,1,1,1,1,1,1,1,1,1,1,1,1,1,1,1,1,1,1,
1,1,1,1,1,1,1,6),(0.,0.0153846153846154,0.0307692307692308,0.0461538461538462,
0.0615384615384615,0.0769230769230769,0.0923076923076923,0.107692307692308,
0.123076923076923,0.138461538461538,0.153846153846154,0.169230769230769,
0.184615384615385,0.2,0.215384615384615,0.230769230769231,0.246153846153846,
0.261538461538462,0.276923076923077,0.292307692307692,0.307692307692308,
0.323076923076923,0.338461538461538,0.353846153846154,0.369230769230769,
0.384615384615385,0.4,0.415384615384615,0.430769230769231,0.446153846153846,
0.461538461538462,0.476923076923077,0.492307692307692,0.507692307692308,
0.523076923076923,0.538461538461538,0.553846153846154,0.569230769230769,
0.584615384615384,0.6,0.615384615384615,0.63076923076923,0.646153846153846,
0.661538461538461,0.676923076923076,0.692307692307692,0.707692307692307,
0.723076923076922,0.738461538461538,0.753846153846153,0.769230769230768,
0.784615384615384,0.799999999999999,0.815384615384614,0.83076923076923,
0.846153846153845,0.86153846153846,0.876923076923076,0.892307692307691,
0.907692307692306,0.923076923076922,0.938461538461537,0.953846153846152,
0.969230769230768,0.984615384615383,1.),.UNSPECIFIED.)
CURVE()
GEOMETRIC_REPRESENTATION_ITEM()
RATIONAL_B_SPLINE_CURVE((1.,1.,1.,1.,1.,1.,1.,1.,1.,1.,1.,1.,1.,1.,1.,1.,
1.,1.,1.,1.,1.,1.,1.,1.,1.,1.,1.,1.,1.,1.,1.,1.,1.,1.,1.,1.,1.,1.,1.,1.,
1.,1.,1.,1.,1.,1.,1.,1.,1.,1.,1.,1.,1.,1.,1.,1.,1.,1.,1.,1.,1.,1.,1.,1.,
1.,1.,1.,1.,1.,1.))
REPRESENTATION_ITEM('')
);
#273=(
BOUNDED_CURVE()
B_SPLINE_CURVE(5,(#39300,#39301,#39302,#39303,#39304,#39305,#39306,#39307,
#39308,#39309,#39310,#39311,#39312,#39313,#39314,#39315,#39316,#39317,#39318,
#39319,#39320,#39321,#39322,#39323,#39324,#39325,#39326,#39327,#39328,#39329,
#39330,#39331,#39332,#39333,#39334,#39335,#39336,#39337,#39338,#39339,#39340,
#39341,#39342,#39343,#39344,#39345,#39346,#39347,#39348,#39349,#39350,#39351,
#39352,#39353,#39354,#39355,#39356,#39357,#39358,#39359,#39360,#39361,#39362,
#39363,#39364,#39365,#39366,#39367,#39368,#39369),.UNSPECIFIED.,.F.,.F.)
B_SPLINE_CURVE_WITH_KNOTS((6,1,1,1,1,1,1,1,1,1,1,1,1,1,1,1,1,1,1,1,1,1,
1,1,1,1,1,1,1,1,1,1,1,1,1,1,1,1,1,1,1,1,1,1,1,1,1,1,1,1,1,1,1,1,1,1,1,1,
1,1,1,1,1,1,1,6),(0.,0.0153846153846154,0.0307692307692308,0.0461538461538462,
0.0615384615384615,0.0769230769230769,0.0923076923076923,0.107692307692308,
0.123076923076923,0.138461538461538,0.153846153846154,0.169230769230769,
0.184615384615385,0.2,0.215384615384615,0.230769230769231,0.246153846153846,
0.261538461538462,0.276923076923077,0.292307692307692,0.307692307692308,
0.323076923076923,0.338461538461538,0.353846153846154,0.369230769230769,
0.384615384615385,0.4,0.415384615384615,0.430769230769231,0.446153846153846,
0.461538461538462,0.476923076923077,0.492307692307692,0.507692307692308,
0.523076923076923,0.538461538461538,0.553846153846154,0.569230769230769,
0.584615384615384,0.6,0.615384615384615,0.63076923076923,0.646153846153846,
0.661538461538461,0.676923076923076,0.692307692307692,0.707692307692307,
0.723076923076922,0.738461538461538,0.753846153846153,0.769230769230768,
0.784615384615384,0.799999999999999,0.815384615384614,0.83076923076923,
0.846153846153845,0.86153846153846,0.876923076923076,0.892307692307691,
0.907692307692306,0.923076923076922,0.938461538461537,0.953846153846152,
0.969230769230768,0.984615384615383,1.),.UNSPECIFIED.)
CURVE()
GEOMETRIC_REPRESENTATION_ITEM()
RATIONAL_B_SPLINE_CURVE((1.,1.,1.,1.,1.,1.,1.,1.,1.,1.,1.,1.,1.,1.,1.,1.,
1.,1.,1.,1.,1.,1.,1.,1.,1.,1.,1.,1.,1.,1.,1.,1.,1.,1.,1.,1.,1.,1.,1.,1.,
1.,1.,1.,1.,1.,1.,1.,1.,1.,1.,1.,1.,1.,1.,1.,1.,1.,1.,1.,1.,1.,1.,1.,1.,
1.,1.,1.,1.,1.,1.))
REPRESENTATION_ITEM('')
);
#274=(
BOUNDED_CURVE()
B_SPLINE_CURVE(5,(#39373,#39374,#39375,#39376,#39377,#39378,#39379,#39380,
#39381,#39382,#39383,#39384,#39385,#39386,#39387,#39388,#39389,#39390,#39391,
#39392,#39393,#39394,#39395,#39396,#39397,#39398,#39399,#39400,#39401,#39402,
#39403,#39404,#39405,#39406,#39407,#39408,#39409,#39410,#39411,#39412,#39413,
#39414,#39415,#39416,#39417,#39418,#39419,#39420,#39421,#39422,#39423,#39424,
#39425,#39426,#39427,#39428,#39429,#39430,#39431,#39432,#39433,#39434,#39435,
#39436,#39437,#39438,#39439,#39440,#39441,#39442),.UNSPECIFIED.,.F.,.F.)
B_SPLINE_CURVE_WITH_KNOTS((6,1,1,1,1,1,1,1,1,1,1,1,1,1,1,1,1,1,1,1,1,1,
1,1,1,1,1,1,1,1,1,1,1,1,1,1,1,1,1,1,1,1,1,1,1,1,1,1,1,1,1,1,1,1,1,1,1,1,
1,1,1,1,1,1,1,6),(0.,0.0153846153846154,0.0307692307692308,0.0461538461538462,
0.0615384615384615,0.0769230769230769,0.0923076923076923,0.107692307692308,
0.123076923076923,0.138461538461538,0.153846153846154,0.169230769230769,
0.184615384615385,0.2,0.215384615384615,0.230769230769231,0.246153846153846,
0.261538461538462,0.276923076923077,0.292307692307692,0.307692307692308,
0.323076923076923,0.338461538461538,0.353846153846154,0.369230769230769,
0.384615384615385,0.4,0.415384615384615,0.430769230769231,0.446153846153846,
0.461538461538462,0.476923076923077,0.492307692307692,0.507692307692308,
0.523076923076923,0.538461538461538,0.553846153846154,0.569230769230769,
0.584615384615384,0.6,0.615384615384615,0.63076923076923,0.646153846153846,
0.661538461538461,0.676923076923076,0.692307692307692,0.707692307692307,
0.723076923076922,0.738461538461538,0.753846153846153,0.769230769230768,
0.784615384615384,0.799999999999999,0.815384615384614,0.83076923076923,
0.846153846153845,0.86153846153846,0.876923076923076,0.892307692307691,
0.907692307692306,0.923076923076922,0.938461538461537,0.953846153846152,
0.969230769230768,0.984615384615383,1.),.UNSPECIFIED.)
CURVE()
GEOMETRIC_REPRESENTATION_ITEM()
RATIONAL_B_SPLINE_CURVE((1.,1.,1.,1.,1.,1.,1.,1.,1.,1.,1.,1.,1.,1.,1.,1.,
1.,1.,1.,1.,1.,1.,1.,1.,1.,1.,1.,1.,1.,1.,1.,1.,1.,1.,1.,1.,1.,1.,1.,1.,
1.,1.,1.,1.,1.,1.,1.,1.,1.,1.,1.,1.,1.,1.,1.,1.,1.,1.,1.,1.,1.,1.,1.,1.,
1.,1.,1.,1.,1.,1.))
REPRESENTATION_ITEM('')
);
#275=(
BOUNDED_CURVE()
B_SPLINE_CURVE(5,(#39446,#39447,#39448,#39449,#39450,#39451,#39452,#39453,
#39454,#39455,#39456,#39457,#39458,#39459,#39460,#39461,#39462,#39463,#39464,
#39465,#39466,#39467,#39468,#39469,#39470,#39471,#39472,#39473,#39474,#39475,
#39476,#39477,#39478,#39479,#39480,#39481,#39482,#39483,#39484,#39485,#39486,
#39487,#39488,#39489,#39490,#39491,#39492,#39493,#39494,#39495,#39496,#39497,
#39498,#39499,#39500,#39501,#39502,#39503,#39504,#39505,#39506,#39507,#39508,
#39509,#39510,#39511,#39512,#39513,#39514,#39515),.UNSPECIFIED.,.F.,.F.)
B_SPLINE_CURVE_WITH_KNOTS((6,1,1,1,1,1,1,1,1,1,1,1,1,1,1,1,1,1,1,1,1,1,
1,1,1,1,1,1,1,1,1,1,1,1,1,1,1,1,1,1,1,1,1,1,1,1,1,1,1,1,1,1,1,1,1,1,1,1,
1,1,1,1,1,1,1,6),(0.,0.0153846153846154,0.0307692307692308,0.0461538461538462,
0.0615384615384615,0.0769230769230769,0.0923076923076923,0.107692307692308,
0.123076923076923,0.138461538461538,0.153846153846154,0.169230769230769,
0.184615384615385,0.2,0.215384615384615,0.230769230769231,0.246153846153846,
0.261538461538462,0.276923076923077,0.292307692307692,0.307692307692308,
0.323076923076923,0.338461538461538,0.353846153846154,0.369230769230769,
0.384615384615385,0.4,0.415384615384615,0.430769230769231,0.446153846153846,
0.461538461538462,0.476923076923077,0.492307692307692,0.507692307692308,
0.523076923076923,0.538461538461538,0.553846153846154,0.569230769230769,
0.584615384615384,0.6,0.615384615384615,0.63076923076923,0.646153846153846,
0.661538461538461,0.676923076923076,0.692307692307692,0.707692307692307,
0.723076923076922,0.738461538461538,0.753846153846153,0.769230769230768,
0.784615384615384,0.799999999999999,0.815384615384614,0.83076923076923,
0.846153846153845,0.86153846153846,0.876923076923076,0.892307692307691,
0.907692307692306,0.923076923076922,0.938461538461537,0.953846153846152,
0.969230769230768,0.984615384615383,1.),.UNSPECIFIED.)
CURVE()
GEOMETRIC_REPRESENTATION_ITEM()
RATIONAL_B_SPLINE_CURVE((1.,1.,1.,1.,1.,1.,1.,1.,1.,1.,1.,1.,1.,1.,1.,1.,
1.,1.,1.,1.,1.,1.,1.,1.,1.,1.,1.,1.,1.,1.,1.,1.,1.,1.,1.,1.,1.,1.,1.,1.,
1.,1.,1.,1.,1.,1.,1.,1.,1.,1.,1.,1.,1.,1.,1.,1.,1.,1.,1.,1.,1.,1.,1.,1.,
1.,1.,1.,1.,1.,1.))
REPRESENTATION_ITEM('')
);
#276=(
BOUNDED_CURVE()
B_SPLINE_CURVE(5,(#39519,#39520,#39521,#39522,#39523,#39524,#39525,#39526,
#39527,#39528,#39529,#39530,#39531,#39532,#39533,#39534,#39535,#39536,#39537,
#39538,#39539,#39540,#39541,#39542,#39543,#39544,#39545,#39546,#39547,#39548,
#39549,#39550,#39551,#39552,#39553,#39554,#39555,#39556,#39557,#39558,#39559,
#39560,#39561,#39562,#39563,#39564,#39565,#39566,#39567,#39568,#39569,#39570,
#39571,#39572,#39573,#39574,#39575,#39576,#39577,#39578,#39579,#39580,#39581,
#39582,#39583,#39584,#39585,#39586,#39587,#39588),.UNSPECIFIED.,.F.,.F.)
B_SPLINE_CURVE_WITH_KNOTS((6,1,1,1,1,1,1,1,1,1,1,1,1,1,1,1,1,1,1,1,1,1,
1,1,1,1,1,1,1,1,1,1,1,1,1,1,1,1,1,1,1,1,1,1,1,1,1,1,1,1,1,1,1,1,1,1,1,1,
1,1,1,1,1,1,1,6),(0.,0.0153846153846154,0.0307692307692308,0.0461538461538462,
0.0615384615384615,0.0769230769230769,0.0923076923076923,0.107692307692308,
0.123076923076923,0.138461538461538,0.153846153846154,0.169230769230769,
0.184615384615385,0.2,0.215384615384615,0.230769230769231,0.246153846153846,
0.261538461538462,0.276923076923077,0.292307692307692,0.307692307692308,
0.323076923076923,0.338461538461538,0.353846153846154,0.369230769230769,
0.384615384615385,0.4,0.415384615384615,0.430769230769231,0.446153846153846,
0.461538461538462,0.476923076923077,0.492307692307692,0.507692307692308,
0.523076923076923,0.538461538461538,0.553846153846154,0.569230769230769,
0.584615384615384,0.6,0.615384615384615,0.63076923076923,0.646153846153846,
0.661538461538461,0.676923076923076,0.692307692307692,0.707692307692307,
0.723076923076922,0.738461538461538,0.753846153846153,0.769230769230768,
0.784615384615384,0.799999999999999,0.815384615384614,0.83076923076923,
0.846153846153845,0.86153846153846,0.876923076923076,0.892307692307691,
0.907692307692306,0.923076923076922,0.938461538461537,0.953846153846152,
0.969230769230768,0.984615384615383,1.),.UNSPECIFIED.)
CURVE()
GEOMETRIC_REPRESENTATION_ITEM()
RATIONAL_B_SPLINE_CURVE((1.,1.,1.,1.,1.,1.,1.,1.,1.,1.,1.,1.,1.,1.,1.,1.,
1.,1.,1.,1.,1.,1.,1.,1.,1.,1.,1.,1.,1.,1.,1.,1.,1.,1.,1.,1.,1.,1.,1.,1.,
1.,1.,1.,1.,1.,1.,1.,1.,1.,1.,1.,1.,1.,1.,1.,1.,1.,1.,1.,1.,1.,1.,1.,1.,
1.,1.,1.,1.,1.,1.))
REPRESENTATION_ITEM('')
);
#277=(
BOUNDED_CURVE()
B_SPLINE_CURVE(5,(#39592,#39593,#39594,#39595,#39596,#39597,#39598,#39599,
#39600,#39601,#39602,#39603,#39604,#39605,#39606,#39607,#39608,#39609,#39610,
#39611,#39612,#39613,#39614,#39615,#39616,#39617,#39618,#39619,#39620,#39621,
#39622,#39623,#39624,#39625,#39626,#39627,#39628,#39629,#39630,#39631,#39632,
#39633,#39634,#39635,#39636,#39637,#39638,#39639,#39640,#39641,#39642,#39643,
#39644,#39645,#39646,#39647,#39648,#39649,#39650,#39651,#39652,#39653,#39654,
#39655,#39656,#39657,#39658,#39659,#39660,#39661),.UNSPECIFIED.,.F.,.F.)
B_SPLINE_CURVE_WITH_KNOTS((6,1,1,1,1,1,1,1,1,1,1,1,1,1,1,1,1,1,1,1,1,1,
1,1,1,1,1,1,1,1,1,1,1,1,1,1,1,1,1,1,1,1,1,1,1,1,1,1,1,1,1,1,1,1,1,1,1,1,
1,1,1,1,1,1,1,6),(0.,0.0153846153846154,0.0307692307692308,0.0461538461538462,
0.0615384615384615,0.0769230769230769,0.0923076923076923,0.107692307692308,
0.123076923076923,0.138461538461538,0.153846153846154,0.169230769230769,
0.184615384615385,0.2,0.215384615384615,0.230769230769231,0.246153846153846,
0.261538461538462,0.276923076923077,0.292307692307692,0.307692307692308,
0.323076923076923,0.338461538461538,0.353846153846154,0.369230769230769,
0.384615384615385,0.4,0.415384615384615,0.430769230769231,0.446153846153846,
0.461538461538462,0.476923076923077,0.492307692307692,0.507692307692308,
0.523076923076923,0.538461538461538,0.553846153846154,0.569230769230769,
0.584615384615384,0.6,0.615384615384615,0.63076923076923,0.646153846153846,
0.661538461538461,0.676923076923076,0.692307692307692,0.707692307692307,
0.723076923076922,0.738461538461538,0.753846153846153,0.769230769230768,
0.784615384615384,0.799999999999999,0.815384615384614,0.83076923076923,
0.846153846153845,0.86153846153846,0.876923076923076,0.892307692307691,
0.907692307692306,0.923076923076922,0.938461538461537,0.953846153846152,
0.969230769230768,0.984615384615383,1.),.UNSPECIFIED.)
CURVE()
GEOMETRIC_REPRESENTATION_ITEM()
RATIONAL_B_SPLINE_CURVE((1.,1.,1.,1.,1.,1.,1.,1.,1.,1.,1.,1.,1.,1.,1.,1.,
1.,1.,1.,1.,1.,1.,1.,1.,1.,1.,1.,1.,1.,1.,1.,1.,1.,1.,1.,1.,1.,1.,1.,1.,
1.,1.,1.,1.,1.,1.,1.,1.,1.,1.,1.,1.,1.,1.,1.,1.,1.,1.,1.,1.,1.,1.,1.,1.,
1.,1.,1.,1.,1.,1.))
REPRESENTATION_ITEM('')
);
#278=(
BOUNDED_CURVE()
B_SPLINE_CURVE(5,(#39665,#39666,#39667,#39668,#39669,#39670,#39671,#39672,
#39673,#39674,#39675,#39676,#39677,#39678,#39679,#39680,#39681,#39682,#39683,
#39684,#39685,#39686,#39687,#39688,#39689,#39690,#39691,#39692,#39693,#39694,
#39695,#39696,#39697,#39698,#39699,#39700,#39701,#39702,#39703,#39704,#39705,
#39706,#39707,#39708,#39709,#39710,#39711,#39712,#39713,#39714,#39715,#39716,
#39717,#39718,#39719,#39720,#39721,#39722,#39723,#39724,#39725,#39726,#39727,
#39728,#39729,#39730,#39731,#39732,#39733,#39734),.UNSPECIFIED.,.F.,.F.)
B_SPLINE_CURVE_WITH_KNOTS((6,1,1,1,1,1,1,1,1,1,1,1,1,1,1,1,1,1,1,1,1,1,
1,1,1,1,1,1,1,1,1,1,1,1,1,1,1,1,1,1,1,1,1,1,1,1,1,1,1,1,1,1,1,1,1,1,1,1,
1,1,1,1,1,1,1,6),(0.,0.0153846153846154,0.0307692307692308,0.0461538461538462,
0.0615384615384615,0.0769230769230769,0.0923076923076923,0.107692307692308,
0.123076923076923,0.138461538461538,0.153846153846154,0.169230769230769,
0.184615384615385,0.2,0.215384615384615,0.230769230769231,0.246153846153846,
0.261538461538462,0.276923076923077,0.292307692307692,0.307692307692308,
0.323076923076923,0.338461538461538,0.353846153846154,0.369230769230769,
0.384615384615385,0.4,0.415384615384615,0.430769230769231,0.446153846153846,
0.461538461538462,0.476923076923077,0.492307692307692,0.507692307692308,
0.523076923076923,0.538461538461538,0.553846153846154,0.569230769230769,
0.584615384615384,0.6,0.615384615384615,0.63076923076923,0.646153846153846,
0.661538461538461,0.676923076923076,0.692307692307692,0.707692307692307,
0.723076923076922,0.738461538461538,0.753846153846153,0.769230769230768,
0.784615384615384,0.799999999999999,0.815384615384614,0.83076923076923,
0.846153846153845,0.86153846153846,0.876923076923076,0.892307692307691,
0.907692307692306,0.923076923076922,0.938461538461537,0.953846153846152,
0.969230769230768,0.984615384615383,1.),.UNSPECIFIED.)
CURVE()
GEOMETRIC_REPRESENTATION_ITEM()
RATIONAL_B_SPLINE_CURVE((1.,1.,1.,1.,1.,1.,1.,1.,1.,1.,1.,1.,1.,1.,1.,1.,
1.,1.,1.,1.,1.,1.,1.,1.,1.,1.,1.,1.,1.,1.,1.,1.,1.,1.,1.,1.,1.,1.,1.,1.,
1.,1.,1.,1.,1.,1.,1.,1.,1.,1.,1.,1.,1.,1.,1.,1.,1.,1.,1.,1.,1.,1.,1.,1.,
1.,1.,1.,1.,1.,1.))
REPRESENTATION_ITEM('')
);
#279=(
BOUNDED_CURVE()
B_SPLINE_CURVE(5,(#39738,#39739,#39740,#39741,#39742,#39743,#39744,#39745,
#39746,#39747,#39748,#39749,#39750,#39751,#39752,#39753,#39754,#39755,#39756,
#39757,#39758,#39759,#39760,#39761,#39762,#39763,#39764,#39765,#39766,#39767,
#39768,#39769,#39770,#39771,#39772,#39773,#39774,#39775,#39776,#39777,#39778,
#39779,#39780,#39781,#39782,#39783,#39784,#39785,#39786,#39787,#39788,#39789,
#39790,#39791,#39792,#39793,#39794,#39795,#39796,#39797,#39798,#39799,#39800,
#39801,#39802,#39803,#39804,#39805,#39806,#39807),.UNSPECIFIED.,.F.,.F.)
B_SPLINE_CURVE_WITH_KNOTS((6,1,1,1,1,1,1,1,1,1,1,1,1,1,1,1,1,1,1,1,1,1,
1,1,1,1,1,1,1,1,1,1,1,1,1,1,1,1,1,1,1,1,1,1,1,1,1,1,1,1,1,1,1,1,1,1,1,1,
1,1,1,1,1,1,1,6),(0.,0.0153846153846154,0.0307692307692308,0.0461538461538462,
0.0615384615384615,0.0769230769230769,0.0923076923076923,0.107692307692308,
0.123076923076923,0.138461538461538,0.153846153846154,0.169230769230769,
0.184615384615385,0.2,0.215384615384615,0.230769230769231,0.246153846153846,
0.261538461538462,0.276923076923077,0.292307692307692,0.307692307692308,
0.323076923076923,0.338461538461538,0.353846153846154,0.369230769230769,
0.384615384615385,0.4,0.415384615384615,0.430769230769231,0.446153846153846,
0.461538461538462,0.476923076923077,0.492307692307692,0.507692307692308,
0.523076923076923,0.538461538461538,0.553846153846154,0.569230769230769,
0.584615384615384,0.6,0.615384615384615,0.63076923076923,0.646153846153846,
0.661538461538461,0.676923076923076,0.692307692307692,0.707692307692307,
0.723076923076922,0.738461538461538,0.753846153846153,0.769230769230768,
0.784615384615384,0.799999999999999,0.815384615384614,0.83076923076923,
0.846153846153845,0.86153846153846,0.876923076923076,0.892307692307691,
0.907692307692306,0.923076923076922,0.938461538461537,0.953846153846152,
0.969230769230768,0.984615384615383,1.),.UNSPECIFIED.)
CURVE()
GEOMETRIC_REPRESENTATION_ITEM()
RATIONAL_B_SPLINE_CURVE((1.,1.,1.,1.,1.,1.,1.,1.,1.,1.,1.,1.,1.,1.,1.,1.,
1.,1.,1.,1.,1.,1.,1.,1.,1.,1.,1.,1.,1.,1.,1.,1.,1.,1.,1.,1.,1.,1.,1.,1.,
1.,1.,1.,1.,1.,1.,1.,1.,1.,1.,1.,1.,1.,1.,1.,1.,1.,1.,1.,1.,1.,1.,1.,1.,
1.,1.,1.,1.,1.,1.))
REPRESENTATION_ITEM('')
);
#280=(
BOUNDED_CURVE()
B_SPLINE_CURVE(5,(#39811,#39812,#39813,#39814,#39815,#39816,#39817,#39818,
#39819,#39820,#39821,#39822,#39823,#39824,#39825,#39826,#39827,#39828,#39829,
#39830,#39831,#39832,#39833,#39834,#39835,#39836,#39837,#39838,#39839,#39840,
#39841,#39842,#39843,#39844,#39845,#39846,#39847,#39848,#39849,#39850,#39851,
#39852,#39853,#39854,#39855,#39856,#39857,#39858,#39859,#39860,#39861,#39862,
#39863,#39864,#39865,#39866,#39867,#39868,#39869,#39870,#39871,#39872,#39873,
#39874,#39875,#39876,#39877,#39878,#39879,#39880),.UNSPECIFIED.,.F.,.F.)
B_SPLINE_CURVE_WITH_KNOTS((6,1,1,1,1,1,1,1,1,1,1,1,1,1,1,1,1,1,1,1,1,1,
1,1,1,1,1,1,1,1,1,1,1,1,1,1,1,1,1,1,1,1,1,1,1,1,1,1,1,1,1,1,1,1,1,1,1,1,
1,1,1,1,1,1,1,6),(0.,0.0153846153846154,0.0307692307692308,0.0461538461538462,
0.0615384615384615,0.0769230769230769,0.0923076923076923,0.107692307692308,
0.123076923076923,0.138461538461538,0.153846153846154,0.169230769230769,
0.184615384615385,0.2,0.215384615384615,0.230769230769231,0.246153846153846,
0.261538461538462,0.276923076923077,0.292307692307692,0.307692307692308,
0.323076923076923,0.338461538461538,0.353846153846154,0.369230769230769,
0.384615384615385,0.4,0.415384615384615,0.430769230769231,0.446153846153846,
0.461538461538462,0.476923076923077,0.492307692307692,0.507692307692308,
0.523076923076923,0.538461538461538,0.553846153846154,0.569230769230769,
0.584615384615384,0.6,0.615384615384615,0.63076923076923,0.646153846153846,
0.661538461538461,0.676923076923076,0.692307692307692,0.707692307692307,
0.723076923076922,0.738461538461538,0.753846153846153,0.769230769230768,
0.784615384615384,0.799999999999999,0.815384615384614,0.83076923076923,
0.846153846153845,0.86153846153846,0.876923076923076,0.892307692307691,
0.907692307692306,0.923076923076922,0.938461538461537,0.953846153846152,
0.969230769230768,0.984615384615383,1.),.UNSPECIFIED.)
CURVE()
GEOMETRIC_REPRESENTATION_ITEM()
RATIONAL_B_SPLINE_CURVE((1.,1.,1.,1.,1.,1.,1.,1.,1.,1.,1.,1.,1.,1.,1.,1.,
1.,1.,1.,1.,1.,1.,1.,1.,1.,1.,1.,1.,1.,1.,1.,1.,1.,1.,1.,1.,1.,1.,1.,1.,
1.,1.,1.,1.,1.,1.,1.,1.,1.,1.,1.,1.,1.,1.,1.,1.,1.,1.,1.,1.,1.,1.,1.,1.,
1.,1.,1.,1.,1.,1.))
REPRESENTATION_ITEM('')
);
#281=(
BOUNDED_CURVE()
B_SPLINE_CURVE(5,(#39884,#39885,#39886,#39887,#39888,#39889,#39890,#39891,
#39892,#39893,#39894,#39895,#39896,#39897,#39898,#39899,#39900,#39901,#39902,
#39903,#39904,#39905,#39906,#39907,#39908,#39909,#39910,#39911,#39912,#39913,
#39914,#39915,#39916,#39917,#39918,#39919,#39920,#39921,#39922,#39923,#39924,
#39925,#39926,#39927,#39928,#39929,#39930,#39931,#39932,#39933,#39934,#39935,
#39936,#39937,#39938,#39939,#39940,#39941,#39942,#39943,#39944,#39945,#39946,
#39947,#39948,#39949,#39950,#39951,#39952,#39953),.UNSPECIFIED.,.F.,.F.)
B_SPLINE_CURVE_WITH_KNOTS((6,1,1,1,1,1,1,1,1,1,1,1,1,1,1,1,1,1,1,1,1,1,
1,1,1,1,1,1,1,1,1,1,1,1,1,1,1,1,1,1,1,1,1,1,1,1,1,1,1,1,1,1,1,1,1,1,1,1,
1,1,1,1,1,1,1,6),(0.,0.0153846153846154,0.0307692307692308,0.0461538461538462,
0.0615384615384615,0.0769230769230769,0.0923076923076923,0.107692307692308,
0.123076923076923,0.138461538461538,0.153846153846154,0.169230769230769,
0.184615384615385,0.2,0.215384615384615,0.230769230769231,0.246153846153846,
0.261538461538462,0.276923076923077,0.292307692307692,0.307692307692308,
0.323076923076923,0.338461538461538,0.353846153846154,0.369230769230769,
0.384615384615385,0.4,0.415384615384615,0.430769230769231,0.446153846153846,
0.461538461538462,0.476923076923077,0.492307692307692,0.507692307692308,
0.523076923076923,0.538461538461538,0.553846153846154,0.569230769230769,
0.584615384615384,0.6,0.615384615384615,0.63076923076923,0.646153846153846,
0.661538461538461,0.676923076923076,0.692307692307692,0.707692307692307,
0.723076923076922,0.738461538461538,0.753846153846153,0.769230769230768,
0.784615384615384,0.799999999999999,0.815384615384614,0.83076923076923,
0.846153846153845,0.86153846153846,0.876923076923076,0.892307692307691,
0.907692307692306,0.923076923076922,0.938461538461537,0.953846153846152,
0.969230769230768,0.984615384615383,1.),.UNSPECIFIED.)
CURVE()
GEOMETRIC_REPRESENTATION_ITEM()
RATIONAL_B_SPLINE_CURVE((1.,1.,1.,1.,1.,1.,1.,1.,1.,1.,1.,1.,1.,1.,1.,1.,
1.,1.,1.,1.,1.,1.,1.,1.,1.,1.,1.,1.,1.,1.,1.,1.,1.,1.,1.,1.,1.,1.,1.,1.,
1.,1.,1.,1.,1.,1.,1.,1.,1.,1.,1.,1.,1.,1.,1.,1.,1.,1.,1.,1.,1.,1.,1.,1.,
1.,1.,1.,1.,1.,1.))
REPRESENTATION_ITEM('')
);
#282=(
BOUNDED_CURVE()
B_SPLINE_CURVE(5,(#39957,#39958,#39959,#39960,#39961,#39962,#39963,#39964,
#39965,#39966,#39967,#39968,#39969,#39970,#39971,#39972,#39973,#39974,#39975,
#39976,#39977,#39978,#39979,#39980,#39981,#39982,#39983,#39984,#39985,#39986,
#39987,#39988,#39989,#39990,#39991,#39992,#39993,#39994,#39995,#39996,#39997,
#39998,#39999,#40000,#40001,#40002,#40003,#40004,#40005,#40006,#40007,#40008,
#40009,#40010,#40011,#40012,#40013,#40014,#40015,#40016,#40017,#40018,#40019,
#40020,#40021,#40022,#40023,#40024,#40025,#40026),.UNSPECIFIED.,.F.,.F.)
B_SPLINE_CURVE_WITH_KNOTS((6,1,1,1,1,1,1,1,1,1,1,1,1,1,1,1,1,1,1,1,1,1,
1,1,1,1,1,1,1,1,1,1,1,1,1,1,1,1,1,1,1,1,1,1,1,1,1,1,1,1,1,1,1,1,1,1,1,1,
1,1,1,1,1,1,1,6),(0.,0.0153846153846154,0.0307692307692308,0.0461538461538462,
0.0615384615384615,0.0769230769230769,0.0923076923076923,0.107692307692308,
0.123076923076923,0.138461538461538,0.153846153846154,0.169230769230769,
0.184615384615385,0.2,0.215384615384615,0.230769230769231,0.246153846153846,
0.261538461538462,0.276923076923077,0.292307692307692,0.307692307692308,
0.323076923076923,0.338461538461538,0.353846153846154,0.369230769230769,
0.384615384615385,0.4,0.415384615384615,0.430769230769231,0.446153846153846,
0.461538461538462,0.476923076923077,0.492307692307692,0.507692307692308,
0.523076923076923,0.538461538461538,0.553846153846154,0.569230769230769,
0.584615384615384,0.6,0.615384615384615,0.63076923076923,0.646153846153846,
0.661538461538461,0.676923076923076,0.692307692307692,0.707692307692307,
0.723076923076922,0.738461538461538,0.753846153846153,0.769230769230768,
0.784615384615384,0.799999999999999,0.815384615384614,0.83076923076923,
0.846153846153845,0.86153846153846,0.876923076923076,0.892307692307691,
0.907692307692306,0.923076923076922,0.938461538461537,0.953846153846152,
0.969230769230768,0.984615384615383,1.),.UNSPECIFIED.)
CURVE()
GEOMETRIC_REPRESENTATION_ITEM()
RATIONAL_B_SPLINE_CURVE((1.,1.,1.,1.,1.,1.,1.,1.,1.,1.,1.,1.,1.,1.,1.,1.,
1.,1.,1.,1.,1.,1.,1.,1.,1.,1.,1.,1.,1.,1.,1.,1.,1.,1.,1.,1.,1.,1.,1.,1.,
1.,1.,1.,1.,1.,1.,1.,1.,1.,1.,1.,1.,1.,1.,1.,1.,1.,1.,1.,1.,1.,1.,1.,1.,
1.,1.,1.,1.,1.,1.))
REPRESENTATION_ITEM('')
);
#283=(
BOUNDED_CURVE()
B_SPLINE_CURVE(5,(#40030,#40031,#40032,#40033,#40034,#40035,#40036,#40037,
#40038,#40039,#40040,#40041,#40042,#40043,#40044,#40045,#40046,#40047,#40048,
#40049,#40050,#40051,#40052,#40053,#40054,#40055,#40056,#40057,#40058,#40059,
#40060,#40061,#40062,#40063,#40064,#40065,#40066,#40067,#40068,#40069,#40070,
#40071,#40072,#40073,#40074,#40075,#40076,#40077,#40078,#40079,#40080,#40081,
#40082,#40083,#40084,#40085,#40086,#40087,#40088,#40089,#40090,#40091,#40092,
#40093,#40094,#40095,#40096,#40097,#40098,#40099),.UNSPECIFIED.,.F.,.F.)
B_SPLINE_CURVE_WITH_KNOTS((6,1,1,1,1,1,1,1,1,1,1,1,1,1,1,1,1,1,1,1,1,1,
1,1,1,1,1,1,1,1,1,1,1,1,1,1,1,1,1,1,1,1,1,1,1,1,1,1,1,1,1,1,1,1,1,1,1,1,
1,1,1,1,1,1,1,6),(0.,0.0153846153846154,0.0307692307692308,0.0461538461538462,
0.0615384615384615,0.0769230769230769,0.0923076923076923,0.107692307692308,
0.123076923076923,0.138461538461538,0.153846153846154,0.169230769230769,
0.184615384615385,0.2,0.215384615384615,0.230769230769231,0.246153846153846,
0.261538461538462,0.276923076923077,0.292307692307692,0.307692307692308,
0.323076923076923,0.338461538461538,0.353846153846154,0.369230769230769,
0.384615384615385,0.4,0.415384615384615,0.430769230769231,0.446153846153846,
0.461538461538462,0.476923076923077,0.492307692307692,0.507692307692308,
0.523076923076923,0.538461538461538,0.553846153846154,0.569230769230769,
0.584615384615384,0.6,0.615384615384615,0.63076923076923,0.646153846153846,
0.661538461538461,0.676923076923076,0.692307692307692,0.707692307692307,
0.723076923076922,0.738461538461538,0.753846153846153,0.769230769230768,
0.784615384615384,0.799999999999999,0.815384615384614,0.83076923076923,
0.846153846153845,0.86153846153846,0.876923076923076,0.892307692307691,
0.907692307692306,0.923076923076922,0.938461538461537,0.953846153846152,
0.969230769230768,0.984615384615383,1.),.UNSPECIFIED.)
CURVE()
GEOMETRIC_REPRESENTATION_ITEM()
RATIONAL_B_SPLINE_CURVE((1.,1.,1.,1.,1.,1.,1.,1.,1.,1.,1.,1.,1.,1.,1.,1.,
1.,1.,1.,1.,1.,1.,1.,1.,1.,1.,1.,1.,1.,1.,1.,1.,1.,1.,1.,1.,1.,1.,1.,1.,
1.,1.,1.,1.,1.,1.,1.,1.,1.,1.,1.,1.,1.,1.,1.,1.,1.,1.,1.,1.,1.,1.,1.,1.,
1.,1.,1.,1.,1.,1.))
REPRESENTATION_ITEM('')
);
#284=(
BOUNDED_CURVE()
B_SPLINE_CURVE(5,(#40103,#40104,#40105,#40106,#40107,#40108,#40109,#40110,
#40111,#40112,#40113,#40114,#40115,#40116,#40117,#40118,#40119,#40120,#40121,
#40122,#40123,#40124,#40125,#40126,#40127,#40128,#40129,#40130,#40131,#40132,
#40133,#40134,#40135,#40136,#40137,#40138,#40139,#40140,#40141,#40142,#40143,
#40144,#40145,#40146,#40147,#40148,#40149,#40150,#40151,#40152,#40153,#40154,
#40155,#40156,#40157,#40158,#40159,#40160,#40161,#40162,#40163,#40164,#40165,
#40166,#40167,#40168,#40169,#40170,#40171,#40172),.UNSPECIFIED.,.F.,.F.)
B_SPLINE_CURVE_WITH_KNOTS((6,1,1,1,1,1,1,1,1,1,1,1,1,1,1,1,1,1,1,1,1,1,
1,1,1,1,1,1,1,1,1,1,1,1,1,1,1,1,1,1,1,1,1,1,1,1,1,1,1,1,1,1,1,1,1,1,1,1,
1,1,1,1,1,1,1,6),(0.,0.0153846153846154,0.0307692307692308,0.0461538461538462,
0.0615384615384615,0.0769230769230769,0.0923076923076923,0.107692307692308,
0.123076923076923,0.138461538461538,0.153846153846154,0.169230769230769,
0.184615384615385,0.2,0.215384615384615,0.230769230769231,0.246153846153846,
0.261538461538462,0.276923076923077,0.292307692307692,0.307692307692308,
0.323076923076923,0.338461538461538,0.353846153846154,0.369230769230769,
0.384615384615385,0.4,0.415384615384615,0.430769230769231,0.446153846153846,
0.461538461538462,0.476923076923077,0.492307692307692,0.507692307692308,
0.523076923076923,0.538461538461538,0.553846153846154,0.569230769230769,
0.584615384615384,0.6,0.615384615384615,0.63076923076923,0.646153846153846,
0.661538461538461,0.676923076923076,0.692307692307692,0.707692307692307,
0.723076923076922,0.738461538461538,0.753846153846153,0.769230769230768,
0.784615384615384,0.799999999999999,0.815384615384614,0.83076923076923,
0.846153846153845,0.86153846153846,0.876923076923076,0.892307692307691,
0.907692307692306,0.923076923076922,0.938461538461537,0.953846153846152,
0.969230769230768,0.984615384615383,1.),.UNSPECIFIED.)
CURVE()
GEOMETRIC_REPRESENTATION_ITEM()
RATIONAL_B_SPLINE_CURVE((1.,1.,1.,1.,1.,1.,1.,1.,1.,1.,1.,1.,1.,1.,1.,1.,
1.,1.,1.,1.,1.,1.,1.,1.,1.,1.,1.,1.,1.,1.,1.,1.,1.,1.,1.,1.,1.,1.,1.,1.,
1.,1.,1.,1.,1.,1.,1.,1.,1.,1.,1.,1.,1.,1.,1.,1.,1.,1.,1.,1.,1.,1.,1.,1.,
1.,1.,1.,1.,1.,1.))
REPRESENTATION_ITEM('')
);
#285=(
BOUNDED_CURVE()
B_SPLINE_CURVE(5,(#40176,#40177,#40178,#40179,#40180,#40181,#40182,#40183,
#40184,#40185,#40186,#40187,#40188,#40189,#40190,#40191,#40192,#40193,#40194,
#40195,#40196,#40197,#40198,#40199,#40200,#40201,#40202,#40203,#40204,#40205,
#40206,#40207,#40208,#40209,#40210,#40211,#40212,#40213,#40214,#40215,#40216,
#40217,#40218,#40219,#40220,#40221,#40222,#40223,#40224,#40225,#40226,#40227,
#40228,#40229,#40230,#40231,#40232,#40233,#40234,#40235,#40236,#40237,#40238,
#40239,#40240,#40241,#40242,#40243,#40244,#40245),.UNSPECIFIED.,.F.,.F.)
B_SPLINE_CURVE_WITH_KNOTS((6,1,1,1,1,1,1,1,1,1,1,1,1,1,1,1,1,1,1,1,1,1,
1,1,1,1,1,1,1,1,1,1,1,1,1,1,1,1,1,1,1,1,1,1,1,1,1,1,1,1,1,1,1,1,1,1,1,1,
1,1,1,1,1,1,1,6),(0.,0.0153846153846154,0.0307692307692308,0.0461538461538462,
0.0615384615384615,0.0769230769230769,0.0923076923076923,0.107692307692308,
0.123076923076923,0.138461538461538,0.153846153846154,0.169230769230769,
0.184615384615385,0.2,0.215384615384615,0.230769230769231,0.246153846153846,
0.261538461538462,0.276923076923077,0.292307692307692,0.307692307692308,
0.323076923076923,0.338461538461538,0.353846153846154,0.369230769230769,
0.384615384615385,0.4,0.415384615384615,0.430769230769231,0.446153846153846,
0.461538461538462,0.476923076923077,0.492307692307692,0.507692307692308,
0.523076923076923,0.538461538461538,0.553846153846154,0.569230769230769,
0.584615384615384,0.6,0.615384615384615,0.63076923076923,0.646153846153846,
0.661538461538461,0.676923076923076,0.692307692307692,0.707692307692307,
0.723076923076922,0.738461538461538,0.753846153846153,0.769230769230768,
0.784615384615384,0.799999999999999,0.815384615384614,0.83076923076923,
0.846153846153845,0.86153846153846,0.876923076923076,0.892307692307691,
0.907692307692306,0.923076923076922,0.938461538461537,0.953846153846152,
0.969230769230768,0.984615384615383,1.),.UNSPECIFIED.)
CURVE()
GEOMETRIC_REPRESENTATION_ITEM()
RATIONAL_B_SPLINE_CURVE((1.,1.,1.,1.,1.,1.,1.,1.,1.,1.,1.,1.,1.,1.,1.,1.,
1.,1.,1.,1.,1.,1.,1.,1.,1.,1.,1.,1.,1.,1.,1.,1.,1.,1.,1.,1.,1.,1.,1.,1.,
1.,1.,1.,1.,1.,1.,1.,1.,1.,1.,1.,1.,1.,1.,1.,1.,1.,1.,1.,1.,1.,1.,1.,1.,
1.,1.,1.,1.,1.,1.))
REPRESENTATION_ITEM('')
);
#286=(
BOUNDED_CURVE()
B_SPLINE_CURVE(5,(#40249,#40250,#40251,#40252,#40253,#40254,#40255,#40256,
#40257,#40258,#40259,#40260,#40261,#40262,#40263,#40264,#40265,#40266,#40267,
#40268,#40269,#40270,#40271,#40272,#40273,#40274,#40275,#40276,#40277,#40278,
#40279,#40280,#40281,#40282,#40283,#40284,#40285,#40286,#40287,#40288,#40289,
#40290,#40291,#40292,#40293,#40294,#40295,#40296,#40297,#40298,#40299,#40300,
#40301,#40302,#40303,#40304,#40305,#40306,#40307,#40308,#40309,#40310,#40311,
#40312,#40313,#40314,#40315,#40316,#40317,#40318),.UNSPECIFIED.,.F.,.F.)
B_SPLINE_CURVE_WITH_KNOTS((6,1,1,1,1,1,1,1,1,1,1,1,1,1,1,1,1,1,1,1,1,1,
1,1,1,1,1,1,1,1,1,1,1,1,1,1,1,1,1,1,1,1,1,1,1,1,1,1,1,1,1,1,1,1,1,1,1,1,
1,1,1,1,1,1,1,6),(0.,0.0153846153846154,0.0307692307692308,0.0461538461538462,
0.0615384615384615,0.0769230769230769,0.0923076923076923,0.107692307692308,
0.123076923076923,0.138461538461538,0.153846153846154,0.169230769230769,
0.184615384615385,0.2,0.215384615384615,0.230769230769231,0.246153846153846,
0.261538461538462,0.276923076923077,0.292307692307692,0.307692307692308,
0.323076923076923,0.338461538461538,0.353846153846154,0.369230769230769,
0.384615384615385,0.4,0.415384615384615,0.430769230769231,0.446153846153846,
0.461538461538462,0.476923076923077,0.492307692307692,0.507692307692308,
0.523076923076923,0.538461538461538,0.553846153846154,0.569230769230769,
0.584615384615384,0.6,0.615384615384615,0.63076923076923,0.646153846153846,
0.661538461538461,0.676923076923076,0.692307692307692,0.707692307692307,
0.723076923076922,0.738461538461538,0.753846153846153,0.769230769230768,
0.784615384615384,0.799999999999999,0.815384615384614,0.83076923076923,
0.846153846153845,0.86153846153846,0.876923076923076,0.892307692307691,
0.907692307692306,0.923076923076922,0.938461538461537,0.953846153846152,
0.969230769230768,0.984615384615383,1.),.UNSPECIFIED.)
CURVE()
GEOMETRIC_REPRESENTATION_ITEM()
RATIONAL_B_SPLINE_CURVE((1.,1.,1.,1.,1.,1.,1.,1.,1.,1.,1.,1.,1.,1.,1.,1.,
1.,1.,1.,1.,1.,1.,1.,1.,1.,1.,1.,1.,1.,1.,1.,1.,1.,1.,1.,1.,1.,1.,1.,1.,
1.,1.,1.,1.,1.,1.,1.,1.,1.,1.,1.,1.,1.,1.,1.,1.,1.,1.,1.,1.,1.,1.,1.,1.,
1.,1.,1.,1.,1.,1.))
REPRESENTATION_ITEM('')
);
#287=(
BOUNDED_CURVE()
B_SPLINE_CURVE(5,(#40322,#40323,#40324,#40325,#40326,#40327,#40328,#40329,
#40330,#40331,#40332,#40333,#40334,#40335,#40336,#40337,#40338,#40339,#40340,
#40341,#40342,#40343,#40344,#40345,#40346,#40347,#40348,#40349,#40350,#40351,
#40352,#40353,#40354,#40355,#40356,#40357,#40358,#40359,#40360,#40361,#40362,
#40363,#40364,#40365,#40366,#40367,#40368,#40369,#40370,#40371,#40372,#40373,
#40374,#40375,#40376,#40377,#40378,#40379,#40380,#40381,#40382,#40383,#40384,
#40385,#40386,#40387,#40388,#40389,#40390,#40391),.UNSPECIFIED.,.F.,.F.)
B_SPLINE_CURVE_WITH_KNOTS((6,1,1,1,1,1,1,1,1,1,1,1,1,1,1,1,1,1,1,1,1,1,
1,1,1,1,1,1,1,1,1,1,1,1,1,1,1,1,1,1,1,1,1,1,1,1,1,1,1,1,1,1,1,1,1,1,1,1,
1,1,1,1,1,1,1,6),(0.,0.0153846153846154,0.0307692307692308,0.0461538461538462,
0.0615384615384615,0.0769230769230769,0.0923076923076923,0.107692307692308,
0.123076923076923,0.138461538461538,0.153846153846154,0.169230769230769,
0.184615384615385,0.2,0.215384615384615,0.230769230769231,0.246153846153846,
0.261538461538462,0.276923076923077,0.292307692307692,0.307692307692308,
0.323076923076923,0.338461538461538,0.353846153846154,0.369230769230769,
0.384615384615385,0.4,0.415384615384615,0.430769230769231,0.446153846153846,
0.461538461538462,0.476923076923077,0.492307692307692,0.507692307692308,
0.523076923076923,0.538461538461538,0.553846153846154,0.569230769230769,
0.584615384615384,0.6,0.615384615384615,0.63076923076923,0.646153846153846,
0.661538461538461,0.676923076923076,0.692307692307692,0.707692307692307,
0.723076923076922,0.738461538461538,0.753846153846153,0.769230769230768,
0.784615384615384,0.799999999999999,0.815384615384614,0.83076923076923,
0.846153846153845,0.86153846153846,0.876923076923076,0.892307692307691,
0.907692307692306,0.923076923076922,0.938461538461537,0.953846153846152,
0.969230769230768,0.984615384615383,1.),.UNSPECIFIED.)
CURVE()
GEOMETRIC_REPRESENTATION_ITEM()
RATIONAL_B_SPLINE_CURVE((1.,1.,1.,1.,1.,1.,1.,1.,1.,1.,1.,1.,1.,1.,1.,1.,
1.,1.,1.,1.,1.,1.,1.,1.,1.,1.,1.,1.,1.,1.,1.,1.,1.,1.,1.,1.,1.,1.,1.,1.,
1.,1.,1.,1.,1.,1.,1.,1.,1.,1.,1.,1.,1.,1.,1.,1.,1.,1.,1.,1.,1.,1.,1.,1.,
1.,1.,1.,1.,1.,1.))
REPRESENTATION_ITEM('')
);
#288=(
BOUNDED_CURVE()
B_SPLINE_CURVE(5,(#40395,#40396,#40397,#40398,#40399,#40400,#40401,#40402,
#40403,#40404,#40405,#40406,#40407,#40408,#40409,#40410,#40411,#40412,#40413,
#40414,#40415,#40416,#40417,#40418,#40419,#40420,#40421,#40422,#40423,#40424,
#40425,#40426,#40427,#40428,#40429,#40430,#40431,#40432,#40433,#40434,#40435,
#40436,#40437,#40438,#40439,#40440,#40441,#40442,#40443,#40444,#40445,#40446,
#40447,#40448,#40449,#40450,#40451,#40452,#40453,#40454,#40455,#40456,#40457,
#40458,#40459,#40460,#40461,#40462,#40463,#40464),.UNSPECIFIED.,.F.,.F.)
B_SPLINE_CURVE_WITH_KNOTS((6,1,1,1,1,1,1,1,1,1,1,1,1,1,1,1,1,1,1,1,1,1,
1,1,1,1,1,1,1,1,1,1,1,1,1,1,1,1,1,1,1,1,1,1,1,1,1,1,1,1,1,1,1,1,1,1,1,1,
1,1,1,1,1,1,1,6),(0.,0.0153846153846154,0.0307692307692308,0.0461538461538462,
0.0615384615384615,0.0769230769230769,0.0923076923076923,0.107692307692308,
0.123076923076923,0.138461538461538,0.153846153846154,0.169230769230769,
0.184615384615385,0.2,0.215384615384615,0.230769230769231,0.246153846153846,
0.261538461538462,0.276923076923077,0.292307692307692,0.307692307692308,
0.323076923076923,0.338461538461538,0.353846153846154,0.369230769230769,
0.384615384615385,0.4,0.415384615384615,0.430769230769231,0.446153846153846,
0.461538461538462,0.476923076923077,0.492307692307692,0.507692307692308,
0.523076923076923,0.538461538461538,0.553846153846154,0.569230769230769,
0.584615384615384,0.6,0.615384615384615,0.63076923076923,0.646153846153846,
0.661538461538461,0.676923076923076,0.692307692307692,0.707692307692307,
0.723076923076922,0.738461538461538,0.753846153846153,0.769230769230768,
0.784615384615384,0.799999999999999,0.815384615384614,0.83076923076923,
0.846153846153845,0.86153846153846,0.876923076923076,0.892307692307691,
0.907692307692306,0.923076923076922,0.938461538461537,0.953846153846152,
0.969230769230768,0.984615384615383,1.),.UNSPECIFIED.)
CURVE()
GEOMETRIC_REPRESENTATION_ITEM()
RATIONAL_B_SPLINE_CURVE((1.,1.,1.,1.,1.,1.,1.,1.,1.,1.,1.,1.,1.,1.,1.,1.,
1.,1.,1.,1.,1.,1.,1.,1.,1.,1.,1.,1.,1.,1.,1.,1.,1.,1.,1.,1.,1.,1.,1.,1.,
1.,1.,1.,1.,1.,1.,1.,1.,1.,1.,1.,1.,1.,1.,1.,1.,1.,1.,1.,1.,1.,1.,1.,1.,
1.,1.,1.,1.,1.,1.))
REPRESENTATION_ITEM('')
);
#289=(
BOUNDED_CURVE()
B_SPLINE_CURVE(5,(#40468,#40469,#40470,#40471,#40472,#40473,#40474,#40475,
#40476,#40477,#40478,#40479,#40480,#40481,#40482,#40483,#40484,#40485,#40486,
#40487,#40488,#40489,#40490,#40491,#40492,#40493,#40494,#40495,#40496,#40497,
#40498,#40499,#40500,#40501,#40502,#40503,#40504,#40505,#40506,#40507,#40508,
#40509,#40510,#40511,#40512,#40513,#40514,#40515,#40516,#40517,#40518,#40519,
#40520,#40521,#40522,#40523,#40524,#40525,#40526,#40527,#40528,#40529,#40530,
#40531,#40532,#40533,#40534,#40535,#40536,#40537),.UNSPECIFIED.,.F.,.F.)
B_SPLINE_CURVE_WITH_KNOTS((6,1,1,1,1,1,1,1,1,1,1,1,1,1,1,1,1,1,1,1,1,1,
1,1,1,1,1,1,1,1,1,1,1,1,1,1,1,1,1,1,1,1,1,1,1,1,1,1,1,1,1,1,1,1,1,1,1,1,
1,1,1,1,1,1,1,6),(0.,0.0153846153846154,0.0307692307692308,0.0461538461538462,
0.0615384615384615,0.0769230769230769,0.0923076923076923,0.107692307692308,
0.123076923076923,0.138461538461538,0.153846153846154,0.169230769230769,
0.184615384615385,0.2,0.215384615384615,0.230769230769231,0.246153846153846,
0.261538461538462,0.276923076923077,0.292307692307692,0.307692307692308,
0.323076923076923,0.338461538461538,0.353846153846154,0.369230769230769,
0.384615384615385,0.4,0.415384615384615,0.430769230769231,0.446153846153846,
0.461538461538462,0.476923076923077,0.492307692307692,0.507692307692308,
0.523076923076923,0.538461538461538,0.553846153846154,0.569230769230769,
0.584615384615384,0.6,0.615384615384615,0.63076923076923,0.646153846153846,
0.661538461538461,0.676923076923076,0.692307692307692,0.707692307692307,
0.723076923076922,0.738461538461538,0.753846153846153,0.769230769230768,
0.784615384615384,0.799999999999999,0.815384615384614,0.83076923076923,
0.846153846153845,0.86153846153846,0.876923076923076,0.892307692307691,
0.907692307692306,0.923076923076922,0.938461538461537,0.953846153846152,
0.969230769230768,0.984615384615383,1.),.UNSPECIFIED.)
CURVE()
GEOMETRIC_REPRESENTATION_ITEM()
RATIONAL_B_SPLINE_CURVE((1.,1.,1.,1.,1.,1.,1.,1.,1.,1.,1.,1.,1.,1.,1.,1.,
1.,1.,1.,1.,1.,1.,1.,1.,1.,1.,1.,1.,1.,1.,1.,1.,1.,1.,1.,1.,1.,1.,1.,1.,
1.,1.,1.,1.,1.,1.,1.,1.,1.,1.,1.,1.,1.,1.,1.,1.,1.,1.,1.,1.,1.,1.,1.,1.,
1.,1.,1.,1.,1.,1.))
REPRESENTATION_ITEM('')
);
#290=(
BOUNDED_CURVE()
B_SPLINE_CURVE(5,(#40540,#40541,#40542,#40543,#40544,#40545,#40546,#40547,
#40548,#40549,#40550,#40551,#40552,#40553,#40554,#40555,#40556,#40557,#40558,
#40559,#40560,#40561,#40562,#40563,#40564,#40565,#40566,#40567,#40568,#40569,
#40570,#40571,#40572,#40573,#40574,#40575,#40576,#40577,#40578,#40579,#40580,
#40581,#40582,#40583,#40584,#40585,#40586,#40587,#40588,#40589,#40590,#40591,
#40592,#40593,#40594,#40595,#40596,#40597,#40598,#40599,#40600,#40601,#40602,
#40603,#40604,#40605,#40606,#40607,#40608,#40609),.UNSPECIFIED.,.F.,.F.)
B_SPLINE_CURVE_WITH_KNOTS((6,1,1,1,1,1,1,1,1,1,1,1,1,1,1,1,1,1,1,1,1,1,
1,1,1,1,1,1,1,1,1,1,1,1,1,1,1,1,1,1,1,1,1,1,1,1,1,1,1,1,1,1,1,1,1,1,1,1,
1,1,1,1,1,1,1,6),(0.,0.0153846153846154,0.0307692307692308,0.0461538461538462,
0.0615384615384615,0.0769230769230769,0.0923076923076923,0.107692307692308,
0.123076923076923,0.138461538461538,0.153846153846154,0.169230769230769,
0.184615384615385,0.2,0.215384615384615,0.230769230769231,0.246153846153846,
0.261538461538462,0.276923076923077,0.292307692307692,0.307692307692308,
0.323076923076923,0.338461538461538,0.353846153846154,0.369230769230769,
0.384615384615385,0.4,0.415384615384615,0.430769230769231,0.446153846153846,
0.461538461538462,0.476923076923077,0.492307692307692,0.507692307692308,
0.523076923076923,0.538461538461538,0.553846153846154,0.569230769230769,
0.584615384615384,0.6,0.615384615384615,0.63076923076923,0.646153846153846,
0.661538461538461,0.676923076923076,0.692307692307692,0.707692307692307,
0.723076923076922,0.738461538461538,0.753846153846153,0.769230769230768,
0.784615384615384,0.799999999999999,0.815384615384614,0.83076923076923,
0.846153846153845,0.86153846153846,0.876923076923076,0.892307692307691,
0.907692307692306,0.923076923076922,0.938461538461537,0.953846153846152,
0.969230769230768,0.984615384615383,1.),.UNSPECIFIED.)
CURVE()
GEOMETRIC_REPRESENTATION_ITEM()
RATIONAL_B_SPLINE_CURVE((1.,1.,1.,1.,1.,1.,1.,1.,1.,1.,1.,1.,1.,1.,1.,1.,
1.,1.,1.,1.,1.,1.,1.,1.,1.,1.,1.,1.,1.,1.,1.,1.,1.,1.,1.,1.,1.,1.,1.,1.,
1.,1.,1.,1.,1.,1.,1.,1.,1.,1.,1.,1.,1.,1.,1.,1.,1.,1.,1.,1.,1.,1.,1.,1.,
1.,1.,1.,1.,1.,1.))
REPRESENTATION_ITEM('')
);
#291=(
BOUNDED_CURVE()
B_SPLINE_CURVE(5,(#40757,#40758,#40759,#40760,#40761,#40762,#40763,#40764,
#40765,#40766,#40767,#40768,#40769,#40770,#40771,#40772,#40773,#40774,#40775,
#40776,#40777,#40778,#40779,#40780,#40781,#40782,#40783,#40784,#40785,#40786,
#40787,#40788,#40789,#40790,#40791,#40792,#40793,#40794,#40795,#40796,#40797,
#40798,#40799,#40800,#40801,#40802,#40803,#40804,#40805,#40806,#40807,#40808,
#40809,#40810,#40811,#40812,#40813,#40814,#40815,#40816,#40817,#40818,#40819,
#40820,#40821,#40822,#40823,#40824,#40825,#40826),.UNSPECIFIED.,.F.,.F.)
B_SPLINE_CURVE_WITH_KNOTS((6,1,1,1,1,1,1,1,1,1,1,1,1,1,1,1,1,1,1,1,1,1,
1,1,1,1,1,1,1,1,1,1,1,1,1,1,1,1,1,1,1,1,1,1,1,1,1,1,1,1,1,1,1,1,1,1,1,1,
1,1,1,1,1,1,1,6),(-1.,-0.984615384615383,-0.969230769230768,-0.953846153846152,
-0.938461538461537,-0.923076923076922,-0.907692307692306,-0.892307692307691,
-0.876923076923076,-0.86153846153846,-0.846153846153845,-0.83076923076923,
-0.815384615384614,-0.799999999999999,-0.784615384615384,-0.769230769230768,
-0.753846153846153,-0.738461538461538,-0.723076923076922,-0.707692307692307,
-0.692307692307692,-0.676923076923076,-0.661538461538461,-0.646153846153846,
-0.63076923076923,-0.615384615384615,-0.6,-0.584615384615384,-0.569230769230769,
-0.553846153846154,-0.538461538461538,-0.523076923076923,-0.507692307692308,
-0.492307692307692,-0.476923076923077,-0.461538461538462,-0.446153846153846,
-0.430769230769231,-0.415384615384615,-0.4,-0.384615384615385,-0.369230769230769,
-0.353846153846154,-0.338461538461538,-0.323076923076923,-0.307692307692308,
-0.292307692307692,-0.276923076923077,-0.261538461538462,-0.246153846153846,
-0.230769230769231,-0.215384615384615,-0.2,-0.184615384615385,-0.169230769230769,
-0.153846153846154,-0.138461538461538,-0.123076923076923,-0.107692307692308,
-0.0923076923076923,-0.0769230769230769,-0.0615384615384615,-0.0461538461538462,
-0.0307692307692308,-0.0153846153846154,0.),.UNSPECIFIED.)
CURVE()
GEOMETRIC_REPRESENTATION_ITEM()
RATIONAL_B_SPLINE_CURVE((1.,1.,1.,1.,1.,1.,1.,1.,1.,1.,1.,1.,1.,1.,1.,1.,
1.,1.,1.,1.,1.,1.,1.,1.,1.,1.,1.,1.,1.,1.,1.,1.,1.,1.,1.,1.,1.,1.,1.,1.,
1.,1.,1.,1.,1.,1.,1.,1.,1.,1.,1.,1.,1.,1.,1.,1.,1.,1.,1.,1.,1.,1.,1.,1.,
1.,1.,1.,1.,1.,1.))
REPRESENTATION_ITEM('')
);
#292=(
BOUNDED_CURVE()
B_SPLINE_CURVE(5,(#40973,#40974,#40975,#40976,#40977,#40978,#40979,#40980,
#40981,#40982,#40983,#40984,#40985,#40986,#40987,#40988,#40989,#40990,#40991,
#40992,#40993,#40994,#40995,#40996,#40997,#40998,#40999,#41000,#41001,#41002,
#41003,#41004,#41005,#41006,#41007,#41008,#41009,#41010,#41011,#41012,#41013,
#41014,#41015,#41016,#41017,#41018,#41019,#41020,#41021,#41022,#41023,#41024,
#41025,#41026,#41027,#41028,#41029,#41030,#41031,#41032,#41033,#41034,#41035,
#41036,#41037,#41038,#41039,#41040,#41041,#41042),.UNSPECIFIED.,.F.,.F.)
B_SPLINE_CURVE_WITH_KNOTS((6,1,1,1,1,1,1,1,1,1,1,1,1,1,1,1,1,1,1,1,1,1,
1,1,1,1,1,1,1,1,1,1,1,1,1,1,1,1,1,1,1,1,1,1,1,1,1,1,1,1,1,1,1,1,1,1,1,1,
1,1,1,1,1,1,1,6),(-1.,-0.984615384615383,-0.969230769230768,-0.953846153846152,
-0.938461538461537,-0.923076923076922,-0.907692307692306,-0.892307692307691,
-0.876923076923076,-0.86153846153846,-0.846153846153845,-0.83076923076923,
-0.815384615384614,-0.799999999999999,-0.784615384615384,-0.769230769230768,
-0.753846153846153,-0.738461538461538,-0.723076923076922,-0.707692307692307,
-0.692307692307692,-0.676923076923076,-0.661538461538461,-0.646153846153846,
-0.63076923076923,-0.615384615384615,-0.6,-0.584615384615384,-0.569230769230769,
-0.553846153846154,-0.538461538461538,-0.523076923076923,-0.507692307692308,
-0.492307692307692,-0.476923076923077,-0.461538461538462,-0.446153846153846,
-0.430769230769231,-0.415384615384615,-0.4,-0.384615384615385,-0.369230769230769,
-0.353846153846154,-0.338461538461538,-0.323076923076923,-0.307692307692308,
-0.292307692307692,-0.276923076923077,-0.261538461538462,-0.246153846153846,
-0.230769230769231,-0.215384615384615,-0.2,-0.184615384615385,-0.169230769230769,
-0.153846153846154,-0.138461538461538,-0.123076923076923,-0.107692307692308,
-0.0923076923076923,-0.0769230769230769,-0.0615384615384615,-0.0461538461538462,
-0.0307692307692308,-0.0153846153846154,0.),.UNSPECIFIED.)
CURVE()
GEOMETRIC_REPRESENTATION_ITEM()
RATIONAL_B_SPLINE_CURVE((1.,1.,1.,1.,1.,1.,1.,1.,1.,1.,1.,1.,1.,1.,1.,1.,
1.,1.,1.,1.,1.,1.,1.,1.,1.,1.,1.,1.,1.,1.,1.,1.,1.,1.,1.,1.,1.,1.,1.,1.,
1.,1.,1.,1.,1.,1.,1.,1.,1.,1.,1.,1.,1.,1.,1.,1.,1.,1.,1.,1.,1.,1.,1.,1.,
1.,1.,1.,1.,1.,1.))
REPRESENTATION_ITEM('')
);
#293=(
BOUNDED_CURVE()
B_SPLINE_CURVE(5,(#41189,#41190,#41191,#41192,#41193,#41194,#41195,#41196,
#41197,#41198,#41199,#41200,#41201,#41202,#41203,#41204,#41205,#41206,#41207,
#41208,#41209,#41210,#41211,#41212,#41213,#41214,#41215,#41216,#41217,#41218,
#41219,#41220,#41221,#41222,#41223,#41224,#41225,#41226,#41227,#41228,#41229,
#41230,#41231,#41232,#41233,#41234,#41235,#41236,#41237,#41238,#41239,#41240,
#41241,#41242,#41243,#41244,#41245,#41246,#41247,#41248,#41249,#41250,#41251,
#41252,#41253,#41254,#41255,#41256,#41257,#41258),.UNSPECIFIED.,.F.,.F.)
B_SPLINE_CURVE_WITH_KNOTS((6,1,1,1,1,1,1,1,1,1,1,1,1,1,1,1,1,1,1,1,1,1,
1,1,1,1,1,1,1,1,1,1,1,1,1,1,1,1,1,1,1,1,1,1,1,1,1,1,1,1,1,1,1,1,1,1,1,1,
1,1,1,1,1,1,1,6),(-1.,-0.984615384615383,-0.969230769230768,-0.953846153846152,
-0.938461538461537,-0.923076923076922,-0.907692307692306,-0.892307692307691,
-0.876923076923076,-0.86153846153846,-0.846153846153845,-0.83076923076923,
-0.815384615384614,-0.799999999999999,-0.784615384615384,-0.769230769230768,
-0.753846153846153,-0.738461538461538,-0.723076923076922,-0.707692307692307,
-0.692307692307692,-0.676923076923076,-0.661538461538461,-0.646153846153846,
-0.63076923076923,-0.615384615384615,-0.6,-0.584615384615384,-0.569230769230769,
-0.553846153846154,-0.538461538461538,-0.523076923076923,-0.507692307692308,
-0.492307692307692,-0.476923076923077,-0.461538461538462,-0.446153846153846,
-0.430769230769231,-0.415384615384615,-0.4,-0.384615384615385,-0.369230769230769,
-0.353846153846154,-0.338461538461538,-0.323076923076923,-0.307692307692308,
-0.292307692307692,-0.276923076923077,-0.261538461538462,-0.246153846153846,
-0.230769230769231,-0.215384615384615,-0.2,-0.184615384615385,-0.169230769230769,
-0.153846153846154,-0.138461538461538,-0.123076923076923,-0.107692307692308,
-0.0923076923076923,-0.0769230769230769,-0.0615384615384615,-0.0461538461538462,
-0.0307692307692308,-0.0153846153846154,0.),.UNSPECIFIED.)
CURVE()
GEOMETRIC_REPRESENTATION_ITEM()
RATIONAL_B_SPLINE_CURVE((1.,1.,1.,1.,1.,1.,1.,1.,1.,1.,1.,1.,1.,1.,1.,1.,
1.,1.,1.,1.,1.,1.,1.,1.,1.,1.,1.,1.,1.,1.,1.,1.,1.,1.,1.,1.,1.,1.,1.,1.,
1.,1.,1.,1.,1.,1.,1.,1.,1.,1.,1.,1.,1.,1.,1.,1.,1.,1.,1.,1.,1.,1.,1.,1.,
1.,1.,1.,1.,1.,1.))
REPRESENTATION_ITEM('')
);
#294=(
BOUNDED_CURVE()
B_SPLINE_CURVE(5,(#41405,#41406,#41407,#41408,#41409,#41410,#41411,#41412,
#41413,#41414,#41415,#41416,#41417,#41418,#41419,#41420,#41421,#41422,#41423,
#41424,#41425,#41426,#41427,#41428,#41429,#41430,#41431,#41432,#41433,#41434,
#41435,#41436,#41437,#41438,#41439,#41440,#41441,#41442,#41443,#41444,#41445,
#41446,#41447,#41448,#41449,#41450,#41451,#41452,#41453,#41454,#41455,#41456,
#41457,#41458,#41459,#41460,#41461,#41462,#41463,#41464,#41465,#41466,#41467,
#41468,#41469,#41470,#41471,#41472,#41473,#41474),.UNSPECIFIED.,.F.,.F.)
B_SPLINE_CURVE_WITH_KNOTS((6,1,1,1,1,1,1,1,1,1,1,1,1,1,1,1,1,1,1,1,1,1,
1,1,1,1,1,1,1,1,1,1,1,1,1,1,1,1,1,1,1,1,1,1,1,1,1,1,1,1,1,1,1,1,1,1,1,1,
1,1,1,1,1,1,1,6),(-1.,-0.984615384615383,-0.969230769230768,-0.953846153846152,
-0.938461538461537,-0.923076923076922,-0.907692307692306,-0.892307692307691,
-0.876923076923076,-0.86153846153846,-0.846153846153845,-0.83076923076923,
-0.815384615384614,-0.799999999999999,-0.784615384615384,-0.769230769230768,
-0.753846153846153,-0.738461538461538,-0.723076923076922,-0.707692307692307,
-0.692307692307692,-0.676923076923076,-0.661538461538461,-0.646153846153846,
-0.63076923076923,-0.615384615384615,-0.6,-0.584615384615384,-0.569230769230769,
-0.553846153846154,-0.538461538461538,-0.523076923076923,-0.507692307692308,
-0.492307692307692,-0.476923076923077,-0.461538461538462,-0.446153846153846,
-0.430769230769231,-0.415384615384615,-0.4,-0.384615384615385,-0.369230769230769,
-0.353846153846154,-0.338461538461538,-0.323076923076923,-0.307692307692308,
-0.292307692307692,-0.276923076923077,-0.261538461538462,-0.246153846153846,
-0.230769230769231,-0.215384615384615,-0.2,-0.184615384615385,-0.169230769230769,
-0.153846153846154,-0.138461538461538,-0.123076923076923,-0.107692307692308,
-0.0923076923076923,-0.0769230769230769,-0.0615384615384615,-0.0461538461538462,
-0.0307692307692308,-0.0153846153846154,0.),.UNSPECIFIED.)
CURVE()
GEOMETRIC_REPRESENTATION_ITEM()
RATIONAL_B_SPLINE_CURVE((1.,1.,1.,1.,1.,1.,1.,1.,1.,1.,1.,1.,1.,1.,1.,1.,
1.,1.,1.,1.,1.,1.,1.,1.,1.,1.,1.,1.,1.,1.,1.,1.,1.,1.,1.,1.,1.,1.,1.,1.,
1.,1.,1.,1.,1.,1.,1.,1.,1.,1.,1.,1.,1.,1.,1.,1.,1.,1.,1.,1.,1.,1.,1.,1.,
1.,1.,1.,1.,1.,1.))
REPRESENTATION_ITEM('')
);
#295=(
BOUNDED_CURVE()
B_SPLINE_CURVE(5,(#41621,#41622,#41623,#41624,#41625,#41626,#41627,#41628,
#41629,#41630,#41631,#41632,#41633,#41634,#41635,#41636,#41637,#41638,#41639,
#41640,#41641,#41642,#41643,#41644,#41645,#41646,#41647,#41648,#41649,#41650,
#41651,#41652,#41653,#41654,#41655,#41656,#41657,#41658,#41659,#41660,#41661,
#41662,#41663,#41664,#41665,#41666,#41667,#41668,#41669,#41670,#41671,#41672,
#41673,#41674,#41675,#41676,#41677,#41678,#41679,#41680,#41681,#41682,#41683,
#41684,#41685,#41686,#41687,#41688,#41689,#41690),.UNSPECIFIED.,.F.,.F.)
B_SPLINE_CURVE_WITH_KNOTS((6,1,1,1,1,1,1,1,1,1,1,1,1,1,1,1,1,1,1,1,1,1,
1,1,1,1,1,1,1,1,1,1,1,1,1,1,1,1,1,1,1,1,1,1,1,1,1,1,1,1,1,1,1,1,1,1,1,1,
1,1,1,1,1,1,1,6),(-1.,-0.984615384615383,-0.969230769230768,-0.953846153846152,
-0.938461538461537,-0.923076923076922,-0.907692307692306,-0.892307692307691,
-0.876923076923076,-0.86153846153846,-0.846153846153845,-0.83076923076923,
-0.815384615384614,-0.799999999999999,-0.784615384615384,-0.769230769230768,
-0.753846153846153,-0.738461538461538,-0.723076923076922,-0.707692307692307,
-0.692307692307692,-0.676923076923076,-0.661538461538461,-0.646153846153846,
-0.63076923076923,-0.615384615384615,-0.6,-0.584615384615384,-0.569230769230769,
-0.553846153846154,-0.538461538461538,-0.523076923076923,-0.507692307692308,
-0.492307692307692,-0.476923076923077,-0.461538461538462,-0.446153846153846,
-0.430769230769231,-0.415384615384615,-0.4,-0.384615384615385,-0.369230769230769,
-0.353846153846154,-0.338461538461538,-0.323076923076923,-0.307692307692308,
-0.292307692307692,-0.276923076923077,-0.261538461538462,-0.246153846153846,
-0.230769230769231,-0.215384615384615,-0.2,-0.184615384615385,-0.169230769230769,
-0.153846153846154,-0.138461538461538,-0.123076923076923,-0.107692307692308,
-0.0923076923076923,-0.0769230769230769,-0.0615384615384615,-0.0461538461538462,
-0.0307692307692308,-0.0153846153846154,0.),.UNSPECIFIED.)
CURVE()
GEOMETRIC_REPRESENTATION_ITEM()
RATIONAL_B_SPLINE_CURVE((1.,1.,1.,1.,1.,1.,1.,1.,1.,1.,1.,1.,1.,1.,1.,1.,
1.,1.,1.,1.,1.,1.,1.,1.,1.,1.,1.,1.,1.,1.,1.,1.,1.,1.,1.,1.,1.,1.,1.,1.,
1.,1.,1.,1.,1.,1.,1.,1.,1.,1.,1.,1.,1.,1.,1.,1.,1.,1.,1.,1.,1.,1.,1.,1.,
1.,1.,1.,1.,1.,1.))
REPRESENTATION_ITEM('')
);
#296=(
BOUNDED_CURVE()
B_SPLINE_CURVE(5,(#41837,#41838,#41839,#41840,#41841,#41842,#41843,#41844,
#41845,#41846,#41847,#41848,#41849,#41850,#41851,#41852,#41853,#41854,#41855,
#41856,#41857,#41858,#41859,#41860,#41861,#41862,#41863,#41864,#41865,#41866,
#41867,#41868,#41869,#41870,#41871,#41872,#41873,#41874,#41875,#41876,#41877,
#41878,#41879,#41880,#41881,#41882,#41883,#41884,#41885,#41886,#41887,#41888,
#41889,#41890,#41891,#41892,#41893,#41894,#41895,#41896,#41897,#41898,#41899,
#41900,#41901,#41902,#41903,#41904,#41905,#41906),.UNSPECIFIED.,.F.,.F.)
B_SPLINE_CURVE_WITH_KNOTS((6,1,1,1,1,1,1,1,1,1,1,1,1,1,1,1,1,1,1,1,1,1,
1,1,1,1,1,1,1,1,1,1,1,1,1,1,1,1,1,1,1,1,1,1,1,1,1,1,1,1,1,1,1,1,1,1,1,1,
1,1,1,1,1,1,1,6),(-1.,-0.984615384615383,-0.969230769230768,-0.953846153846152,
-0.938461538461537,-0.923076923076922,-0.907692307692306,-0.892307692307691,
-0.876923076923076,-0.86153846153846,-0.846153846153845,-0.83076923076923,
-0.815384615384614,-0.799999999999999,-0.784615384615384,-0.769230769230768,
-0.753846153846153,-0.738461538461538,-0.723076923076922,-0.707692307692307,
-0.692307692307692,-0.676923076923076,-0.661538461538461,-0.646153846153846,
-0.63076923076923,-0.615384615384615,-0.6,-0.584615384615384,-0.569230769230769,
-0.553846153846154,-0.538461538461538,-0.523076923076923,-0.507692307692308,
-0.492307692307692,-0.476923076923077,-0.461538461538462,-0.446153846153846,
-0.430769230769231,-0.415384615384615,-0.4,-0.384615384615385,-0.369230769230769,
-0.353846153846154,-0.338461538461538,-0.323076923076923,-0.307692307692308,
-0.292307692307692,-0.276923076923077,-0.261538461538462,-0.246153846153846,
-0.230769230769231,-0.215384615384615,-0.2,-0.184615384615385,-0.169230769230769,
-0.153846153846154,-0.138461538461538,-0.123076923076923,-0.107692307692308,
-0.0923076923076923,-0.0769230769230769,-0.0615384615384615,-0.0461538461538462,
-0.0307692307692308,-0.0153846153846154,0.),.UNSPECIFIED.)
CURVE()
GEOMETRIC_REPRESENTATION_ITEM()
RATIONAL_B_SPLINE_CURVE((1.,1.,1.,1.,1.,1.,1.,1.,1.,1.,1.,1.,1.,1.,1.,1.,
1.,1.,1.,1.,1.,1.,1.,1.,1.,1.,1.,1.,1.,1.,1.,1.,1.,1.,1.,1.,1.,1.,1.,1.,
1.,1.,1.,1.,1.,1.,1.,1.,1.,1.,1.,1.,1.,1.,1.,1.,1.,1.,1.,1.,1.,1.,1.,1.,
1.,1.,1.,1.,1.,1.))
REPRESENTATION_ITEM('')
);
#297=(
BOUNDED_CURVE()
B_SPLINE_CURVE(5,(#42053,#42054,#42055,#42056,#42057,#42058,#42059,#42060,
#42061,#42062,#42063,#42064,#42065,#42066,#42067,#42068,#42069,#42070,#42071,
#42072,#42073,#42074,#42075,#42076,#42077,#42078,#42079,#42080,#42081,#42082,
#42083,#42084,#42085,#42086,#42087,#42088,#42089,#42090,#42091,#42092,#42093,
#42094,#42095,#42096,#42097,#42098,#42099,#42100,#42101,#42102,#42103,#42104,
#42105,#42106,#42107,#42108,#42109,#42110,#42111,#42112,#42113,#42114,#42115,
#42116,#42117,#42118,#42119,#42120,#42121,#42122),.UNSPECIFIED.,.F.,.F.)
B_SPLINE_CURVE_WITH_KNOTS((6,1,1,1,1,1,1,1,1,1,1,1,1,1,1,1,1,1,1,1,1,1,
1,1,1,1,1,1,1,1,1,1,1,1,1,1,1,1,1,1,1,1,1,1,1,1,1,1,1,1,1,1,1,1,1,1,1,1,
1,1,1,1,1,1,1,6),(-1.,-0.984615384615383,-0.969230769230768,-0.953846153846152,
-0.938461538461537,-0.923076923076922,-0.907692307692306,-0.892307692307691,
-0.876923076923076,-0.86153846153846,-0.846153846153845,-0.83076923076923,
-0.815384615384614,-0.799999999999999,-0.784615384615384,-0.769230769230768,
-0.753846153846153,-0.738461538461538,-0.723076923076922,-0.707692307692307,
-0.692307692307692,-0.676923076923076,-0.661538461538461,-0.646153846153846,
-0.63076923076923,-0.615384615384615,-0.6,-0.584615384615384,-0.569230769230769,
-0.553846153846154,-0.538461538461538,-0.523076923076923,-0.507692307692308,
-0.492307692307692,-0.476923076923077,-0.461538461538462,-0.446153846153846,
-0.430769230769231,-0.415384615384615,-0.4,-0.384615384615385,-0.369230769230769,
-0.353846153846154,-0.338461538461538,-0.323076923076923,-0.307692307692308,
-0.292307692307692,-0.276923076923077,-0.261538461538462,-0.246153846153846,
-0.230769230769231,-0.215384615384615,-0.2,-0.184615384615385,-0.169230769230769,
-0.153846153846154,-0.138461538461538,-0.123076923076923,-0.107692307692308,
-0.0923076923076923,-0.0769230769230769,-0.0615384615384615,-0.0461538461538462,
-0.0307692307692308,-0.0153846153846154,0.),.UNSPECIFIED.)
CURVE()
GEOMETRIC_REPRESENTATION_ITEM()
RATIONAL_B_SPLINE_CURVE((1.,1.,1.,1.,1.,1.,1.,1.,1.,1.,1.,1.,1.,1.,1.,1.,
1.,1.,1.,1.,1.,1.,1.,1.,1.,1.,1.,1.,1.,1.,1.,1.,1.,1.,1.,1.,1.,1.,1.,1.,
1.,1.,1.,1.,1.,1.,1.,1.,1.,1.,1.,1.,1.,1.,1.,1.,1.,1.,1.,1.,1.,1.,1.,1.,
1.,1.,1.,1.,1.,1.))
REPRESENTATION_ITEM('')
);
#298=(
BOUNDED_CURVE()
B_SPLINE_CURVE(5,(#42269,#42270,#42271,#42272,#42273,#42274,#42275,#42276,
#42277,#42278,#42279,#42280,#42281,#42282,#42283,#42284,#42285,#42286,#42287,
#42288,#42289,#42290,#42291,#42292,#42293,#42294,#42295,#42296,#42297,#42298,
#42299,#42300,#42301,#42302,#42303,#42304,#42305,#42306,#42307,#42308,#42309,
#42310,#42311,#42312,#42313,#42314,#42315,#42316,#42317,#42318,#42319,#42320,
#42321,#42322,#42323,#42324,#42325,#42326,#42327,#42328,#42329,#42330,#42331,
#42332,#42333,#42334,#42335,#42336,#42337,#42338),.UNSPECIFIED.,.F.,.F.)
B_SPLINE_CURVE_WITH_KNOTS((6,1,1,1,1,1,1,1,1,1,1,1,1,1,1,1,1,1,1,1,1,1,
1,1,1,1,1,1,1,1,1,1,1,1,1,1,1,1,1,1,1,1,1,1,1,1,1,1,1,1,1,1,1,1,1,1,1,1,
1,1,1,1,1,1,1,6),(-1.,-0.984615384615383,-0.969230769230768,-0.953846153846152,
-0.938461538461537,-0.923076923076922,-0.907692307692306,-0.892307692307691,
-0.876923076923076,-0.86153846153846,-0.846153846153845,-0.83076923076923,
-0.815384615384614,-0.799999999999999,-0.784615384615384,-0.769230769230768,
-0.753846153846153,-0.738461538461538,-0.723076923076922,-0.707692307692307,
-0.692307692307692,-0.676923076923076,-0.661538461538461,-0.646153846153846,
-0.63076923076923,-0.615384615384615,-0.6,-0.584615384615384,-0.569230769230769,
-0.553846153846154,-0.538461538461538,-0.523076923076923,-0.507692307692308,
-0.492307692307692,-0.476923076923077,-0.461538461538462,-0.446153846153846,
-0.430769230769231,-0.415384615384615,-0.4,-0.384615384615385,-0.369230769230769,
-0.353846153846154,-0.338461538461538,-0.323076923076923,-0.307692307692308,
-0.292307692307692,-0.276923076923077,-0.261538461538462,-0.246153846153846,
-0.230769230769231,-0.215384615384615,-0.2,-0.184615384615385,-0.169230769230769,
-0.153846153846154,-0.138461538461538,-0.123076923076923,-0.107692307692308,
-0.0923076923076923,-0.0769230769230769,-0.0615384615384615,-0.0461538461538462,
-0.0307692307692308,-0.0153846153846154,0.),.UNSPECIFIED.)
CURVE()
GEOMETRIC_REPRESENTATION_ITEM()
RATIONAL_B_SPLINE_CURVE((1.,1.,1.,1.,1.,1.,1.,1.,1.,1.,1.,1.,1.,1.,1.,1.,
1.,1.,1.,1.,1.,1.,1.,1.,1.,1.,1.,1.,1.,1.,1.,1.,1.,1.,1.,1.,1.,1.,1.,1.,
1.,1.,1.,1.,1.,1.,1.,1.,1.,1.,1.,1.,1.,1.,1.,1.,1.,1.,1.,1.,1.,1.,1.,1.,
1.,1.,1.,1.,1.,1.))
REPRESENTATION_ITEM('')
);
#299=(
BOUNDED_CURVE()
B_SPLINE_CURVE(5,(#42485,#42486,#42487,#42488,#42489,#42490,#42491,#42492,
#42493,#42494,#42495,#42496,#42497,#42498,#42499,#42500,#42501,#42502,#42503,
#42504,#42505,#42506,#42507,#42508,#42509,#42510,#42511,#42512,#42513,#42514,
#42515,#42516,#42517,#42518,#42519,#42520,#42521,#42522,#42523,#42524,#42525,
#42526,#42527,#42528,#42529,#42530,#42531,#42532,#42533,#42534,#42535,#42536,
#42537,#42538,#42539,#42540,#42541,#42542,#42543,#42544,#42545,#42546,#42547,
#42548,#42549,#42550,#42551,#42552,#42553,#42554),.UNSPECIFIED.,.F.,.F.)
B_SPLINE_CURVE_WITH_KNOTS((6,1,1,1,1,1,1,1,1,1,1,1,1,1,1,1,1,1,1,1,1,1,
1,1,1,1,1,1,1,1,1,1,1,1,1,1,1,1,1,1,1,1,1,1,1,1,1,1,1,1,1,1,1,1,1,1,1,1,
1,1,1,1,1,1,1,6),(-1.,-0.984615384615383,-0.969230769230768,-0.953846153846152,
-0.938461538461537,-0.923076923076922,-0.907692307692306,-0.892307692307691,
-0.876923076923076,-0.86153846153846,-0.846153846153845,-0.83076923076923,
-0.815384615384614,-0.799999999999999,-0.784615384615384,-0.769230769230768,
-0.753846153846153,-0.738461538461538,-0.723076923076922,-0.707692307692307,
-0.692307692307692,-0.676923076923076,-0.661538461538461,-0.646153846153846,
-0.63076923076923,-0.615384615384615,-0.6,-0.584615384615384,-0.569230769230769,
-0.553846153846154,-0.538461538461538,-0.523076923076923,-0.507692307692308,
-0.492307692307692,-0.476923076923077,-0.461538461538462,-0.446153846153846,
-0.430769230769231,-0.415384615384615,-0.4,-0.384615384615385,-0.369230769230769,
-0.353846153846154,-0.338461538461538,-0.323076923076923,-0.307692307692308,
-0.292307692307692,-0.276923076923077,-0.261538461538462,-0.246153846153846,
-0.230769230769231,-0.215384615384615,-0.2,-0.184615384615385,-0.169230769230769,
-0.153846153846154,-0.138461538461538,-0.123076923076923,-0.107692307692308,
-0.0923076923076923,-0.0769230769230769,-0.0615384615384615,-0.0461538461538462,
-0.0307692307692308,-0.0153846153846154,0.),.UNSPECIFIED.)
CURVE()
GEOMETRIC_REPRESENTATION_ITEM()
RATIONAL_B_SPLINE_CURVE((1.,1.,1.,1.,1.,1.,1.,1.,1.,1.,1.,1.,1.,1.,1.,1.,
1.,1.,1.,1.,1.,1.,1.,1.,1.,1.,1.,1.,1.,1.,1.,1.,1.,1.,1.,1.,1.,1.,1.,1.,
1.,1.,1.,1.,1.,1.,1.,1.,1.,1.,1.,1.,1.,1.,1.,1.,1.,1.,1.,1.,1.,1.,1.,1.,
1.,1.,1.,1.,1.,1.))
REPRESENTATION_ITEM('')
);
#300=(
BOUNDED_CURVE()
B_SPLINE_CURVE(5,(#42701,#42702,#42703,#42704,#42705,#42706,#42707,#42708,
#42709,#42710,#42711,#42712,#42713,#42714,#42715,#42716,#42717,#42718,#42719,
#42720,#42721,#42722,#42723,#42724,#42725,#42726,#42727,#42728,#42729,#42730,
#42731,#42732,#42733,#42734,#42735,#42736,#42737,#42738,#42739,#42740,#42741,
#42742,#42743,#42744,#42745,#42746,#42747,#42748,#42749,#42750,#42751,#42752,
#42753,#42754,#42755,#42756,#42757,#42758,#42759,#42760,#42761,#42762,#42763,
#42764,#42765,#42766,#42767,#42768,#42769,#42770),.UNSPECIFIED.,.F.,.F.)
B_SPLINE_CURVE_WITH_KNOTS((6,1,1,1,1,1,1,1,1,1,1,1,1,1,1,1,1,1,1,1,1,1,
1,1,1,1,1,1,1,1,1,1,1,1,1,1,1,1,1,1,1,1,1,1,1,1,1,1,1,1,1,1,1,1,1,1,1,1,
1,1,1,1,1,1,1,6),(-1.,-0.984615384615383,-0.969230769230768,-0.953846153846152,
-0.938461538461537,-0.923076923076922,-0.907692307692306,-0.892307692307691,
-0.876923076923076,-0.86153846153846,-0.846153846153845,-0.83076923076923,
-0.815384615384614,-0.799999999999999,-0.784615384615384,-0.769230769230768,
-0.753846153846153,-0.738461538461538,-0.723076923076922,-0.707692307692307,
-0.692307692307692,-0.676923076923076,-0.661538461538461,-0.646153846153846,
-0.63076923076923,-0.615384615384615,-0.6,-0.584615384615384,-0.569230769230769,
-0.553846153846154,-0.538461538461538,-0.523076923076923,-0.507692307692308,
-0.492307692307692,-0.476923076923077,-0.461538461538462,-0.446153846153846,
-0.430769230769231,-0.415384615384615,-0.4,-0.384615384615385,-0.369230769230769,
-0.353846153846154,-0.338461538461538,-0.323076923076923,-0.307692307692308,
-0.292307692307692,-0.276923076923077,-0.261538461538462,-0.246153846153846,
-0.230769230769231,-0.215384615384615,-0.2,-0.184615384615385,-0.169230769230769,
-0.153846153846154,-0.138461538461538,-0.123076923076923,-0.107692307692308,
-0.0923076923076923,-0.0769230769230769,-0.0615384615384615,-0.0461538461538462,
-0.0307692307692308,-0.0153846153846154,0.),.UNSPECIFIED.)
CURVE()
GEOMETRIC_REPRESENTATION_ITEM()
RATIONAL_B_SPLINE_CURVE((1.,1.,1.,1.,1.,1.,1.,1.,1.,1.,1.,1.,1.,1.,1.,1.,
1.,1.,1.,1.,1.,1.,1.,1.,1.,1.,1.,1.,1.,1.,1.,1.,1.,1.,1.,1.,1.,1.,1.,1.,
1.,1.,1.,1.,1.,1.,1.,1.,1.,1.,1.,1.,1.,1.,1.,1.,1.,1.,1.,1.,1.,1.,1.,1.,
1.,1.,1.,1.,1.,1.))
REPRESENTATION_ITEM('')
);
#301=(
BOUNDED_CURVE()
B_SPLINE_CURVE(5,(#42917,#42918,#42919,#42920,#42921,#42922,#42923,#42924,
#42925,#42926,#42927,#42928,#42929,#42930,#42931,#42932,#42933,#42934,#42935,
#42936,#42937,#42938,#42939,#42940,#42941,#42942,#42943,#42944,#42945,#42946,
#42947,#42948,#42949,#42950,#42951,#42952,#42953,#42954,#42955,#42956,#42957,
#42958,#42959,#42960,#42961,#42962,#42963,#42964,#42965,#42966,#42967,#42968,
#42969,#42970,#42971,#42972,#42973,#42974,#42975,#42976,#42977,#42978,#42979,
#42980,#42981,#42982,#42983,#42984,#42985,#42986),.UNSPECIFIED.,.F.,.F.)
B_SPLINE_CURVE_WITH_KNOTS((6,1,1,1,1,1,1,1,1,1,1,1,1,1,1,1,1,1,1,1,1,1,
1,1,1,1,1,1,1,1,1,1,1,1,1,1,1,1,1,1,1,1,1,1,1,1,1,1,1,1,1,1,1,1,1,1,1,1,
1,1,1,1,1,1,1,6),(-1.,-0.984615384615383,-0.969230769230768,-0.953846153846152,
-0.938461538461537,-0.923076923076922,-0.907692307692306,-0.892307692307691,
-0.876923076923076,-0.86153846153846,-0.846153846153845,-0.83076923076923,
-0.815384615384614,-0.799999999999999,-0.784615384615384,-0.769230769230768,
-0.753846153846153,-0.738461538461538,-0.723076923076922,-0.707692307692307,
-0.692307692307692,-0.676923076923076,-0.661538461538461,-0.646153846153846,
-0.63076923076923,-0.615384615384615,-0.6,-0.584615384615384,-0.569230769230769,
-0.553846153846154,-0.538461538461538,-0.523076923076923,-0.507692307692308,
-0.492307692307692,-0.476923076923077,-0.461538461538462,-0.446153846153846,
-0.430769230769231,-0.415384615384615,-0.4,-0.384615384615385,-0.369230769230769,
-0.353846153846154,-0.338461538461538,-0.323076923076923,-0.307692307692308,
-0.292307692307692,-0.276923076923077,-0.261538461538462,-0.246153846153846,
-0.230769230769231,-0.215384615384615,-0.2,-0.184615384615385,-0.169230769230769,
-0.153846153846154,-0.138461538461538,-0.123076923076923,-0.107692307692308,
-0.0923076923076923,-0.0769230769230769,-0.0615384615384615,-0.0461538461538462,
-0.0307692307692308,-0.0153846153846154,0.),.UNSPECIFIED.)
CURVE()
GEOMETRIC_REPRESENTATION_ITEM()
RATIONAL_B_SPLINE_CURVE((1.,1.,1.,1.,1.,1.,1.,1.,1.,1.,1.,1.,1.,1.,1.,1.,
1.,1.,1.,1.,1.,1.,1.,1.,1.,1.,1.,1.,1.,1.,1.,1.,1.,1.,1.,1.,1.,1.,1.,1.,
1.,1.,1.,1.,1.,1.,1.,1.,1.,1.,1.,1.,1.,1.,1.,1.,1.,1.,1.,1.,1.,1.,1.,1.,
1.,1.,1.,1.,1.,1.))
REPRESENTATION_ITEM('')
);
#302=(
BOUNDED_CURVE()
B_SPLINE_CURVE(5,(#43133,#43134,#43135,#43136,#43137,#43138,#43139,#43140,
#43141,#43142,#43143,#43144,#43145,#43146,#43147,#43148,#43149,#43150,#43151,
#43152,#43153,#43154,#43155,#43156,#43157,#43158,#43159,#43160,#43161,#43162,
#43163,#43164,#43165,#43166,#43167,#43168,#43169,#43170,#43171,#43172,#43173,
#43174,#43175,#43176,#43177,#43178,#43179,#43180,#43181,#43182,#43183,#43184,
#43185,#43186,#43187,#43188,#43189,#43190,#43191,#43192,#43193,#43194,#43195,
#43196,#43197,#43198,#43199,#43200,#43201,#43202),.UNSPECIFIED.,.F.,.F.)
B_SPLINE_CURVE_WITH_KNOTS((6,1,1,1,1,1,1,1,1,1,1,1,1,1,1,1,1,1,1,1,1,1,
1,1,1,1,1,1,1,1,1,1,1,1,1,1,1,1,1,1,1,1,1,1,1,1,1,1,1,1,1,1,1,1,1,1,1,1,
1,1,1,1,1,1,1,6),(-1.,-0.984615384615383,-0.969230769230768,-0.953846153846152,
-0.938461538461537,-0.923076923076922,-0.907692307692306,-0.892307692307691,
-0.876923076923076,-0.86153846153846,-0.846153846153845,-0.83076923076923,
-0.815384615384614,-0.799999999999999,-0.784615384615384,-0.769230769230768,
-0.753846153846153,-0.738461538461538,-0.723076923076922,-0.707692307692307,
-0.692307692307692,-0.676923076923076,-0.661538461538461,-0.646153846153846,
-0.63076923076923,-0.615384615384615,-0.6,-0.584615384615384,-0.569230769230769,
-0.553846153846154,-0.538461538461538,-0.523076923076923,-0.507692307692308,
-0.492307692307692,-0.476923076923077,-0.461538461538462,-0.446153846153846,
-0.430769230769231,-0.415384615384615,-0.4,-0.384615384615385,-0.369230769230769,
-0.353846153846154,-0.338461538461538,-0.323076923076923,-0.307692307692308,
-0.292307692307692,-0.276923076923077,-0.261538461538462,-0.246153846153846,
-0.230769230769231,-0.215384615384615,-0.2,-0.184615384615385,-0.169230769230769,
-0.153846153846154,-0.138461538461538,-0.123076923076923,-0.107692307692308,
-0.0923076923076923,-0.0769230769230769,-0.0615384615384615,-0.0461538461538462,
-0.0307692307692308,-0.0153846153846154,0.),.UNSPECIFIED.)
CURVE()
GEOMETRIC_REPRESENTATION_ITEM()
RATIONAL_B_SPLINE_CURVE((1.,1.,1.,1.,1.,1.,1.,1.,1.,1.,1.,1.,1.,1.,1.,1.,
1.,1.,1.,1.,1.,1.,1.,1.,1.,1.,1.,1.,1.,1.,1.,1.,1.,1.,1.,1.,1.,1.,1.,1.,
1.,1.,1.,1.,1.,1.,1.,1.,1.,1.,1.,1.,1.,1.,1.,1.,1.,1.,1.,1.,1.,1.,1.,1.,
1.,1.,1.,1.,1.,1.))
REPRESENTATION_ITEM('')
);
#303=(
BOUNDED_CURVE()
B_SPLINE_CURVE(5,(#43349,#43350,#43351,#43352,#43353,#43354,#43355,#43356,
#43357,#43358,#43359,#43360,#43361,#43362,#43363,#43364,#43365,#43366,#43367,
#43368,#43369,#43370,#43371,#43372,#43373,#43374,#43375,#43376,#43377,#43378,
#43379,#43380,#43381,#43382,#43383,#43384,#43385,#43386,#43387,#43388,#43389,
#43390,#43391,#43392,#43393,#43394,#43395,#43396,#43397,#43398,#43399,#43400,
#43401,#43402,#43403,#43404,#43405,#43406,#43407,#43408,#43409,#43410,#43411,
#43412,#43413,#43414,#43415,#43416,#43417,#43418),.UNSPECIFIED.,.F.,.F.)
B_SPLINE_CURVE_WITH_KNOTS((6,1,1,1,1,1,1,1,1,1,1,1,1,1,1,1,1,1,1,1,1,1,
1,1,1,1,1,1,1,1,1,1,1,1,1,1,1,1,1,1,1,1,1,1,1,1,1,1,1,1,1,1,1,1,1,1,1,1,
1,1,1,1,1,1,1,6),(-1.,-0.984615384615383,-0.969230769230768,-0.953846153846152,
-0.938461538461537,-0.923076923076922,-0.907692307692306,-0.892307692307691,
-0.876923076923076,-0.86153846153846,-0.846153846153845,-0.83076923076923,
-0.815384615384614,-0.799999999999999,-0.784615384615384,-0.769230769230768,
-0.753846153846153,-0.738461538461538,-0.723076923076922,-0.707692307692307,
-0.692307692307692,-0.676923076923076,-0.661538461538461,-0.646153846153846,
-0.63076923076923,-0.615384615384615,-0.6,-0.584615384615384,-0.569230769230769,
-0.553846153846154,-0.538461538461538,-0.523076923076923,-0.507692307692308,
-0.492307692307692,-0.476923076923077,-0.461538461538462,-0.446153846153846,
-0.430769230769231,-0.415384615384615,-0.4,-0.384615384615385,-0.369230769230769,
-0.353846153846154,-0.338461538461538,-0.323076923076923,-0.307692307692308,
-0.292307692307692,-0.276923076923077,-0.261538461538462,-0.246153846153846,
-0.230769230769231,-0.215384615384615,-0.2,-0.184615384615385,-0.169230769230769,
-0.153846153846154,-0.138461538461538,-0.123076923076923,-0.107692307692308,
-0.0923076923076923,-0.0769230769230769,-0.0615384615384615,-0.0461538461538462,
-0.0307692307692308,-0.0153846153846154,0.),.UNSPECIFIED.)
CURVE()
GEOMETRIC_REPRESENTATION_ITEM()
RATIONAL_B_SPLINE_CURVE((1.,1.,1.,1.,1.,1.,1.,1.,1.,1.,1.,1.,1.,1.,1.,1.,
1.,1.,1.,1.,1.,1.,1.,1.,1.,1.,1.,1.,1.,1.,1.,1.,1.,1.,1.,1.,1.,1.,1.,1.,
1.,1.,1.,1.,1.,1.,1.,1.,1.,1.,1.,1.,1.,1.,1.,1.,1.,1.,1.,1.,1.,1.,1.,1.,
1.,1.,1.,1.,1.,1.))
REPRESENTATION_ITEM('')
);
#304=(
BOUNDED_CURVE()
B_SPLINE_CURVE(5,(#43565,#43566,#43567,#43568,#43569,#43570,#43571,#43572,
#43573,#43574,#43575,#43576,#43577,#43578,#43579,#43580,#43581,#43582,#43583,
#43584,#43585,#43586,#43587,#43588,#43589,#43590,#43591,#43592,#43593,#43594,
#43595,#43596,#43597,#43598,#43599,#43600,#43601,#43602,#43603,#43604,#43605,
#43606,#43607,#43608,#43609,#43610,#43611,#43612,#43613,#43614,#43615,#43616,
#43617,#43618,#43619,#43620,#43621,#43622,#43623,#43624,#43625,#43626,#43627,
#43628,#43629,#43630,#43631,#43632,#43633,#43634),.UNSPECIFIED.,.F.,.F.)
B_SPLINE_CURVE_WITH_KNOTS((6,1,1,1,1,1,1,1,1,1,1,1,1,1,1,1,1,1,1,1,1,1,
1,1,1,1,1,1,1,1,1,1,1,1,1,1,1,1,1,1,1,1,1,1,1,1,1,1,1,1,1,1,1,1,1,1,1,1,
1,1,1,1,1,1,1,6),(-1.,-0.984615384615383,-0.969230769230768,-0.953846153846152,
-0.938461538461537,-0.923076923076922,-0.907692307692306,-0.892307692307691,
-0.876923076923076,-0.86153846153846,-0.846153846153845,-0.83076923076923,
-0.815384615384614,-0.799999999999999,-0.784615384615384,-0.769230769230768,
-0.753846153846153,-0.738461538461538,-0.723076923076922,-0.707692307692307,
-0.692307692307692,-0.676923076923076,-0.661538461538461,-0.646153846153846,
-0.63076923076923,-0.615384615384615,-0.6,-0.584615384615384,-0.569230769230769,
-0.553846153846154,-0.538461538461538,-0.523076923076923,-0.507692307692308,
-0.492307692307692,-0.476923076923077,-0.461538461538462,-0.446153846153846,
-0.430769230769231,-0.415384615384615,-0.4,-0.384615384615385,-0.369230769230769,
-0.353846153846154,-0.338461538461538,-0.323076923076923,-0.307692307692308,
-0.292307692307692,-0.276923076923077,-0.261538461538462,-0.246153846153846,
-0.230769230769231,-0.215384615384615,-0.2,-0.184615384615385,-0.169230769230769,
-0.153846153846154,-0.138461538461538,-0.123076923076923,-0.107692307692308,
-0.0923076923076923,-0.0769230769230769,-0.0615384615384615,-0.0461538461538462,
-0.0307692307692308,-0.0153846153846154,0.),.UNSPECIFIED.)
CURVE()
GEOMETRIC_REPRESENTATION_ITEM()
RATIONAL_B_SPLINE_CURVE((1.,1.,1.,1.,1.,1.,1.,1.,1.,1.,1.,1.,1.,1.,1.,1.,
1.,1.,1.,1.,1.,1.,1.,1.,1.,1.,1.,1.,1.,1.,1.,1.,1.,1.,1.,1.,1.,1.,1.,1.,
1.,1.,1.,1.,1.,1.,1.,1.,1.,1.,1.,1.,1.,1.,1.,1.,1.,1.,1.,1.,1.,1.,1.,1.,
1.,1.,1.,1.,1.,1.))
REPRESENTATION_ITEM('')
);
#305=(
BOUNDED_CURVE()
B_SPLINE_CURVE(5,(#43781,#43782,#43783,#43784,#43785,#43786,#43787,#43788,
#43789,#43790,#43791,#43792,#43793,#43794,#43795,#43796,#43797,#43798,#43799,
#43800,#43801,#43802,#43803,#43804,#43805,#43806,#43807,#43808,#43809,#43810,
#43811,#43812,#43813,#43814,#43815,#43816,#43817,#43818,#43819,#43820,#43821,
#43822,#43823,#43824,#43825,#43826,#43827,#43828,#43829,#43830,#43831,#43832,
#43833,#43834,#43835,#43836,#43837,#43838,#43839,#43840,#43841,#43842,#43843,
#43844,#43845,#43846,#43847,#43848,#43849,#43850),.UNSPECIFIED.,.F.,.F.)
B_SPLINE_CURVE_WITH_KNOTS((6,1,1,1,1,1,1,1,1,1,1,1,1,1,1,1,1,1,1,1,1,1,
1,1,1,1,1,1,1,1,1,1,1,1,1,1,1,1,1,1,1,1,1,1,1,1,1,1,1,1,1,1,1,1,1,1,1,1,
1,1,1,1,1,1,1,6),(-1.,-0.984615384615383,-0.969230769230768,-0.953846153846152,
-0.938461538461537,-0.923076923076922,-0.907692307692306,-0.892307692307691,
-0.876923076923076,-0.86153846153846,-0.846153846153845,-0.83076923076923,
-0.815384615384614,-0.799999999999999,-0.784615384615384,-0.769230769230768,
-0.753846153846153,-0.738461538461538,-0.723076923076922,-0.707692307692307,
-0.692307692307692,-0.676923076923076,-0.661538461538461,-0.646153846153846,
-0.63076923076923,-0.615384615384615,-0.6,-0.584615384615384,-0.569230769230769,
-0.553846153846154,-0.538461538461538,-0.523076923076923,-0.507692307692308,
-0.492307692307692,-0.476923076923077,-0.461538461538462,-0.446153846153846,
-0.430769230769231,-0.415384615384615,-0.4,-0.384615384615385,-0.369230769230769,
-0.353846153846154,-0.338461538461538,-0.323076923076923,-0.307692307692308,
-0.292307692307692,-0.276923076923077,-0.261538461538462,-0.246153846153846,
-0.230769230769231,-0.215384615384615,-0.2,-0.184615384615385,-0.169230769230769,
-0.153846153846154,-0.138461538461538,-0.123076923076923,-0.107692307692308,
-0.0923076923076923,-0.0769230769230769,-0.0615384615384615,-0.0461538461538462,
-0.0307692307692308,-0.0153846153846154,0.),.UNSPECIFIED.)
CURVE()
GEOMETRIC_REPRESENTATION_ITEM()
RATIONAL_B_SPLINE_CURVE((1.,1.,1.,1.,1.,1.,1.,1.,1.,1.,1.,1.,1.,1.,1.,1.,
1.,1.,1.,1.,1.,1.,1.,1.,1.,1.,1.,1.,1.,1.,1.,1.,1.,1.,1.,1.,1.,1.,1.,1.,
1.,1.,1.,1.,1.,1.,1.,1.,1.,1.,1.,1.,1.,1.,1.,1.,1.,1.,1.,1.,1.,1.,1.,1.,
1.,1.,1.,1.,1.,1.))
REPRESENTATION_ITEM('')
);
#306=(
BOUNDED_CURVE()
B_SPLINE_CURVE(5,(#43997,#43998,#43999,#44000,#44001,#44002,#44003,#44004,
#44005,#44006,#44007,#44008,#44009,#44010,#44011,#44012,#44013,#44014,#44015,
#44016,#44017,#44018,#44019,#44020,#44021,#44022,#44023,#44024,#44025,#44026,
#44027,#44028,#44029,#44030,#44031,#44032,#44033,#44034,#44035,#44036,#44037,
#44038,#44039,#44040,#44041,#44042,#44043,#44044,#44045,#44046,#44047,#44048,
#44049,#44050,#44051,#44052,#44053,#44054,#44055,#44056,#44057,#44058,#44059,
#44060,#44061,#44062,#44063,#44064,#44065,#44066),.UNSPECIFIED.,.F.,.F.)
B_SPLINE_CURVE_WITH_KNOTS((6,1,1,1,1,1,1,1,1,1,1,1,1,1,1,1,1,1,1,1,1,1,
1,1,1,1,1,1,1,1,1,1,1,1,1,1,1,1,1,1,1,1,1,1,1,1,1,1,1,1,1,1,1,1,1,1,1,1,
1,1,1,1,1,1,1,6),(-1.,-0.984615384615383,-0.969230769230768,-0.953846153846152,
-0.938461538461537,-0.923076923076922,-0.907692307692306,-0.892307692307691,
-0.876923076923076,-0.86153846153846,-0.846153846153845,-0.83076923076923,
-0.815384615384614,-0.799999999999999,-0.784615384615384,-0.769230769230768,
-0.753846153846153,-0.738461538461538,-0.723076923076922,-0.707692307692307,
-0.692307692307692,-0.676923076923076,-0.661538461538461,-0.646153846153846,
-0.63076923076923,-0.615384615384615,-0.6,-0.584615384615384,-0.569230769230769,
-0.553846153846154,-0.538461538461538,-0.523076923076923,-0.507692307692308,
-0.492307692307692,-0.476923076923077,-0.461538461538462,-0.446153846153846,
-0.430769230769231,-0.415384615384615,-0.4,-0.384615384615385,-0.369230769230769,
-0.353846153846154,-0.338461538461538,-0.323076923076923,-0.307692307692308,
-0.292307692307692,-0.276923076923077,-0.261538461538462,-0.246153846153846,
-0.230769230769231,-0.215384615384615,-0.2,-0.184615384615385,-0.169230769230769,
-0.153846153846154,-0.138461538461538,-0.123076923076923,-0.107692307692308,
-0.0923076923076923,-0.0769230769230769,-0.0615384615384615,-0.0461538461538462,
-0.0307692307692308,-0.0153846153846154,0.),.UNSPECIFIED.)
CURVE()
GEOMETRIC_REPRESENTATION_ITEM()
RATIONAL_B_SPLINE_CURVE((1.,1.,1.,1.,1.,1.,1.,1.,1.,1.,1.,1.,1.,1.,1.,1.,
1.,1.,1.,1.,1.,1.,1.,1.,1.,1.,1.,1.,1.,1.,1.,1.,1.,1.,1.,1.,1.,1.,1.,1.,
1.,1.,1.,1.,1.,1.,1.,1.,1.,1.,1.,1.,1.,1.,1.,1.,1.,1.,1.,1.,1.,1.,1.,1.,
1.,1.,1.,1.,1.,1.))
REPRESENTATION_ITEM('')
);
#307=(
BOUNDED_CURVE()
B_SPLINE_CURVE(5,(#44213,#44214,#44215,#44216,#44217,#44218,#44219,#44220,
#44221,#44222,#44223,#44224,#44225,#44226,#44227,#44228,#44229,#44230,#44231,
#44232,#44233,#44234,#44235,#44236,#44237,#44238,#44239,#44240,#44241,#44242,
#44243,#44244,#44245,#44246,#44247,#44248,#44249,#44250,#44251,#44252,#44253,
#44254,#44255,#44256,#44257,#44258,#44259,#44260,#44261,#44262,#44263,#44264,
#44265,#44266,#44267,#44268,#44269,#44270,#44271,#44272,#44273,#44274,#44275,
#44276,#44277,#44278,#44279,#44280,#44281,#44282),.UNSPECIFIED.,.F.,.F.)
B_SPLINE_CURVE_WITH_KNOTS((6,1,1,1,1,1,1,1,1,1,1,1,1,1,1,1,1,1,1,1,1,1,
1,1,1,1,1,1,1,1,1,1,1,1,1,1,1,1,1,1,1,1,1,1,1,1,1,1,1,1,1,1,1,1,1,1,1,1,
1,1,1,1,1,1,1,6),(-1.,-0.984615384615383,-0.969230769230768,-0.953846153846152,
-0.938461538461537,-0.923076923076922,-0.907692307692306,-0.892307692307691,
-0.876923076923076,-0.86153846153846,-0.846153846153845,-0.83076923076923,
-0.815384615384614,-0.799999999999999,-0.784615384615384,-0.769230769230768,
-0.753846153846153,-0.738461538461538,-0.723076923076922,-0.707692307692307,
-0.692307692307692,-0.676923076923076,-0.661538461538461,-0.646153846153846,
-0.63076923076923,-0.615384615384615,-0.6,-0.584615384615384,-0.569230769230769,
-0.553846153846154,-0.538461538461538,-0.523076923076923,-0.507692307692308,
-0.492307692307692,-0.476923076923077,-0.461538461538462,-0.446153846153846,
-0.430769230769231,-0.415384615384615,-0.4,-0.384615384615385,-0.369230769230769,
-0.353846153846154,-0.338461538461538,-0.323076923076923,-0.307692307692308,
-0.292307692307692,-0.276923076923077,-0.261538461538462,-0.246153846153846,
-0.230769230769231,-0.215384615384615,-0.2,-0.184615384615385,-0.169230769230769,
-0.153846153846154,-0.138461538461538,-0.123076923076923,-0.107692307692308,
-0.0923076923076923,-0.0769230769230769,-0.0615384615384615,-0.0461538461538462,
-0.0307692307692308,-0.0153846153846154,0.),.UNSPECIFIED.)
CURVE()
GEOMETRIC_REPRESENTATION_ITEM()
RATIONAL_B_SPLINE_CURVE((1.,1.,1.,1.,1.,1.,1.,1.,1.,1.,1.,1.,1.,1.,1.,1.,
1.,1.,1.,1.,1.,1.,1.,1.,1.,1.,1.,1.,1.,1.,1.,1.,1.,1.,1.,1.,1.,1.,1.,1.,
1.,1.,1.,1.,1.,1.,1.,1.,1.,1.,1.,1.,1.,1.,1.,1.,1.,1.,1.,1.,1.,1.,1.,1.,
1.,1.,1.,1.,1.,1.))
REPRESENTATION_ITEM('')
);
#308=(
BOUNDED_CURVE()
B_SPLINE_CURVE(5,(#44429,#44430,#44431,#44432,#44433,#44434,#44435,#44436,
#44437,#44438,#44439,#44440,#44441,#44442,#44443,#44444,#44445,#44446,#44447,
#44448,#44449,#44450,#44451,#44452,#44453,#44454,#44455,#44456,#44457,#44458,
#44459,#44460,#44461,#44462,#44463,#44464,#44465,#44466,#44467,#44468,#44469,
#44470,#44471,#44472,#44473,#44474,#44475,#44476,#44477,#44478,#44479,#44480,
#44481,#44482,#44483,#44484,#44485,#44486,#44487,#44488,#44489,#44490,#44491,
#44492,#44493,#44494,#44495,#44496,#44497,#44498),.UNSPECIFIED.,.F.,.F.)
B_SPLINE_CURVE_WITH_KNOTS((6,1,1,1,1,1,1,1,1,1,1,1,1,1,1,1,1,1,1,1,1,1,
1,1,1,1,1,1,1,1,1,1,1,1,1,1,1,1,1,1,1,1,1,1,1,1,1,1,1,1,1,1,1,1,1,1,1,1,
1,1,1,1,1,1,1,6),(-1.,-0.984615384615383,-0.969230769230768,-0.953846153846152,
-0.938461538461537,-0.923076923076922,-0.907692307692306,-0.892307692307691,
-0.876923076923076,-0.86153846153846,-0.846153846153845,-0.83076923076923,
-0.815384615384614,-0.799999999999999,-0.784615384615384,-0.769230769230768,
-0.753846153846153,-0.738461538461538,-0.723076923076922,-0.707692307692307,
-0.692307692307692,-0.676923076923076,-0.661538461538461,-0.646153846153846,
-0.63076923076923,-0.615384615384615,-0.6,-0.584615384615384,-0.569230769230769,
-0.553846153846154,-0.538461538461538,-0.523076923076923,-0.507692307692308,
-0.492307692307692,-0.476923076923077,-0.461538461538462,-0.446153846153846,
-0.430769230769231,-0.415384615384615,-0.4,-0.384615384615385,-0.369230769230769,
-0.353846153846154,-0.338461538461538,-0.323076923076923,-0.307692307692308,
-0.292307692307692,-0.276923076923077,-0.261538461538462,-0.246153846153846,
-0.230769230769231,-0.215384615384615,-0.2,-0.184615384615385,-0.169230769230769,
-0.153846153846154,-0.138461538461538,-0.123076923076923,-0.107692307692308,
-0.0923076923076923,-0.0769230769230769,-0.0615384615384615,-0.0461538461538462,
-0.0307692307692308,-0.0153846153846154,0.),.UNSPECIFIED.)
CURVE()
GEOMETRIC_REPRESENTATION_ITEM()
RATIONAL_B_SPLINE_CURVE((1.,1.,1.,1.,1.,1.,1.,1.,1.,1.,1.,1.,1.,1.,1.,1.,
1.,1.,1.,1.,1.,1.,1.,1.,1.,1.,1.,1.,1.,1.,1.,1.,1.,1.,1.,1.,1.,1.,1.,1.,
1.,1.,1.,1.,1.,1.,1.,1.,1.,1.,1.,1.,1.,1.,1.,1.,1.,1.,1.,1.,1.,1.,1.,1.,
1.,1.,1.,1.,1.,1.))
REPRESENTATION_ITEM('')
);
#309=(
BOUNDED_CURVE()
B_SPLINE_CURVE(5,(#44645,#44646,#44647,#44648,#44649,#44650,#44651,#44652,
#44653,#44654,#44655,#44656,#44657,#44658,#44659,#44660,#44661,#44662,#44663,
#44664,#44665,#44666,#44667,#44668,#44669,#44670,#44671,#44672,#44673,#44674,
#44675,#44676,#44677,#44678,#44679,#44680,#44681,#44682,#44683,#44684,#44685,
#44686,#44687,#44688,#44689,#44690,#44691,#44692,#44693,#44694,#44695,#44696,
#44697,#44698,#44699,#44700,#44701,#44702,#44703,#44704,#44705,#44706,#44707,
#44708,#44709,#44710,#44711,#44712,#44713,#44714),.UNSPECIFIED.,.F.,.F.)
B_SPLINE_CURVE_WITH_KNOTS((6,1,1,1,1,1,1,1,1,1,1,1,1,1,1,1,1,1,1,1,1,1,
1,1,1,1,1,1,1,1,1,1,1,1,1,1,1,1,1,1,1,1,1,1,1,1,1,1,1,1,1,1,1,1,1,1,1,1,
1,1,1,1,1,1,1,6),(-1.,-0.984615384615383,-0.969230769230768,-0.953846153846152,
-0.938461538461537,-0.923076923076922,-0.907692307692306,-0.892307692307691,
-0.876923076923076,-0.86153846153846,-0.846153846153845,-0.83076923076923,
-0.815384615384614,-0.799999999999999,-0.784615384615384,-0.769230769230768,
-0.753846153846153,-0.738461538461538,-0.723076923076922,-0.707692307692307,
-0.692307692307692,-0.676923076923076,-0.661538461538461,-0.646153846153846,
-0.63076923076923,-0.615384615384615,-0.6,-0.584615384615384,-0.569230769230769,
-0.553846153846154,-0.538461538461538,-0.523076923076923,-0.507692307692308,
-0.492307692307692,-0.476923076923077,-0.461538461538462,-0.446153846153846,
-0.430769230769231,-0.415384615384615,-0.4,-0.384615384615385,-0.369230769230769,
-0.353846153846154,-0.338461538461538,-0.323076923076923,-0.307692307692308,
-0.292307692307692,-0.276923076923077,-0.261538461538462,-0.246153846153846,
-0.230769230769231,-0.215384615384615,-0.2,-0.184615384615385,-0.169230769230769,
-0.153846153846154,-0.138461538461538,-0.123076923076923,-0.107692307692308,
-0.0923076923076923,-0.0769230769230769,-0.0615384615384615,-0.0461538461538462,
-0.0307692307692308,-0.0153846153846154,0.),.UNSPECIFIED.)
CURVE()
GEOMETRIC_REPRESENTATION_ITEM()
RATIONAL_B_SPLINE_CURVE((1.,1.,1.,1.,1.,1.,1.,1.,1.,1.,1.,1.,1.,1.,1.,1.,
1.,1.,1.,1.,1.,1.,1.,1.,1.,1.,1.,1.,1.,1.,1.,1.,1.,1.,1.,1.,1.,1.,1.,1.,
1.,1.,1.,1.,1.,1.,1.,1.,1.,1.,1.,1.,1.,1.,1.,1.,1.,1.,1.,1.,1.,1.,1.,1.,
1.,1.,1.,1.,1.,1.))
REPRESENTATION_ITEM('')
);
#310=(
BOUNDED_CURVE()
B_SPLINE_CURVE(5,(#44861,#44862,#44863,#44864,#44865,#44866,#44867,#44868,
#44869,#44870,#44871,#44872,#44873,#44874,#44875,#44876,#44877,#44878,#44879,
#44880,#44881,#44882,#44883,#44884,#44885,#44886,#44887,#44888,#44889,#44890,
#44891,#44892,#44893,#44894,#44895,#44896,#44897,#44898,#44899,#44900,#44901,
#44902,#44903,#44904,#44905,#44906,#44907,#44908,#44909,#44910,#44911,#44912,
#44913,#44914,#44915,#44916,#44917,#44918,#44919,#44920,#44921,#44922,#44923,
#44924,#44925,#44926,#44927,#44928,#44929,#44930),.UNSPECIFIED.,.F.,.F.)
B_SPLINE_CURVE_WITH_KNOTS((6,1,1,1,1,1,1,1,1,1,1,1,1,1,1,1,1,1,1,1,1,1,
1,1,1,1,1,1,1,1,1,1,1,1,1,1,1,1,1,1,1,1,1,1,1,1,1,1,1,1,1,1,1,1,1,1,1,1,
1,1,1,1,1,1,1,6),(-1.,-0.984615384615383,-0.969230769230768,-0.953846153846152,
-0.938461538461537,-0.923076923076922,-0.907692307692306,-0.892307692307691,
-0.876923076923076,-0.86153846153846,-0.846153846153845,-0.83076923076923,
-0.815384615384614,-0.799999999999999,-0.784615384615384,-0.769230769230768,
-0.753846153846153,-0.738461538461538,-0.723076923076922,-0.707692307692307,
-0.692307692307692,-0.676923076923076,-0.661538461538461,-0.646153846153846,
-0.63076923076923,-0.615384615384615,-0.6,-0.584615384615384,-0.569230769230769,
-0.553846153846154,-0.538461538461538,-0.523076923076923,-0.507692307692308,
-0.492307692307692,-0.476923076923077,-0.461538461538462,-0.446153846153846,
-0.430769230769231,-0.415384615384615,-0.4,-0.384615384615385,-0.369230769230769,
-0.353846153846154,-0.338461538461538,-0.323076923076923,-0.307692307692308,
-0.292307692307692,-0.276923076923077,-0.261538461538462,-0.246153846153846,
-0.230769230769231,-0.215384615384615,-0.2,-0.184615384615385,-0.169230769230769,
-0.153846153846154,-0.138461538461538,-0.123076923076923,-0.107692307692308,
-0.0923076923076923,-0.0769230769230769,-0.0615384615384615,-0.0461538461538462,
-0.0307692307692308,-0.0153846153846154,0.),.UNSPECIFIED.)
CURVE()
GEOMETRIC_REPRESENTATION_ITEM()
RATIONAL_B_SPLINE_CURVE((1.,1.,1.,1.,1.,1.,1.,1.,1.,1.,1.,1.,1.,1.,1.,1.,
1.,1.,1.,1.,1.,1.,1.,1.,1.,1.,1.,1.,1.,1.,1.,1.,1.,1.,1.,1.,1.,1.,1.,1.,
1.,1.,1.,1.,1.,1.,1.,1.,1.,1.,1.,1.,1.,1.,1.,1.,1.,1.,1.,1.,1.,1.,1.,1.,
1.,1.,1.,1.,1.,1.))
REPRESENTATION_ITEM('')
);
#311=(
BOUNDED_CURVE()
B_SPLINE_CURVE(5,(#45077,#45078,#45079,#45080,#45081,#45082,#45083,#45084,
#45085,#45086,#45087,#45088,#45089,#45090,#45091,#45092,#45093,#45094,#45095,
#45096,#45097,#45098,#45099,#45100,#45101,#45102,#45103,#45104,#45105,#45106,
#45107,#45108,#45109,#45110,#45111,#45112,#45113,#45114,#45115,#45116,#45117,
#45118,#45119,#45120,#45121,#45122,#45123,#45124,#45125,#45126,#45127,#45128,
#45129,#45130,#45131,#45132,#45133,#45134,#45135,#45136,#45137,#45138,#45139,
#45140,#45141,#45142,#45143,#45144,#45145,#45146),.UNSPECIFIED.,.F.,.F.)
B_SPLINE_CURVE_WITH_KNOTS((6,1,1,1,1,1,1,1,1,1,1,1,1,1,1,1,1,1,1,1,1,1,
1,1,1,1,1,1,1,1,1,1,1,1,1,1,1,1,1,1,1,1,1,1,1,1,1,1,1,1,1,1,1,1,1,1,1,1,
1,1,1,1,1,1,1,6),(-1.,-0.984615384615383,-0.969230769230768,-0.953846153846152,
-0.938461538461537,-0.923076923076922,-0.907692307692306,-0.892307692307691,
-0.876923076923076,-0.86153846153846,-0.846153846153845,-0.83076923076923,
-0.815384615384614,-0.799999999999999,-0.784615384615384,-0.769230769230768,
-0.753846153846153,-0.738461538461538,-0.723076923076922,-0.707692307692307,
-0.692307692307692,-0.676923076923076,-0.661538461538461,-0.646153846153846,
-0.63076923076923,-0.615384615384615,-0.6,-0.584615384615384,-0.569230769230769,
-0.553846153846154,-0.538461538461538,-0.523076923076923,-0.507692307692308,
-0.492307692307692,-0.476923076923077,-0.461538461538462,-0.446153846153846,
-0.430769230769231,-0.415384615384615,-0.4,-0.384615384615385,-0.369230769230769,
-0.353846153846154,-0.338461538461538,-0.323076923076923,-0.307692307692308,
-0.292307692307692,-0.276923076923077,-0.261538461538462,-0.246153846153846,
-0.230769230769231,-0.215384615384615,-0.2,-0.184615384615385,-0.169230769230769,
-0.153846153846154,-0.138461538461538,-0.123076923076923,-0.107692307692308,
-0.0923076923076923,-0.0769230769230769,-0.0615384615384615,-0.0461538461538462,
-0.0307692307692308,-0.0153846153846154,0.),.UNSPECIFIED.)
CURVE()
GEOMETRIC_REPRESENTATION_ITEM()
RATIONAL_B_SPLINE_CURVE((1.,1.,1.,1.,1.,1.,1.,1.,1.,1.,1.,1.,1.,1.,1.,1.,
1.,1.,1.,1.,1.,1.,1.,1.,1.,1.,1.,1.,1.,1.,1.,1.,1.,1.,1.,1.,1.,1.,1.,1.,
1.,1.,1.,1.,1.,1.,1.,1.,1.,1.,1.,1.,1.,1.,1.,1.,1.,1.,1.,1.,1.,1.,1.,1.,
1.,1.,1.,1.,1.,1.))
REPRESENTATION_ITEM('')
);
#312=(
BOUNDED_CURVE()
B_SPLINE_CURVE(5,(#45293,#45294,#45295,#45296,#45297,#45298,#45299,#45300,
#45301,#45302,#45303,#45304,#45305,#45306,#45307,#45308,#45309,#45310,#45311,
#45312,#45313,#45314,#45315,#45316,#45317,#45318,#45319,#45320,#45321,#45322,
#45323,#45324,#45325,#45326,#45327,#45328,#45329,#45330,#45331,#45332,#45333,
#45334,#45335,#45336,#45337,#45338,#45339,#45340,#45341,#45342,#45343,#45344,
#45345,#45346,#45347,#45348,#45349,#45350,#45351,#45352,#45353,#45354,#45355,
#45356,#45357,#45358,#45359,#45360,#45361,#45362),.UNSPECIFIED.,.F.,.F.)
B_SPLINE_CURVE_WITH_KNOTS((6,1,1,1,1,1,1,1,1,1,1,1,1,1,1,1,1,1,1,1,1,1,
1,1,1,1,1,1,1,1,1,1,1,1,1,1,1,1,1,1,1,1,1,1,1,1,1,1,1,1,1,1,1,1,1,1,1,1,
1,1,1,1,1,1,1,6),(-1.,-0.984615384615383,-0.969230769230768,-0.953846153846152,
-0.938461538461537,-0.923076923076922,-0.907692307692306,-0.892307692307691,
-0.876923076923076,-0.86153846153846,-0.846153846153845,-0.83076923076923,
-0.815384615384614,-0.799999999999999,-0.784615384615384,-0.769230769230768,
-0.753846153846153,-0.738461538461538,-0.723076923076922,-0.707692307692307,
-0.692307692307692,-0.676923076923076,-0.661538461538461,-0.646153846153846,
-0.63076923076923,-0.615384615384615,-0.6,-0.584615384615384,-0.569230769230769,
-0.553846153846154,-0.538461538461538,-0.523076923076923,-0.507692307692308,
-0.492307692307692,-0.476923076923077,-0.461538461538462,-0.446153846153846,
-0.430769230769231,-0.415384615384615,-0.4,-0.384615384615385,-0.369230769230769,
-0.353846153846154,-0.338461538461538,-0.323076923076923,-0.307692307692308,
-0.292307692307692,-0.276923076923077,-0.261538461538462,-0.246153846153846,
-0.230769230769231,-0.215384615384615,-0.2,-0.184615384615385,-0.169230769230769,
-0.153846153846154,-0.138461538461538,-0.123076923076923,-0.107692307692308,
-0.0923076923076923,-0.0769230769230769,-0.0615384615384615,-0.0461538461538462,
-0.0307692307692308,-0.0153846153846154,0.),.UNSPECIFIED.)
CURVE()
GEOMETRIC_REPRESENTATION_ITEM()
RATIONAL_B_SPLINE_CURVE((1.,1.,1.,1.,1.,1.,1.,1.,1.,1.,1.,1.,1.,1.,1.,1.,
1.,1.,1.,1.,1.,1.,1.,1.,1.,1.,1.,1.,1.,1.,1.,1.,1.,1.,1.,1.,1.,1.,1.,1.,
1.,1.,1.,1.,1.,1.,1.,1.,1.,1.,1.,1.,1.,1.,1.,1.,1.,1.,1.,1.,1.,1.,1.,1.,
1.,1.,1.,1.,1.,1.))
REPRESENTATION_ITEM('')
);
#313=(
BOUNDED_CURVE()
B_SPLINE_CURVE(5,(#45509,#45510,#45511,#45512,#45513,#45514,#45515,#45516,
#45517,#45518,#45519,#45520,#45521,#45522,#45523,#45524,#45525,#45526,#45527,
#45528,#45529,#45530,#45531,#45532,#45533,#45534,#45535,#45536,#45537,#45538,
#45539,#45540,#45541,#45542,#45543,#45544,#45545,#45546,#45547,#45548,#45549,
#45550,#45551,#45552,#45553,#45554,#45555,#45556,#45557,#45558,#45559,#45560,
#45561,#45562,#45563,#45564,#45565,#45566,#45567,#45568,#45569,#45570,#45571,
#45572,#45573,#45574,#45575,#45576,#45577,#45578),.UNSPECIFIED.,.F.,.F.)
B_SPLINE_CURVE_WITH_KNOTS((6,1,1,1,1,1,1,1,1,1,1,1,1,1,1,1,1,1,1,1,1,1,
1,1,1,1,1,1,1,1,1,1,1,1,1,1,1,1,1,1,1,1,1,1,1,1,1,1,1,1,1,1,1,1,1,1,1,1,
1,1,1,1,1,1,1,6),(-1.,-0.984615384615383,-0.969230769230768,-0.953846153846152,
-0.938461538461537,-0.923076923076922,-0.907692307692306,-0.892307692307691,
-0.876923076923076,-0.86153846153846,-0.846153846153845,-0.83076923076923,
-0.815384615384614,-0.799999999999999,-0.784615384615384,-0.769230769230768,
-0.753846153846153,-0.738461538461538,-0.723076923076922,-0.707692307692307,
-0.692307692307692,-0.676923076923076,-0.661538461538461,-0.646153846153846,
-0.63076923076923,-0.615384615384615,-0.6,-0.584615384615384,-0.569230769230769,
-0.553846153846154,-0.538461538461538,-0.523076923076923,-0.507692307692308,
-0.492307692307692,-0.476923076923077,-0.461538461538462,-0.446153846153846,
-0.430769230769231,-0.415384615384615,-0.4,-0.384615384615385,-0.369230769230769,
-0.353846153846154,-0.338461538461538,-0.323076923076923,-0.307692307692308,
-0.292307692307692,-0.276923076923077,-0.261538461538462,-0.246153846153846,
-0.230769230769231,-0.215384615384615,-0.2,-0.184615384615385,-0.169230769230769,
-0.153846153846154,-0.138461538461538,-0.123076923076923,-0.107692307692308,
-0.0923076923076923,-0.0769230769230769,-0.0615384615384615,-0.0461538461538462,
-0.0307692307692308,-0.0153846153846154,0.),.UNSPECIFIED.)
CURVE()
GEOMETRIC_REPRESENTATION_ITEM()
RATIONAL_B_SPLINE_CURVE((1.,1.,1.,1.,1.,1.,1.,1.,1.,1.,1.,1.,1.,1.,1.,1.,
1.,1.,1.,1.,1.,1.,1.,1.,1.,1.,1.,1.,1.,1.,1.,1.,1.,1.,1.,1.,1.,1.,1.,1.,
1.,1.,1.,1.,1.,1.,1.,1.,1.,1.,1.,1.,1.,1.,1.,1.,1.,1.,1.,1.,1.,1.,1.,1.,
1.,1.,1.,1.,1.,1.))
REPRESENTATION_ITEM('')
);
#314=(
BOUNDED_CURVE()
B_SPLINE_CURVE(5,(#45725,#45726,#45727,#45728,#45729,#45730,#45731,#45732,
#45733,#45734,#45735,#45736,#45737,#45738,#45739,#45740,#45741,#45742,#45743,
#45744,#45745,#45746,#45747,#45748,#45749,#45750,#45751,#45752,#45753,#45754,
#45755,#45756,#45757,#45758,#45759,#45760,#45761,#45762,#45763,#45764,#45765,
#45766,#45767,#45768,#45769,#45770,#45771,#45772,#45773,#45774,#45775,#45776,
#45777,#45778,#45779,#45780,#45781,#45782,#45783,#45784,#45785,#45786,#45787,
#45788,#45789,#45790,#45791,#45792,#45793,#45794),.UNSPECIFIED.,.F.,.F.)
B_SPLINE_CURVE_WITH_KNOTS((6,1,1,1,1,1,1,1,1,1,1,1,1,1,1,1,1,1,1,1,1,1,
1,1,1,1,1,1,1,1,1,1,1,1,1,1,1,1,1,1,1,1,1,1,1,1,1,1,1,1,1,1,1,1,1,1,1,1,
1,1,1,1,1,1,1,6),(-1.,-0.984615384615383,-0.969230769230768,-0.953846153846152,
-0.938461538461537,-0.923076923076922,-0.907692307692306,-0.892307692307691,
-0.876923076923076,-0.86153846153846,-0.846153846153845,-0.83076923076923,
-0.815384615384614,-0.799999999999999,-0.784615384615384,-0.769230769230768,
-0.753846153846153,-0.738461538461538,-0.723076923076922,-0.707692307692307,
-0.692307692307692,-0.676923076923076,-0.661538461538461,-0.646153846153846,
-0.63076923076923,-0.615384615384615,-0.6,-0.584615384615384,-0.569230769230769,
-0.553846153846154,-0.538461538461538,-0.523076923076923,-0.507692307692308,
-0.492307692307692,-0.476923076923077,-0.461538461538462,-0.446153846153846,
-0.430769230769231,-0.415384615384615,-0.4,-0.384615384615385,-0.369230769230769,
-0.353846153846154,-0.338461538461538,-0.323076923076923,-0.307692307692308,
-0.292307692307692,-0.276923076923077,-0.261538461538462,-0.246153846153846,
-0.230769230769231,-0.215384615384615,-0.2,-0.184615384615385,-0.169230769230769,
-0.153846153846154,-0.138461538461538,-0.123076923076923,-0.107692307692308,
-0.0923076923076923,-0.0769230769230769,-0.0615384615384615,-0.0461538461538462,
-0.0307692307692308,-0.0153846153846154,0.),.UNSPECIFIED.)
CURVE()
GEOMETRIC_REPRESENTATION_ITEM()
RATIONAL_B_SPLINE_CURVE((1.,1.,1.,1.,1.,1.,1.,1.,1.,1.,1.,1.,1.,1.,1.,1.,
1.,1.,1.,1.,1.,1.,1.,1.,1.,1.,1.,1.,1.,1.,1.,1.,1.,1.,1.,1.,1.,1.,1.,1.,
1.,1.,1.,1.,1.,1.,1.,1.,1.,1.,1.,1.,1.,1.,1.,1.,1.,1.,1.,1.,1.,1.,1.,1.,
1.,1.,1.,1.,1.,1.))
REPRESENTATION_ITEM('')
);
#315=(
BOUNDED_CURVE()
B_SPLINE_CURVE(5,(#45941,#45942,#45943,#45944,#45945,#45946,#45947,#45948,
#45949,#45950,#45951,#45952,#45953,#45954,#45955,#45956,#45957,#45958,#45959,
#45960,#45961,#45962,#45963,#45964,#45965,#45966,#45967,#45968,#45969,#45970,
#45971,#45972,#45973,#45974,#45975,#45976,#45977,#45978,#45979,#45980,#45981,
#45982,#45983,#45984,#45985,#45986,#45987,#45988,#45989,#45990,#45991,#45992,
#45993,#45994,#45995,#45996,#45997,#45998,#45999,#46000,#46001,#46002,#46003,
#46004,#46005,#46006,#46007,#46008,#46009,#46010),.UNSPECIFIED.,.F.,.F.)
B_SPLINE_CURVE_WITH_KNOTS((6,1,1,1,1,1,1,1,1,1,1,1,1,1,1,1,1,1,1,1,1,1,
1,1,1,1,1,1,1,1,1,1,1,1,1,1,1,1,1,1,1,1,1,1,1,1,1,1,1,1,1,1,1,1,1,1,1,1,
1,1,1,1,1,1,1,6),(-1.,-0.984615384615383,-0.969230769230768,-0.953846153846152,
-0.938461538461537,-0.923076923076922,-0.907692307692306,-0.892307692307691,
-0.876923076923076,-0.86153846153846,-0.846153846153845,-0.83076923076923,
-0.815384615384614,-0.799999999999999,-0.784615384615384,-0.769230769230768,
-0.753846153846153,-0.738461538461538,-0.723076923076922,-0.707692307692307,
-0.692307692307692,-0.676923076923076,-0.661538461538461,-0.646153846153846,
-0.63076923076923,-0.615384615384615,-0.6,-0.584615384615384,-0.569230769230769,
-0.553846153846154,-0.538461538461538,-0.523076923076923,-0.507692307692308,
-0.492307692307692,-0.476923076923077,-0.461538461538462,-0.446153846153846,
-0.430769230769231,-0.415384615384615,-0.4,-0.384615384615385,-0.369230769230769,
-0.353846153846154,-0.338461538461538,-0.323076923076923,-0.307692307692308,
-0.292307692307692,-0.276923076923077,-0.261538461538462,-0.246153846153846,
-0.230769230769231,-0.215384615384615,-0.2,-0.184615384615385,-0.169230769230769,
-0.153846153846154,-0.138461538461538,-0.123076923076923,-0.107692307692308,
-0.0923076923076923,-0.0769230769230769,-0.0615384615384615,-0.0461538461538462,
-0.0307692307692308,-0.0153846153846154,0.),.UNSPECIFIED.)
CURVE()
GEOMETRIC_REPRESENTATION_ITEM()
RATIONAL_B_SPLINE_CURVE((1.,1.,1.,1.,1.,1.,1.,1.,1.,1.,1.,1.,1.,1.,1.,1.,
1.,1.,1.,1.,1.,1.,1.,1.,1.,1.,1.,1.,1.,1.,1.,1.,1.,1.,1.,1.,1.,1.,1.,1.,
1.,1.,1.,1.,1.,1.,1.,1.,1.,1.,1.,1.,1.,1.,1.,1.,1.,1.,1.,1.,1.,1.,1.,1.,
1.,1.,1.,1.,1.,1.))
REPRESENTATION_ITEM('')
);
#316=(
BOUNDED_CURVE()
B_SPLINE_CURVE(5,(#46157,#46158,#46159,#46160,#46161,#46162,#46163,#46164,
#46165,#46166,#46167,#46168,#46169,#46170,#46171,#46172,#46173,#46174,#46175,
#46176,#46177,#46178,#46179,#46180,#46181,#46182,#46183,#46184,#46185,#46186,
#46187,#46188,#46189,#46190,#46191,#46192,#46193,#46194,#46195,#46196,#46197,
#46198,#46199,#46200,#46201,#46202,#46203,#46204,#46205,#46206,#46207,#46208,
#46209,#46210,#46211,#46212,#46213,#46214,#46215,#46216,#46217,#46218,#46219,
#46220,#46221,#46222,#46223,#46224,#46225,#46226),.UNSPECIFIED.,.F.,.F.)
B_SPLINE_CURVE_WITH_KNOTS((6,1,1,1,1,1,1,1,1,1,1,1,1,1,1,1,1,1,1,1,1,1,
1,1,1,1,1,1,1,1,1,1,1,1,1,1,1,1,1,1,1,1,1,1,1,1,1,1,1,1,1,1,1,1,1,1,1,1,
1,1,1,1,1,1,1,6),(-1.,-0.984615384615383,-0.969230769230768,-0.953846153846152,
-0.938461538461537,-0.923076923076922,-0.907692307692306,-0.892307692307691,
-0.876923076923076,-0.86153846153846,-0.846153846153845,-0.83076923076923,
-0.815384615384614,-0.799999999999999,-0.784615384615384,-0.769230769230768,
-0.753846153846153,-0.738461538461538,-0.723076923076922,-0.707692307692307,
-0.692307692307692,-0.676923076923076,-0.661538461538461,-0.646153846153846,
-0.63076923076923,-0.615384615384615,-0.6,-0.584615384615384,-0.569230769230769,
-0.553846153846154,-0.538461538461538,-0.523076923076923,-0.507692307692308,
-0.492307692307692,-0.476923076923077,-0.461538461538462,-0.446153846153846,
-0.430769230769231,-0.415384615384615,-0.4,-0.384615384615385,-0.369230769230769,
-0.353846153846154,-0.338461538461538,-0.323076923076923,-0.307692307692308,
-0.292307692307692,-0.276923076923077,-0.261538461538462,-0.246153846153846,
-0.230769230769231,-0.215384615384615,-0.2,-0.184615384615385,-0.169230769230769,
-0.153846153846154,-0.138461538461538,-0.123076923076923,-0.107692307692308,
-0.0923076923076923,-0.0769230769230769,-0.0615384615384615,-0.0461538461538462,
-0.0307692307692308,-0.0153846153846154,0.),.UNSPECIFIED.)
CURVE()
GEOMETRIC_REPRESENTATION_ITEM()
RATIONAL_B_SPLINE_CURVE((1.,1.,1.,1.,1.,1.,1.,1.,1.,1.,1.,1.,1.,1.,1.,1.,
1.,1.,1.,1.,1.,1.,1.,1.,1.,1.,1.,1.,1.,1.,1.,1.,1.,1.,1.,1.,1.,1.,1.,1.,
1.,1.,1.,1.,1.,1.,1.,1.,1.,1.,1.,1.,1.,1.,1.,1.,1.,1.,1.,1.,1.,1.,1.,1.,
1.,1.,1.,1.,1.,1.))
REPRESENTATION_ITEM('')
);
#317=(
BOUNDED_CURVE()
B_SPLINE_CURVE(5,(#46373,#46374,#46375,#46376,#46377,#46378,#46379,#46380,
#46381,#46382,#46383,#46384,#46385,#46386,#46387,#46388,#46389,#46390,#46391,
#46392,#46393,#46394,#46395,#46396,#46397,#46398,#46399,#46400,#46401,#46402,
#46403,#46404,#46405,#46406,#46407,#46408,#46409,#46410,#46411,#46412,#46413,
#46414,#46415,#46416,#46417,#46418,#46419,#46420,#46421,#46422,#46423,#46424,
#46425,#46426,#46427,#46428,#46429,#46430,#46431,#46432,#46433,#46434,#46435,
#46436,#46437,#46438,#46439,#46440,#46441,#46442),.UNSPECIFIED.,.F.,.F.)
B_SPLINE_CURVE_WITH_KNOTS((6,1,1,1,1,1,1,1,1,1,1,1,1,1,1,1,1,1,1,1,1,1,
1,1,1,1,1,1,1,1,1,1,1,1,1,1,1,1,1,1,1,1,1,1,1,1,1,1,1,1,1,1,1,1,1,1,1,1,
1,1,1,1,1,1,1,6),(-1.,-0.984615384615383,-0.969230769230768,-0.953846153846152,
-0.938461538461537,-0.923076923076922,-0.907692307692306,-0.892307692307691,
-0.876923076923076,-0.86153846153846,-0.846153846153845,-0.83076923076923,
-0.815384615384614,-0.799999999999999,-0.784615384615384,-0.769230769230768,
-0.753846153846153,-0.738461538461538,-0.723076923076922,-0.707692307692307,
-0.692307692307692,-0.676923076923076,-0.661538461538461,-0.646153846153846,
-0.63076923076923,-0.615384615384615,-0.6,-0.584615384615384,-0.569230769230769,
-0.553846153846154,-0.538461538461538,-0.523076923076923,-0.507692307692308,
-0.492307692307692,-0.476923076923077,-0.461538461538462,-0.446153846153846,
-0.430769230769231,-0.415384615384615,-0.4,-0.384615384615385,-0.369230769230769,
-0.353846153846154,-0.338461538461538,-0.323076923076923,-0.307692307692308,
-0.292307692307692,-0.276923076923077,-0.261538461538462,-0.246153846153846,
-0.230769230769231,-0.215384615384615,-0.2,-0.184615384615385,-0.169230769230769,
-0.153846153846154,-0.138461538461538,-0.123076923076923,-0.107692307692308,
-0.0923076923076923,-0.0769230769230769,-0.0615384615384615,-0.0461538461538462,
-0.0307692307692308,-0.0153846153846154,0.),.UNSPECIFIED.)
CURVE()
GEOMETRIC_REPRESENTATION_ITEM()
RATIONAL_B_SPLINE_CURVE((1.,1.,1.,1.,1.,1.,1.,1.,1.,1.,1.,1.,1.,1.,1.,1.,
1.,1.,1.,1.,1.,1.,1.,1.,1.,1.,1.,1.,1.,1.,1.,1.,1.,1.,1.,1.,1.,1.,1.,1.,
1.,1.,1.,1.,1.,1.,1.,1.,1.,1.,1.,1.,1.,1.,1.,1.,1.,1.,1.,1.,1.,1.,1.,1.,
1.,1.,1.,1.,1.,1.))
REPRESENTATION_ITEM('')
);
#318=(
BOUNDED_CURVE()
B_SPLINE_CURVE(5,(#46589,#46590,#46591,#46592,#46593,#46594,#46595,#46596,
#46597,#46598,#46599,#46600,#46601,#46602,#46603,#46604,#46605,#46606,#46607,
#46608,#46609,#46610,#46611,#46612,#46613,#46614,#46615,#46616,#46617,#46618,
#46619,#46620,#46621,#46622,#46623,#46624,#46625,#46626,#46627,#46628,#46629,
#46630,#46631,#46632,#46633,#46634,#46635,#46636,#46637,#46638,#46639,#46640,
#46641,#46642,#46643,#46644,#46645,#46646,#46647,#46648,#46649,#46650,#46651,
#46652,#46653,#46654,#46655,#46656,#46657,#46658),.UNSPECIFIED.,.F.,.F.)
B_SPLINE_CURVE_WITH_KNOTS((6,1,1,1,1,1,1,1,1,1,1,1,1,1,1,1,1,1,1,1,1,1,
1,1,1,1,1,1,1,1,1,1,1,1,1,1,1,1,1,1,1,1,1,1,1,1,1,1,1,1,1,1,1,1,1,1,1,1,
1,1,1,1,1,1,1,6),(-1.,-0.984615384615383,-0.969230769230768,-0.953846153846152,
-0.938461538461537,-0.923076923076922,-0.907692307692306,-0.892307692307691,
-0.876923076923076,-0.86153846153846,-0.846153846153845,-0.83076923076923,
-0.815384615384614,-0.799999999999999,-0.784615384615384,-0.769230769230768,
-0.753846153846153,-0.738461538461538,-0.723076923076922,-0.707692307692307,
-0.692307692307692,-0.676923076923076,-0.661538461538461,-0.646153846153846,
-0.63076923076923,-0.615384615384615,-0.6,-0.584615384615384,-0.569230769230769,
-0.553846153846154,-0.538461538461538,-0.523076923076923,-0.507692307692308,
-0.492307692307692,-0.476923076923077,-0.461538461538462,-0.446153846153846,
-0.430769230769231,-0.415384615384615,-0.4,-0.384615384615385,-0.369230769230769,
-0.353846153846154,-0.338461538461538,-0.323076923076923,-0.307692307692308,
-0.292307692307692,-0.276923076923077,-0.261538461538462,-0.246153846153846,
-0.230769230769231,-0.215384615384615,-0.2,-0.184615384615385,-0.169230769230769,
-0.153846153846154,-0.138461538461538,-0.123076923076923,-0.107692307692308,
-0.0923076923076923,-0.0769230769230769,-0.0615384615384615,-0.0461538461538462,
-0.0307692307692308,-0.0153846153846154,0.),.UNSPECIFIED.)
CURVE()
GEOMETRIC_REPRESENTATION_ITEM()
RATIONAL_B_SPLINE_CURVE((1.,1.,1.,1.,1.,1.,1.,1.,1.,1.,1.,1.,1.,1.,1.,1.,
1.,1.,1.,1.,1.,1.,1.,1.,1.,1.,1.,1.,1.,1.,1.,1.,1.,1.,1.,1.,1.,1.,1.,1.,
1.,1.,1.,1.,1.,1.,1.,1.,1.,1.,1.,1.,1.,1.,1.,1.,1.,1.,1.,1.,1.,1.,1.,1.,
1.,1.,1.,1.,1.,1.))
REPRESENTATION_ITEM('')
);
#319=(
BOUNDED_CURVE()
B_SPLINE_CURVE(5,(#46805,#46806,#46807,#46808,#46809,#46810,#46811,#46812,
#46813,#46814,#46815,#46816,#46817,#46818,#46819,#46820,#46821,#46822,#46823,
#46824,#46825,#46826,#46827,#46828,#46829,#46830,#46831,#46832,#46833,#46834,
#46835,#46836,#46837,#46838,#46839,#46840,#46841,#46842,#46843,#46844,#46845,
#46846,#46847,#46848,#46849,#46850,#46851,#46852,#46853,#46854,#46855,#46856,
#46857,#46858,#46859,#46860,#46861,#46862,#46863,#46864,#46865,#46866,#46867,
#46868,#46869,#46870,#46871,#46872,#46873,#46874),.UNSPECIFIED.,.F.,.F.)
B_SPLINE_CURVE_WITH_KNOTS((6,1,1,1,1,1,1,1,1,1,1,1,1,1,1,1,1,1,1,1,1,1,
1,1,1,1,1,1,1,1,1,1,1,1,1,1,1,1,1,1,1,1,1,1,1,1,1,1,1,1,1,1,1,1,1,1,1,1,
1,1,1,1,1,1,1,6),(-1.,-0.984615384615383,-0.969230769230768,-0.953846153846152,
-0.938461538461537,-0.923076923076922,-0.907692307692306,-0.892307692307691,
-0.876923076923076,-0.86153846153846,-0.846153846153845,-0.83076923076923,
-0.815384615384614,-0.799999999999999,-0.784615384615384,-0.769230769230768,
-0.753846153846153,-0.738461538461538,-0.723076923076922,-0.707692307692307,
-0.692307692307692,-0.676923076923076,-0.661538461538461,-0.646153846153846,
-0.63076923076923,-0.615384615384615,-0.6,-0.584615384615384,-0.569230769230769,
-0.553846153846154,-0.538461538461538,-0.523076923076923,-0.507692307692308,
-0.492307692307692,-0.476923076923077,-0.461538461538462,-0.446153846153846,
-0.430769230769231,-0.415384615384615,-0.4,-0.384615384615385,-0.369230769230769,
-0.353846153846154,-0.338461538461538,-0.323076923076923,-0.307692307692308,
-0.292307692307692,-0.276923076923077,-0.261538461538462,-0.246153846153846,
-0.230769230769231,-0.215384615384615,-0.2,-0.184615384615385,-0.169230769230769,
-0.153846153846154,-0.138461538461538,-0.123076923076923,-0.107692307692308,
-0.0923076923076923,-0.0769230769230769,-0.0615384615384615,-0.0461538461538462,
-0.0307692307692308,-0.0153846153846154,0.),.UNSPECIFIED.)
CURVE()
GEOMETRIC_REPRESENTATION_ITEM()
RATIONAL_B_SPLINE_CURVE((1.,1.,1.,1.,1.,1.,1.,1.,1.,1.,1.,1.,1.,1.,1.,1.,
1.,1.,1.,1.,1.,1.,1.,1.,1.,1.,1.,1.,1.,1.,1.,1.,1.,1.,1.,1.,1.,1.,1.,1.,
1.,1.,1.,1.,1.,1.,1.,1.,1.,1.,1.,1.,1.,1.,1.,1.,1.,1.,1.,1.,1.,1.,1.,1.,
1.,1.,1.,1.,1.,1.))
REPRESENTATION_ITEM('')
);
#320=(
BOUNDED_CURVE()
B_SPLINE_CURVE(5,(#47021,#47022,#47023,#47024,#47025,#47026,#47027,#47028,
#47029,#47030,#47031,#47032,#47033,#47034,#47035,#47036,#47037,#47038,#47039,
#47040,#47041,#47042,#47043,#47044,#47045,#47046,#47047,#47048,#47049,#47050,
#47051,#47052,#47053,#47054,#47055,#47056,#47057,#47058,#47059,#47060,#47061,
#47062,#47063,#47064,#47065,#47066,#47067,#47068,#47069,#47070,#47071,#47072,
#47073,#47074,#47075,#47076,#47077,#47078,#47079,#47080,#47081,#47082,#47083,
#47084,#47085,#47086,#47087,#47088,#47089,#47090),.UNSPECIFIED.,.F.,.F.)
B_SPLINE_CURVE_WITH_KNOTS((6,1,1,1,1,1,1,1,1,1,1,1,1,1,1,1,1,1,1,1,1,1,
1,1,1,1,1,1,1,1,1,1,1,1,1,1,1,1,1,1,1,1,1,1,1,1,1,1,1,1,1,1,1,1,1,1,1,1,
1,1,1,1,1,1,1,6),(-1.,-0.984615384615383,-0.969230769230768,-0.953846153846152,
-0.938461538461537,-0.923076923076922,-0.907692307692306,-0.892307692307691,
-0.876923076923076,-0.86153846153846,-0.846153846153845,-0.83076923076923,
-0.815384615384614,-0.799999999999999,-0.784615384615384,-0.769230769230768,
-0.753846153846153,-0.738461538461538,-0.723076923076922,-0.707692307692307,
-0.692307692307692,-0.676923076923076,-0.661538461538461,-0.646153846153846,
-0.63076923076923,-0.615384615384615,-0.6,-0.584615384615384,-0.569230769230769,
-0.553846153846154,-0.538461538461538,-0.523076923076923,-0.507692307692308,
-0.492307692307692,-0.476923076923077,-0.461538461538462,-0.446153846153846,
-0.430769230769231,-0.415384615384615,-0.4,-0.384615384615385,-0.369230769230769,
-0.353846153846154,-0.338461538461538,-0.323076923076923,-0.307692307692308,
-0.292307692307692,-0.276923076923077,-0.261538461538462,-0.246153846153846,
-0.230769230769231,-0.215384615384615,-0.2,-0.184615384615385,-0.169230769230769,
-0.153846153846154,-0.138461538461538,-0.123076923076923,-0.107692307692308,
-0.0923076923076923,-0.0769230769230769,-0.0615384615384615,-0.0461538461538462,
-0.0307692307692308,-0.0153846153846154,0.),.UNSPECIFIED.)
CURVE()
GEOMETRIC_REPRESENTATION_ITEM()
RATIONAL_B_SPLINE_CURVE((1.,1.,1.,1.,1.,1.,1.,1.,1.,1.,1.,1.,1.,1.,1.,1.,
1.,1.,1.,1.,1.,1.,1.,1.,1.,1.,1.,1.,1.,1.,1.,1.,1.,1.,1.,1.,1.,1.,1.,1.,
1.,1.,1.,1.,1.,1.,1.,1.,1.,1.,1.,1.,1.,1.,1.,1.,1.,1.,1.,1.,1.,1.,1.,1.,
1.,1.,1.,1.,1.,1.))
REPRESENTATION_ITEM('')
);
#321=(
BOUNDED_CURVE()
B_SPLINE_CURVE(5,(#47237,#47238,#47239,#47240,#47241,#47242,#47243,#47244,
#47245,#47246,#47247,#47248,#47249,#47250,#47251,#47252,#47253,#47254,#47255,
#47256,#47257,#47258,#47259,#47260,#47261,#47262,#47263,#47264,#47265,#47266,
#47267,#47268,#47269,#47270,#47271,#47272,#47273,#47274,#47275,#47276,#47277,
#47278,#47279,#47280,#47281,#47282,#47283,#47284,#47285,#47286,#47287,#47288,
#47289,#47290,#47291,#47292,#47293,#47294,#47295,#47296,#47297,#47298,#47299,
#47300,#47301,#47302,#47303,#47304,#47305,#47306),.UNSPECIFIED.,.F.,.F.)
B_SPLINE_CURVE_WITH_KNOTS((6,1,1,1,1,1,1,1,1,1,1,1,1,1,1,1,1,1,1,1,1,1,
1,1,1,1,1,1,1,1,1,1,1,1,1,1,1,1,1,1,1,1,1,1,1,1,1,1,1,1,1,1,1,1,1,1,1,1,
1,1,1,1,1,1,1,6),(-1.,-0.984615384615383,-0.969230769230768,-0.953846153846152,
-0.938461538461537,-0.923076923076922,-0.907692307692306,-0.892307692307691,
-0.876923076923076,-0.86153846153846,-0.846153846153845,-0.83076923076923,
-0.815384615384614,-0.799999999999999,-0.784615384615384,-0.769230769230768,
-0.753846153846153,-0.738461538461538,-0.723076923076922,-0.707692307692307,
-0.692307692307692,-0.676923076923076,-0.661538461538461,-0.646153846153846,
-0.63076923076923,-0.615384615384615,-0.6,-0.584615384615384,-0.569230769230769,
-0.553846153846154,-0.538461538461538,-0.523076923076923,-0.507692307692308,
-0.492307692307692,-0.476923076923077,-0.461538461538462,-0.446153846153846,
-0.430769230769231,-0.415384615384615,-0.4,-0.384615384615385,-0.369230769230769,
-0.353846153846154,-0.338461538461538,-0.323076923076923,-0.307692307692308,
-0.292307692307692,-0.276923076923077,-0.261538461538462,-0.246153846153846,
-0.230769230769231,-0.215384615384615,-0.2,-0.184615384615385,-0.169230769230769,
-0.153846153846154,-0.138461538461538,-0.123076923076923,-0.107692307692308,
-0.0923076923076923,-0.0769230769230769,-0.0615384615384615,-0.0461538461538462,
-0.0307692307692308,-0.0153846153846154,0.),.UNSPECIFIED.)
CURVE()
GEOMETRIC_REPRESENTATION_ITEM()
RATIONAL_B_SPLINE_CURVE((1.,1.,1.,1.,1.,1.,1.,1.,1.,1.,1.,1.,1.,1.,1.,1.,
1.,1.,1.,1.,1.,1.,1.,1.,1.,1.,1.,1.,1.,1.,1.,1.,1.,1.,1.,1.,1.,1.,1.,1.,
1.,1.,1.,1.,1.,1.,1.,1.,1.,1.,1.,1.,1.,1.,1.,1.,1.,1.,1.,1.,1.,1.,1.,1.,
1.,1.,1.,1.,1.,1.))
REPRESENTATION_ITEM('')
);
#322=(
BOUNDED_CURVE()
B_SPLINE_CURVE(5,(#47453,#47454,#47455,#47456,#47457,#47458,#47459,#47460,
#47461,#47462,#47463,#47464,#47465,#47466,#47467,#47468,#47469,#47470,#47471,
#47472,#47473,#47474,#47475,#47476,#47477,#47478,#47479,#47480,#47481,#47482,
#47483,#47484,#47485,#47486,#47487,#47488,#47489,#47490,#47491,#47492,#47493,
#47494,#47495,#47496,#47497,#47498,#47499,#47500,#47501,#47502,#47503,#47504,
#47505,#47506,#47507,#47508,#47509,#47510,#47511,#47512,#47513,#47514,#47515,
#47516,#47517,#47518,#47519,#47520,#47521,#47522),.UNSPECIFIED.,.F.,.F.)
B_SPLINE_CURVE_WITH_KNOTS((6,1,1,1,1,1,1,1,1,1,1,1,1,1,1,1,1,1,1,1,1,1,
1,1,1,1,1,1,1,1,1,1,1,1,1,1,1,1,1,1,1,1,1,1,1,1,1,1,1,1,1,1,1,1,1,1,1,1,
1,1,1,1,1,1,1,6),(-1.,-0.984615384615383,-0.969230769230768,-0.953846153846152,
-0.938461538461537,-0.923076923076922,-0.907692307692306,-0.892307692307691,
-0.876923076923076,-0.86153846153846,-0.846153846153845,-0.83076923076923,
-0.815384615384614,-0.799999999999999,-0.784615384615384,-0.769230769230768,
-0.753846153846153,-0.738461538461538,-0.723076923076922,-0.707692307692307,
-0.692307692307692,-0.676923076923076,-0.661538461538461,-0.646153846153846,
-0.63076923076923,-0.615384615384615,-0.6,-0.584615384615384,-0.569230769230769,
-0.553846153846154,-0.538461538461538,-0.523076923076923,-0.507692307692308,
-0.492307692307692,-0.476923076923077,-0.461538461538462,-0.446153846153846,
-0.430769230769231,-0.415384615384615,-0.4,-0.384615384615385,-0.369230769230769,
-0.353846153846154,-0.338461538461538,-0.323076923076923,-0.307692307692308,
-0.292307692307692,-0.276923076923077,-0.261538461538462,-0.246153846153846,
-0.230769230769231,-0.215384615384615,-0.2,-0.184615384615385,-0.169230769230769,
-0.153846153846154,-0.138461538461538,-0.123076923076923,-0.107692307692308,
-0.0923076923076923,-0.0769230769230769,-0.0615384615384615,-0.0461538461538462,
-0.0307692307692308,-0.0153846153846154,0.),.UNSPECIFIED.)
CURVE()
GEOMETRIC_REPRESENTATION_ITEM()
RATIONAL_B_SPLINE_CURVE((1.,1.,1.,1.,1.,1.,1.,1.,1.,1.,1.,1.,1.,1.,1.,1.,
1.,1.,1.,1.,1.,1.,1.,1.,1.,1.,1.,1.,1.,1.,1.,1.,1.,1.,1.,1.,1.,1.,1.,1.,
1.,1.,1.,1.,1.,1.,1.,1.,1.,1.,1.,1.,1.,1.,1.,1.,1.,1.,1.,1.,1.,1.,1.,1.,
1.,1.,1.,1.,1.,1.))
REPRESENTATION_ITEM('')
);
#323=(
BOUNDED_CURVE()
B_SPLINE_CURVE(5,(#47669,#47670,#47671,#47672,#47673,#47674,#47675,#47676,
#47677,#47678,#47679,#47680,#47681,#47682,#47683,#47684,#47685,#47686,#47687,
#47688,#47689,#47690,#47691,#47692,#47693,#47694,#47695,#47696,#47697,#47698,
#47699,#47700,#47701,#47702,#47703,#47704,#47705,#47706,#47707,#47708,#47709,
#47710,#47711,#47712,#47713,#47714,#47715,#47716,#47717,#47718,#47719,#47720,
#47721,#47722,#47723,#47724,#47725,#47726,#47727,#47728,#47729,#47730,#47731,
#47732,#47733,#47734,#47735,#47736,#47737,#47738),.UNSPECIFIED.,.F.,.F.)
B_SPLINE_CURVE_WITH_KNOTS((6,1,1,1,1,1,1,1,1,1,1,1,1,1,1,1,1,1,1,1,1,1,
1,1,1,1,1,1,1,1,1,1,1,1,1,1,1,1,1,1,1,1,1,1,1,1,1,1,1,1,1,1,1,1,1,1,1,1,
1,1,1,1,1,1,1,6),(-1.,-0.984615384615383,-0.969230769230768,-0.953846153846152,
-0.938461538461537,-0.923076923076922,-0.907692307692306,-0.892307692307691,
-0.876923076923076,-0.86153846153846,-0.846153846153845,-0.83076923076923,
-0.815384615384614,-0.799999999999999,-0.784615384615384,-0.769230769230768,
-0.753846153846153,-0.738461538461538,-0.723076923076922,-0.707692307692307,
-0.692307692307692,-0.676923076923076,-0.661538461538461,-0.646153846153846,
-0.63076923076923,-0.615384615384615,-0.6,-0.584615384615384,-0.569230769230769,
-0.553846153846154,-0.538461538461538,-0.523076923076923,-0.507692307692308,
-0.492307692307692,-0.476923076923077,-0.461538461538462,-0.446153846153846,
-0.430769230769231,-0.415384615384615,-0.4,-0.384615384615385,-0.369230769230769,
-0.353846153846154,-0.338461538461538,-0.323076923076923,-0.307692307692308,
-0.292307692307692,-0.276923076923077,-0.261538461538462,-0.246153846153846,
-0.230769230769231,-0.215384615384615,-0.2,-0.184615384615385,-0.169230769230769,
-0.153846153846154,-0.138461538461538,-0.123076923076923,-0.107692307692308,
-0.0923076923076923,-0.0769230769230769,-0.0615384615384615,-0.0461538461538462,
-0.0307692307692308,-0.0153846153846154,0.),.UNSPECIFIED.)
CURVE()
GEOMETRIC_REPRESENTATION_ITEM()
RATIONAL_B_SPLINE_CURVE((1.,1.,1.,1.,1.,1.,1.,1.,1.,1.,1.,1.,1.,1.,1.,1.,
1.,1.,1.,1.,1.,1.,1.,1.,1.,1.,1.,1.,1.,1.,1.,1.,1.,1.,1.,1.,1.,1.,1.,1.,
1.,1.,1.,1.,1.,1.,1.,1.,1.,1.,1.,1.,1.,1.,1.,1.,1.,1.,1.,1.,1.,1.,1.,1.,
1.,1.,1.,1.,1.,1.))
REPRESENTATION_ITEM('')
);
#324=(
BOUNDED_CURVE()
B_SPLINE_CURVE(5,(#47885,#47886,#47887,#47888,#47889,#47890,#47891,#47892,
#47893,#47894,#47895,#47896,#47897,#47898,#47899,#47900,#47901,#47902,#47903,
#47904,#47905,#47906,#47907,#47908,#47909,#47910,#47911,#47912,#47913,#47914,
#47915,#47916,#47917,#47918,#47919,#47920,#47921,#47922,#47923,#47924,#47925,
#47926,#47927,#47928,#47929,#47930,#47931,#47932,#47933,#47934,#47935,#47936,
#47937,#47938,#47939,#47940,#47941,#47942,#47943,#47944,#47945,#47946,#47947,
#47948,#47949,#47950,#47951,#47952,#47953,#47954),.UNSPECIFIED.,.F.,.F.)
B_SPLINE_CURVE_WITH_KNOTS((6,1,1,1,1,1,1,1,1,1,1,1,1,1,1,1,1,1,1,1,1,1,
1,1,1,1,1,1,1,1,1,1,1,1,1,1,1,1,1,1,1,1,1,1,1,1,1,1,1,1,1,1,1,1,1,1,1,1,
1,1,1,1,1,1,1,6),(-1.,-0.984615384615383,-0.969230769230768,-0.953846153846152,
-0.938461538461537,-0.923076923076922,-0.907692307692306,-0.892307692307691,
-0.876923076923076,-0.86153846153846,-0.846153846153845,-0.83076923076923,
-0.815384615384614,-0.799999999999999,-0.784615384615384,-0.769230769230768,
-0.753846153846153,-0.738461538461538,-0.723076923076922,-0.707692307692307,
-0.692307692307692,-0.676923076923076,-0.661538461538461,-0.646153846153846,
-0.63076923076923,-0.615384615384615,-0.6,-0.584615384615384,-0.569230769230769,
-0.553846153846154,-0.538461538461538,-0.523076923076923,-0.507692307692308,
-0.492307692307692,-0.476923076923077,-0.461538461538462,-0.446153846153846,
-0.430769230769231,-0.415384615384615,-0.4,-0.384615384615385,-0.369230769230769,
-0.353846153846154,-0.338461538461538,-0.323076923076923,-0.307692307692308,
-0.292307692307692,-0.276923076923077,-0.261538461538462,-0.246153846153846,
-0.230769230769231,-0.215384615384615,-0.2,-0.184615384615385,-0.169230769230769,
-0.153846153846154,-0.138461538461538,-0.123076923076923,-0.107692307692308,
-0.0923076923076923,-0.0769230769230769,-0.0615384615384615,-0.0461538461538462,
-0.0307692307692308,-0.0153846153846154,0.),.UNSPECIFIED.)
CURVE()
GEOMETRIC_REPRESENTATION_ITEM()
RATIONAL_B_SPLINE_CURVE((1.,1.,1.,1.,1.,1.,1.,1.,1.,1.,1.,1.,1.,1.,1.,1.,
1.,1.,1.,1.,1.,1.,1.,1.,1.,1.,1.,1.,1.,1.,1.,1.,1.,1.,1.,1.,1.,1.,1.,1.,
1.,1.,1.,1.,1.,1.,1.,1.,1.,1.,1.,1.,1.,1.,1.,1.,1.,1.,1.,1.,1.,1.,1.,1.,
1.,1.,1.,1.,1.,1.))
REPRESENTATION_ITEM('')
);
#325=(
BOUNDED_CURVE()
B_SPLINE_CURVE(5,(#48101,#48102,#48103,#48104,#48105,#48106,#48107,#48108,
#48109,#48110,#48111,#48112,#48113,#48114,#48115,#48116,#48117,#48118,#48119,
#48120,#48121,#48122,#48123,#48124,#48125,#48126,#48127,#48128,#48129,#48130,
#48131,#48132,#48133,#48134,#48135,#48136,#48137,#48138,#48139,#48140,#48141,
#48142,#48143,#48144,#48145,#48146,#48147,#48148,#48149,#48150,#48151,#48152,
#48153,#48154,#48155,#48156,#48157,#48158,#48159,#48160,#48161,#48162,#48163,
#48164,#48165,#48166,#48167,#48168,#48169,#48170),.UNSPECIFIED.,.F.,.F.)
B_SPLINE_CURVE_WITH_KNOTS((6,1,1,1,1,1,1,1,1,1,1,1,1,1,1,1,1,1,1,1,1,1,
1,1,1,1,1,1,1,1,1,1,1,1,1,1,1,1,1,1,1,1,1,1,1,1,1,1,1,1,1,1,1,1,1,1,1,1,
1,1,1,1,1,1,1,6),(-1.,-0.984615384615383,-0.969230769230768,-0.953846153846152,
-0.938461538461537,-0.923076923076922,-0.907692307692306,-0.892307692307691,
-0.876923076923076,-0.86153846153846,-0.846153846153845,-0.83076923076923,
-0.815384615384614,-0.799999999999999,-0.784615384615384,-0.769230769230768,
-0.753846153846153,-0.738461538461538,-0.723076923076922,-0.707692307692307,
-0.692307692307692,-0.676923076923076,-0.661538461538461,-0.646153846153846,
-0.63076923076923,-0.615384615384615,-0.6,-0.584615384615384,-0.569230769230769,
-0.553846153846154,-0.538461538461538,-0.523076923076923,-0.507692307692308,
-0.492307692307692,-0.476923076923077,-0.461538461538462,-0.446153846153846,
-0.430769230769231,-0.415384615384615,-0.4,-0.384615384615385,-0.369230769230769,
-0.353846153846154,-0.338461538461538,-0.323076923076923,-0.307692307692308,
-0.292307692307692,-0.276923076923077,-0.261538461538462,-0.246153846153846,
-0.230769230769231,-0.215384615384615,-0.2,-0.184615384615385,-0.169230769230769,
-0.153846153846154,-0.138461538461538,-0.123076923076923,-0.107692307692308,
-0.0923076923076923,-0.0769230769230769,-0.0615384615384615,-0.0461538461538462,
-0.0307692307692308,-0.0153846153846154,0.),.UNSPECIFIED.)
CURVE()
GEOMETRIC_REPRESENTATION_ITEM()
RATIONAL_B_SPLINE_CURVE((1.,1.,1.,1.,1.,1.,1.,1.,1.,1.,1.,1.,1.,1.,1.,1.,
1.,1.,1.,1.,1.,1.,1.,1.,1.,1.,1.,1.,1.,1.,1.,1.,1.,1.,1.,1.,1.,1.,1.,1.,
1.,1.,1.,1.,1.,1.,1.,1.,1.,1.,1.,1.,1.,1.,1.,1.,1.,1.,1.,1.,1.,1.,1.,1.,
1.,1.,1.,1.,1.,1.))
REPRESENTATION_ITEM('')
);
#326=(
BOUNDED_CURVE()
B_SPLINE_CURVE(5,(#48317,#48318,#48319,#48320,#48321,#48322,#48323,#48324,
#48325,#48326,#48327,#48328,#48329,#48330,#48331,#48332,#48333,#48334,#48335,
#48336,#48337,#48338,#48339,#48340,#48341,#48342,#48343,#48344,#48345,#48346,
#48347,#48348,#48349,#48350,#48351,#48352,#48353,#48354,#48355,#48356,#48357,
#48358,#48359,#48360,#48361,#48362,#48363,#48364,#48365,#48366,#48367,#48368,
#48369,#48370,#48371,#48372,#48373,#48374,#48375,#48376,#48377,#48378,#48379,
#48380,#48381,#48382,#48383,#48384,#48385,#48386),.UNSPECIFIED.,.F.,.F.)
B_SPLINE_CURVE_WITH_KNOTS((6,1,1,1,1,1,1,1,1,1,1,1,1,1,1,1,1,1,1,1,1,1,
1,1,1,1,1,1,1,1,1,1,1,1,1,1,1,1,1,1,1,1,1,1,1,1,1,1,1,1,1,1,1,1,1,1,1,1,
1,1,1,1,1,1,1,6),(-1.,-0.984615384615383,-0.969230769230768,-0.953846153846152,
-0.938461538461537,-0.923076923076922,-0.907692307692306,-0.892307692307691,
-0.876923076923076,-0.86153846153846,-0.846153846153845,-0.83076923076923,
-0.815384615384614,-0.799999999999999,-0.784615384615384,-0.769230769230768,
-0.753846153846153,-0.738461538461538,-0.723076923076922,-0.707692307692307,
-0.692307692307692,-0.676923076923076,-0.661538461538461,-0.646153846153846,
-0.63076923076923,-0.615384615384615,-0.6,-0.584615384615384,-0.569230769230769,
-0.553846153846154,-0.538461538461538,-0.523076923076923,-0.507692307692308,
-0.492307692307692,-0.476923076923077,-0.461538461538462,-0.446153846153846,
-0.430769230769231,-0.415384615384615,-0.4,-0.384615384615385,-0.369230769230769,
-0.353846153846154,-0.338461538461538,-0.323076923076923,-0.307692307692308,
-0.292307692307692,-0.276923076923077,-0.261538461538462,-0.246153846153846,
-0.230769230769231,-0.215384615384615,-0.2,-0.184615384615385,-0.169230769230769,
-0.153846153846154,-0.138461538461538,-0.123076923076923,-0.107692307692308,
-0.0923076923076923,-0.0769230769230769,-0.0615384615384615,-0.0461538461538462,
-0.0307692307692308,-0.0153846153846154,0.),.UNSPECIFIED.)
CURVE()
GEOMETRIC_REPRESENTATION_ITEM()
RATIONAL_B_SPLINE_CURVE((1.,1.,1.,1.,1.,1.,1.,1.,1.,1.,1.,1.,1.,1.,1.,1.,
1.,1.,1.,1.,1.,1.,1.,1.,1.,1.,1.,1.,1.,1.,1.,1.,1.,1.,1.,1.,1.,1.,1.,1.,
1.,1.,1.,1.,1.,1.,1.,1.,1.,1.,1.,1.,1.,1.,1.,1.,1.,1.,1.,1.,1.,1.,1.,1.,
1.,1.,1.,1.,1.,1.))
REPRESENTATION_ITEM('')
);
#327=(
BOUNDED_CURVE()
B_SPLINE_CURVE(5,(#48533,#48534,#48535,#48536,#48537,#48538,#48539,#48540,
#48541,#48542,#48543,#48544,#48545,#48546,#48547,#48548,#48549,#48550,#48551,
#48552,#48553,#48554,#48555,#48556,#48557,#48558,#48559,#48560,#48561,#48562,
#48563,#48564,#48565,#48566,#48567,#48568,#48569,#48570,#48571,#48572,#48573,
#48574,#48575,#48576,#48577,#48578,#48579,#48580,#48581,#48582,#48583,#48584,
#48585,#48586,#48587,#48588,#48589,#48590,#48591,#48592,#48593,#48594,#48595,
#48596,#48597,#48598,#48599,#48600,#48601,#48602),.UNSPECIFIED.,.F.,.F.)
B_SPLINE_CURVE_WITH_KNOTS((6,1,1,1,1,1,1,1,1,1,1,1,1,1,1,1,1,1,1,1,1,1,
1,1,1,1,1,1,1,1,1,1,1,1,1,1,1,1,1,1,1,1,1,1,1,1,1,1,1,1,1,1,1,1,1,1,1,1,
1,1,1,1,1,1,1,6),(-1.,-0.984615384615383,-0.969230769230768,-0.953846153846152,
-0.938461538461537,-0.923076923076922,-0.907692307692306,-0.892307692307691,
-0.876923076923076,-0.86153846153846,-0.846153846153845,-0.83076923076923,
-0.815384615384614,-0.799999999999999,-0.784615384615384,-0.769230769230768,
-0.753846153846153,-0.738461538461538,-0.723076923076922,-0.707692307692307,
-0.692307692307692,-0.676923076923076,-0.661538461538461,-0.646153846153846,
-0.63076923076923,-0.615384615384615,-0.6,-0.584615384615384,-0.569230769230769,
-0.553846153846154,-0.538461538461538,-0.523076923076923,-0.507692307692308,
-0.492307692307692,-0.476923076923077,-0.461538461538462,-0.446153846153846,
-0.430769230769231,-0.415384615384615,-0.4,-0.384615384615385,-0.369230769230769,
-0.353846153846154,-0.338461538461538,-0.323076923076923,-0.307692307692308,
-0.292307692307692,-0.276923076923077,-0.261538461538462,-0.246153846153846,
-0.230769230769231,-0.215384615384615,-0.2,-0.184615384615385,-0.169230769230769,
-0.153846153846154,-0.138461538461538,-0.123076923076923,-0.107692307692308,
-0.0923076923076923,-0.0769230769230769,-0.0615384615384615,-0.0461538461538462,
-0.0307692307692308,-0.0153846153846154,0.),.UNSPECIFIED.)
CURVE()
GEOMETRIC_REPRESENTATION_ITEM()
RATIONAL_B_SPLINE_CURVE((1.,1.,1.,1.,1.,1.,1.,1.,1.,1.,1.,1.,1.,1.,1.,1.,
1.,1.,1.,1.,1.,1.,1.,1.,1.,1.,1.,1.,1.,1.,1.,1.,1.,1.,1.,1.,1.,1.,1.,1.,
1.,1.,1.,1.,1.,1.,1.,1.,1.,1.,1.,1.,1.,1.,1.,1.,1.,1.,1.,1.,1.,1.,1.,1.,
1.,1.,1.,1.,1.,1.))
REPRESENTATION_ITEM('')
);
#328=(
BOUNDED_CURVE()
B_SPLINE_CURVE(5,(#48749,#48750,#48751,#48752,#48753,#48754,#48755,#48756,
#48757,#48758,#48759,#48760,#48761,#48762,#48763,#48764,#48765,#48766,#48767,
#48768,#48769,#48770,#48771,#48772,#48773,#48774,#48775,#48776,#48777,#48778,
#48779,#48780,#48781,#48782,#48783,#48784,#48785,#48786,#48787,#48788,#48789,
#48790,#48791,#48792,#48793,#48794,#48795,#48796,#48797,#48798,#48799,#48800,
#48801,#48802,#48803,#48804,#48805,#48806,#48807,#48808,#48809,#48810,#48811,
#48812,#48813,#48814,#48815,#48816,#48817,#48818),.UNSPECIFIED.,.F.,.F.)
B_SPLINE_CURVE_WITH_KNOTS((6,1,1,1,1,1,1,1,1,1,1,1,1,1,1,1,1,1,1,1,1,1,
1,1,1,1,1,1,1,1,1,1,1,1,1,1,1,1,1,1,1,1,1,1,1,1,1,1,1,1,1,1,1,1,1,1,1,1,
1,1,1,1,1,1,1,6),(-1.,-0.984615384615383,-0.969230769230768,-0.953846153846152,
-0.938461538461537,-0.923076923076922,-0.907692307692306,-0.892307692307691,
-0.876923076923076,-0.86153846153846,-0.846153846153845,-0.83076923076923,
-0.815384615384614,-0.799999999999999,-0.784615384615384,-0.769230769230768,
-0.753846153846153,-0.738461538461538,-0.723076923076922,-0.707692307692307,
-0.692307692307692,-0.676923076923076,-0.661538461538461,-0.646153846153846,
-0.63076923076923,-0.615384615384615,-0.6,-0.584615384615384,-0.569230769230769,
-0.553846153846154,-0.538461538461538,-0.523076923076923,-0.507692307692308,
-0.492307692307692,-0.476923076923077,-0.461538461538462,-0.446153846153846,
-0.430769230769231,-0.415384615384615,-0.4,-0.384615384615385,-0.369230769230769,
-0.353846153846154,-0.338461538461538,-0.323076923076923,-0.307692307692308,
-0.292307692307692,-0.276923076923077,-0.261538461538462,-0.246153846153846,
-0.230769230769231,-0.215384615384615,-0.2,-0.184615384615385,-0.169230769230769,
-0.153846153846154,-0.138461538461538,-0.123076923076923,-0.107692307692308,
-0.0923076923076923,-0.0769230769230769,-0.0615384615384615,-0.0461538461538462,
-0.0307692307692308,-0.0153846153846154,0.),.UNSPECIFIED.)
CURVE()
GEOMETRIC_REPRESENTATION_ITEM()
RATIONAL_B_SPLINE_CURVE((1.,1.,1.,1.,1.,1.,1.,1.,1.,1.,1.,1.,1.,1.,1.,1.,
1.,1.,1.,1.,1.,1.,1.,1.,1.,1.,1.,1.,1.,1.,1.,1.,1.,1.,1.,1.,1.,1.,1.,1.,
1.,1.,1.,1.,1.,1.,1.,1.,1.,1.,1.,1.,1.,1.,1.,1.,1.,1.,1.,1.,1.,1.,1.,1.,
1.,1.,1.,1.,1.,1.))
REPRESENTATION_ITEM('')
);
#329=(
BOUNDED_CURVE()
B_SPLINE_CURVE(5,(#48965,#48966,#48967,#48968,#48969,#48970,#48971,#48972,
#48973,#48974,#48975,#48976,#48977,#48978,#48979,#48980,#48981,#48982,#48983,
#48984,#48985,#48986,#48987,#48988,#48989,#48990,#48991,#48992,#48993,#48994,
#48995,#48996,#48997,#48998,#48999,#49000,#49001,#49002,#49003,#49004,#49005,
#49006,#49007,#49008,#49009,#49010,#49011,#49012,#49013,#49014,#49015,#49016,
#49017,#49018,#49019,#49020,#49021,#49022,#49023,#49024,#49025,#49026,#49027,
#49028,#49029,#49030,#49031,#49032,#49033,#49034),.UNSPECIFIED.,.F.,.F.)
B_SPLINE_CURVE_WITH_KNOTS((6,1,1,1,1,1,1,1,1,1,1,1,1,1,1,1,1,1,1,1,1,1,
1,1,1,1,1,1,1,1,1,1,1,1,1,1,1,1,1,1,1,1,1,1,1,1,1,1,1,1,1,1,1,1,1,1,1,1,
1,1,1,1,1,1,1,6),(-1.,-0.984615384615383,-0.969230769230768,-0.953846153846152,
-0.938461538461537,-0.923076923076922,-0.907692307692306,-0.892307692307691,
-0.876923076923076,-0.86153846153846,-0.846153846153845,-0.83076923076923,
-0.815384615384614,-0.799999999999999,-0.784615384615384,-0.769230769230768,
-0.753846153846153,-0.738461538461538,-0.723076923076922,-0.707692307692307,
-0.692307692307692,-0.676923076923076,-0.661538461538461,-0.646153846153846,
-0.63076923076923,-0.615384615384615,-0.6,-0.584615384615384,-0.569230769230769,
-0.553846153846154,-0.538461538461538,-0.523076923076923,-0.507692307692308,
-0.492307692307692,-0.476923076923077,-0.461538461538462,-0.446153846153846,
-0.430769230769231,-0.415384615384615,-0.4,-0.384615384615385,-0.369230769230769,
-0.353846153846154,-0.338461538461538,-0.323076923076923,-0.307692307692308,
-0.292307692307692,-0.276923076923077,-0.261538461538462,-0.246153846153846,
-0.230769230769231,-0.215384615384615,-0.2,-0.184615384615385,-0.169230769230769,
-0.153846153846154,-0.138461538461538,-0.123076923076923,-0.107692307692308,
-0.0923076923076923,-0.0769230769230769,-0.0615384615384615,-0.0461538461538462,
-0.0307692307692308,-0.0153846153846154,0.),.UNSPECIFIED.)
CURVE()
GEOMETRIC_REPRESENTATION_ITEM()
RATIONAL_B_SPLINE_CURVE((1.,1.,1.,1.,1.,1.,1.,1.,1.,1.,1.,1.,1.,1.,1.,1.,
1.,1.,1.,1.,1.,1.,1.,1.,1.,1.,1.,1.,1.,1.,1.,1.,1.,1.,1.,1.,1.,1.,1.,1.,
1.,1.,1.,1.,1.,1.,1.,1.,1.,1.,1.,1.,1.,1.,1.,1.,1.,1.,1.,1.,1.,1.,1.,1.,
1.,1.,1.,1.,1.,1.))
REPRESENTATION_ITEM('')
);
#330=(
BOUNDED_CURVE()
B_SPLINE_CURVE(5,(#49181,#49182,#49183,#49184,#49185,#49186,#49187,#49188,
#49189,#49190,#49191,#49192,#49193,#49194,#49195,#49196,#49197,#49198,#49199,
#49200,#49201,#49202,#49203,#49204,#49205,#49206,#49207,#49208,#49209,#49210,
#49211,#49212,#49213,#49214,#49215,#49216,#49217,#49218,#49219,#49220,#49221,
#49222,#49223,#49224,#49225,#49226,#49227,#49228,#49229,#49230,#49231,#49232,
#49233,#49234,#49235,#49236,#49237,#49238,#49239,#49240,#49241,#49242,#49243,
#49244,#49245,#49246,#49247,#49248,#49249,#49250),.UNSPECIFIED.,.F.,.F.)
B_SPLINE_CURVE_WITH_KNOTS((6,1,1,1,1,1,1,1,1,1,1,1,1,1,1,1,1,1,1,1,1,1,
1,1,1,1,1,1,1,1,1,1,1,1,1,1,1,1,1,1,1,1,1,1,1,1,1,1,1,1,1,1,1,1,1,1,1,1,
1,1,1,1,1,1,1,6),(-1.,-0.984615384615383,-0.969230769230768,-0.953846153846152,
-0.938461538461537,-0.923076923076922,-0.907692307692306,-0.892307692307691,
-0.876923076923076,-0.86153846153846,-0.846153846153845,-0.83076923076923,
-0.815384615384614,-0.799999999999999,-0.784615384615384,-0.769230769230768,
-0.753846153846153,-0.738461538461538,-0.723076923076922,-0.707692307692307,
-0.692307692307692,-0.676923076923076,-0.661538461538461,-0.646153846153846,
-0.63076923076923,-0.615384615384615,-0.6,-0.584615384615384,-0.569230769230769,
-0.553846153846154,-0.538461538461538,-0.523076923076923,-0.507692307692308,
-0.492307692307692,-0.476923076923077,-0.461538461538462,-0.446153846153846,
-0.430769230769231,-0.415384615384615,-0.4,-0.384615384615385,-0.369230769230769,
-0.353846153846154,-0.338461538461538,-0.323076923076923,-0.307692307692308,
-0.292307692307692,-0.276923076923077,-0.261538461538462,-0.246153846153846,
-0.230769230769231,-0.215384615384615,-0.2,-0.184615384615385,-0.169230769230769,
-0.153846153846154,-0.138461538461538,-0.123076923076923,-0.107692307692308,
-0.0923076923076923,-0.0769230769230769,-0.0615384615384615,-0.0461538461538462,
-0.0307692307692308,-0.0153846153846154,0.),.UNSPECIFIED.)
CURVE()
GEOMETRIC_REPRESENTATION_ITEM()
RATIONAL_B_SPLINE_CURVE((1.,1.,1.,1.,1.,1.,1.,1.,1.,1.,1.,1.,1.,1.,1.,1.,
1.,1.,1.,1.,1.,1.,1.,1.,1.,1.,1.,1.,1.,1.,1.,1.,1.,1.,1.,1.,1.,1.,1.,1.,
1.,1.,1.,1.,1.,1.,1.,1.,1.,1.,1.,1.,1.,1.,1.,1.,1.,1.,1.,1.,1.,1.,1.,1.,
1.,1.,1.,1.,1.,1.))
REPRESENTATION_ITEM('')
);
#331=(
BOUNDED_CURVE()
B_SPLINE_CURVE(5,(#49632,#49633,#49634,#49635,#49636,#49637,#49638,#49639,
#49640,#49641,#49642,#49643,#49644,#49645,#49646,#49647,#49648,#49649,#49650,
#49651,#49652,#49653,#49654,#49655,#49656,#49657,#49658,#49659,#49660,#49661,
#49662,#49663,#49664,#49665,#49666,#49667,#49668,#49669,#49670,#49671,#49672,
#49673,#49674,#49675,#49676,#49677,#49678,#49679,#49680,#49681,#49682,#49683,
#49684,#49685,#49686,#49687,#49688,#49689,#49690,#49691,#49692,#49693,#49694,
#49695,#49696,#49697,#49698,#49699,#49700,#49701),.UNSPECIFIED.,.F.,.F.)
B_SPLINE_CURVE_WITH_KNOTS((6,1,1,1,1,1,1,1,1,1,1,1,1,1,1,1,1,1,1,1,1,1,
1,1,1,1,1,1,1,1,1,1,1,1,1,1,1,1,1,1,1,1,1,1,1,1,1,1,1,1,1,1,1,1,1,1,1,1,
1,1,1,1,1,1,1,6),(0.00577184337450058,0.0153846153846154,0.0307692307692308,
0.0461538461538462,0.0615384615384615,0.0769230769230769,0.0923076923076923,
0.107692307692308,0.123076923076923,0.138461538461538,0.153846153846154,
0.169230769230769,0.184615384615385,0.2,0.215384615384615,0.230769230769231,
0.246153846153846,0.261538461538462,0.276923076923077,0.292307692307692,
0.307692307692308,0.323076923076923,0.338461538461538,0.353846153846154,
0.369230769230769,0.384615384615385,0.4,0.415384615384615,0.430769230769231,
0.446153846153846,0.461538461538462,0.476923076923077,0.492307692307692,
0.507692307692308,0.523076923076923,0.538461538461538,0.553846153846154,
0.569230769230769,0.584615384615384,0.6,0.615384615384615,0.63076923076923,
0.646153846153846,0.661538461538461,0.676923076923076,0.692307692307692,
0.707692307692307,0.723076923076922,0.738461538461538,0.753846153846153,
0.769230769230768,0.784615384615384,0.799999999999999,0.815384615384614,
0.83076923076923,0.846153846153845,0.86153846153846,0.876923076923076,0.892307692307691,
0.907692307692306,0.923076923076922,0.938461538461537,0.953846153846152,
0.969230769230768,0.984615384615383,1.),.UNSPECIFIED.)
CURVE()
GEOMETRIC_REPRESENTATION_ITEM()
RATIONAL_B_SPLINE_CURVE((1.,1.,1.,1.,1.,1.,1.,1.,1.,1.,1.,1.,1.,1.,1.,1.,
1.,1.,1.,1.,1.,1.,1.,1.,1.,1.,1.,1.,1.,1.,1.,1.,1.,1.,1.,1.,1.,1.,1.,1.,
1.,1.,1.,1.,1.,1.,1.,1.,1.,1.,1.,1.,1.,1.,1.,1.,1.,1.,1.,1.,1.,1.,1.,1.,
1.,1.,1.,1.,1.,1.))
REPRESENTATION_ITEM('')
);
#332=(
BOUNDED_CURVE()
B_SPLINE_CURVE(5,(#49705,#49706,#49707,#49708,#49709,#49710,#49711,#49712,
#49713,#49714,#49715,#49716,#49717,#49718,#49719,#49720,#49721,#49722,#49723,
#49724,#49725,#49726,#49727,#49728,#49729,#49730,#49731,#49732,#49733,#49734,
#49735,#49736,#49737,#49738,#49739,#49740,#49741,#49742,#49743,#49744,#49745,
#49746,#49747,#49748,#49749,#49750,#49751,#49752,#49753,#49754,#49755,#49756,
#49757,#49758,#49759,#49760,#49761,#49762,#49763,#49764,#49765,#49766,#49767,
#49768,#49769,#49770,#49771,#49772,#49773,#49774),.UNSPECIFIED.,.F.,.F.)
B_SPLINE_CURVE_WITH_KNOTS((6,1,1,1,1,1,1,1,1,1,1,1,1,1,1,1,1,1,1,1,1,1,
1,1,1,1,1,1,1,1,1,1,1,1,1,1,1,1,1,1,1,1,1,1,1,1,1,1,1,1,1,1,1,1,1,1,1,1,
1,1,1,1,1,1,1,6),(0.,0.0153846153846154,0.0307692307692308,0.0461538461538462,
0.0615384615384615,0.0769230769230769,0.0923076923076923,0.107692307692308,
0.123076923076923,0.138461538461538,0.153846153846154,0.169230769230769,
0.184615384615385,0.2,0.215384615384615,0.230769230769231,0.246153846153846,
0.261538461538462,0.276923076923077,0.292307692307692,0.307692307692308,
0.323076923076923,0.338461538461538,0.353846153846154,0.369230769230769,
0.384615384615385,0.4,0.415384615384615,0.430769230769231,0.446153846153846,
0.461538461538462,0.476923076923077,0.492307692307692,0.507692307692308,
0.523076923076923,0.538461538461538,0.553846153846154,0.569230769230769,
0.584615384615384,0.6,0.615384615384615,0.63076923076923,0.646153846153846,
0.661538461538461,0.676923076923076,0.692307692307692,0.707692307692307,
0.723076923076922,0.738461538461538,0.753846153846153,0.769230769230768,
0.784615384615384,0.799999999999999,0.815384615384614,0.83076923076923,
0.846153846153845,0.86153846153846,0.876923076923076,0.892307692307691,
0.907692307692306,0.923076923076922,0.938461538461537,0.953846153846152,
0.969230769230768,0.984615384615383,0.994228156739708),.UNSPECIFIED.)
CURVE()
GEOMETRIC_REPRESENTATION_ITEM()
RATIONAL_B_SPLINE_CURVE((1.,1.,1.,1.,1.,1.,1.,1.,1.,1.,1.,1.,1.,1.,1.,1.,
1.,1.,1.,1.,1.,1.,1.,1.,1.,1.,1.,1.,1.,1.,1.,1.,1.,1.,1.,1.,1.,1.,1.,1.,
1.,1.,1.,1.,1.,1.,1.,1.,1.,1.,1.,1.,1.,1.,1.,1.,1.,1.,1.,1.,1.,1.,1.,1.,
1.,1.,1.,1.,1.,1.))
REPRESENTATION_ITEM('')
);
#333=(
BOUNDED_CURVE()
B_SPLINE_CURVE(5,(#49778,#49779,#49780,#49781,#49782,#49783,#49784,#49785,
#49786,#49787,#49788,#49789,#49790,#49791,#49792,#49793,#49794,#49795,#49796,
#49797,#49798,#49799,#49800,#49801,#49802,#49803,#49804,#49805,#49806,#49807,
#49808,#49809,#49810,#49811,#49812,#49813,#49814,#49815,#49816,#49817,#49818,
#49819,#49820,#49821,#49822,#49823,#49824,#49825,#49826,#49827,#49828,#49829,
#49830,#49831,#49832,#49833,#49834,#49835,#49836,#49837,#49838,#49839,#49840,
#49841,#49842,#49843,#49844,#49845,#49846,#49847),.UNSPECIFIED.,.F.,.F.)
B_SPLINE_CURVE_WITH_KNOTS((6,1,1,1,1,1,1,1,1,1,1,1,1,1,1,1,1,1,1,1,1,1,
1,1,1,1,1,1,1,1,1,1,1,1,1,1,1,1,1,1,1,1,1,1,1,1,1,1,1,1,1,1,1,1,1,1,1,1,
1,1,1,1,1,1,1,6),(0.0057718433745091,0.0153846153846154,0.0307692307692308,
0.0461538461538462,0.0615384615384615,0.0769230769230769,0.0923076923076923,
0.107692307692308,0.123076923076923,0.138461538461538,0.153846153846154,
0.169230769230769,0.184615384615385,0.2,0.215384615384615,0.230769230769231,
0.246153846153846,0.261538461538462,0.276923076923077,0.292307692307692,
0.307692307692308,0.323076923076923,0.338461538461538,0.353846153846154,
0.369230769230769,0.384615384615385,0.4,0.415384615384615,0.430769230769231,
0.446153846153846,0.461538461538462,0.476923076923077,0.492307692307692,
0.507692307692308,0.523076923076923,0.538461538461538,0.553846153846154,
0.569230769230769,0.584615384615384,0.6,0.615384615384615,0.63076923076923,
0.646153846153846,0.661538461538461,0.676923076923076,0.692307692307692,
0.707692307692307,0.723076923076922,0.738461538461538,0.753846153846153,
0.769230769230768,0.784615384615384,0.799999999999999,0.815384615384614,
0.83076923076923,0.846153846153845,0.86153846153846,0.876923076923076,0.892307692307691,
0.907692307692306,0.923076923076922,0.938461538461537,0.953846153846152,
0.969230769230768,0.984615384615383,1.),.UNSPECIFIED.)
CURVE()
GEOMETRIC_REPRESENTATION_ITEM()
RATIONAL_B_SPLINE_CURVE((1.,1.,1.,1.,1.,1.,1.,1.,1.,1.,1.,1.,1.,1.,1.,1.,
1.,1.,1.,1.,1.,1.,1.,1.,1.,1.,1.,1.,1.,1.,1.,1.,1.,1.,1.,1.,1.,1.,1.,1.,
1.,1.,1.,1.,1.,1.,1.,1.,1.,1.,1.,1.,1.,1.,1.,1.,1.,1.,1.,1.,1.,1.,1.,1.,
1.,1.,1.,1.,1.,1.))
REPRESENTATION_ITEM('')
);
#334=(
BOUNDED_CURVE()
B_SPLINE_CURVE(5,(#49851,#49852,#49853,#49854,#49855,#49856,#49857,#49858,
#49859,#49860,#49861,#49862,#49863,#49864,#49865,#49866,#49867,#49868,#49869,
#49870,#49871,#49872,#49873,#49874,#49875,#49876,#49877,#49878,#49879,#49880,
#49881,#49882,#49883,#49884,#49885,#49886,#49887,#49888,#49889,#49890,#49891,
#49892,#49893,#49894,#49895,#49896,#49897,#49898,#49899,#49900,#49901,#49902,
#49903,#49904,#49905,#49906,#49907,#49908,#49909,#49910,#49911,#49912,#49913,
#49914,#49915,#49916,#49917,#49918,#49919,#49920),.UNSPECIFIED.,.F.,.F.)
B_SPLINE_CURVE_WITH_KNOTS((6,1,1,1,1,1,1,1,1,1,1,1,1,1,1,1,1,1,1,1,1,1,
1,1,1,1,1,1,1,1,1,1,1,1,1,1,1,1,1,1,1,1,1,1,1,1,1,1,1,1,1,1,1,1,1,1,1,1,
1,1,1,1,1,1,1,6),(0.,0.0153846153846154,0.0307692307692308,0.0461538461538462,
0.0615384615384615,0.0769230769230769,0.0923076923076923,0.107692307692308,
0.123076923076923,0.138461538461538,0.153846153846154,0.169230769230769,
0.184615384615385,0.2,0.215384615384615,0.230769230769231,0.246153846153846,
0.261538461538462,0.276923076923077,0.292307692307692,0.307692307692308,
0.323076923076923,0.338461538461538,0.353846153846154,0.369230769230769,
0.384615384615385,0.4,0.415384615384615,0.430769230769231,0.446153846153846,
0.461538461538462,0.476923076923077,0.492307692307692,0.507692307692308,
0.523076923076923,0.538461538461538,0.553846153846154,0.569230769230769,
0.584615384615384,0.6,0.615384615384615,0.63076923076923,0.646153846153846,
0.661538461538461,0.676923076923076,0.692307692307692,0.707692307692307,
0.723076923076922,0.738461538461538,0.753846153846153,0.769230769230768,
0.784615384615384,0.799999999999999,0.815384615384614,0.83076923076923,
0.846153846153845,0.86153846153846,0.876923076923076,0.892307692307691,
0.907692307692306,0.923076923076922,0.938461538461537,0.953846153846152,
0.969230769230768,0.984615384615383,0.994228156739689),.UNSPECIFIED.)
CURVE()
GEOMETRIC_REPRESENTATION_ITEM()
RATIONAL_B_SPLINE_CURVE((1.,1.,1.,1.,1.,1.,1.,1.,1.,1.,1.,1.,1.,1.,1.,1.,
1.,1.,1.,1.,1.,1.,1.,1.,1.,1.,1.,1.,1.,1.,1.,1.,1.,1.,1.,1.,1.,1.,1.,1.,
1.,1.,1.,1.,1.,1.,1.,1.,1.,1.,1.,1.,1.,1.,1.,1.,1.,1.,1.,1.,1.,1.,1.,1.,
1.,1.,1.,1.,1.,1.))
REPRESENTATION_ITEM('')
);
#335=(
BOUNDED_CURVE()
B_SPLINE_CURVE(5,(#49924,#49925,#49926,#49927,#49928,#49929,#49930,#49931,
#49932,#49933,#49934,#49935,#49936,#49937,#49938,#49939,#49940,#49941,#49942,
#49943,#49944,#49945,#49946,#49947,#49948,#49949,#49950,#49951,#49952,#49953,
#49954,#49955,#49956,#49957,#49958,#49959,#49960,#49961,#49962,#49963,#49964,
#49965,#49966,#49967,#49968,#49969,#49970,#49971,#49972,#49973,#49974,#49975,
#49976,#49977,#49978,#49979,#49980,#49981,#49982,#49983,#49984,#49985,#49986,
#49987,#49988,#49989,#49990,#49991,#49992,#49993),.UNSPECIFIED.,.F.,.F.)
B_SPLINE_CURVE_WITH_KNOTS((6,1,1,1,1,1,1,1,1,1,1,1,1,1,1,1,1,1,1,1,1,1,
1,1,1,1,1,1,1,1,1,1,1,1,1,1,1,1,1,1,1,1,1,1,1,1,1,1,1,1,1,1,1,1,1,1,1,1,
1,1,1,1,1,1,1,6),(0.00577184337448946,0.0153846153846154,0.0307692307692308,
0.0461538461538462,0.0615384615384615,0.0769230769230769,0.0923076923076923,
0.107692307692308,0.123076923076923,0.138461538461538,0.153846153846154,
0.169230769230769,0.184615384615385,0.2,0.215384615384615,0.230769230769231,
0.246153846153846,0.261538461538462,0.276923076923077,0.292307692307692,
0.307692307692308,0.323076923076923,0.338461538461538,0.353846153846154,
0.369230769230769,0.384615384615385,0.4,0.415384615384615,0.430769230769231,
0.446153846153846,0.461538461538462,0.476923076923077,0.492307692307692,
0.507692307692308,0.523076923076923,0.538461538461538,0.553846153846154,
0.569230769230769,0.584615384615384,0.6,0.615384615384615,0.63076923076923,
0.646153846153846,0.661538461538461,0.676923076923076,0.692307692307692,
0.707692307692307,0.723076923076922,0.738461538461538,0.753846153846153,
0.769230769230768,0.784615384615384,0.799999999999999,0.815384615384614,
0.83076923076923,0.846153846153845,0.86153846153846,0.876923076923076,0.892307692307691,
0.907692307692306,0.923076923076922,0.938461538461537,0.953846153846152,
0.969230769230768,0.984615384615383,1.),.UNSPECIFIED.)
CURVE()
GEOMETRIC_REPRESENTATION_ITEM()
RATIONAL_B_SPLINE_CURVE((1.,1.,1.,1.,1.,1.,1.,1.,1.,1.,1.,1.,1.,1.,1.,1.,
1.,1.,1.,1.,1.,1.,1.,1.,1.,1.,1.,1.,1.,1.,1.,1.,1.,1.,1.,1.,1.,1.,1.,1.,
1.,1.,1.,1.,1.,1.,1.,1.,1.,1.,1.,1.,1.,1.,1.,1.,1.,1.,1.,1.,1.,1.,1.,1.,
1.,1.,1.,1.,1.,1.))
REPRESENTATION_ITEM('')
);
#336=(
BOUNDED_CURVE()
B_SPLINE_CURVE(5,(#49997,#49998,#49999,#50000,#50001,#50002,#50003,#50004,
#50005,#50006,#50007,#50008,#50009,#50010,#50011,#50012,#50013,#50014,#50015,
#50016,#50017,#50018,#50019,#50020,#50021,#50022,#50023,#50024,#50025,#50026,
#50027,#50028,#50029,#50030,#50031,#50032,#50033,#50034,#50035,#50036,#50037,
#50038,#50039,#50040,#50041,#50042,#50043,#50044,#50045,#50046,#50047,#50048,
#50049,#50050,#50051,#50052,#50053,#50054,#50055,#50056,#50057,#50058,#50059,
#50060,#50061,#50062,#50063,#50064,#50065,#50066),.UNSPECIFIED.,.F.,.F.)
B_SPLINE_CURVE_WITH_KNOTS((6,1,1,1,1,1,1,1,1,1,1,1,1,1,1,1,1,1,1,1,1,1,
1,1,1,1,1,1,1,1,1,1,1,1,1,1,1,1,1,1,1,1,1,1,1,1,1,1,1,1,1,1,1,1,1,1,1,1,
1,1,1,1,1,1,1,6),(0.,0.0153846153846154,0.0307692307692308,0.0461538461538462,
0.0615384615384615,0.0769230769230769,0.0923076923076923,0.107692307692308,
0.123076923076923,0.138461538461538,0.153846153846154,0.169230769230769,
0.184615384615385,0.2,0.215384615384615,0.230769230769231,0.246153846153846,
0.261538461538462,0.276923076923077,0.292307692307692,0.307692307692308,
0.323076923076923,0.338461538461538,0.353846153846154,0.369230769230769,
0.384615384615385,0.4,0.415384615384615,0.430769230769231,0.446153846153846,
0.461538461538462,0.476923076923077,0.492307692307692,0.507692307692308,
0.523076923076923,0.538461538461538,0.553846153846154,0.569230769230769,
0.584615384615384,0.6,0.615384615384615,0.63076923076923,0.646153846153846,
0.661538461538461,0.676923076923076,0.692307692307692,0.707692307692307,
0.723076923076922,0.738461538461538,0.753846153846153,0.769230769230768,
0.784615384615384,0.799999999999999,0.815384615384614,0.83076923076923,
0.846153846153845,0.86153846153846,0.876923076923076,0.892307692307691,
0.907692307692306,0.923076923076922,0.938461538461537,0.953846153846152,
0.969230769230768,0.984615384615383,0.994228156739718),.UNSPECIFIED.)
CURVE()
GEOMETRIC_REPRESENTATION_ITEM()
RATIONAL_B_SPLINE_CURVE((1.,1.,1.,1.,1.,1.,1.,1.,1.,1.,1.,1.,1.,1.,1.,1.,
1.,1.,1.,1.,1.,1.,1.,1.,1.,1.,1.,1.,1.,1.,1.,1.,1.,1.,1.,1.,1.,1.,1.,1.,
1.,1.,1.,1.,1.,1.,1.,1.,1.,1.,1.,1.,1.,1.,1.,1.,1.,1.,1.,1.,1.,1.,1.,1.,
1.,1.,1.,1.,1.,1.))
REPRESENTATION_ITEM('')
);
#337=(
BOUNDED_CURVE()
B_SPLINE_CURVE(5,(#50070,#50071,#50072,#50073,#50074,#50075,#50076,#50077,
#50078,#50079,#50080,#50081,#50082,#50083,#50084,#50085,#50086,#50087,#50088,
#50089,#50090,#50091,#50092,#50093,#50094,#50095,#50096,#50097,#50098,#50099,
#50100,#50101,#50102,#50103,#50104,#50105,#50106,#50107,#50108,#50109,#50110,
#50111,#50112,#50113,#50114,#50115,#50116,#50117,#50118,#50119,#50120,#50121,
#50122,#50123,#50124,#50125,#50126,#50127,#50128,#50129,#50130,#50131,#50132,
#50133,#50134,#50135,#50136,#50137,#50138,#50139),.UNSPECIFIED.,.F.,.F.)
B_SPLINE_CURVE_WITH_KNOTS((6,1,1,1,1,1,1,1,1,1,1,1,1,1,1,1,1,1,1,1,1,1,
1,1,1,1,1,1,1,1,1,1,1,1,1,1,1,1,1,1,1,1,1,1,1,1,1,1,1,1,1,1,1,1,1,1,1,1,
1,1,1,1,1,1,1,6),(0.00577184337450897,0.0153846153846154,0.0307692307692308,
0.0461538461538462,0.0615384615384615,0.0769230769230769,0.0923076923076923,
0.107692307692308,0.123076923076923,0.138461538461538,0.153846153846154,
0.169230769230769,0.184615384615385,0.2,0.215384615384615,0.230769230769231,
0.246153846153846,0.261538461538462,0.276923076923077,0.292307692307692,
0.307692307692308,0.323076923076923,0.338461538461538,0.353846153846154,
0.369230769230769,0.384615384615385,0.4,0.415384615384615,0.430769230769231,
0.446153846153846,0.461538461538462,0.476923076923077,0.492307692307692,
0.507692307692308,0.523076923076923,0.538461538461538,0.553846153846154,
0.569230769230769,0.584615384615384,0.6,0.615384615384615,0.63076923076923,
0.646153846153846,0.661538461538461,0.676923076923076,0.692307692307692,
0.707692307692307,0.723076923076922,0.738461538461538,0.753846153846153,
0.769230769230768,0.784615384615384,0.799999999999999,0.815384615384614,
0.83076923076923,0.846153846153845,0.86153846153846,0.876923076923076,0.892307692307691,
0.907692307692306,0.923076923076922,0.938461538461537,0.953846153846152,
0.969230769230768,0.984615384615383,1.),.UNSPECIFIED.)
CURVE()
GEOMETRIC_REPRESENTATION_ITEM()
RATIONAL_B_SPLINE_CURVE((1.,1.,1.,1.,1.,1.,1.,1.,1.,1.,1.,1.,1.,1.,1.,1.,
1.,1.,1.,1.,1.,1.,1.,1.,1.,1.,1.,1.,1.,1.,1.,1.,1.,1.,1.,1.,1.,1.,1.,1.,
1.,1.,1.,1.,1.,1.,1.,1.,1.,1.,1.,1.,1.,1.,1.,1.,1.,1.,1.,1.,1.,1.,1.,1.,
1.,1.,1.,1.,1.,1.))
REPRESENTATION_ITEM('')
);
#338=(
BOUNDED_CURVE()
B_SPLINE_CURVE(5,(#50143,#50144,#50145,#50146,#50147,#50148,#50149,#50150,
#50151,#50152,#50153,#50154,#50155,#50156,#50157,#50158,#50159,#50160,#50161,
#50162,#50163,#50164,#50165,#50166,#50167,#50168,#50169,#50170,#50171,#50172,
#50173,#50174,#50175,#50176,#50177,#50178,#50179,#50180,#50181,#50182,#50183,
#50184,#50185,#50186,#50187,#50188,#50189,#50190,#50191,#50192,#50193,#50194,
#50195,#50196,#50197,#50198,#50199,#50200,#50201,#50202,#50203,#50204,#50205,
#50206,#50207,#50208,#50209,#50210,#50211,#50212),.UNSPECIFIED.,.F.,.F.)
B_SPLINE_CURVE_WITH_KNOTS((6,1,1,1,1,1,1,1,1,1,1,1,1,1,1,1,1,1,1,1,1,1,
1,1,1,1,1,1,1,1,1,1,1,1,1,1,1,1,1,1,1,1,1,1,1,1,1,1,1,1,1,1,1,1,1,1,1,1,
1,1,1,1,1,1,1,6),(0.,0.0153846153846154,0.0307692307692308,0.0461538461538462,
0.0615384615384615,0.0769230769230769,0.0923076923076923,0.107692307692308,
0.123076923076923,0.138461538461538,0.153846153846154,0.169230769230769,
0.184615384615385,0.2,0.215384615384615,0.230769230769231,0.246153846153846,
0.261538461538462,0.276923076923077,0.292307692307692,0.307692307692308,
0.323076923076923,0.338461538461538,0.353846153846154,0.369230769230769,
0.384615384615385,0.4,0.415384615384615,0.430769230769231,0.446153846153846,
0.461538461538462,0.476923076923077,0.492307692307692,0.507692307692308,
0.523076923076923,0.538461538461538,0.553846153846154,0.569230769230769,
0.584615384615384,0.6,0.615384615384615,0.63076923076923,0.646153846153846,
0.661538461538461,0.676923076923076,0.692307692307692,0.707692307692307,
0.723076923076922,0.738461538461538,0.753846153846153,0.769230769230768,
0.784615384615384,0.799999999999999,0.815384615384614,0.83076923076923,
0.846153846153845,0.86153846153846,0.876923076923076,0.892307692307691,
0.907692307692306,0.923076923076922,0.938461538461537,0.953846153846152,
0.969230769230768,0.984615384615383,0.994228156739701),.UNSPECIFIED.)
CURVE()
GEOMETRIC_REPRESENTATION_ITEM()
RATIONAL_B_SPLINE_CURVE((1.,1.,1.,1.,1.,1.,1.,1.,1.,1.,1.,1.,1.,1.,1.,1.,
1.,1.,1.,1.,1.,1.,1.,1.,1.,1.,1.,1.,1.,1.,1.,1.,1.,1.,1.,1.,1.,1.,1.,1.,
1.,1.,1.,1.,1.,1.,1.,1.,1.,1.,1.,1.,1.,1.,1.,1.,1.,1.,1.,1.,1.,1.,1.,1.,
1.,1.,1.,1.,1.,1.))
REPRESENTATION_ITEM('')
);
#339=(
BOUNDED_CURVE()
B_SPLINE_CURVE(5,(#50216,#50217,#50218,#50219,#50220,#50221,#50222,#50223,
#50224,#50225,#50226,#50227,#50228,#50229,#50230,#50231,#50232,#50233,#50234,
#50235,#50236,#50237,#50238,#50239,#50240,#50241,#50242,#50243,#50244,#50245,
#50246,#50247,#50248,#50249,#50250,#50251,#50252,#50253,#50254,#50255,#50256,
#50257,#50258,#50259,#50260,#50261,#50262,#50263,#50264,#50265,#50266,#50267,
#50268,#50269,#50270,#50271,#50272,#50273,#50274,#50275,#50276,#50277,#50278,
#50279,#50280,#50281,#50282,#50283,#50284,#50285),.UNSPECIFIED.,.F.,.F.)
B_SPLINE_CURVE_WITH_KNOTS((6,1,1,1,1,1,1,1,1,1,1,1,1,1,1,1,1,1,1,1,1,1,
1,1,1,1,1,1,1,1,1,1,1,1,1,1,1,1,1,1,1,1,1,1,1,1,1,1,1,1,1,1,1,1,1,1,1,1,
1,1,1,1,1,1,1,6),(0.00577184337451001,0.0153846153846154,0.0307692307692308,
0.0461538461538462,0.0615384615384615,0.0769230769230769,0.0923076923076923,
0.107692307692308,0.123076923076923,0.138461538461538,0.153846153846154,
0.169230769230769,0.184615384615385,0.2,0.215384615384615,0.230769230769231,
0.246153846153846,0.261538461538462,0.276923076923077,0.292307692307692,
0.307692307692308,0.323076923076923,0.338461538461538,0.353846153846154,
0.369230769230769,0.384615384615385,0.4,0.415384615384615,0.430769230769231,
0.446153846153846,0.461538461538462,0.476923076923077,0.492307692307692,
0.507692307692308,0.523076923076923,0.538461538461538,0.553846153846154,
0.569230769230769,0.584615384615384,0.6,0.615384615384615,0.63076923076923,
0.646153846153846,0.661538461538461,0.676923076923076,0.692307692307692,
0.707692307692307,0.723076923076922,0.738461538461538,0.753846153846153,
0.769230769230768,0.784615384615384,0.799999999999999,0.815384615384614,
0.83076923076923,0.846153846153845,0.86153846153846,0.876923076923076,0.892307692307691,
0.907692307692306,0.923076923076922,0.938461538461537,0.953846153846152,
0.969230769230768,0.984615384615383,1.),.UNSPECIFIED.)
CURVE()
GEOMETRIC_REPRESENTATION_ITEM()
RATIONAL_B_SPLINE_CURVE((1.,1.,1.,1.,1.,1.,1.,1.,1.,1.,1.,1.,1.,1.,1.,1.,
1.,1.,1.,1.,1.,1.,1.,1.,1.,1.,1.,1.,1.,1.,1.,1.,1.,1.,1.,1.,1.,1.,1.,1.,
1.,1.,1.,1.,1.,1.,1.,1.,1.,1.,1.,1.,1.,1.,1.,1.,1.,1.,1.,1.,1.,1.,1.,1.,
1.,1.,1.,1.,1.,1.))
REPRESENTATION_ITEM('')
);
#340=(
BOUNDED_CURVE()
B_SPLINE_CURVE(5,(#50289,#50290,#50291,#50292,#50293,#50294,#50295,#50296,
#50297,#50298,#50299,#50300,#50301,#50302,#50303,#50304,#50305,#50306,#50307,
#50308,#50309,#50310,#50311,#50312,#50313,#50314,#50315,#50316,#50317,#50318,
#50319,#50320,#50321,#50322,#50323,#50324,#50325,#50326,#50327,#50328,#50329,
#50330,#50331,#50332,#50333,#50334,#50335,#50336,#50337,#50338,#50339,#50340,
#50341,#50342,#50343,#50344,#50345,#50346,#50347,#50348,#50349,#50350,#50351,
#50352,#50353,#50354,#50355,#50356,#50357,#50358),.UNSPECIFIED.,.F.,.F.)
B_SPLINE_CURVE_WITH_KNOTS((6,1,1,1,1,1,1,1,1,1,1,1,1,1,1,1,1,1,1,1,1,1,
1,1,1,1,1,1,1,1,1,1,1,1,1,1,1,1,1,1,1,1,1,1,1,1,1,1,1,1,1,1,1,1,1,1,1,1,
1,1,1,1,1,1,1,6),(0.,0.0153846153846154,0.0307692307692308,0.0461538461538462,
0.0615384615384615,0.0769230769230769,0.0923076923076923,0.107692307692308,
0.123076923076923,0.138461538461538,0.153846153846154,0.169230769230769,
0.184615384615385,0.2,0.215384615384615,0.230769230769231,0.246153846153846,
0.261538461538462,0.276923076923077,0.292307692307692,0.307692307692308,
0.323076923076923,0.338461538461538,0.353846153846154,0.369230769230769,
0.384615384615385,0.4,0.415384615384615,0.430769230769231,0.446153846153846,
0.461538461538462,0.476923076923077,0.492307692307692,0.507692307692308,
0.523076923076923,0.538461538461538,0.553846153846154,0.569230769230769,
0.584615384615384,0.6,0.615384615384615,0.63076923076923,0.646153846153846,
0.661538461538461,0.676923076923076,0.692307692307692,0.707692307692307,
0.723076923076922,0.738461538461538,0.753846153846153,0.769230769230768,
0.784615384615384,0.799999999999999,0.815384615384614,0.83076923076923,
0.846153846153845,0.86153846153846,0.876923076923076,0.892307692307691,
0.907692307692306,0.923076923076922,0.938461538461537,0.953846153846152,
0.969230769230768,0.984615384615383,0.994228156739697),.UNSPECIFIED.)
CURVE()
GEOMETRIC_REPRESENTATION_ITEM()
RATIONAL_B_SPLINE_CURVE((1.,1.,1.,1.,1.,1.,1.,1.,1.,1.,1.,1.,1.,1.,1.,1.,
1.,1.,1.,1.,1.,1.,1.,1.,1.,1.,1.,1.,1.,1.,1.,1.,1.,1.,1.,1.,1.,1.,1.,1.,
1.,1.,1.,1.,1.,1.,1.,1.,1.,1.,1.,1.,1.,1.,1.,1.,1.,1.,1.,1.,1.,1.,1.,1.,
1.,1.,1.,1.,1.,1.))
REPRESENTATION_ITEM('')
);
#341=(
BOUNDED_CURVE()
B_SPLINE_CURVE(5,(#50362,#50363,#50364,#50365,#50366,#50367,#50368,#50369,
#50370,#50371,#50372,#50373,#50374,#50375,#50376,#50377,#50378,#50379,#50380,
#50381,#50382,#50383,#50384,#50385,#50386,#50387,#50388,#50389,#50390,#50391,
#50392,#50393,#50394,#50395,#50396,#50397,#50398,#50399,#50400,#50401,#50402,
#50403,#50404,#50405,#50406,#50407,#50408,#50409,#50410,#50411,#50412,#50413,
#50414,#50415,#50416,#50417,#50418,#50419,#50420,#50421,#50422,#50423,#50424,
#50425,#50426,#50427,#50428,#50429,#50430,#50431),.UNSPECIFIED.,.F.,.F.)
B_SPLINE_CURVE_WITH_KNOTS((6,1,1,1,1,1,1,1,1,1,1,1,1,1,1,1,1,1,1,1,1,1,
1,1,1,1,1,1,1,1,1,1,1,1,1,1,1,1,1,1,1,1,1,1,1,1,1,1,1,1,1,1,1,1,1,1,1,1,
1,1,1,1,1,1,1,6),(0.00577184337452306,0.0153846153846154,0.0307692307692308,
0.0461538461538462,0.0615384615384615,0.0769230769230769,0.0923076923076923,
0.107692307692308,0.123076923076923,0.138461538461538,0.153846153846154,
0.169230769230769,0.184615384615385,0.2,0.215384615384615,0.230769230769231,
0.246153846153846,0.261538461538462,0.276923076923077,0.292307692307692,
0.307692307692308,0.323076923076923,0.338461538461538,0.353846153846154,
0.369230769230769,0.384615384615385,0.4,0.415384615384615,0.430769230769231,
0.446153846153846,0.461538461538462,0.476923076923077,0.492307692307692,
0.507692307692308,0.523076923076923,0.538461538461538,0.553846153846154,
0.569230769230769,0.584615384615384,0.6,0.615384615384615,0.63076923076923,
0.646153846153846,0.661538461538461,0.676923076923076,0.692307692307692,
0.707692307692307,0.723076923076922,0.738461538461538,0.753846153846153,
0.769230769230768,0.784615384615384,0.799999999999999,0.815384615384614,
0.83076923076923,0.846153846153845,0.86153846153846,0.876923076923076,0.892307692307691,
0.907692307692306,0.923076923076922,0.938461538461537,0.953846153846152,
0.969230769230768,0.984615384615383,1.),.UNSPECIFIED.)
CURVE()
GEOMETRIC_REPRESENTATION_ITEM()
RATIONAL_B_SPLINE_CURVE((1.,1.,1.,1.,1.,1.,1.,1.,1.,1.,1.,1.,1.,1.,1.,1.,
1.,1.,1.,1.,1.,1.,1.,1.,1.,1.,1.,1.,1.,1.,1.,1.,1.,1.,1.,1.,1.,1.,1.,1.,
1.,1.,1.,1.,1.,1.,1.,1.,1.,1.,1.,1.,1.,1.,1.,1.,1.,1.,1.,1.,1.,1.,1.,1.,
1.,1.,1.,1.,1.,1.))
REPRESENTATION_ITEM('')
);
#342=(
BOUNDED_CURVE()
B_SPLINE_CURVE(5,(#50435,#50436,#50437,#50438,#50439,#50440,#50441,#50442,
#50443,#50444,#50445,#50446,#50447,#50448,#50449,#50450,#50451,#50452,#50453,
#50454,#50455,#50456,#50457,#50458,#50459,#50460,#50461,#50462,#50463,#50464,
#50465,#50466,#50467,#50468,#50469,#50470,#50471,#50472,#50473,#50474,#50475,
#50476,#50477,#50478,#50479,#50480,#50481,#50482,#50483,#50484,#50485,#50486,
#50487,#50488,#50489,#50490,#50491,#50492,#50493,#50494,#50495,#50496,#50497,
#50498,#50499,#50500,#50501,#50502,#50503,#50504),.UNSPECIFIED.,.F.,.F.)
B_SPLINE_CURVE_WITH_KNOTS((6,1,1,1,1,1,1,1,1,1,1,1,1,1,1,1,1,1,1,1,1,1,
1,1,1,1,1,1,1,1,1,1,1,1,1,1,1,1,1,1,1,1,1,1,1,1,1,1,1,1,1,1,1,1,1,1,1,1,
1,1,1,1,1,1,1,6),(0.,0.0153846153846154,0.0307692307692308,0.0461538461538462,
0.0615384615384615,0.0769230769230769,0.0923076923076923,0.107692307692308,
0.123076923076923,0.138461538461538,0.153846153846154,0.169230769230769,
0.184615384615385,0.2,0.215384615384615,0.230769230769231,0.246153846153846,
0.261538461538462,0.276923076923077,0.292307692307692,0.307692307692308,
0.323076923076923,0.338461538461538,0.353846153846154,0.369230769230769,
0.384615384615385,0.4,0.415384615384615,0.430769230769231,0.446153846153846,
0.461538461538462,0.476923076923077,0.492307692307692,0.507692307692308,
0.523076923076923,0.538461538461538,0.553846153846154,0.569230769230769,
0.584615384615384,0.6,0.615384615384615,0.63076923076923,0.646153846153846,
0.661538461538461,0.676923076923076,0.692307692307692,0.707692307692307,
0.723076923076922,0.738461538461538,0.753846153846153,0.769230769230768,
0.784615384615384,0.799999999999999,0.815384615384614,0.83076923076923,
0.846153846153845,0.86153846153846,0.876923076923076,0.892307692307691,
0.907692307692306,0.923076923076922,0.938461538461537,0.953846153846152,
0.969230769230768,0.984615384615383,0.994228156739688),.UNSPECIFIED.)
CURVE()
GEOMETRIC_REPRESENTATION_ITEM()
RATIONAL_B_SPLINE_CURVE((1.,1.,1.,1.,1.,1.,1.,1.,1.,1.,1.,1.,1.,1.,1.,1.,
1.,1.,1.,1.,1.,1.,1.,1.,1.,1.,1.,1.,1.,1.,1.,1.,1.,1.,1.,1.,1.,1.,1.,1.,
1.,1.,1.,1.,1.,1.,1.,1.,1.,1.,1.,1.,1.,1.,1.,1.,1.,1.,1.,1.,1.,1.,1.,1.,
1.,1.,1.,1.,1.,1.))
REPRESENTATION_ITEM('')
);
#343=(
BOUNDED_CURVE()
B_SPLINE_CURVE(5,(#50508,#50509,#50510,#50511,#50512,#50513,#50514,#50515,
#50516,#50517,#50518,#50519,#50520,#50521,#50522,#50523,#50524,#50525,#50526,
#50527,#50528,#50529,#50530,#50531,#50532,#50533,#50534,#50535,#50536,#50537,
#50538,#50539,#50540,#50541,#50542,#50543,#50544,#50545,#50546,#50547,#50548,
#50549,#50550,#50551,#50552,#50553,#50554,#50555,#50556,#50557,#50558,#50559,
#50560,#50561,#50562,#50563,#50564,#50565,#50566,#50567,#50568,#50569,#50570,
#50571,#50572,#50573,#50574,#50575,#50576,#50577),.UNSPECIFIED.,.F.,.F.)
B_SPLINE_CURVE_WITH_KNOTS((6,1,1,1,1,1,1,1,1,1,1,1,1,1,1,1,1,1,1,1,1,1,
1,1,1,1,1,1,1,1,1,1,1,1,1,1,1,1,1,1,1,1,1,1,1,1,1,1,1,1,1,1,1,1,1,1,1,1,
1,1,1,1,1,1,1,6),(0.00577184337449862,0.0153846153846154,0.0307692307692308,
0.0461538461538462,0.0615384615384615,0.0769230769230769,0.0923076923076923,
0.107692307692308,0.123076923076923,0.138461538461538,0.153846153846154,
0.169230769230769,0.184615384615385,0.2,0.215384615384615,0.230769230769231,
0.246153846153846,0.261538461538462,0.276923076923077,0.292307692307692,
0.307692307692308,0.323076923076923,0.338461538461538,0.353846153846154,
0.369230769230769,0.384615384615385,0.4,0.415384615384615,0.430769230769231,
0.446153846153846,0.461538461538462,0.476923076923077,0.492307692307692,
0.507692307692308,0.523076923076923,0.538461538461538,0.553846153846154,
0.569230769230769,0.584615384615384,0.6,0.615384615384615,0.63076923076923,
0.646153846153846,0.661538461538461,0.676923076923076,0.692307692307692,
0.707692307692307,0.723076923076922,0.738461538461538,0.753846153846153,
0.769230769230768,0.784615384615384,0.799999999999999,0.815384615384614,
0.83076923076923,0.846153846153845,0.86153846153846,0.876923076923076,0.892307692307691,
0.907692307692306,0.923076923076922,0.938461538461537,0.953846153846152,
0.969230769230768,0.984615384615383,1.),.UNSPECIFIED.)
CURVE()
GEOMETRIC_REPRESENTATION_ITEM()
RATIONAL_B_SPLINE_CURVE((1.,1.,1.,1.,1.,1.,1.,1.,1.,1.,1.,1.,1.,1.,1.,1.,
1.,1.,1.,1.,1.,1.,1.,1.,1.,1.,1.,1.,1.,1.,1.,1.,1.,1.,1.,1.,1.,1.,1.,1.,
1.,1.,1.,1.,1.,1.,1.,1.,1.,1.,1.,1.,1.,1.,1.,1.,1.,1.,1.,1.,1.,1.,1.,1.,
1.,1.,1.,1.,1.,1.))
REPRESENTATION_ITEM('')
);
#344=(
BOUNDED_CURVE()
B_SPLINE_CURVE(5,(#50581,#50582,#50583,#50584,#50585,#50586,#50587,#50588,
#50589,#50590,#50591,#50592,#50593,#50594,#50595,#50596,#50597,#50598,#50599,
#50600,#50601,#50602,#50603,#50604,#50605,#50606,#50607,#50608,#50609,#50610,
#50611,#50612,#50613,#50614,#50615,#50616,#50617,#50618,#50619,#50620,#50621,
#50622,#50623,#50624,#50625,#50626,#50627,#50628,#50629,#50630,#50631,#50632,
#50633,#50634,#50635,#50636,#50637,#50638,#50639,#50640,#50641,#50642,#50643,
#50644,#50645,#50646,#50647,#50648,#50649,#50650),.UNSPECIFIED.,.F.,.F.)
B_SPLINE_CURVE_WITH_KNOTS((6,1,1,1,1,1,1,1,1,1,1,1,1,1,1,1,1,1,1,1,1,1,
1,1,1,1,1,1,1,1,1,1,1,1,1,1,1,1,1,1,1,1,1,1,1,1,1,1,1,1,1,1,1,1,1,1,1,1,
1,1,1,1,1,1,1,6),(0.,0.0153846153846154,0.0307692307692308,0.0461538461538462,
0.0615384615384615,0.0769230769230769,0.0923076923076923,0.107692307692308,
0.123076923076923,0.138461538461538,0.153846153846154,0.169230769230769,
0.184615384615385,0.2,0.215384615384615,0.230769230769231,0.246153846153846,
0.261538461538462,0.276923076923077,0.292307692307692,0.307692307692308,
0.323076923076923,0.338461538461538,0.353846153846154,0.369230769230769,
0.384615384615385,0.4,0.415384615384615,0.430769230769231,0.446153846153846,
0.461538461538462,0.476923076923077,0.492307692307692,0.507692307692308,
0.523076923076923,0.538461538461538,0.553846153846154,0.569230769230769,
0.584615384615384,0.6,0.615384615384615,0.63076923076923,0.646153846153846,
0.661538461538461,0.676923076923076,0.692307692307692,0.707692307692307,
0.723076923076922,0.738461538461538,0.753846153846153,0.769230769230768,
0.784615384615384,0.799999999999999,0.815384615384614,0.83076923076923,
0.846153846153845,0.86153846153846,0.876923076923076,0.892307692307691,
0.907692307692306,0.923076923076922,0.938461538461537,0.953846153846152,
0.969230769230768,0.984615384615383,0.994228156739696),.UNSPECIFIED.)
CURVE()
GEOMETRIC_REPRESENTATION_ITEM()
RATIONAL_B_SPLINE_CURVE((1.,1.,1.,1.,1.,1.,1.,1.,1.,1.,1.,1.,1.,1.,1.,1.,
1.,1.,1.,1.,1.,1.,1.,1.,1.,1.,1.,1.,1.,1.,1.,1.,1.,1.,1.,1.,1.,1.,1.,1.,
1.,1.,1.,1.,1.,1.,1.,1.,1.,1.,1.,1.,1.,1.,1.,1.,1.,1.,1.,1.,1.,1.,1.,1.,
1.,1.,1.,1.,1.,1.))
REPRESENTATION_ITEM('')
);
#345=(
BOUNDED_CURVE()
B_SPLINE_CURVE(5,(#50654,#50655,#50656,#50657,#50658,#50659,#50660,#50661,
#50662,#50663,#50664,#50665,#50666,#50667,#50668,#50669,#50670,#50671,#50672,
#50673,#50674,#50675,#50676,#50677,#50678,#50679,#50680,#50681,#50682,#50683,
#50684,#50685,#50686,#50687,#50688,#50689,#50690,#50691,#50692,#50693,#50694,
#50695,#50696,#50697,#50698,#50699,#50700,#50701,#50702,#50703,#50704,#50705,
#50706,#50707,#50708,#50709,#50710,#50711,#50712,#50713,#50714,#50715,#50716,
#50717,#50718,#50719,#50720,#50721,#50722,#50723),.UNSPECIFIED.,.F.,.F.)
B_SPLINE_CURVE_WITH_KNOTS((6,1,1,1,1,1,1,1,1,1,1,1,1,1,1,1,1,1,1,1,1,1,
1,1,1,1,1,1,1,1,1,1,1,1,1,1,1,1,1,1,1,1,1,1,1,1,1,1,1,1,1,1,1,1,1,1,1,1,
1,1,1,1,1,1,1,6),(0.00577184337452068,0.0153846153846154,0.0307692307692308,
0.0461538461538462,0.0615384615384615,0.0769230769230769,0.0923076923076923,
0.107692307692308,0.123076923076923,0.138461538461538,0.153846153846154,
0.169230769230769,0.184615384615385,0.2,0.215384615384615,0.230769230769231,
0.246153846153846,0.261538461538462,0.276923076923077,0.292307692307692,
0.307692307692308,0.323076923076923,0.338461538461538,0.353846153846154,
0.369230769230769,0.384615384615385,0.4,0.415384615384615,0.430769230769231,
0.446153846153846,0.461538461538462,0.476923076923077,0.492307692307692,
0.507692307692308,0.523076923076923,0.538461538461538,0.553846153846154,
0.569230769230769,0.584615384615384,0.6,0.615384615384615,0.63076923076923,
0.646153846153846,0.661538461538461,0.676923076923076,0.692307692307692,
0.707692307692307,0.723076923076922,0.738461538461538,0.753846153846153,
0.769230769230768,0.784615384615384,0.799999999999999,0.815384615384614,
0.83076923076923,0.846153846153845,0.86153846153846,0.876923076923076,0.892307692307691,
0.907692307692306,0.923076923076922,0.938461538461537,0.953846153846152,
0.969230769230768,0.984615384615383,1.),.UNSPECIFIED.)
CURVE()
GEOMETRIC_REPRESENTATION_ITEM()
RATIONAL_B_SPLINE_CURVE((1.,1.,1.,1.,1.,1.,1.,1.,1.,1.,1.,1.,1.,1.,1.,1.,
1.,1.,1.,1.,1.,1.,1.,1.,1.,1.,1.,1.,1.,1.,1.,1.,1.,1.,1.,1.,1.,1.,1.,1.,
1.,1.,1.,1.,1.,1.,1.,1.,1.,1.,1.,1.,1.,1.,1.,1.,1.,1.,1.,1.,1.,1.,1.,1.,
1.,1.,1.,1.,1.,1.))
REPRESENTATION_ITEM('')
);
#346=(
BOUNDED_CURVE()
B_SPLINE_CURVE(5,(#50727,#50728,#50729,#50730,#50731,#50732,#50733,#50734,
#50735,#50736,#50737,#50738,#50739,#50740,#50741,#50742,#50743,#50744,#50745,
#50746,#50747,#50748,#50749,#50750,#50751,#50752,#50753,#50754,#50755,#50756,
#50757,#50758,#50759,#50760,#50761,#50762,#50763,#50764,#50765,#50766,#50767,
#50768,#50769,#50770,#50771,#50772,#50773,#50774,#50775,#50776,#50777,#50778,
#50779,#50780,#50781,#50782,#50783,#50784,#50785,#50786,#50787,#50788,#50789,
#50790,#50791,#50792,#50793,#50794,#50795,#50796),.UNSPECIFIED.,.F.,.F.)
B_SPLINE_CURVE_WITH_KNOTS((6,1,1,1,1,1,1,1,1,1,1,1,1,1,1,1,1,1,1,1,1,1,
1,1,1,1,1,1,1,1,1,1,1,1,1,1,1,1,1,1,1,1,1,1,1,1,1,1,1,1,1,1,1,1,1,1,1,1,
1,1,1,1,1,1,1,6),(0.,0.0153846153846154,0.0307692307692308,0.0461538461538462,
0.0615384615384615,0.0769230769230769,0.0923076923076923,0.107692307692308,
0.123076923076923,0.138461538461538,0.153846153846154,0.169230769230769,
0.184615384615385,0.2,0.215384615384615,0.230769230769231,0.246153846153846,
0.261538461538462,0.276923076923077,0.292307692307692,0.307692307692308,
0.323076923076923,0.338461538461538,0.353846153846154,0.369230769230769,
0.384615384615385,0.4,0.415384615384615,0.430769230769231,0.446153846153846,
0.461538461538462,0.476923076923077,0.492307692307692,0.507692307692308,
0.523076923076923,0.538461538461538,0.553846153846154,0.569230769230769,
0.584615384615384,0.6,0.615384615384615,0.63076923076923,0.646153846153846,
0.661538461538461,0.676923076923076,0.692307692307692,0.707692307692307,
0.723076923076922,0.738461538461538,0.753846153846153,0.769230769230768,
0.784615384615384,0.799999999999999,0.815384615384614,0.83076923076923,
0.846153846153845,0.86153846153846,0.876923076923076,0.892307692307691,
0.907692307692306,0.923076923076922,0.938461538461537,0.953846153846152,
0.969230769230768,0.984615384615383,0.994228156739698),.UNSPECIFIED.)
CURVE()
GEOMETRIC_REPRESENTATION_ITEM()
RATIONAL_B_SPLINE_CURVE((1.,1.,1.,1.,1.,1.,1.,1.,1.,1.,1.,1.,1.,1.,1.,1.,
1.,1.,1.,1.,1.,1.,1.,1.,1.,1.,1.,1.,1.,1.,1.,1.,1.,1.,1.,1.,1.,1.,1.,1.,
1.,1.,1.,1.,1.,1.,1.,1.,1.,1.,1.,1.,1.,1.,1.,1.,1.,1.,1.,1.,1.,1.,1.,1.,
1.,1.,1.,1.,1.,1.))
REPRESENTATION_ITEM('')
);
#347=(
BOUNDED_CURVE()
B_SPLINE_CURVE(5,(#50800,#50801,#50802,#50803,#50804,#50805,#50806,#50807,
#50808,#50809,#50810,#50811,#50812,#50813,#50814,#50815,#50816,#50817,#50818,
#50819,#50820,#50821,#50822,#50823,#50824,#50825,#50826,#50827,#50828,#50829,
#50830,#50831,#50832,#50833,#50834,#50835,#50836,#50837,#50838,#50839,#50840,
#50841,#50842,#50843,#50844,#50845,#50846,#50847,#50848,#50849,#50850,#50851,
#50852,#50853,#50854,#50855,#50856,#50857,#50858,#50859,#50860,#50861,#50862,
#50863,#50864,#50865,#50866,#50867,#50868,#50869),.UNSPECIFIED.,.F.,.F.)
B_SPLINE_CURVE_WITH_KNOTS((6,1,1,1,1,1,1,1,1,1,1,1,1,1,1,1,1,1,1,1,1,1,
1,1,1,1,1,1,1,1,1,1,1,1,1,1,1,1,1,1,1,1,1,1,1,1,1,1,1,1,1,1,1,1,1,1,1,1,
1,1,1,1,1,1,1,6),(0.00577184337451607,0.0153846153846154,0.0307692307692308,
0.0461538461538462,0.0615384615384615,0.0769230769230769,0.0923076923076923,
0.107692307692308,0.123076923076923,0.138461538461538,0.153846153846154,
0.169230769230769,0.184615384615385,0.2,0.215384615384615,0.230769230769231,
0.246153846153846,0.261538461538462,0.276923076923077,0.292307692307692,
0.307692307692308,0.323076923076923,0.338461538461538,0.353846153846154,
0.369230769230769,0.384615384615385,0.4,0.415384615384615,0.430769230769231,
0.446153846153846,0.461538461538462,0.476923076923077,0.492307692307692,
0.507692307692308,0.523076923076923,0.538461538461538,0.553846153846154,
0.569230769230769,0.584615384615384,0.6,0.615384615384615,0.63076923076923,
0.646153846153846,0.661538461538461,0.676923076923076,0.692307692307692,
0.707692307692307,0.723076923076922,0.738461538461538,0.753846153846153,
0.769230769230768,0.784615384615384,0.799999999999999,0.815384615384614,
0.83076923076923,0.846153846153845,0.86153846153846,0.876923076923076,0.892307692307691,
0.907692307692306,0.923076923076922,0.938461538461537,0.953846153846152,
0.969230769230768,0.984615384615383,1.),.UNSPECIFIED.)
CURVE()
GEOMETRIC_REPRESENTATION_ITEM()
RATIONAL_B_SPLINE_CURVE((1.,1.,1.,1.,1.,1.,1.,1.,1.,1.,1.,1.,1.,1.,1.,1.,
1.,1.,1.,1.,1.,1.,1.,1.,1.,1.,1.,1.,1.,1.,1.,1.,1.,1.,1.,1.,1.,1.,1.,1.,
1.,1.,1.,1.,1.,1.,1.,1.,1.,1.,1.,1.,1.,1.,1.,1.,1.,1.,1.,1.,1.,1.,1.,1.,
1.,1.,1.,1.,1.,1.))
REPRESENTATION_ITEM('')
);
#348=(
BOUNDED_CURVE()
B_SPLINE_CURVE(5,(#50873,#50874,#50875,#50876,#50877,#50878,#50879,#50880,
#50881,#50882,#50883,#50884,#50885,#50886,#50887,#50888,#50889,#50890,#50891,
#50892,#50893,#50894,#50895,#50896,#50897,#50898,#50899,#50900,#50901,#50902,
#50903,#50904,#50905,#50906,#50907,#50908,#50909,#50910,#50911,#50912,#50913,
#50914,#50915,#50916,#50917,#50918,#50919,#50920,#50921,#50922,#50923,#50924,
#50925,#50926,#50927,#50928,#50929,#50930,#50931,#50932,#50933,#50934,#50935,
#50936,#50937,#50938,#50939,#50940,#50941,#50942),.UNSPECIFIED.,.F.,.F.)
B_SPLINE_CURVE_WITH_KNOTS((6,1,1,1,1,1,1,1,1,1,1,1,1,1,1,1,1,1,1,1,1,1,
1,1,1,1,1,1,1,1,1,1,1,1,1,1,1,1,1,1,1,1,1,1,1,1,1,1,1,1,1,1,1,1,1,1,1,1,
1,1,1,1,1,1,1,6),(0.,0.0153846153846154,0.0307692307692308,0.0461538461538462,
0.0615384615384615,0.0769230769230769,0.0923076923076923,0.107692307692308,
0.123076923076923,0.138461538461538,0.153846153846154,0.169230769230769,
0.184615384615385,0.2,0.215384615384615,0.230769230769231,0.246153846153846,
0.261538461538462,0.276923076923077,0.292307692307692,0.307692307692308,
0.323076923076923,0.338461538461538,0.353846153846154,0.369230769230769,
0.384615384615385,0.4,0.415384615384615,0.430769230769231,0.446153846153846,
0.461538461538462,0.476923076923077,0.492307692307692,0.507692307692308,
0.523076923076923,0.538461538461538,0.553846153846154,0.569230769230769,
0.584615384615384,0.6,0.615384615384615,0.63076923076923,0.646153846153846,
0.661538461538461,0.676923076923076,0.692307692307692,0.707692307692307,
0.723076923076922,0.738461538461538,0.753846153846153,0.769230769230768,
0.784615384615384,0.799999999999999,0.815384615384614,0.83076923076923,
0.846153846153845,0.86153846153846,0.876923076923076,0.892307692307691,
0.907692307692306,0.923076923076922,0.938461538461537,0.953846153846152,
0.969230769230768,0.984615384615383,0.994228156739704),.UNSPECIFIED.)
CURVE()
GEOMETRIC_REPRESENTATION_ITEM()
RATIONAL_B_SPLINE_CURVE((1.,1.,1.,1.,1.,1.,1.,1.,1.,1.,1.,1.,1.,1.,1.,1.,
1.,1.,1.,1.,1.,1.,1.,1.,1.,1.,1.,1.,1.,1.,1.,1.,1.,1.,1.,1.,1.,1.,1.,1.,
1.,1.,1.,1.,1.,1.,1.,1.,1.,1.,1.,1.,1.,1.,1.,1.,1.,1.,1.,1.,1.,1.,1.,1.,
1.,1.,1.,1.,1.,1.))
REPRESENTATION_ITEM('')
);
#349=(
BOUNDED_CURVE()
B_SPLINE_CURVE(5,(#50946,#50947,#50948,#50949,#50950,#50951,#50952,#50953,
#50954,#50955,#50956,#50957,#50958,#50959,#50960,#50961,#50962,#50963,#50964,
#50965,#50966,#50967,#50968,#50969,#50970,#50971,#50972,#50973,#50974,#50975,
#50976,#50977,#50978,#50979,#50980,#50981,#50982,#50983,#50984,#50985,#50986,
#50987,#50988,#50989,#50990,#50991,#50992,#50993,#50994,#50995,#50996,#50997,
#50998,#50999,#51000,#51001,#51002,#51003,#51004,#51005,#51006,#51007,#51008,
#51009,#51010,#51011,#51012,#51013,#51014,#51015),.UNSPECIFIED.,.F.,.F.)
B_SPLINE_CURVE_WITH_KNOTS((6,1,1,1,1,1,1,1,1,1,1,1,1,1,1,1,1,1,1,1,1,1,
1,1,1,1,1,1,1,1,1,1,1,1,1,1,1,1,1,1,1,1,1,1,1,1,1,1,1,1,1,1,1,1,1,1,1,1,
1,1,1,1,1,1,1,6),(0.00577184337449692,0.0153846153846154,0.0307692307692308,
0.0461538461538462,0.0615384615384615,0.0769230769230769,0.0923076923076923,
0.107692307692308,0.123076923076923,0.138461538461538,0.153846153846154,
0.169230769230769,0.184615384615385,0.2,0.215384615384615,0.230769230769231,
0.246153846153846,0.261538461538462,0.276923076923077,0.292307692307692,
0.307692307692308,0.323076923076923,0.338461538461538,0.353846153846154,
0.369230769230769,0.384615384615385,0.4,0.415384615384615,0.430769230769231,
0.446153846153846,0.461538461538462,0.476923076923077,0.492307692307692,
0.507692307692308,0.523076923076923,0.538461538461538,0.553846153846154,
0.569230769230769,0.584615384615384,0.6,0.615384615384615,0.63076923076923,
0.646153846153846,0.661538461538461,0.676923076923076,0.692307692307692,
0.707692307692307,0.723076923076922,0.738461538461538,0.753846153846153,
0.769230769230768,0.784615384615384,0.799999999999999,0.815384615384614,
0.83076923076923,0.846153846153845,0.86153846153846,0.876923076923076,0.892307692307691,
0.907692307692306,0.923076923076922,0.938461538461537,0.953846153846152,
0.969230769230768,0.984615384615383,1.),.UNSPECIFIED.)
CURVE()
GEOMETRIC_REPRESENTATION_ITEM()
RATIONAL_B_SPLINE_CURVE((1.,1.,1.,1.,1.,1.,1.,1.,1.,1.,1.,1.,1.,1.,1.,1.,
1.,1.,1.,1.,1.,1.,1.,1.,1.,1.,1.,1.,1.,1.,1.,1.,1.,1.,1.,1.,1.,1.,1.,1.,
1.,1.,1.,1.,1.,1.,1.,1.,1.,1.,1.,1.,1.,1.,1.,1.,1.,1.,1.,1.,1.,1.,1.,1.,
1.,1.,1.,1.,1.,1.))
REPRESENTATION_ITEM('')
);
#350=(
BOUNDED_CURVE()
B_SPLINE_CURVE(5,(#51019,#51020,#51021,#51022,#51023,#51024,#51025,#51026,
#51027,#51028,#51029,#51030,#51031,#51032,#51033,#51034,#51035,#51036,#51037,
#51038,#51039,#51040,#51041,#51042,#51043,#51044,#51045,#51046,#51047,#51048,
#51049,#51050,#51051,#51052,#51053,#51054,#51055,#51056,#51057,#51058,#51059,
#51060,#51061,#51062,#51063,#51064,#51065,#51066,#51067,#51068,#51069,#51070,
#51071,#51072,#51073,#51074,#51075,#51076,#51077,#51078,#51079,#51080,#51081,
#51082,#51083,#51084,#51085,#51086,#51087,#51088),.UNSPECIFIED.,.F.,.F.)
B_SPLINE_CURVE_WITH_KNOTS((6,1,1,1,1,1,1,1,1,1,1,1,1,1,1,1,1,1,1,1,1,1,
1,1,1,1,1,1,1,1,1,1,1,1,1,1,1,1,1,1,1,1,1,1,1,1,1,1,1,1,1,1,1,1,1,1,1,1,
1,1,1,1,1,1,1,6),(0.,0.0153846153846154,0.0307692307692308,0.0461538461538462,
0.0615384615384615,0.0769230769230769,0.0923076923076923,0.107692307692308,
0.123076923076923,0.138461538461538,0.153846153846154,0.169230769230769,
0.184615384615385,0.2,0.215384615384615,0.230769230769231,0.246153846153846,
0.261538461538462,0.276923076923077,0.292307692307692,0.307692307692308,
0.323076923076923,0.338461538461538,0.353846153846154,0.369230769230769,
0.384615384615385,0.4,0.415384615384615,0.430769230769231,0.446153846153846,
0.461538461538462,0.476923076923077,0.492307692307692,0.507692307692308,
0.523076923076923,0.538461538461538,0.553846153846154,0.569230769230769,
0.584615384615384,0.6,0.615384615384615,0.63076923076923,0.646153846153846,
0.661538461538461,0.676923076923076,0.692307692307692,0.707692307692307,
0.723076923076922,0.738461538461538,0.753846153846153,0.769230769230768,
0.784615384615384,0.799999999999999,0.815384615384614,0.83076923076923,
0.846153846153845,0.86153846153846,0.876923076923076,0.892307692307691,
0.907692307692306,0.923076923076922,0.938461538461537,0.953846153846152,
0.969230769230768,0.984615384615383,0.994228156739711),.UNSPECIFIED.)
CURVE()
GEOMETRIC_REPRESENTATION_ITEM()
RATIONAL_B_SPLINE_CURVE((1.,1.,1.,1.,1.,1.,1.,1.,1.,1.,1.,1.,1.,1.,1.,1.,
1.,1.,1.,1.,1.,1.,1.,1.,1.,1.,1.,1.,1.,1.,1.,1.,1.,1.,1.,1.,1.,1.,1.,1.,
1.,1.,1.,1.,1.,1.,1.,1.,1.,1.,1.,1.,1.,1.,1.,1.,1.,1.,1.,1.,1.,1.,1.,1.,
1.,1.,1.,1.,1.,1.))
REPRESENTATION_ITEM('')
);
#351=(
BOUNDED_CURVE()
B_SPLINE_CURVE(5,(#51092,#51093,#51094,#51095,#51096,#51097,#51098,#51099,
#51100,#51101,#51102,#51103,#51104,#51105,#51106,#51107,#51108,#51109,#51110,
#51111,#51112,#51113,#51114,#51115,#51116,#51117,#51118,#51119,#51120,#51121,
#51122,#51123,#51124,#51125,#51126,#51127,#51128,#51129,#51130,#51131,#51132,
#51133,#51134,#51135,#51136,#51137,#51138,#51139,#51140,#51141,#51142,#51143,
#51144,#51145,#51146,#51147,#51148,#51149,#51150,#51151,#51152,#51153,#51154,
#51155,#51156,#51157,#51158,#51159,#51160,#51161),.UNSPECIFIED.,.F.,.F.)
B_SPLINE_CURVE_WITH_KNOTS((6,1,1,1,1,1,1,1,1,1,1,1,1,1,1,1,1,1,1,1,1,1,
1,1,1,1,1,1,1,1,1,1,1,1,1,1,1,1,1,1,1,1,1,1,1,1,1,1,1,1,1,1,1,1,1,1,1,1,
1,1,1,1,1,1,1,6),(0.00577184337450058,0.0153846153846154,0.0307692307692308,
0.0461538461538462,0.0615384615384615,0.0769230769230769,0.0923076923076923,
0.107692307692308,0.123076923076923,0.138461538461538,0.153846153846154,
0.169230769230769,0.184615384615385,0.2,0.215384615384615,0.230769230769231,
0.246153846153846,0.261538461538462,0.276923076923077,0.292307692307692,
0.307692307692308,0.323076923076923,0.338461538461538,0.353846153846154,
0.369230769230769,0.384615384615385,0.4,0.415384615384615,0.430769230769231,
0.446153846153846,0.461538461538462,0.476923076923077,0.492307692307692,
0.507692307692308,0.523076923076923,0.538461538461538,0.553846153846154,
0.569230769230769,0.584615384615384,0.6,0.615384615384615,0.63076923076923,
0.646153846153846,0.661538461538461,0.676923076923076,0.692307692307692,
0.707692307692307,0.723076923076922,0.738461538461538,0.753846153846153,
0.769230769230768,0.784615384615384,0.799999999999999,0.815384615384614,
0.83076923076923,0.846153846153845,0.86153846153846,0.876923076923076,0.892307692307691,
0.907692307692306,0.923076923076922,0.938461538461537,0.953846153846152,
0.969230769230768,0.984615384615383,1.),.UNSPECIFIED.)
CURVE()
GEOMETRIC_REPRESENTATION_ITEM()
RATIONAL_B_SPLINE_CURVE((1.,1.,1.,1.,1.,1.,1.,1.,1.,1.,1.,1.,1.,1.,1.,1.,
1.,1.,1.,1.,1.,1.,1.,1.,1.,1.,1.,1.,1.,1.,1.,1.,1.,1.,1.,1.,1.,1.,1.,1.,
1.,1.,1.,1.,1.,1.,1.,1.,1.,1.,1.,1.,1.,1.,1.,1.,1.,1.,1.,1.,1.,1.,1.,1.,
1.,1.,1.,1.,1.,1.))
REPRESENTATION_ITEM('')
);
#352=(
BOUNDED_CURVE()
B_SPLINE_CURVE(5,(#51165,#51166,#51167,#51168,#51169,#51170,#51171,#51172,
#51173,#51174,#51175,#51176,#51177,#51178,#51179,#51180,#51181,#51182,#51183,
#51184,#51185,#51186,#51187,#51188,#51189,#51190,#51191,#51192,#51193,#51194,
#51195,#51196,#51197,#51198,#51199,#51200,#51201,#51202,#51203,#51204,#51205,
#51206,#51207,#51208,#51209,#51210,#51211,#51212,#51213,#51214,#51215,#51216,
#51217,#51218,#51219,#51220,#51221,#51222,#51223,#51224,#51225,#51226,#51227,
#51228,#51229,#51230,#51231,#51232,#51233,#51234),.UNSPECIFIED.,.F.,.F.)
B_SPLINE_CURVE_WITH_KNOTS((6,1,1,1,1,1,1,1,1,1,1,1,1,1,1,1,1,1,1,1,1,1,
1,1,1,1,1,1,1,1,1,1,1,1,1,1,1,1,1,1,1,1,1,1,1,1,1,1,1,1,1,1,1,1,1,1,1,1,
1,1,1,1,1,1,1,6),(0.,0.0153846153846154,0.0307692307692308,0.0461538461538462,
0.0615384615384615,0.0769230769230769,0.0923076923076923,0.107692307692308,
0.123076923076923,0.138461538461538,0.153846153846154,0.169230769230769,
0.184615384615385,0.2,0.215384615384615,0.230769230769231,0.246153846153846,
0.261538461538462,0.276923076923077,0.292307692307692,0.307692307692308,
0.323076923076923,0.338461538461538,0.353846153846154,0.369230769230769,
0.384615384615385,0.4,0.415384615384615,0.430769230769231,0.446153846153846,
0.461538461538462,0.476923076923077,0.492307692307692,0.507692307692308,
0.523076923076923,0.538461538461538,0.553846153846154,0.569230769230769,
0.584615384615384,0.6,0.615384615384615,0.63076923076923,0.646153846153846,
0.661538461538461,0.676923076923076,0.692307692307692,0.707692307692307,
0.723076923076922,0.738461538461538,0.753846153846153,0.769230769230768,
0.784615384615384,0.799999999999999,0.815384615384614,0.83076923076923,
0.846153846153845,0.86153846153846,0.876923076923076,0.892307692307691,
0.907692307692306,0.923076923076922,0.938461538461537,0.953846153846152,
0.969230769230768,0.984615384615383,0.994228156739701),.UNSPECIFIED.)
CURVE()
GEOMETRIC_REPRESENTATION_ITEM()
RATIONAL_B_SPLINE_CURVE((1.,1.,1.,1.,1.,1.,1.,1.,1.,1.,1.,1.,1.,1.,1.,1.,
1.,1.,1.,1.,1.,1.,1.,1.,1.,1.,1.,1.,1.,1.,1.,1.,1.,1.,1.,1.,1.,1.,1.,1.,
1.,1.,1.,1.,1.,1.,1.,1.,1.,1.,1.,1.,1.,1.,1.,1.,1.,1.,1.,1.,1.,1.,1.,1.,
1.,1.,1.,1.,1.,1.))
REPRESENTATION_ITEM('')
);
#353=(
BOUNDED_CURVE()
B_SPLINE_CURVE(5,(#51238,#51239,#51240,#51241,#51242,#51243,#51244,#51245,
#51246,#51247,#51248,#51249,#51250,#51251,#51252,#51253,#51254,#51255,#51256,
#51257,#51258,#51259,#51260,#51261,#51262,#51263,#51264,#51265,#51266,#51267,
#51268,#51269,#51270,#51271,#51272,#51273,#51274,#51275,#51276,#51277,#51278,
#51279,#51280,#51281,#51282,#51283,#51284,#51285,#51286,#51287,#51288,#51289,
#51290,#51291,#51292,#51293,#51294,#51295,#51296,#51297,#51298,#51299,#51300,
#51301,#51302,#51303,#51304,#51305,#51306,#51307),.UNSPECIFIED.,.F.,.F.)
B_SPLINE_CURVE_WITH_KNOTS((6,1,1,1,1,1,1,1,1,1,1,1,1,1,1,1,1,1,1,1,1,1,
1,1,1,1,1,1,1,1,1,1,1,1,1,1,1,1,1,1,1,1,1,1,1,1,1,1,1,1,1,1,1,1,1,1,1,1,
1,1,1,1,1,1,1,6),(0.0057718433745091,0.0153846153846154,0.0307692307692308,
0.0461538461538462,0.0615384615384615,0.0769230769230769,0.0923076923076923,
0.107692307692308,0.123076923076923,0.138461538461538,0.153846153846154,
0.169230769230769,0.184615384615385,0.2,0.215384615384615,0.230769230769231,
0.246153846153846,0.261538461538462,0.276923076923077,0.292307692307692,
0.307692307692308,0.323076923076923,0.338461538461538,0.353846153846154,
0.369230769230769,0.384615384615385,0.4,0.415384615384615,0.430769230769231,
0.446153846153846,0.461538461538462,0.476923076923077,0.492307692307692,
0.507692307692308,0.523076923076923,0.538461538461538,0.553846153846154,
0.569230769230769,0.584615384615384,0.6,0.615384615384615,0.63076923076923,
0.646153846153846,0.661538461538461,0.676923076923076,0.692307692307692,
0.707692307692307,0.723076923076922,0.738461538461538,0.753846153846153,
0.769230769230768,0.784615384615384,0.799999999999999,0.815384615384614,
0.83076923076923,0.846153846153845,0.86153846153846,0.876923076923076,0.892307692307691,
0.907692307692306,0.923076923076922,0.938461538461537,0.953846153846152,
0.969230769230768,0.984615384615383,1.),.UNSPECIFIED.)
CURVE()
GEOMETRIC_REPRESENTATION_ITEM()
RATIONAL_B_SPLINE_CURVE((1.,1.,1.,1.,1.,1.,1.,1.,1.,1.,1.,1.,1.,1.,1.,1.,
1.,1.,1.,1.,1.,1.,1.,1.,1.,1.,1.,1.,1.,1.,1.,1.,1.,1.,1.,1.,1.,1.,1.,1.,
1.,1.,1.,1.,1.,1.,1.,1.,1.,1.,1.,1.,1.,1.,1.,1.,1.,1.,1.,1.,1.,1.,1.,1.,
1.,1.,1.,1.,1.,1.))
REPRESENTATION_ITEM('')
);
#354=(
BOUNDED_CURVE()
B_SPLINE_CURVE(5,(#51311,#51312,#51313,#51314,#51315,#51316,#51317,#51318,
#51319,#51320,#51321,#51322,#51323,#51324,#51325,#51326,#51327,#51328,#51329,
#51330,#51331,#51332,#51333,#51334,#51335,#51336,#51337,#51338,#51339,#51340,
#51341,#51342,#51343,#51344,#51345,#51346,#51347,#51348,#51349,#51350,#51351,
#51352,#51353,#51354,#51355,#51356,#51357,#51358,#51359,#51360,#51361,#51362,
#51363,#51364,#51365,#51366,#51367,#51368,#51369,#51370,#51371,#51372,#51373,
#51374,#51375,#51376,#51377,#51378,#51379,#51380),.UNSPECIFIED.,.F.,.F.)
B_SPLINE_CURVE_WITH_KNOTS((6,1,1,1,1,1,1,1,1,1,1,1,1,1,1,1,1,1,1,1,1,1,
1,1,1,1,1,1,1,1,1,1,1,1,1,1,1,1,1,1,1,1,1,1,1,1,1,1,1,1,1,1,1,1,1,1,1,1,
1,1,1,1,1,1,1,6),(0.,0.0153846153846154,0.0307692307692308,0.0461538461538462,
0.0615384615384615,0.0769230769230769,0.0923076923076923,0.107692307692308,
0.123076923076923,0.138461538461538,0.153846153846154,0.169230769230769,
0.184615384615385,0.2,0.215384615384615,0.230769230769231,0.246153846153846,
0.261538461538462,0.276923076923077,0.292307692307692,0.307692307692308,
0.323076923076923,0.338461538461538,0.353846153846154,0.369230769230769,
0.384615384615385,0.4,0.415384615384615,0.430769230769231,0.446153846153846,
0.461538461538462,0.476923076923077,0.492307692307692,0.507692307692308,
0.523076923076923,0.538461538461538,0.553846153846154,0.569230769230769,
0.584615384615384,0.6,0.615384615384615,0.63076923076923,0.646153846153846,
0.661538461538461,0.676923076923076,0.692307692307692,0.707692307692307,
0.723076923076922,0.738461538461538,0.753846153846153,0.769230769230768,
0.784615384615384,0.799999999999999,0.815384615384614,0.83076923076923,
0.846153846153845,0.86153846153846,0.876923076923076,0.892307692307691,
0.907692307692306,0.923076923076922,0.938461538461537,0.953846153846152,
0.969230769230768,0.984615384615383,0.994228156739689),.UNSPECIFIED.)
CURVE()
GEOMETRIC_REPRESENTATION_ITEM()
RATIONAL_B_SPLINE_CURVE((1.,1.,1.,1.,1.,1.,1.,1.,1.,1.,1.,1.,1.,1.,1.,1.,
1.,1.,1.,1.,1.,1.,1.,1.,1.,1.,1.,1.,1.,1.,1.,1.,1.,1.,1.,1.,1.,1.,1.,1.,
1.,1.,1.,1.,1.,1.,1.,1.,1.,1.,1.,1.,1.,1.,1.,1.,1.,1.,1.,1.,1.,1.,1.,1.,
1.,1.,1.,1.,1.,1.))
REPRESENTATION_ITEM('')
);
#355=(
BOUNDED_CURVE()
B_SPLINE_CURVE(5,(#51384,#51385,#51386,#51387,#51388,#51389,#51390,#51391,
#51392,#51393,#51394,#51395,#51396,#51397,#51398,#51399,#51400,#51401,#51402,
#51403,#51404,#51405,#51406,#51407,#51408,#51409,#51410,#51411,#51412,#51413,
#51414,#51415,#51416,#51417,#51418,#51419,#51420,#51421,#51422,#51423,#51424,
#51425,#51426,#51427,#51428,#51429,#51430,#51431,#51432,#51433,#51434,#51435,
#51436,#51437,#51438,#51439,#51440,#51441,#51442,#51443,#51444,#51445,#51446,
#51447,#51448,#51449,#51450,#51451,#51452,#51453),.UNSPECIFIED.,.F.,.F.)
B_SPLINE_CURVE_WITH_KNOTS((6,1,1,1,1,1,1,1,1,1,1,1,1,1,1,1,1,1,1,1,1,1,
1,1,1,1,1,1,1,1,1,1,1,1,1,1,1,1,1,1,1,1,1,1,1,1,1,1,1,1,1,1,1,1,1,1,1,1,
1,1,1,1,1,1,1,6),(0.00577184337450777,0.0153846153846154,0.0307692307692308,
0.0461538461538462,0.0615384615384615,0.0769230769230769,0.0923076923076923,
0.107692307692308,0.123076923076923,0.138461538461538,0.153846153846154,
0.169230769230769,0.184615384615385,0.2,0.215384615384615,0.230769230769231,
0.246153846153846,0.261538461538462,0.276923076923077,0.292307692307692,
0.307692307692308,0.323076923076923,0.338461538461538,0.353846153846154,
0.369230769230769,0.384615384615385,0.4,0.415384615384615,0.430769230769231,
0.446153846153846,0.461538461538462,0.476923076923077,0.492307692307692,
0.507692307692308,0.523076923076923,0.538461538461538,0.553846153846154,
0.569230769230769,0.584615384615384,0.6,0.615384615384615,0.63076923076923,
0.646153846153846,0.661538461538461,0.676923076923076,0.692307692307692,
0.707692307692307,0.723076923076922,0.738461538461538,0.753846153846153,
0.769230769230768,0.784615384615384,0.799999999999999,0.815384615384614,
0.83076923076923,0.846153846153845,0.86153846153846,0.876923076923076,0.892307692307691,
0.907692307692306,0.923076923076922,0.938461538461537,0.953846153846152,
0.969230769230768,0.984615384615383,1.),.UNSPECIFIED.)
CURVE()
GEOMETRIC_REPRESENTATION_ITEM()
RATIONAL_B_SPLINE_CURVE((1.,1.,1.,1.,1.,1.,1.,1.,1.,1.,1.,1.,1.,1.,1.,1.,
1.,1.,1.,1.,1.,1.,1.,1.,1.,1.,1.,1.,1.,1.,1.,1.,1.,1.,1.,1.,1.,1.,1.,1.,
1.,1.,1.,1.,1.,1.,1.,1.,1.,1.,1.,1.,1.,1.,1.,1.,1.,1.,1.,1.,1.,1.,1.,1.,
1.,1.,1.,1.,1.,1.))
REPRESENTATION_ITEM('')
);
#356=(
BOUNDED_CURVE()
B_SPLINE_CURVE(5,(#51457,#51458,#51459,#51460,#51461,#51462,#51463,#51464,
#51465,#51466,#51467,#51468,#51469,#51470,#51471,#51472,#51473,#51474,#51475,
#51476,#51477,#51478,#51479,#51480,#51481,#51482,#51483,#51484,#51485,#51486,
#51487,#51488,#51489,#51490,#51491,#51492,#51493,#51494,#51495,#51496,#51497,
#51498,#51499,#51500,#51501,#51502,#51503,#51504,#51505,#51506,#51507,#51508,
#51509,#51510,#51511,#51512,#51513,#51514,#51515,#51516,#51517,#51518,#51519,
#51520,#51521,#51522,#51523,#51524,#51525,#51526),.UNSPECIFIED.,.F.,.F.)
B_SPLINE_CURVE_WITH_KNOTS((6,1,1,1,1,1,1,1,1,1,1,1,1,1,1,1,1,1,1,1,1,1,
1,1,1,1,1,1,1,1,1,1,1,1,1,1,1,1,1,1,1,1,1,1,1,1,1,1,1,1,1,1,1,1,1,1,1,1,
1,1,1,1,1,1,1,6),(0.,0.0153846153846154,0.0307692307692308,0.0461538461538462,
0.0615384615384615,0.0769230769230769,0.0923076923076923,0.107692307692308,
0.123076923076923,0.138461538461538,0.153846153846154,0.169230769230769,
0.184615384615385,0.2,0.215384615384615,0.230769230769231,0.246153846153846,
0.261538461538462,0.276923076923077,0.292307692307692,0.307692307692308,
0.323076923076923,0.338461538461538,0.353846153846154,0.369230769230769,
0.384615384615385,0.4,0.415384615384615,0.430769230769231,0.446153846153846,
0.461538461538462,0.476923076923077,0.492307692307692,0.507692307692308,
0.523076923076923,0.538461538461538,0.553846153846154,0.569230769230769,
0.584615384615384,0.6,0.615384615384615,0.63076923076923,0.646153846153846,
0.661538461538461,0.676923076923076,0.692307692307692,0.707692307692307,
0.723076923076922,0.738461538461538,0.753846153846153,0.769230769230768,
0.784615384615384,0.799999999999999,0.815384615384614,0.83076923076923,
0.846153846153845,0.86153846153846,0.876923076923076,0.892307692307691,
0.907692307692306,0.923076923076922,0.938461538461537,0.953846153846152,
0.969230769230768,0.984615384615383,0.994228156739701),.UNSPECIFIED.)
CURVE()
GEOMETRIC_REPRESENTATION_ITEM()
RATIONAL_B_SPLINE_CURVE((1.,1.,1.,1.,1.,1.,1.,1.,1.,1.,1.,1.,1.,1.,1.,1.,
1.,1.,1.,1.,1.,1.,1.,1.,1.,1.,1.,1.,1.,1.,1.,1.,1.,1.,1.,1.,1.,1.,1.,1.,
1.,1.,1.,1.,1.,1.,1.,1.,1.,1.,1.,1.,1.,1.,1.,1.,1.,1.,1.,1.,1.,1.,1.,1.,
1.,1.,1.,1.,1.,1.))
REPRESENTATION_ITEM('')
);
#357=(
BOUNDED_CURVE()
B_SPLINE_CURVE(5,(#51530,#51531,#51532,#51533,#51534,#51535,#51536,#51537,
#51538,#51539,#51540,#51541,#51542,#51543,#51544,#51545,#51546,#51547,#51548,
#51549,#51550,#51551,#51552,#51553,#51554,#51555,#51556,#51557,#51558,#51559,
#51560,#51561,#51562,#51563,#51564,#51565,#51566,#51567,#51568,#51569,#51570,
#51571,#51572,#51573,#51574,#51575,#51576,#51577,#51578,#51579,#51580,#51581,
#51582,#51583,#51584,#51585,#51586,#51587,#51588,#51589,#51590,#51591,#51592,
#51593,#51594,#51595,#51596,#51597,#51598,#51599),.UNSPECIFIED.,.F.,.F.)
B_SPLINE_CURVE_WITH_KNOTS((6,1,1,1,1,1,1,1,1,1,1,1,1,1,1,1,1,1,1,1,1,1,
1,1,1,1,1,1,1,1,1,1,1,1,1,1,1,1,1,1,1,1,1,1,1,1,1,1,1,1,1,1,1,1,1,1,1,1,
1,1,1,1,1,1,1,6),(0.00577184337450172,0.0153846153846154,0.0307692307692308,
0.0461538461538462,0.0615384615384615,0.0769230769230769,0.0923076923076923,
0.107692307692308,0.123076923076923,0.138461538461538,0.153846153846154,
0.169230769230769,0.184615384615385,0.2,0.215384615384615,0.230769230769231,
0.246153846153846,0.261538461538462,0.276923076923077,0.292307692307692,
0.307692307692308,0.323076923076923,0.338461538461538,0.353846153846154,
0.369230769230769,0.384615384615385,0.4,0.415384615384615,0.430769230769231,
0.446153846153846,0.461538461538462,0.476923076923077,0.492307692307692,
0.507692307692308,0.523076923076923,0.538461538461538,0.553846153846154,
0.569230769230769,0.584615384615384,0.6,0.615384615384615,0.63076923076923,
0.646153846153846,0.661538461538461,0.676923076923076,0.692307692307692,
0.707692307692307,0.723076923076922,0.738461538461538,0.753846153846153,
0.769230769230768,0.784615384615384,0.799999999999999,0.815384615384614,
0.83076923076923,0.846153846153845,0.86153846153846,0.876923076923076,0.892307692307691,
0.907692307692306,0.923076923076922,0.938461538461537,0.953846153846152,
0.969230769230768,0.984615384615383,1.),.UNSPECIFIED.)
CURVE()
GEOMETRIC_REPRESENTATION_ITEM()
RATIONAL_B_SPLINE_CURVE((1.,1.,1.,1.,1.,1.,1.,1.,1.,1.,1.,1.,1.,1.,1.,1.,
1.,1.,1.,1.,1.,1.,1.,1.,1.,1.,1.,1.,1.,1.,1.,1.,1.,1.,1.,1.,1.,1.,1.,1.,
1.,1.,1.,1.,1.,1.,1.,1.,1.,1.,1.,1.,1.,1.,1.,1.,1.,1.,1.,1.,1.,1.,1.,1.,
1.,1.,1.,1.,1.,1.))
REPRESENTATION_ITEM('')
);
#358=(
BOUNDED_CURVE()
B_SPLINE_CURVE(5,(#51603,#51604,#51605,#51606,#51607,#51608,#51609,#51610,
#51611,#51612,#51613,#51614,#51615,#51616,#51617,#51618,#51619,#51620,#51621,
#51622,#51623,#51624,#51625,#51626,#51627,#51628,#51629,#51630,#51631,#51632,
#51633,#51634,#51635,#51636,#51637,#51638,#51639,#51640,#51641,#51642,#51643,
#51644,#51645,#51646,#51647,#51648,#51649,#51650,#51651,#51652,#51653,#51654,
#51655,#51656,#51657,#51658,#51659,#51660,#51661,#51662,#51663,#51664,#51665,
#51666,#51667,#51668,#51669,#51670,#51671,#51672),.UNSPECIFIED.,.F.,.F.)
B_SPLINE_CURVE_WITH_KNOTS((6,1,1,1,1,1,1,1,1,1,1,1,1,1,1,1,1,1,1,1,1,1,
1,1,1,1,1,1,1,1,1,1,1,1,1,1,1,1,1,1,1,1,1,1,1,1,1,1,1,1,1,1,1,1,1,1,1,1,
1,1,1,1,1,1,1,6),(0.,0.0153846153846154,0.0307692307692308,0.0461538461538462,
0.0615384615384615,0.0769230769230769,0.0923076923076923,0.107692307692308,
0.123076923076923,0.138461538461538,0.153846153846154,0.169230769230769,
0.184615384615385,0.2,0.215384615384615,0.230769230769231,0.246153846153846,
0.261538461538462,0.276923076923077,0.292307692307692,0.307692307692308,
0.323076923076923,0.338461538461538,0.353846153846154,0.369230769230769,
0.384615384615385,0.4,0.415384615384615,0.430769230769231,0.446153846153846,
0.461538461538462,0.476923076923077,0.492307692307692,0.507692307692308,
0.523076923076923,0.538461538461538,0.553846153846154,0.569230769230769,
0.584615384615384,0.6,0.615384615384615,0.63076923076923,0.646153846153846,
0.661538461538461,0.676923076923076,0.692307692307692,0.707692307692307,
0.723076923076922,0.738461538461538,0.753846153846153,0.769230769230768,
0.784615384615384,0.799999999999999,0.815384615384614,0.83076923076923,
0.846153846153845,0.86153846153846,0.876923076923076,0.892307692307691,
0.907692307692306,0.923076923076922,0.938461538461537,0.953846153846152,
0.969230769230768,0.984615384615383,0.99422815673971),.UNSPECIFIED.)
CURVE()
GEOMETRIC_REPRESENTATION_ITEM()
RATIONAL_B_SPLINE_CURVE((1.,1.,1.,1.,1.,1.,1.,1.,1.,1.,1.,1.,1.,1.,1.,1.,
1.,1.,1.,1.,1.,1.,1.,1.,1.,1.,1.,1.,1.,1.,1.,1.,1.,1.,1.,1.,1.,1.,1.,1.,
1.,1.,1.,1.,1.,1.,1.,1.,1.,1.,1.,1.,1.,1.,1.,1.,1.,1.,1.,1.,1.,1.,1.,1.,
1.,1.,1.,1.,1.,1.))
REPRESENTATION_ITEM('')
);
#359=(
BOUNDED_CURVE()
B_SPLINE_CURVE(5,(#51676,#51677,#51678,#51679,#51680,#51681,#51682,#51683,
#51684,#51685,#51686,#51687,#51688,#51689,#51690,#51691,#51692,#51693,#51694,
#51695,#51696,#51697,#51698,#51699,#51700,#51701,#51702,#51703,#51704,#51705,
#51706,#51707,#51708,#51709,#51710,#51711,#51712,#51713,#51714,#51715,#51716,
#51717,#51718,#51719,#51720,#51721,#51722,#51723,#51724,#51725,#51726,#51727,
#51728,#51729,#51730,#51731,#51732,#51733,#51734,#51735,#51736,#51737,#51738,
#51739,#51740,#51741,#51742,#51743,#51744,#51745),.UNSPECIFIED.,.F.,.F.)
B_SPLINE_CURVE_WITH_KNOTS((6,1,1,1,1,1,1,1,1,1,1,1,1,1,1,1,1,1,1,1,1,1,
1,1,1,1,1,1,1,1,1,1,1,1,1,1,1,1,1,1,1,1,1,1,1,1,1,1,1,1,1,1,1,1,1,1,1,1,
1,1,1,1,1,1,1,6),(0.00577184337448657,0.0153846153846154,0.0307692307692308,
0.0461538461538462,0.0615384615384615,0.0769230769230769,0.0923076923076923,
0.107692307692308,0.123076923076923,0.138461538461538,0.153846153846154,
0.169230769230769,0.184615384615385,0.2,0.215384615384615,0.230769230769231,
0.246153846153846,0.261538461538462,0.276923076923077,0.292307692307692,
0.307692307692308,0.323076923076923,0.338461538461538,0.353846153846154,
0.369230769230769,0.384615384615385,0.4,0.415384615384615,0.430769230769231,
0.446153846153846,0.461538461538462,0.476923076923077,0.492307692307692,
0.507692307692308,0.523076923076923,0.538461538461538,0.553846153846154,
0.569230769230769,0.584615384615384,0.6,0.615384615384615,0.63076923076923,
0.646153846153846,0.661538461538461,0.676923076923076,0.692307692307692,
0.707692307692307,0.723076923076922,0.738461538461538,0.753846153846153,
0.769230769230768,0.784615384615384,0.799999999999999,0.815384615384614,
0.83076923076923,0.846153846153845,0.86153846153846,0.876923076923076,0.892307692307691,
0.907692307692306,0.923076923076922,0.938461538461537,0.953846153846152,
0.969230769230768,0.984615384615383,1.),.UNSPECIFIED.)
CURVE()
GEOMETRIC_REPRESENTATION_ITEM()
RATIONAL_B_SPLINE_CURVE((1.,1.,1.,1.,1.,1.,1.,1.,1.,1.,1.,1.,1.,1.,1.,1.,
1.,1.,1.,1.,1.,1.,1.,1.,1.,1.,1.,1.,1.,1.,1.,1.,1.,1.,1.,1.,1.,1.,1.,1.,
1.,1.,1.,1.,1.,1.,1.,1.,1.,1.,1.,1.,1.,1.,1.,1.,1.,1.,1.,1.,1.,1.,1.,1.,
1.,1.,1.,1.,1.,1.))
REPRESENTATION_ITEM('')
);
#360=(
BOUNDED_CURVE()
B_SPLINE_CURVE(5,(#51749,#51750,#51751,#51752,#51753,#51754,#51755,#51756,
#51757,#51758,#51759,#51760,#51761,#51762,#51763,#51764,#51765,#51766,#51767,
#51768,#51769,#51770,#51771,#51772,#51773,#51774,#51775,#51776,#51777,#51778,
#51779,#51780,#51781,#51782,#51783,#51784,#51785,#51786,#51787,#51788,#51789,
#51790,#51791,#51792,#51793,#51794,#51795,#51796,#51797,#51798,#51799,#51800,
#51801,#51802,#51803,#51804,#51805,#51806,#51807,#51808,#51809,#51810,#51811,
#51812,#51813,#51814,#51815,#51816,#51817,#51818),.UNSPECIFIED.,.F.,.F.)
B_SPLINE_CURVE_WITH_KNOTS((6,1,1,1,1,1,1,1,1,1,1,1,1,1,1,1,1,1,1,1,1,1,
1,1,1,1,1,1,1,1,1,1,1,1,1,1,1,1,1,1,1,1,1,1,1,1,1,1,1,1,1,1,1,1,1,1,1,1,
1,1,1,1,1,1,1,6),(0.,0.0153846153846154,0.0307692307692308,0.0461538461538462,
0.0615384615384615,0.0769230769230769,0.0923076923076923,0.107692307692308,
0.123076923076923,0.138461538461538,0.153846153846154,0.169230769230769,
0.184615384615385,0.2,0.215384615384615,0.230769230769231,0.246153846153846,
0.261538461538462,0.276923076923077,0.292307692307692,0.307692307692308,
0.323076923076923,0.338461538461538,0.353846153846154,0.369230769230769,
0.384615384615385,0.4,0.415384615384615,0.430769230769231,0.446153846153846,
0.461538461538462,0.476923076923077,0.492307692307692,0.507692307692308,
0.523076923076923,0.538461538461538,0.553846153846154,0.569230769230769,
0.584615384615384,0.6,0.615384615384615,0.63076923076923,0.646153846153846,
0.661538461538461,0.676923076923076,0.692307692307692,0.707692307692307,
0.723076923076922,0.738461538461538,0.753846153846153,0.769230769230768,
0.784615384615384,0.799999999999999,0.815384615384614,0.83076923076923,
0.846153846153845,0.86153846153846,0.876923076923076,0.892307692307691,
0.907692307692306,0.923076923076922,0.938461538461537,0.953846153846152,
0.969230769230768,0.984615384615383,0.994228156739709),.UNSPECIFIED.)
CURVE()
GEOMETRIC_REPRESENTATION_ITEM()
RATIONAL_B_SPLINE_CURVE((1.,1.,1.,1.,1.,1.,1.,1.,1.,1.,1.,1.,1.,1.,1.,1.,
1.,1.,1.,1.,1.,1.,1.,1.,1.,1.,1.,1.,1.,1.,1.,1.,1.,1.,1.,1.,1.,1.,1.,1.,
1.,1.,1.,1.,1.,1.,1.,1.,1.,1.,1.,1.,1.,1.,1.,1.,1.,1.,1.,1.,1.,1.,1.,1.,
1.,1.,1.,1.,1.,1.))
REPRESENTATION_ITEM('')
);
#361=(
BOUNDED_CURVE()
B_SPLINE_CURVE(5,(#51822,#51823,#51824,#51825,#51826,#51827,#51828,#51829,
#51830,#51831,#51832,#51833,#51834,#51835,#51836,#51837,#51838,#51839,#51840,
#51841,#51842,#51843,#51844,#51845,#51846,#51847,#51848,#51849,#51850,#51851,
#51852,#51853,#51854,#51855,#51856,#51857,#51858,#51859,#51860,#51861,#51862,
#51863,#51864,#51865,#51866,#51867,#51868,#51869,#51870,#51871,#51872,#51873,
#51874,#51875,#51876,#51877,#51878,#51879,#51880,#51881,#51882,#51883,#51884,
#51885,#51886,#51887,#51888,#51889,#51890,#51891),.UNSPECIFIED.,.F.,.F.)
B_SPLINE_CURVE_WITH_KNOTS((6,1,1,1,1,1,1,1,1,1,1,1,1,1,1,1,1,1,1,1,1,1,
1,1,1,1,1,1,1,1,1,1,1,1,1,1,1,1,1,1,1,1,1,1,1,1,1,1,1,1,1,1,1,1,1,1,1,1,
1,1,1,1,1,1,1,6),(0.00577184337451094,0.0153846153846154,0.0307692307692308,
0.0461538461538462,0.0615384615384615,0.0769230769230769,0.0923076923076923,
0.107692307692308,0.123076923076923,0.138461538461538,0.153846153846154,
0.169230769230769,0.184615384615385,0.2,0.215384615384615,0.230769230769231,
0.246153846153846,0.261538461538462,0.276923076923077,0.292307692307692,
0.307692307692308,0.323076923076923,0.338461538461538,0.353846153846154,
0.369230769230769,0.384615384615385,0.4,0.415384615384615,0.430769230769231,
0.446153846153846,0.461538461538462,0.476923076923077,0.492307692307692,
0.507692307692308,0.523076923076923,0.538461538461538,0.553846153846154,
0.569230769230769,0.584615384615384,0.6,0.615384615384615,0.63076923076923,
0.646153846153846,0.661538461538461,0.676923076923076,0.692307692307692,
0.707692307692307,0.723076923076922,0.738461538461538,0.753846153846153,
0.769230769230768,0.784615384615384,0.799999999999999,0.815384615384614,
0.83076923076923,0.846153846153845,0.86153846153846,0.876923076923076,0.892307692307691,
0.907692307692306,0.923076923076922,0.938461538461537,0.953846153846152,
0.969230769230768,0.984615384615383,1.),.UNSPECIFIED.)
CURVE()
GEOMETRIC_REPRESENTATION_ITEM()
RATIONAL_B_SPLINE_CURVE((1.,1.,1.,1.,1.,1.,1.,1.,1.,1.,1.,1.,1.,1.,1.,1.,
1.,1.,1.,1.,1.,1.,1.,1.,1.,1.,1.,1.,1.,1.,1.,1.,1.,1.,1.,1.,1.,1.,1.,1.,
1.,1.,1.,1.,1.,1.,1.,1.,1.,1.,1.,1.,1.,1.,1.,1.,1.,1.,1.,1.,1.,1.,1.,1.,
1.,1.,1.,1.,1.,1.))
REPRESENTATION_ITEM('')
);
#362=(
BOUNDED_CURVE()
B_SPLINE_CURVE(5,(#51895,#51896,#51897,#51898,#51899,#51900,#51901,#51902,
#51903,#51904,#51905,#51906,#51907,#51908,#51909,#51910,#51911,#51912,#51913,
#51914,#51915,#51916,#51917,#51918,#51919,#51920,#51921,#51922,#51923,#51924,
#51925,#51926,#51927,#51928,#51929,#51930,#51931,#51932,#51933,#51934,#51935,
#51936,#51937,#51938,#51939,#51940,#51941,#51942,#51943,#51944,#51945,#51946,
#51947,#51948,#51949,#51950,#51951,#51952,#51953,#51954,#51955,#51956,#51957,
#51958,#51959,#51960,#51961,#51962,#51963,#51964),.UNSPECIFIED.,.F.,.F.)
B_SPLINE_CURVE_WITH_KNOTS((6,1,1,1,1,1,1,1,1,1,1,1,1,1,1,1,1,1,1,1,1,1,
1,1,1,1,1,1,1,1,1,1,1,1,1,1,1,1,1,1,1,1,1,1,1,1,1,1,1,1,1,1,1,1,1,1,1,1,
1,1,1,1,1,1,1,6),(0.,0.0153846153846154,0.0307692307692308,0.0461538461538462,
0.0615384615384615,0.0769230769230769,0.0923076923076923,0.107692307692308,
0.123076923076923,0.138461538461538,0.153846153846154,0.169230769230769,
0.184615384615385,0.2,0.215384615384615,0.230769230769231,0.246153846153846,
0.261538461538462,0.276923076923077,0.292307692307692,0.307692307692308,
0.323076923076923,0.338461538461538,0.353846153846154,0.369230769230769,
0.384615384615385,0.4,0.415384615384615,0.430769230769231,0.446153846153846,
0.461538461538462,0.476923076923077,0.492307692307692,0.507692307692308,
0.523076923076923,0.538461538461538,0.553846153846154,0.569230769230769,
0.584615384615384,0.6,0.615384615384615,0.63076923076923,0.646153846153846,
0.661538461538461,0.676923076923076,0.692307692307692,0.707692307692307,
0.723076923076922,0.738461538461538,0.753846153846153,0.769230769230768,
0.784615384615384,0.799999999999999,0.815384615384614,0.83076923076923,
0.846153846153845,0.86153846153846,0.876923076923076,0.892307692307691,
0.907692307692306,0.923076923076922,0.938461538461537,0.953846153846152,
0.969230769230768,0.984615384615383,0.994228156739701),.UNSPECIFIED.)
CURVE()
GEOMETRIC_REPRESENTATION_ITEM()
RATIONAL_B_SPLINE_CURVE((1.,1.,1.,1.,1.,1.,1.,1.,1.,1.,1.,1.,1.,1.,1.,1.,
1.,1.,1.,1.,1.,1.,1.,1.,1.,1.,1.,1.,1.,1.,1.,1.,1.,1.,1.,1.,1.,1.,1.,1.,
1.,1.,1.,1.,1.,1.,1.,1.,1.,1.,1.,1.,1.,1.,1.,1.,1.,1.,1.,1.,1.,1.,1.,1.,
1.,1.,1.,1.,1.,1.))
REPRESENTATION_ITEM('')
);
#363=(
BOUNDED_CURVE()
B_SPLINE_CURVE(5,(#51968,#51969,#51970,#51971,#51972,#51973,#51974,#51975,
#51976,#51977,#51978,#51979,#51980,#51981,#51982,#51983,#51984,#51985,#51986,
#51987,#51988,#51989,#51990,#51991,#51992,#51993,#51994,#51995,#51996,#51997,
#51998,#51999,#52000,#52001,#52002,#52003,#52004,#52005,#52006,#52007,#52008,
#52009,#52010,#52011,#52012,#52013,#52014,#52015,#52016,#52017,#52018,#52019,
#52020,#52021,#52022,#52023,#52024,#52025,#52026,#52027,#52028,#52029,#52030,
#52031,#52032,#52033,#52034,#52035,#52036,#52037),.UNSPECIFIED.,.F.,.F.)
B_SPLINE_CURVE_WITH_KNOTS((6,1,1,1,1,1,1,1,1,1,1,1,1,1,1,1,1,1,1,1,1,1,
1,1,1,1,1,1,1,1,1,1,1,1,1,1,1,1,1,1,1,1,1,1,1,1,1,1,1,1,1,1,1,1,1,1,1,1,
1,1,1,1,1,1,1,6),(0.0057718433745102,0.0153846153846154,0.0307692307692308,
0.0461538461538462,0.0615384615384615,0.0769230769230769,0.0923076923076923,
0.107692307692308,0.123076923076923,0.138461538461538,0.153846153846154,
0.169230769230769,0.184615384615385,0.2,0.215384615384615,0.230769230769231,
0.246153846153846,0.261538461538462,0.276923076923077,0.292307692307692,
0.307692307692308,0.323076923076923,0.338461538461538,0.353846153846154,
0.369230769230769,0.384615384615385,0.4,0.415384615384615,0.430769230769231,
0.446153846153846,0.461538461538462,0.476923076923077,0.492307692307692,
0.507692307692308,0.523076923076923,0.538461538461538,0.553846153846154,
0.569230769230769,0.584615384615384,0.6,0.615384615384615,0.63076923076923,
0.646153846153846,0.661538461538461,0.676923076923076,0.692307692307692,
0.707692307692307,0.723076923076922,0.738461538461538,0.753846153846153,
0.769230769230768,0.784615384615384,0.799999999999999,0.815384615384614,
0.83076923076923,0.846153846153845,0.86153846153846,0.876923076923076,0.892307692307691,
0.907692307692306,0.923076923076922,0.938461538461537,0.953846153846152,
0.969230769230768,0.984615384615383,1.),.UNSPECIFIED.)
CURVE()
GEOMETRIC_REPRESENTATION_ITEM()
RATIONAL_B_SPLINE_CURVE((1.,1.,1.,1.,1.,1.,1.,1.,1.,1.,1.,1.,1.,1.,1.,1.,
1.,1.,1.,1.,1.,1.,1.,1.,1.,1.,1.,1.,1.,1.,1.,1.,1.,1.,1.,1.,1.,1.,1.,1.,
1.,1.,1.,1.,1.,1.,1.,1.,1.,1.,1.,1.,1.,1.,1.,1.,1.,1.,1.,1.,1.,1.,1.,1.,
1.,1.,1.,1.,1.,1.))
REPRESENTATION_ITEM('')
);
#364=(
BOUNDED_CURVE()
B_SPLINE_CURVE(5,(#52041,#52042,#52043,#52044,#52045,#52046,#52047,#52048,
#52049,#52050,#52051,#52052,#52053,#52054,#52055,#52056,#52057,#52058,#52059,
#52060,#52061,#52062,#52063,#52064,#52065,#52066,#52067,#52068,#52069,#52070,
#52071,#52072,#52073,#52074,#52075,#52076,#52077,#52078,#52079,#52080,#52081,
#52082,#52083,#52084,#52085,#52086,#52087,#52088,#52089,#52090,#52091,#52092,
#52093,#52094,#52095,#52096,#52097,#52098,#52099,#52100,#52101,#52102,#52103,
#52104,#52105,#52106,#52107,#52108,#52109,#52110),.UNSPECIFIED.,.F.,.F.)
B_SPLINE_CURVE_WITH_KNOTS((6,1,1,1,1,1,1,1,1,1,1,1,1,1,1,1,1,1,1,1,1,1,
1,1,1,1,1,1,1,1,1,1,1,1,1,1,1,1,1,1,1,1,1,1,1,1,1,1,1,1,1,1,1,1,1,1,1,1,
1,1,1,1,1,1,1,6),(0.,0.0153846153846154,0.0307692307692308,0.0461538461538462,
0.0615384615384615,0.0769230769230769,0.0923076923076923,0.107692307692308,
0.123076923076923,0.138461538461538,0.153846153846154,0.169230769230769,
0.184615384615385,0.2,0.215384615384615,0.230769230769231,0.246153846153846,
0.261538461538462,0.276923076923077,0.292307692307692,0.307692307692308,
0.323076923076923,0.338461538461538,0.353846153846154,0.369230769230769,
0.384615384615385,0.4,0.415384615384615,0.430769230769231,0.446153846153846,
0.461538461538462,0.476923076923077,0.492307692307692,0.507692307692308,
0.523076923076923,0.538461538461538,0.553846153846154,0.569230769230769,
0.584615384615384,0.6,0.615384615384615,0.63076923076923,0.646153846153846,
0.661538461538461,0.676923076923076,0.692307692307692,0.707692307692307,
0.723076923076922,0.738461538461538,0.753846153846153,0.769230769230768,
0.784615384615384,0.799999999999999,0.815384615384614,0.83076923076923,
0.846153846153845,0.86153846153846,0.876923076923076,0.892307692307691,
0.907692307692306,0.923076923076922,0.938461538461537,0.953846153846152,
0.969230769230768,0.984615384615383,0.994228156739694),.UNSPECIFIED.)
CURVE()
GEOMETRIC_REPRESENTATION_ITEM()
RATIONAL_B_SPLINE_CURVE((1.,1.,1.,1.,1.,1.,1.,1.,1.,1.,1.,1.,1.,1.,1.,1.,
1.,1.,1.,1.,1.,1.,1.,1.,1.,1.,1.,1.,1.,1.,1.,1.,1.,1.,1.,1.,1.,1.,1.,1.,
1.,1.,1.,1.,1.,1.,1.,1.,1.,1.,1.,1.,1.,1.,1.,1.,1.,1.,1.,1.,1.,1.,1.,1.,
1.,1.,1.,1.,1.,1.))
REPRESENTATION_ITEM('')
);
#365=(
BOUNDED_CURVE()
B_SPLINE_CURVE(5,(#52114,#52115,#52116,#52117,#52118,#52119,#52120,#52121,
#52122,#52123,#52124,#52125,#52126,#52127,#52128,#52129,#52130,#52131,#52132,
#52133,#52134,#52135,#52136,#52137,#52138,#52139,#52140,#52141,#52142,#52143,
#52144,#52145,#52146,#52147,#52148,#52149,#52150,#52151,#52152,#52153,#52154,
#52155,#52156,#52157,#52158,#52159,#52160,#52161,#52162,#52163,#52164,#52165,
#52166,#52167,#52168,#52169,#52170,#52171,#52172,#52173,#52174,#52175,#52176,
#52177,#52178,#52179,#52180,#52181,#52182,#52183),.UNSPECIFIED.,.F.,.F.)
B_SPLINE_CURVE_WITH_KNOTS((6,1,1,1,1,1,1,1,1,1,1,1,1,1,1,1,1,1,1,1,1,1,
1,1,1,1,1,1,1,1,1,1,1,1,1,1,1,1,1,1,1,1,1,1,1,1,1,1,1,1,1,1,1,1,1,1,1,1,
1,1,1,1,1,1,1,6),(0.00577184337452044,0.0153846153846154,0.0307692307692308,
0.0461538461538462,0.0615384615384615,0.0769230769230769,0.0923076923076923,
0.107692307692308,0.123076923076923,0.138461538461538,0.153846153846154,
0.169230769230769,0.184615384615385,0.2,0.215384615384615,0.230769230769231,
0.246153846153846,0.261538461538462,0.276923076923077,0.292307692307692,
0.307692307692308,0.323076923076923,0.338461538461538,0.353846153846154,
0.369230769230769,0.384615384615385,0.4,0.415384615384615,0.430769230769231,
0.446153846153846,0.461538461538462,0.476923076923077,0.492307692307692,
0.507692307692308,0.523076923076923,0.538461538461538,0.553846153846154,
0.569230769230769,0.584615384615384,0.6,0.615384615384615,0.63076923076923,
0.646153846153846,0.661538461538461,0.676923076923076,0.692307692307692,
0.707692307692307,0.723076923076922,0.738461538461538,0.753846153846153,
0.769230769230768,0.784615384615384,0.799999999999999,0.815384615384614,
0.83076923076923,0.846153846153845,0.86153846153846,0.876923076923076,0.892307692307691,
0.907692307692306,0.923076923076922,0.938461538461537,0.953846153846152,
0.969230769230768,0.984615384615383,1.),.UNSPECIFIED.)
CURVE()
GEOMETRIC_REPRESENTATION_ITEM()
RATIONAL_B_SPLINE_CURVE((1.,1.,1.,1.,1.,1.,1.,1.,1.,1.,1.,1.,1.,1.,1.,1.,
1.,1.,1.,1.,1.,1.,1.,1.,1.,1.,1.,1.,1.,1.,1.,1.,1.,1.,1.,1.,1.,1.,1.,1.,
1.,1.,1.,1.,1.,1.,1.,1.,1.,1.,1.,1.,1.,1.,1.,1.,1.,1.,1.,1.,1.,1.,1.,1.,
1.,1.,1.,1.,1.,1.))
REPRESENTATION_ITEM('')
);
#366=(
BOUNDED_CURVE()
B_SPLINE_CURVE(5,(#52187,#52188,#52189,#52190,#52191,#52192,#52193,#52194,
#52195,#52196,#52197,#52198,#52199,#52200,#52201,#52202,#52203,#52204,#52205,
#52206,#52207,#52208,#52209,#52210,#52211,#52212,#52213,#52214,#52215,#52216,
#52217,#52218,#52219,#52220,#52221,#52222,#52223,#52224,#52225,#52226,#52227,
#52228,#52229,#52230,#52231,#52232,#52233,#52234,#52235,#52236,#52237,#52238,
#52239,#52240,#52241,#52242,#52243,#52244,#52245,#52246,#52247,#52248,#52249,
#52250,#52251,#52252,#52253,#52254,#52255,#52256),.UNSPECIFIED.,.F.,.F.)
B_SPLINE_CURVE_WITH_KNOTS((6,1,1,1,1,1,1,1,1,1,1,1,1,1,1,1,1,1,1,1,1,1,
1,1,1,1,1,1,1,1,1,1,1,1,1,1,1,1,1,1,1,1,1,1,1,1,1,1,1,1,1,1,1,1,1,1,1,1,
1,1,1,1,1,1,1,6),(0.,0.0153846153846154,0.0307692307692308,0.0461538461538462,
0.0615384615384615,0.0769230769230769,0.0923076923076923,0.107692307692308,
0.123076923076923,0.138461538461538,0.153846153846154,0.169230769230769,
0.184615384615385,0.2,0.215384615384615,0.230769230769231,0.246153846153846,
0.261538461538462,0.276923076923077,0.292307692307692,0.307692307692308,
0.323076923076923,0.338461538461538,0.353846153846154,0.369230769230769,
0.384615384615385,0.4,0.415384615384615,0.430769230769231,0.446153846153846,
0.461538461538462,0.476923076923077,0.492307692307692,0.507692307692308,
0.523076923076923,0.538461538461538,0.553846153846154,0.569230769230769,
0.584615384615384,0.6,0.615384615384615,0.63076923076923,0.646153846153846,
0.661538461538461,0.676923076923076,0.692307692307692,0.707692307692307,
0.723076923076922,0.738461538461538,0.753846153846153,0.769230769230768,
0.784615384615384,0.799999999999999,0.815384615384614,0.83076923076923,
0.846153846153845,0.86153846153846,0.876923076923076,0.892307692307691,
0.907692307692306,0.923076923076922,0.938461538461537,0.953846153846152,
0.969230769230768,0.984615384615383,0.994228156739698),.UNSPECIFIED.)
CURVE()
GEOMETRIC_REPRESENTATION_ITEM()
RATIONAL_B_SPLINE_CURVE((1.,1.,1.,1.,1.,1.,1.,1.,1.,1.,1.,1.,1.,1.,1.,1.,
1.,1.,1.,1.,1.,1.,1.,1.,1.,1.,1.,1.,1.,1.,1.,1.,1.,1.,1.,1.,1.,1.,1.,1.,
1.,1.,1.,1.,1.,1.,1.,1.,1.,1.,1.,1.,1.,1.,1.,1.,1.,1.,1.,1.,1.,1.,1.,1.,
1.,1.,1.,1.,1.,1.))
REPRESENTATION_ITEM('')
);
#367=(
BOUNDED_CURVE()
B_SPLINE_CURVE(5,(#52260,#52261,#52262,#52263,#52264,#52265,#52266,#52267,
#52268,#52269,#52270,#52271,#52272,#52273,#52274,#52275,#52276,#52277,#52278,
#52279,#52280,#52281,#52282,#52283,#52284,#52285,#52286,#52287,#52288,#52289,
#52290,#52291,#52292,#52293,#52294,#52295,#52296,#52297,#52298,#52299,#52300,
#52301,#52302,#52303,#52304,#52305,#52306,#52307,#52308,#52309,#52310,#52311,
#52312,#52313,#52314,#52315,#52316,#52317,#52318,#52319,#52320,#52321,#52322,
#52323,#52324,#52325,#52326,#52327,#52328,#52329),.UNSPECIFIED.,.F.,.F.)
B_SPLINE_CURVE_WITH_KNOTS((6,1,1,1,1,1,1,1,1,1,1,1,1,1,1,1,1,1,1,1,1,1,
1,1,1,1,1,1,1,1,1,1,1,1,1,1,1,1,1,1,1,1,1,1,1,1,1,1,1,1,1,1,1,1,1,1,1,1,
1,1,1,1,1,1,1,6),(0.00577184337451607,0.0153846153846154,0.0307692307692308,
0.0461538461538462,0.0615384615384615,0.0769230769230769,0.0923076923076923,
0.107692307692308,0.123076923076923,0.138461538461538,0.153846153846154,
0.169230769230769,0.184615384615385,0.2,0.215384615384615,0.230769230769231,
0.246153846153846,0.261538461538462,0.276923076923077,0.292307692307692,
0.307692307692308,0.323076923076923,0.338461538461538,0.353846153846154,
0.369230769230769,0.384615384615385,0.4,0.415384615384615,0.430769230769231,
0.446153846153846,0.461538461538462,0.476923076923077,0.492307692307692,
0.507692307692308,0.523076923076923,0.538461538461538,0.553846153846154,
0.569230769230769,0.584615384615384,0.6,0.615384615384615,0.63076923076923,
0.646153846153846,0.661538461538461,0.676923076923076,0.692307692307692,
0.707692307692307,0.723076923076922,0.738461538461538,0.753846153846153,
0.769230769230768,0.784615384615384,0.799999999999999,0.815384615384614,
0.83076923076923,0.846153846153845,0.86153846153846,0.876923076923076,0.892307692307691,
0.907692307692306,0.923076923076922,0.938461538461537,0.953846153846152,
0.969230769230768,0.984615384615383,1.),.UNSPECIFIED.)
CURVE()
GEOMETRIC_REPRESENTATION_ITEM()
RATIONAL_B_SPLINE_CURVE((1.,1.,1.,1.,1.,1.,1.,1.,1.,1.,1.,1.,1.,1.,1.,1.,
1.,1.,1.,1.,1.,1.,1.,1.,1.,1.,1.,1.,1.,1.,1.,1.,1.,1.,1.,1.,1.,1.,1.,1.,
1.,1.,1.,1.,1.,1.,1.,1.,1.,1.,1.,1.,1.,1.,1.,1.,1.,1.,1.,1.,1.,1.,1.,1.,
1.,1.,1.,1.,1.,1.))
REPRESENTATION_ITEM('')
);
#368=(
BOUNDED_CURVE()
B_SPLINE_CURVE(5,(#52333,#52334,#52335,#52336,#52337,#52338,#52339,#52340,
#52341,#52342,#52343,#52344,#52345,#52346,#52347,#52348,#52349,#52350,#52351,
#52352,#52353,#52354,#52355,#52356,#52357,#52358,#52359,#52360,#52361,#52362,
#52363,#52364,#52365,#52366,#52367,#52368,#52369,#52370,#52371,#52372,#52373,
#52374,#52375,#52376,#52377,#52378,#52379,#52380,#52381,#52382,#52383,#52384,
#52385,#52386,#52387,#52388,#52389,#52390,#52391,#52392,#52393,#52394,#52395,
#52396,#52397,#52398,#52399,#52400,#52401,#52402),.UNSPECIFIED.,.F.,.F.)
B_SPLINE_CURVE_WITH_KNOTS((6,1,1,1,1,1,1,1,1,1,1,1,1,1,1,1,1,1,1,1,1,1,
1,1,1,1,1,1,1,1,1,1,1,1,1,1,1,1,1,1,1,1,1,1,1,1,1,1,1,1,1,1,1,1,1,1,1,1,
1,1,1,1,1,1,1,6),(0.,0.0153846153846154,0.0307692307692308,0.0461538461538462,
0.0615384615384615,0.0769230769230769,0.0923076923076923,0.107692307692308,
0.123076923076923,0.138461538461538,0.153846153846154,0.169230769230769,
0.184615384615385,0.2,0.215384615384615,0.230769230769231,0.246153846153846,
0.261538461538462,0.276923076923077,0.292307692307692,0.307692307692308,
0.323076923076923,0.338461538461538,0.353846153846154,0.369230769230769,
0.384615384615385,0.4,0.415384615384615,0.430769230769231,0.446153846153846,
0.461538461538462,0.476923076923077,0.492307692307692,0.507692307692308,
0.523076923076923,0.538461538461538,0.553846153846154,0.569230769230769,
0.584615384615384,0.6,0.615384615384615,0.63076923076923,0.646153846153846,
0.661538461538461,0.676923076923076,0.692307692307692,0.707692307692307,
0.723076923076922,0.738461538461538,0.753846153846153,0.769230769230768,
0.784615384615384,0.799999999999999,0.815384615384614,0.83076923076923,
0.846153846153845,0.86153846153846,0.876923076923076,0.892307692307691,
0.907692307692306,0.923076923076922,0.938461538461537,0.953846153846152,
0.969230769230768,0.984615384615383,0.994228156739704),.UNSPECIFIED.)
CURVE()
GEOMETRIC_REPRESENTATION_ITEM()
RATIONAL_B_SPLINE_CURVE((1.,1.,1.,1.,1.,1.,1.,1.,1.,1.,1.,1.,1.,1.,1.,1.,
1.,1.,1.,1.,1.,1.,1.,1.,1.,1.,1.,1.,1.,1.,1.,1.,1.,1.,1.,1.,1.,1.,1.,1.,
1.,1.,1.,1.,1.,1.,1.,1.,1.,1.,1.,1.,1.,1.,1.,1.,1.,1.,1.,1.,1.,1.,1.,1.,
1.,1.,1.,1.,1.,1.))
REPRESENTATION_ITEM('')
);
#369=(
BOUNDED_CURVE()
B_SPLINE_CURVE(5,(#52406,#52407,#52408,#52409,#52410,#52411,#52412,#52413,
#52414,#52415,#52416,#52417,#52418,#52419,#52420,#52421,#52422,#52423,#52424,
#52425,#52426,#52427,#52428,#52429,#52430,#52431,#52432,#52433,#52434,#52435,
#52436,#52437,#52438,#52439,#52440,#52441,#52442,#52443,#52444,#52445,#52446,
#52447,#52448,#52449,#52450,#52451,#52452,#52453,#52454,#52455,#52456,#52457,
#52458,#52459,#52460,#52461,#52462,#52463,#52464,#52465,#52466,#52467,#52468,
#52469,#52470,#52471,#52472,#52473,#52474,#52475),.UNSPECIFIED.,.F.,.F.)
B_SPLINE_CURVE_WITH_KNOTS((6,1,1,1,1,1,1,1,1,1,1,1,1,1,1,1,1,1,1,1,1,1,
1,1,1,1,1,1,1,1,1,1,1,1,1,1,1,1,1,1,1,1,1,1,1,1,1,1,1,1,1,1,1,1,1,1,1,1,
1,1,1,1,1,1,1,6),(0.00577184337449682,0.0153846153846154,0.0307692307692308,
0.0461538461538462,0.0615384615384615,0.0769230769230769,0.0923076923076923,
0.107692307692308,0.123076923076923,0.138461538461538,0.153846153846154,
0.169230769230769,0.184615384615385,0.2,0.215384615384615,0.230769230769231,
0.246153846153846,0.261538461538462,0.276923076923077,0.292307692307692,
0.307692307692308,0.323076923076923,0.338461538461538,0.353846153846154,
0.369230769230769,0.384615384615385,0.4,0.415384615384615,0.430769230769231,
0.446153846153846,0.461538461538462,0.476923076923077,0.492307692307692,
0.507692307692308,0.523076923076923,0.538461538461538,0.553846153846154,
0.569230769230769,0.584615384615384,0.6,0.615384615384615,0.63076923076923,
0.646153846153846,0.661538461538461,0.676923076923076,0.692307692307692,
0.707692307692307,0.723076923076922,0.738461538461538,0.753846153846153,
0.769230769230768,0.784615384615384,0.799999999999999,0.815384615384614,
0.83076923076923,0.846153846153845,0.86153846153846,0.876923076923076,0.892307692307691,
0.907692307692306,0.923076923076922,0.938461538461537,0.953846153846152,
0.969230769230768,0.984615384615383,1.),.UNSPECIFIED.)
CURVE()
GEOMETRIC_REPRESENTATION_ITEM()
RATIONAL_B_SPLINE_CURVE((1.,1.,1.,1.,1.,1.,1.,1.,1.,1.,1.,1.,1.,1.,1.,1.,
1.,1.,1.,1.,1.,1.,1.,1.,1.,1.,1.,1.,1.,1.,1.,1.,1.,1.,1.,1.,1.,1.,1.,1.,
1.,1.,1.,1.,1.,1.,1.,1.,1.,1.,1.,1.,1.,1.,1.,1.,1.,1.,1.,1.,1.,1.,1.,1.,
1.,1.,1.,1.,1.,1.))
REPRESENTATION_ITEM('')
);
#370=(
BOUNDED_CURVE()
B_SPLINE_CURVE(5,(#52479,#52480,#52481,#52482,#52483,#52484,#52485,#52486,
#52487,#52488,#52489,#52490,#52491,#52492,#52493,#52494,#52495,#52496,#52497,
#52498,#52499,#52500,#52501,#52502,#52503,#52504,#52505,#52506,#52507,#52508,
#52509,#52510,#52511,#52512,#52513,#52514,#52515,#52516,#52517,#52518,#52519,
#52520,#52521,#52522,#52523,#52524,#52525,#52526,#52527,#52528,#52529,#52530,
#52531,#52532,#52533,#52534,#52535,#52536,#52537,#52538,#52539,#52540,#52541,
#52542,#52543,#52544,#52545,#52546,#52547,#52548),.UNSPECIFIED.,.F.,.F.)
B_SPLINE_CURVE_WITH_KNOTS((6,1,1,1,1,1,1,1,1,1,1,1,1,1,1,1,1,1,1,1,1,1,
1,1,1,1,1,1,1,1,1,1,1,1,1,1,1,1,1,1,1,1,1,1,1,1,1,1,1,1,1,1,1,1,1,1,1,1,
1,1,1,1,1,1,1,6),(0.,0.0153846153846154,0.0307692307692308,0.0461538461538462,
0.0615384615384615,0.0769230769230769,0.0923076923076923,0.107692307692308,
0.123076923076923,0.138461538461538,0.153846153846154,0.169230769230769,
0.184615384615385,0.2,0.215384615384615,0.230769230769231,0.246153846153846,
0.261538461538462,0.276923076923077,0.292307692307692,0.307692307692308,
0.323076923076923,0.338461538461538,0.353846153846154,0.369230769230769,
0.384615384615385,0.4,0.415384615384615,0.430769230769231,0.446153846153846,
0.461538461538462,0.476923076923077,0.492307692307692,0.507692307692308,
0.523076923076923,0.538461538461538,0.553846153846154,0.569230769230769,
0.584615384615384,0.6,0.615384615384615,0.63076923076923,0.646153846153846,
0.661538461538461,0.676923076923076,0.692307692307692,0.707692307692307,
0.723076923076922,0.738461538461538,0.753846153846153,0.769230769230768,
0.784615384615384,0.799999999999999,0.815384615384614,0.83076923076923,
0.846153846153845,0.86153846153846,0.876923076923076,0.892307692307691,
0.907692307692306,0.923076923076922,0.938461538461537,0.953846153846152,
0.969230769230768,0.984615384615383,0.994228156739711),.UNSPECIFIED.)
CURVE()
GEOMETRIC_REPRESENTATION_ITEM()
RATIONAL_B_SPLINE_CURVE((1.,1.,1.,1.,1.,1.,1.,1.,1.,1.,1.,1.,1.,1.,1.,1.,
1.,1.,1.,1.,1.,1.,1.,1.,1.,1.,1.,1.,1.,1.,1.,1.,1.,1.,1.,1.,1.,1.,1.,1.,
1.,1.,1.,1.,1.,1.,1.,1.,1.,1.,1.,1.,1.,1.,1.,1.,1.,1.,1.,1.,1.,1.,1.,1.,
1.,1.,1.,1.,1.,1.))
REPRESENTATION_ITEM('')
);
#371=(
BOUNDED_CURVE()
B_SPLINE_CURVE(5,(#52552,#52553,#52554,#52555,#52556,#52557,#52558,#52559,
#52560,#52561,#52562,#52563,#52564,#52565,#52566,#52567,#52568,#52569,#52570,
#52571,#52572,#52573,#52574,#52575,#52576,#52577,#52578,#52579,#52580,#52581,
#52582,#52583,#52584,#52585,#52586,#52587,#52588,#52589,#52590,#52591,#52592,
#52593,#52594,#52595,#52596,#52597,#52598,#52599,#52600,#52601,#52602,#52603,
#52604,#52605,#52606,#52607,#52608,#52609,#52610,#52611,#52612,#52613,#52614,
#52615,#52616,#52617,#52618,#52619,#52620,#52621),.UNSPECIFIED.,.F.,.F.)
B_SPLINE_CURVE_WITH_KNOTS((6,1,1,1,1,1,1,1,1,1,1,1,1,1,1,1,1,1,1,1,1,1,
1,1,1,1,1,1,1,1,1,1,1,1,1,1,1,1,1,1,1,1,1,1,1,1,1,1,1,1,1,1,1,1,1,1,1,1,
1,1,1,1,1,1,1,6),(0.00577184337450313,0.0153846153846154,0.0307692307692308,
0.0461538461538462,0.0615384615384615,0.0769230769230769,0.0923076923076923,
0.107692307692308,0.123076923076923,0.138461538461538,0.153846153846154,
0.169230769230769,0.184615384615385,0.2,0.215384615384615,0.230769230769231,
0.246153846153846,0.261538461538462,0.276923076923077,0.292307692307692,
0.307692307692308,0.323076923076923,0.338461538461538,0.353846153846154,
0.369230769230769,0.384615384615385,0.4,0.415384615384615,0.430769230769231,
0.446153846153846,0.461538461538462,0.476923076923077,0.492307692307692,
0.507692307692308,0.523076923076923,0.538461538461538,0.553846153846154,
0.569230769230769,0.584615384615384,0.6,0.615384615384615,0.63076923076923,
0.646153846153846,0.661538461538461,0.676923076923076,0.692307692307692,
0.707692307692307,0.723076923076922,0.738461538461538,0.753846153846153,
0.769230769230768,0.784615384615384,0.799999999999999,0.815384615384614,
0.83076923076923,0.846153846153845,0.86153846153846,0.876923076923076,0.892307692307691,
0.907692307692306,0.923076923076922,0.938461538461537,0.953846153846152,
0.969230769230768,0.984615384615383,1.),.UNSPECIFIED.)
CURVE()
GEOMETRIC_REPRESENTATION_ITEM()
RATIONAL_B_SPLINE_CURVE((1.,1.,1.,1.,1.,1.,1.,1.,1.,1.,1.,1.,1.,1.,1.,1.,
1.,1.,1.,1.,1.,1.,1.,1.,1.,1.,1.,1.,1.,1.,1.,1.,1.,1.,1.,1.,1.,1.,1.,1.,
1.,1.,1.,1.,1.,1.,1.,1.,1.,1.,1.,1.,1.,1.,1.,1.,1.,1.,1.,1.,1.,1.,1.,1.,
1.,1.,1.,1.,1.,1.))
REPRESENTATION_ITEM('')
);
#372=(
BOUNDED_CURVE()
B_SPLINE_CURVE(5,(#52625,#52626,#52627,#52628,#52629,#52630,#52631,#52632,
#52633,#52634,#52635,#52636,#52637,#52638,#52639,#52640,#52641,#52642,#52643,
#52644,#52645,#52646,#52647,#52648,#52649,#52650,#52651,#52652,#52653,#52654,
#52655,#52656,#52657,#52658,#52659,#52660,#52661,#52662,#52663,#52664,#52665,
#52666,#52667,#52668,#52669,#52670,#52671,#52672,#52673,#52674,#52675,#52676,
#52677,#52678,#52679,#52680,#52681,#52682,#52683,#52684,#52685,#52686,#52687,
#52688,#52689,#52690,#52691,#52692,#52693,#52694),.UNSPECIFIED.,.F.,.F.)
B_SPLINE_CURVE_WITH_KNOTS((6,1,1,1,1,1,1,1,1,1,1,1,1,1,1,1,1,1,1,1,1,1,
1,1,1,1,1,1,1,1,1,1,1,1,1,1,1,1,1,1,1,1,1,1,1,1,1,1,1,1,1,1,1,1,1,1,1,1,
1,1,1,1,1,1,1,6),(0.,0.0153846153846154,0.0307692307692308,0.0461538461538462,
0.0615384615384615,0.0769230769230769,0.0923076923076923,0.107692307692308,
0.123076923076923,0.138461538461538,0.153846153846154,0.169230769230769,
0.184615384615385,0.2,0.215384615384615,0.230769230769231,0.246153846153846,
0.261538461538462,0.276923076923077,0.292307692307692,0.307692307692308,
0.323076923076923,0.338461538461538,0.353846153846154,0.369230769230769,
0.384615384615385,0.4,0.415384615384615,0.430769230769231,0.446153846153846,
0.461538461538462,0.476923076923077,0.492307692307692,0.507692307692308,
0.523076923076923,0.538461538461538,0.553846153846154,0.569230769230769,
0.584615384615384,0.6,0.615384615384615,0.63076923076923,0.646153846153846,
0.661538461538461,0.676923076923076,0.692307692307692,0.707692307692307,
0.723076923076922,0.738461538461538,0.753846153846153,0.769230769230768,
0.784615384615384,0.799999999999999,0.815384615384614,0.83076923076923,
0.846153846153845,0.86153846153846,0.876923076923076,0.892307692307691,
0.907692307692306,0.923076923076922,0.938461538461537,0.953846153846152,
0.969230769230768,0.984615384615383,0.9942281567397),.UNSPECIFIED.)
CURVE()
GEOMETRIC_REPRESENTATION_ITEM()
RATIONAL_B_SPLINE_CURVE((1.,1.,1.,1.,1.,1.,1.,1.,1.,1.,1.,1.,1.,1.,1.,1.,
1.,1.,1.,1.,1.,1.,1.,1.,1.,1.,1.,1.,1.,1.,1.,1.,1.,1.,1.,1.,1.,1.,1.,1.,
1.,1.,1.,1.,1.,1.,1.,1.,1.,1.,1.,1.,1.,1.,1.,1.,1.,1.,1.,1.,1.,1.,1.,1.,
1.,1.,1.,1.,1.,1.))
REPRESENTATION_ITEM('')
);
#373=(
BOUNDED_CURVE()
B_SPLINE_CURVE(5,(#52698,#52699,#52700,#52701,#52702,#52703,#52704,#52705,
#52706,#52707,#52708,#52709,#52710,#52711,#52712,#52713,#52714,#52715,#52716,
#52717,#52718,#52719,#52720,#52721,#52722,#52723,#52724,#52725,#52726,#52727,
#52728,#52729,#52730,#52731,#52732,#52733,#52734,#52735,#52736,#52737,#52738,
#52739,#52740,#52741,#52742,#52743,#52744,#52745,#52746,#52747,#52748,#52749,
#52750,#52751,#52752,#52753,#52754,#52755,#52756,#52757,#52758,#52759,#52760,
#52761,#52762,#52763,#52764,#52765,#52766,#52767),.UNSPECIFIED.,.F.,.F.)
B_SPLINE_CURVE_WITH_KNOTS((6,1,1,1,1,1,1,1,1,1,1,1,1,1,1,1,1,1,1,1,1,1,
1,1,1,1,1,1,1,1,1,1,1,1,1,1,1,1,1,1,1,1,1,1,1,1,1,1,1,1,1,1,1,1,1,1,1,1,
1,1,1,1,1,1,1,6),(0.00577184337452087,0.0153846153846154,0.0307692307692308,
0.0461538461538462,0.0615384615384615,0.0769230769230769,0.0923076923076923,
0.107692307692308,0.123076923076923,0.138461538461538,0.153846153846154,
0.169230769230769,0.184615384615385,0.2,0.215384615384615,0.230769230769231,
0.246153846153846,0.261538461538462,0.276923076923077,0.292307692307692,
0.307692307692308,0.323076923076923,0.338461538461538,0.353846153846154,
0.369230769230769,0.384615384615385,0.4,0.415384615384615,0.430769230769231,
0.446153846153846,0.461538461538462,0.476923076923077,0.492307692307692,
0.507692307692308,0.523076923076923,0.538461538461538,0.553846153846154,
0.569230769230769,0.584615384615384,0.6,0.615384615384615,0.63076923076923,
0.646153846153846,0.661538461538461,0.676923076923076,0.692307692307692,
0.707692307692307,0.723076923076922,0.738461538461538,0.753846153846153,
0.769230769230768,0.784615384615384,0.799999999999999,0.815384615384614,
0.83076923076923,0.846153846153845,0.86153846153846,0.876923076923076,0.892307692307691,
0.907692307692306,0.923076923076922,0.938461538461537,0.953846153846152,
0.969230769230768,0.984615384615383,1.),.UNSPECIFIED.)
CURVE()
GEOMETRIC_REPRESENTATION_ITEM()
RATIONAL_B_SPLINE_CURVE((1.,1.,1.,1.,1.,1.,1.,1.,1.,1.,1.,1.,1.,1.,1.,1.,
1.,1.,1.,1.,1.,1.,1.,1.,1.,1.,1.,1.,1.,1.,1.,1.,1.,1.,1.,1.,1.,1.,1.,1.,
1.,1.,1.,1.,1.,1.,1.,1.,1.,1.,1.,1.,1.,1.,1.,1.,1.,1.,1.,1.,1.,1.,1.,1.,
1.,1.,1.,1.,1.,1.))
REPRESENTATION_ITEM('')
);
#374=(
BOUNDED_CURVE()
B_SPLINE_CURVE(5,(#52771,#52772,#52773,#52774,#52775,#52776,#52777,#52778,
#52779,#52780,#52781,#52782,#52783,#52784,#52785,#52786,#52787,#52788,#52789,
#52790,#52791,#52792,#52793,#52794,#52795,#52796,#52797,#52798,#52799,#52800,
#52801,#52802,#52803,#52804,#52805,#52806,#52807,#52808,#52809,#52810,#52811,
#52812,#52813,#52814,#52815,#52816,#52817,#52818,#52819,#52820,#52821,#52822,
#52823,#52824,#52825,#52826,#52827,#52828,#52829,#52830,#52831,#52832,#52833,
#52834,#52835,#52836,#52837,#52838,#52839,#52840),.UNSPECIFIED.,.F.,.F.)
B_SPLINE_CURVE_WITH_KNOTS((6,1,1,1,1,1,1,1,1,1,1,1,1,1,1,1,1,1,1,1,1,1,
1,1,1,1,1,1,1,1,1,1,1,1,1,1,1,1,1,1,1,1,1,1,1,1,1,1,1,1,1,1,1,1,1,1,1,1,
1,1,1,1,1,1,1,6),(0.,0.0153846153846154,0.0307692307692308,0.0461538461538462,
0.0615384615384615,0.0769230769230769,0.0923076923076923,0.107692307692308,
0.123076923076923,0.138461538461538,0.153846153846154,0.169230769230769,
0.184615384615385,0.2,0.215384615384615,0.230769230769231,0.246153846153846,
0.261538461538462,0.276923076923077,0.292307692307692,0.307692307692308,
0.323076923076923,0.338461538461538,0.353846153846154,0.369230769230769,
0.384615384615385,0.4,0.415384615384615,0.430769230769231,0.446153846153846,
0.461538461538462,0.476923076923077,0.492307692307692,0.507692307692308,
0.523076923076923,0.538461538461538,0.553846153846154,0.569230769230769,
0.584615384615384,0.6,0.615384615384615,0.63076923076923,0.646153846153846,
0.661538461538461,0.676923076923076,0.692307692307692,0.707692307692307,
0.723076923076922,0.738461538461538,0.753846153846153,0.769230769230768,
0.784615384615384,0.799999999999999,0.815384615384614,0.83076923076923,
0.846153846153845,0.86153846153846,0.876923076923076,0.892307692307691,
0.907692307692306,0.923076923076922,0.938461538461537,0.953846153846152,
0.969230769230768,0.984615384615383,0.994228156739692),.UNSPECIFIED.)
CURVE()
GEOMETRIC_REPRESENTATION_ITEM()
RATIONAL_B_SPLINE_CURVE((1.,1.,1.,1.,1.,1.,1.,1.,1.,1.,1.,1.,1.,1.,1.,1.,
1.,1.,1.,1.,1.,1.,1.,1.,1.,1.,1.,1.,1.,1.,1.,1.,1.,1.,1.,1.,1.,1.,1.,1.,
1.,1.,1.,1.,1.,1.,1.,1.,1.,1.,1.,1.,1.,1.,1.,1.,1.,1.,1.,1.,1.,1.,1.,1.,
1.,1.,1.,1.,1.,1.))
REPRESENTATION_ITEM('')
);
#375=(
BOUNDED_CURVE()
B_SPLINE_CURVE(5,(#52844,#52845,#52846,#52847,#52848,#52849,#52850,#52851,
#52852,#52853,#52854,#52855,#52856,#52857,#52858,#52859,#52860,#52861,#52862,
#52863,#52864,#52865,#52866,#52867,#52868,#52869,#52870,#52871,#52872,#52873,
#52874,#52875,#52876,#52877,#52878,#52879,#52880,#52881,#52882,#52883,#52884,
#52885,#52886,#52887,#52888,#52889,#52890,#52891,#52892,#52893,#52894,#52895,
#52896,#52897,#52898,#52899,#52900,#52901,#52902,#52903,#52904,#52905,#52906,
#52907,#52908,#52909,#52910,#52911,#52912,#52913),.UNSPECIFIED.,.F.,.F.)
B_SPLINE_CURVE_WITH_KNOTS((6,1,1,1,1,1,1,1,1,1,1,1,1,1,1,1,1,1,1,1,1,1,
1,1,1,1,1,1,1,1,1,1,1,1,1,1,1,1,1,1,1,1,1,1,1,1,1,1,1,1,1,1,1,1,1,1,1,1,
1,1,1,1,1,1,1,6),(0.00577184337450777,0.0153846153846154,0.0307692307692308,
0.0461538461538462,0.0615384615384615,0.0769230769230769,0.0923076923076923,
0.107692307692308,0.123076923076923,0.138461538461538,0.153846153846154,
0.169230769230769,0.184615384615385,0.2,0.215384615384615,0.230769230769231,
0.246153846153846,0.261538461538462,0.276923076923077,0.292307692307692,
0.307692307692308,0.323076923076923,0.338461538461538,0.353846153846154,
0.369230769230769,0.384615384615385,0.4,0.415384615384615,0.430769230769231,
0.446153846153846,0.461538461538462,0.476923076923077,0.492307692307692,
0.507692307692308,0.523076923076923,0.538461538461538,0.553846153846154,
0.569230769230769,0.584615384615384,0.6,0.615384615384615,0.63076923076923,
0.646153846153846,0.661538461538461,0.676923076923076,0.692307692307692,
0.707692307692307,0.723076923076922,0.738461538461538,0.753846153846153,
0.769230769230768,0.784615384615384,0.799999999999999,0.815384615384614,
0.83076923076923,0.846153846153845,0.86153846153846,0.876923076923076,0.892307692307691,
0.907692307692306,0.923076923076922,0.938461538461537,0.953846153846152,
0.969230769230768,0.984615384615383,1.),.UNSPECIFIED.)
CURVE()
GEOMETRIC_REPRESENTATION_ITEM()
RATIONAL_B_SPLINE_CURVE((1.,1.,1.,1.,1.,1.,1.,1.,1.,1.,1.,1.,1.,1.,1.,1.,
1.,1.,1.,1.,1.,1.,1.,1.,1.,1.,1.,1.,1.,1.,1.,1.,1.,1.,1.,1.,1.,1.,1.,1.,
1.,1.,1.,1.,1.,1.,1.,1.,1.,1.,1.,1.,1.,1.,1.,1.,1.,1.,1.,1.,1.,1.,1.,1.,
1.,1.,1.,1.,1.,1.))
REPRESENTATION_ITEM('')
);
#376=(
BOUNDED_CURVE()
B_SPLINE_CURVE(5,(#52917,#52918,#52919,#52920,#52921,#52922,#52923,#52924,
#52925,#52926,#52927,#52928,#52929,#52930,#52931,#52932,#52933,#52934,#52935,
#52936,#52937,#52938,#52939,#52940,#52941,#52942,#52943,#52944,#52945,#52946,
#52947,#52948,#52949,#52950,#52951,#52952,#52953,#52954,#52955,#52956,#52957,
#52958,#52959,#52960,#52961,#52962,#52963,#52964,#52965,#52966,#52967,#52968,
#52969,#52970,#52971,#52972,#52973,#52974,#52975,#52976,#52977,#52978,#52979,
#52980,#52981,#52982,#52983,#52984,#52985,#52986),.UNSPECIFIED.,.F.,.F.)
B_SPLINE_CURVE_WITH_KNOTS((6,1,1,1,1,1,1,1,1,1,1,1,1,1,1,1,1,1,1,1,1,1,
1,1,1,1,1,1,1,1,1,1,1,1,1,1,1,1,1,1,1,1,1,1,1,1,1,1,1,1,1,1,1,1,1,1,1,1,
1,1,1,1,1,1,1,6),(0.,0.0153846153846154,0.0307692307692308,0.0461538461538462,
0.0615384615384615,0.0769230769230769,0.0923076923076923,0.107692307692308,
0.123076923076923,0.138461538461538,0.153846153846154,0.169230769230769,
0.184615384615385,0.2,0.215384615384615,0.230769230769231,0.246153846153846,
0.261538461538462,0.276923076923077,0.292307692307692,0.307692307692308,
0.323076923076923,0.338461538461538,0.353846153846154,0.369230769230769,
0.384615384615385,0.4,0.415384615384615,0.430769230769231,0.446153846153846,
0.461538461538462,0.476923076923077,0.492307692307692,0.507692307692308,
0.523076923076923,0.538461538461538,0.553846153846154,0.569230769230769,
0.584615384615384,0.6,0.615384615384615,0.63076923076923,0.646153846153846,
0.661538461538461,0.676923076923076,0.692307692307692,0.707692307692307,
0.723076923076922,0.738461538461538,0.753846153846153,0.769230769230768,
0.784615384615384,0.799999999999999,0.815384615384614,0.83076923076923,
0.846153846153845,0.86153846153846,0.876923076923076,0.892307692307691,
0.907692307692306,0.923076923076922,0.938461538461537,0.953846153846152,
0.969230769230768,0.984615384615383,0.994228156739701),.UNSPECIFIED.)
CURVE()
GEOMETRIC_REPRESENTATION_ITEM()
RATIONAL_B_SPLINE_CURVE((1.,1.,1.,1.,1.,1.,1.,1.,1.,1.,1.,1.,1.,1.,1.,1.,
1.,1.,1.,1.,1.,1.,1.,1.,1.,1.,1.,1.,1.,1.,1.,1.,1.,1.,1.,1.,1.,1.,1.,1.,
1.,1.,1.,1.,1.,1.,1.,1.,1.,1.,1.,1.,1.,1.,1.,1.,1.,1.,1.,1.,1.,1.,1.,1.,
1.,1.,1.,1.,1.,1.))
REPRESENTATION_ITEM('')
);
#377=(
BOUNDED_CURVE()
B_SPLINE_CURVE(5,(#52990,#52991,#52992,#52993,#52994,#52995,#52996,#52997,
#52998,#52999,#53000,#53001,#53002,#53003,#53004,#53005,#53006,#53007,#53008,
#53009,#53010,#53011,#53012,#53013,#53014,#53015,#53016,#53017,#53018,#53019,
#53020,#53021,#53022,#53023,#53024,#53025,#53026,#53027,#53028,#53029,#53030,
#53031,#53032,#53033,#53034,#53035,#53036,#53037,#53038,#53039,#53040,#53041,
#53042,#53043,#53044,#53045,#53046,#53047,#53048,#53049,#53050,#53051,#53052,
#53053,#53054,#53055,#53056,#53057,#53058,#53059),.UNSPECIFIED.,.F.,.F.)
B_SPLINE_CURVE_WITH_KNOTS((6,1,1,1,1,1,1,1,1,1,1,1,1,1,1,1,1,1,1,1,1,1,
1,1,1,1,1,1,1,1,1,1,1,1,1,1,1,1,1,1,1,1,1,1,1,1,1,1,1,1,1,1,1,1,1,1,1,1,
1,1,1,1,1,1,1,6),(0.00577184337450943,0.0153846153846154,0.0307692307692308,
0.0461538461538462,0.0615384615384615,0.0769230769230769,0.0923076923076923,
0.107692307692308,0.123076923076923,0.138461538461538,0.153846153846154,
0.169230769230769,0.184615384615385,0.2,0.215384615384615,0.230769230769231,
0.246153846153846,0.261538461538462,0.276923076923077,0.292307692307692,
0.307692307692308,0.323076923076923,0.338461538461538,0.353846153846154,
0.369230769230769,0.384615384615385,0.4,0.415384615384615,0.430769230769231,
0.446153846153846,0.461538461538462,0.476923076923077,0.492307692307692,
0.507692307692308,0.523076923076923,0.538461538461538,0.553846153846154,
0.569230769230769,0.584615384615384,0.6,0.615384615384615,0.63076923076923,
0.646153846153846,0.661538461538461,0.676923076923076,0.692307692307692,
0.707692307692307,0.723076923076922,0.738461538461538,0.753846153846153,
0.769230769230768,0.784615384615384,0.799999999999999,0.815384615384614,
0.83076923076923,0.846153846153845,0.86153846153846,0.876923076923076,0.892307692307691,
0.907692307692306,0.923076923076922,0.938461538461537,0.953846153846152,
0.969230769230768,0.984615384615383,1.),.UNSPECIFIED.)
CURVE()
GEOMETRIC_REPRESENTATION_ITEM()
RATIONAL_B_SPLINE_CURVE((1.,1.,1.,1.,1.,1.,1.,1.,1.,1.,1.,1.,1.,1.,1.,1.,
1.,1.,1.,1.,1.,1.,1.,1.,1.,1.,1.,1.,1.,1.,1.,1.,1.,1.,1.,1.,1.,1.,1.,1.,
1.,1.,1.,1.,1.,1.,1.,1.,1.,1.,1.,1.,1.,1.,1.,1.,1.,1.,1.,1.,1.,1.,1.,1.,
1.,1.,1.,1.,1.,1.))
REPRESENTATION_ITEM('')
);
#378=(
BOUNDED_CURVE()
B_SPLINE_CURVE(5,(#53063,#53064,#53065,#53066,#53067,#53068,#53069,#53070,
#53071,#53072,#53073,#53074,#53075,#53076,#53077,#53078,#53079,#53080,#53081,
#53082,#53083,#53084,#53085,#53086,#53087,#53088,#53089,#53090,#53091,#53092,
#53093,#53094,#53095,#53096,#53097,#53098,#53099,#53100,#53101,#53102,#53103,
#53104,#53105,#53106,#53107,#53108,#53109,#53110,#53111,#53112,#53113,#53114,
#53115,#53116,#53117,#53118,#53119,#53120,#53121,#53122,#53123,#53124,#53125,
#53126,#53127,#53128,#53129,#53130,#53131,#53132),.UNSPECIFIED.,.F.,.F.)
B_SPLINE_CURVE_WITH_KNOTS((6,1,1,1,1,1,1,1,1,1,1,1,1,1,1,1,1,1,1,1,1,1,
1,1,1,1,1,1,1,1,1,1,1,1,1,1,1,1,1,1,1,1,1,1,1,1,1,1,1,1,1,1,1,1,1,1,1,1,
1,1,1,1,1,1,1,6),(0.,0.0153846153846154,0.0307692307692308,0.0461538461538462,
0.0615384615384615,0.0769230769230769,0.0923076923076923,0.107692307692308,
0.123076923076923,0.138461538461538,0.153846153846154,0.169230769230769,
0.184615384615385,0.2,0.215384615384615,0.230769230769231,0.246153846153846,
0.261538461538462,0.276923076923077,0.292307692307692,0.307692307692308,
0.323076923076923,0.338461538461538,0.353846153846154,0.369230769230769,
0.384615384615385,0.4,0.415384615384615,0.430769230769231,0.446153846153846,
0.461538461538462,0.476923076923077,0.492307692307692,0.507692307692308,
0.523076923076923,0.538461538461538,0.553846153846154,0.569230769230769,
0.584615384615384,0.6,0.615384615384615,0.63076923076923,0.646153846153846,
0.661538461538461,0.676923076923076,0.692307692307692,0.707692307692307,
0.723076923076922,0.738461538461538,0.753846153846153,0.769230769230768,
0.784615384615384,0.799999999999999,0.815384615384614,0.83076923076923,
0.846153846153845,0.86153846153846,0.876923076923076,0.892307692307691,
0.907692307692306,0.923076923076922,0.938461538461537,0.953846153846152,
0.969230769230768,0.984615384615383,0.994228156739699),.UNSPECIFIED.)
CURVE()
GEOMETRIC_REPRESENTATION_ITEM()
RATIONAL_B_SPLINE_CURVE((1.,1.,1.,1.,1.,1.,1.,1.,1.,1.,1.,1.,1.,1.,1.,1.,
1.,1.,1.,1.,1.,1.,1.,1.,1.,1.,1.,1.,1.,1.,1.,1.,1.,1.,1.,1.,1.,1.,1.,1.,
1.,1.,1.,1.,1.,1.,1.,1.,1.,1.,1.,1.,1.,1.,1.,1.,1.,1.,1.,1.,1.,1.,1.,1.,
1.,1.,1.,1.,1.,1.))
REPRESENTATION_ITEM('')
);
#379=(
BOUNDED_CURVE()
B_SPLINE_CURVE(5,(#53136,#53137,#53138,#53139,#53140,#53141,#53142,#53143,
#53144,#53145,#53146,#53147,#53148,#53149,#53150,#53151,#53152,#53153,#53154,
#53155,#53156,#53157,#53158,#53159,#53160,#53161,#53162,#53163,#53164,#53165,
#53166,#53167,#53168,#53169,#53170,#53171,#53172,#53173,#53174,#53175,#53176,
#53177,#53178,#53179,#53180,#53181,#53182,#53183,#53184,#53185,#53186,#53187,
#53188,#53189,#53190,#53191,#53192,#53193,#53194,#53195,#53196,#53197,#53198,
#53199,#53200,#53201,#53202,#53203,#53204,#53205),.UNSPECIFIED.,.F.,.F.)
B_SPLINE_CURVE_WITH_KNOTS((6,1,1,1,1,1,1,1,1,1,1,1,1,1,1,1,1,1,1,1,1,1,
1,1,1,1,1,1,1,1,1,1,1,1,1,1,1,1,1,1,1,1,1,1,1,1,1,1,1,1,1,1,1,1,1,1,1,1,
1,1,1,1,1,1,1,6),(0.00577184337448657,0.0153846153846154,0.0307692307692308,
0.0461538461538462,0.0615384615384615,0.0769230769230769,0.0923076923076923,
0.107692307692308,0.123076923076923,0.138461538461538,0.153846153846154,
0.169230769230769,0.184615384615385,0.2,0.215384615384615,0.230769230769231,
0.246153846153846,0.261538461538462,0.276923076923077,0.292307692307692,
0.307692307692308,0.323076923076923,0.338461538461538,0.353846153846154,
0.369230769230769,0.384615384615385,0.4,0.415384615384615,0.430769230769231,
0.446153846153846,0.461538461538462,0.476923076923077,0.492307692307692,
0.507692307692308,0.523076923076923,0.538461538461538,0.553846153846154,
0.569230769230769,0.584615384615384,0.6,0.615384615384615,0.63076923076923,
0.646153846153846,0.661538461538461,0.676923076923076,0.692307692307692,
0.707692307692307,0.723076923076922,0.738461538461538,0.753846153846153,
0.769230769230768,0.784615384615384,0.799999999999999,0.815384615384614,
0.83076923076923,0.846153846153845,0.86153846153846,0.876923076923076,0.892307692307691,
0.907692307692306,0.923076923076922,0.938461538461537,0.953846153846152,
0.969230769230768,0.984615384615383,1.),.UNSPECIFIED.)
CURVE()
GEOMETRIC_REPRESENTATION_ITEM()
RATIONAL_B_SPLINE_CURVE((1.,1.,1.,1.,1.,1.,1.,1.,1.,1.,1.,1.,1.,1.,1.,1.,
1.,1.,1.,1.,1.,1.,1.,1.,1.,1.,1.,1.,1.,1.,1.,1.,1.,1.,1.,1.,1.,1.,1.,1.,
1.,1.,1.,1.,1.,1.,1.,1.,1.,1.,1.,1.,1.,1.,1.,1.,1.,1.,1.,1.,1.,1.,1.,1.,
1.,1.,1.,1.,1.,1.))
REPRESENTATION_ITEM('')
);
#380=(
BOUNDED_CURVE()
B_SPLINE_CURVE(5,(#53209,#53210,#53211,#53212,#53213,#53214,#53215,#53216,
#53217,#53218,#53219,#53220,#53221,#53222,#53223,#53224,#53225,#53226,#53227,
#53228,#53229,#53230,#53231,#53232,#53233,#53234,#53235,#53236,#53237,#53238,
#53239,#53240,#53241,#53242,#53243,#53244,#53245,#53246,#53247,#53248,#53249,
#53250,#53251,#53252,#53253,#53254,#53255,#53256,#53257,#53258,#53259,#53260,
#53261,#53262,#53263,#53264,#53265,#53266,#53267,#53268,#53269,#53270,#53271,
#53272,#53273,#53274,#53275,#53276,#53277,#53278),.UNSPECIFIED.,.F.,.F.)
B_SPLINE_CURVE_WITH_KNOTS((6,1,1,1,1,1,1,1,1,1,1,1,1,1,1,1,1,1,1,1,1,1,
1,1,1,1,1,1,1,1,1,1,1,1,1,1,1,1,1,1,1,1,1,1,1,1,1,1,1,1,1,1,1,1,1,1,1,1,
1,1,1,1,1,1,1,6),(0.,0.0153846153846154,0.0307692307692308,0.0461538461538462,
0.0615384615384615,0.0769230769230769,0.0923076923076923,0.107692307692308,
0.123076923076923,0.138461538461538,0.153846153846154,0.169230769230769,
0.184615384615385,0.2,0.215384615384615,0.230769230769231,0.246153846153846,
0.261538461538462,0.276923076923077,0.292307692307692,0.307692307692308,
0.323076923076923,0.338461538461538,0.353846153846154,0.369230769230769,
0.384615384615385,0.4,0.415384615384615,0.430769230769231,0.446153846153846,
0.461538461538462,0.476923076923077,0.492307692307692,0.507692307692308,
0.523076923076923,0.538461538461538,0.553846153846154,0.569230769230769,
0.584615384615384,0.6,0.615384615384615,0.63076923076923,0.646153846153846,
0.661538461538461,0.676923076923076,0.692307692307692,0.707692307692307,
0.723076923076922,0.738461538461538,0.753846153846153,0.769230769230768,
0.784615384615384,0.799999999999999,0.815384615384614,0.83076923076923,
0.846153846153845,0.86153846153846,0.876923076923076,0.892307692307691,
0.907692307692306,0.923076923076922,0.938461538461537,0.953846153846152,
0.969230769230768,0.984615384615383,0.994228156739709),.UNSPECIFIED.)
CURVE()
GEOMETRIC_REPRESENTATION_ITEM()
RATIONAL_B_SPLINE_CURVE((1.,1.,1.,1.,1.,1.,1.,1.,1.,1.,1.,1.,1.,1.,1.,1.,
1.,1.,1.,1.,1.,1.,1.,1.,1.,1.,1.,1.,1.,1.,1.,1.,1.,1.,1.,1.,1.,1.,1.,1.,
1.,1.,1.,1.,1.,1.,1.,1.,1.,1.,1.,1.,1.,1.,1.,1.,1.,1.,1.,1.,1.,1.,1.,1.,
1.,1.,1.,1.,1.,1.))
REPRESENTATION_ITEM('')
);
#381=(
BOUNDED_CURVE()
B_SPLINE_CURVE(5,(#53282,#53283,#53284,#53285,#53286,#53287,#53288,#53289,
#53290,#53291,#53292,#53293,#53294,#53295,#53296,#53297,#53298,#53299,#53300,
#53301,#53302,#53303,#53304,#53305,#53306,#53307,#53308,#53309,#53310,#53311,
#53312,#53313,#53314,#53315,#53316,#53317,#53318,#53319,#53320,#53321,#53322,
#53323,#53324,#53325,#53326,#53327,#53328,#53329,#53330,#53331,#53332,#53333,
#53334,#53335,#53336,#53337,#53338,#53339,#53340,#53341,#53342,#53343,#53344,
#53345,#53346,#53347,#53348,#53349,#53350,#53351),.UNSPECIFIED.,.F.,.F.)
B_SPLINE_CURVE_WITH_KNOTS((6,1,1,1,1,1,1,1,1,1,1,1,1,1,1,1,1,1,1,1,1,1,
1,1,1,1,1,1,1,1,1,1,1,1,1,1,1,1,1,1,1,1,1,1,1,1,1,1,1,1,1,1,1,1,1,1,1,1,
1,1,1,1,1,1,1,6),(0.00577184337451132,0.0153846153846154,0.0307692307692308,
0.0461538461538462,0.0615384615384615,0.0769230769230769,0.0923076923076923,
0.107692307692308,0.123076923076923,0.138461538461538,0.153846153846154,
0.169230769230769,0.184615384615385,0.2,0.215384615384615,0.230769230769231,
0.246153846153846,0.261538461538462,0.276923076923077,0.292307692307692,
0.307692307692308,0.323076923076923,0.338461538461538,0.353846153846154,
0.369230769230769,0.384615384615385,0.4,0.415384615384615,0.430769230769231,
0.446153846153846,0.461538461538462,0.476923076923077,0.492307692307692,
0.507692307692308,0.523076923076923,0.538461538461538,0.553846153846154,
0.569230769230769,0.584615384615384,0.6,0.615384615384615,0.63076923076923,
0.646153846153846,0.661538461538461,0.676923076923076,0.692307692307692,
0.707692307692307,0.723076923076922,0.738461538461538,0.753846153846153,
0.769230769230768,0.784615384615384,0.799999999999999,0.815384615384614,
0.83076923076923,0.846153846153845,0.86153846153846,0.876923076923076,0.892307692307691,
0.907692307692306,0.923076923076922,0.938461538461537,0.953846153846152,
0.969230769230768,0.984615384615383,1.),.UNSPECIFIED.)
CURVE()
GEOMETRIC_REPRESENTATION_ITEM()
RATIONAL_B_SPLINE_CURVE((1.,1.,1.,1.,1.,1.,1.,1.,1.,1.,1.,1.,1.,1.,1.,1.,
1.,1.,1.,1.,1.,1.,1.,1.,1.,1.,1.,1.,1.,1.,1.,1.,1.,1.,1.,1.,1.,1.,1.,1.,
1.,1.,1.,1.,1.,1.,1.,1.,1.,1.,1.,1.,1.,1.,1.,1.,1.,1.,1.,1.,1.,1.,1.,1.,
1.,1.,1.,1.,1.,1.))
REPRESENTATION_ITEM('')
);
#382=(
BOUNDED_CURVE()
B_SPLINE_CURVE(5,(#53355,#53356,#53357,#53358,#53359,#53360,#53361,#53362,
#53363,#53364,#53365,#53366,#53367,#53368,#53369,#53370,#53371,#53372,#53373,
#53374,#53375,#53376,#53377,#53378,#53379,#53380,#53381,#53382,#53383,#53384,
#53385,#53386,#53387,#53388,#53389,#53390,#53391,#53392,#53393,#53394,#53395,
#53396,#53397,#53398,#53399,#53400,#53401,#53402,#53403,#53404,#53405,#53406,
#53407,#53408,#53409,#53410,#53411,#53412,#53413,#53414,#53415,#53416,#53417,
#53418,#53419,#53420,#53421,#53422,#53423,#53424),.UNSPECIFIED.,.F.,.F.)
B_SPLINE_CURVE_WITH_KNOTS((6,1,1,1,1,1,1,1,1,1,1,1,1,1,1,1,1,1,1,1,1,1,
1,1,1,1,1,1,1,1,1,1,1,1,1,1,1,1,1,1,1,1,1,1,1,1,1,1,1,1,1,1,1,1,1,1,1,1,
1,1,1,1,1,1,1,6),(0.,0.0153846153846154,0.0307692307692308,0.0461538461538462,
0.0615384615384615,0.0769230769230769,0.0923076923076923,0.107692307692308,
0.123076923076923,0.138461538461538,0.153846153846154,0.169230769230769,
0.184615384615385,0.2,0.215384615384615,0.230769230769231,0.246153846153846,
0.261538461538462,0.276923076923077,0.292307692307692,0.307692307692308,
0.323076923076923,0.338461538461538,0.353846153846154,0.369230769230769,
0.384615384615385,0.4,0.415384615384615,0.430769230769231,0.446153846153846,
0.461538461538462,0.476923076923077,0.492307692307692,0.507692307692308,
0.523076923076923,0.538461538461538,0.553846153846154,0.569230769230769,
0.584615384615384,0.6,0.615384615384615,0.63076923076923,0.646153846153846,
0.661538461538461,0.676923076923076,0.692307692307692,0.707692307692307,
0.723076923076922,0.738461538461538,0.753846153846153,0.769230769230768,
0.784615384615384,0.799999999999999,0.815384615384614,0.83076923076923,
0.846153846153845,0.86153846153846,0.876923076923076,0.892307692307691,
0.907692307692306,0.923076923076922,0.938461538461537,0.953846153846152,
0.969230769230768,0.984615384615383,0.994228156739705),.UNSPECIFIED.)
CURVE()
GEOMETRIC_REPRESENTATION_ITEM()
RATIONAL_B_SPLINE_CURVE((1.,1.,1.,1.,1.,1.,1.,1.,1.,1.,1.,1.,1.,1.,1.,1.,
1.,1.,1.,1.,1.,1.,1.,1.,1.,1.,1.,1.,1.,1.,1.,1.,1.,1.,1.,1.,1.,1.,1.,1.,
1.,1.,1.,1.,1.,1.,1.,1.,1.,1.,1.,1.,1.,1.,1.,1.,1.,1.,1.,1.,1.,1.,1.,1.,
1.,1.,1.,1.,1.,1.))
REPRESENTATION_ITEM('')
);
#383=(
BOUNDED_CURVE()
B_SPLINE_CURVE(5,(#53428,#53429,#53430,#53431,#53432,#53433,#53434,#53435,
#53436,#53437,#53438,#53439,#53440,#53441,#53442,#53443,#53444,#53445,#53446,
#53447,#53448,#53449,#53450,#53451,#53452,#53453,#53454,#53455,#53456,#53457,
#53458,#53459,#53460,#53461,#53462,#53463,#53464,#53465,#53466,#53467,#53468,
#53469,#53470,#53471,#53472,#53473,#53474,#53475,#53476,#53477,#53478,#53479,
#53480,#53481,#53482,#53483,#53484,#53485,#53486,#53487,#53488,#53489,#53490,
#53491,#53492,#53493,#53494,#53495,#53496,#53497),.UNSPECIFIED.,.F.,.F.)
B_SPLINE_CURVE_WITH_KNOTS((6,1,1,1,1,1,1,1,1,1,1,1,1,1,1,1,1,1,1,1,1,1,
1,1,1,1,1,1,1,1,1,1,1,1,1,1,1,1,1,1,1,1,1,1,1,1,1,1,1,1,1,1,1,1,1,1,1,1,
1,1,1,1,1,1,1,6),(0.00577184337450072,0.0153846153846154,0.0307692307692308,
0.0461538461538462,0.0615384615384615,0.0769230769230769,0.0923076923076923,
0.107692307692308,0.123076923076923,0.138461538461538,0.153846153846154,
0.169230769230769,0.184615384615385,0.2,0.215384615384615,0.230769230769231,
0.246153846153846,0.261538461538462,0.276923076923077,0.292307692307692,
0.307692307692308,0.323076923076923,0.338461538461538,0.353846153846154,
0.369230769230769,0.384615384615385,0.4,0.415384615384615,0.430769230769231,
0.446153846153846,0.461538461538462,0.476923076923077,0.492307692307692,
0.507692307692308,0.523076923076923,0.538461538461538,0.553846153846154,
0.569230769230769,0.584615384615384,0.6,0.615384615384615,0.63076923076923,
0.646153846153846,0.661538461538461,0.676923076923076,0.692307692307692,
0.707692307692307,0.723076923076922,0.738461538461538,0.753846153846153,
0.769230769230768,0.784615384615384,0.799999999999999,0.815384615384614,
0.83076923076923,0.846153846153845,0.86153846153846,0.876923076923076,0.892307692307691,
0.907692307692306,0.923076923076922,0.938461538461537,0.953846153846152,
0.969230769230768,0.984615384615383,1.),.UNSPECIFIED.)
CURVE()
GEOMETRIC_REPRESENTATION_ITEM()
RATIONAL_B_SPLINE_CURVE((1.,1.,1.,1.,1.,1.,1.,1.,1.,1.,1.,1.,1.,1.,1.,1.,
1.,1.,1.,1.,1.,1.,1.,1.,1.,1.,1.,1.,1.,1.,1.,1.,1.,1.,1.,1.,1.,1.,1.,1.,
1.,1.,1.,1.,1.,1.,1.,1.,1.,1.,1.,1.,1.,1.,1.,1.,1.,1.,1.,1.,1.,1.,1.,1.,
1.,1.,1.,1.,1.,1.))
REPRESENTATION_ITEM('')
);
#384=(
BOUNDED_CURVE()
B_SPLINE_CURVE(5,(#53501,#53502,#53503,#53504,#53505,#53506,#53507,#53508,
#53509,#53510,#53511,#53512,#53513,#53514,#53515,#53516,#53517,#53518,#53519,
#53520,#53521,#53522,#53523,#53524,#53525,#53526,#53527,#53528,#53529,#53530,
#53531,#53532,#53533,#53534,#53535,#53536,#53537,#53538,#53539,#53540,#53541,
#53542,#53543,#53544,#53545,#53546,#53547,#53548,#53549,#53550,#53551,#53552,
#53553,#53554,#53555,#53556,#53557,#53558,#53559,#53560,#53561,#53562,#53563,
#53564,#53565,#53566,#53567,#53568,#53569,#53570),.UNSPECIFIED.,.F.,.F.)
B_SPLINE_CURVE_WITH_KNOTS((6,1,1,1,1,1,1,1,1,1,1,1,1,1,1,1,1,1,1,1,1,1,
1,1,1,1,1,1,1,1,1,1,1,1,1,1,1,1,1,1,1,1,1,1,1,1,1,1,1,1,1,1,1,1,1,1,1,1,
1,1,1,1,1,1,1,6),(0.,0.0153846153846154,0.0307692307692308,0.0461538461538462,
0.0615384615384615,0.0769230769230769,0.0923076923076923,0.107692307692308,
0.123076923076923,0.138461538461538,0.153846153846154,0.169230769230769,
0.184615384615385,0.2,0.215384615384615,0.230769230769231,0.246153846153846,
0.261538461538462,0.276923076923077,0.292307692307692,0.307692307692308,
0.323076923076923,0.338461538461538,0.353846153846154,0.369230769230769,
0.384615384615385,0.4,0.415384615384615,0.430769230769231,0.446153846153846,
0.461538461538462,0.476923076923077,0.492307692307692,0.507692307692308,
0.523076923076923,0.538461538461538,0.553846153846154,0.569230769230769,
0.584615384615384,0.6,0.615384615384615,0.63076923076923,0.646153846153846,
0.661538461538461,0.676923076923076,0.692307692307692,0.707692307692307,
0.723076923076922,0.738461538461538,0.753846153846153,0.769230769230768,
0.784615384615384,0.799999999999999,0.815384615384614,0.83076923076923,
0.846153846153845,0.86153846153846,0.876923076923076,0.892307692307691,
0.907692307692306,0.923076923076922,0.938461538461537,0.953846153846152,
0.969230769230768,0.984615384615383,0.994228156739706),.UNSPECIFIED.)
CURVE()
GEOMETRIC_REPRESENTATION_ITEM()
RATIONAL_B_SPLINE_CURVE((1.,1.,1.,1.,1.,1.,1.,1.,1.,1.,1.,1.,1.,1.,1.,1.,
1.,1.,1.,1.,1.,1.,1.,1.,1.,1.,1.,1.,1.,1.,1.,1.,1.,1.,1.,1.,1.,1.,1.,1.,
1.,1.,1.,1.,1.,1.,1.,1.,1.,1.,1.,1.,1.,1.,1.,1.,1.,1.,1.,1.,1.,1.,1.,1.,
1.,1.,1.,1.,1.,1.))
REPRESENTATION_ITEM('')
);
#385=(
BOUNDED_CURVE()
B_SPLINE_CURVE(5,(#53574,#53575,#53576,#53577,#53578,#53579,#53580,#53581,
#53582,#53583,#53584,#53585,#53586,#53587,#53588,#53589,#53590,#53591,#53592,
#53593,#53594,#53595,#53596,#53597,#53598,#53599,#53600,#53601,#53602,#53603,
#53604,#53605,#53606,#53607,#53608,#53609,#53610,#53611,#53612,#53613,#53614,
#53615,#53616,#53617,#53618,#53619,#53620,#53621,#53622,#53623,#53624,#53625,
#53626,#53627,#53628,#53629,#53630,#53631,#53632,#53633,#53634,#53635,#53636,
#53637,#53638,#53639,#53640,#53641,#53642,#53643),.UNSPECIFIED.,.F.,.F.)
B_SPLINE_CURVE_WITH_KNOTS((6,1,1,1,1,1,1,1,1,1,1,1,1,1,1,1,1,1,1,1,1,1,
1,1,1,1,1,1,1,1,1,1,1,1,1,1,1,1,1,1,1,1,1,1,1,1,1,1,1,1,1,1,1,1,1,1,1,1,
1,1,1,1,1,1,1,6),(0.00577184337450902,0.0153846153846154,0.0307692307692308,
0.0461538461538462,0.0615384615384615,0.0769230769230769,0.0923076923076923,
0.107692307692308,0.123076923076923,0.138461538461538,0.153846153846154,
0.169230769230769,0.184615384615385,0.2,0.215384615384615,0.230769230769231,
0.246153846153846,0.261538461538462,0.276923076923077,0.292307692307692,
0.307692307692308,0.323076923076923,0.338461538461538,0.353846153846154,
0.369230769230769,0.384615384615385,0.4,0.415384615384615,0.430769230769231,
0.446153846153846,0.461538461538462,0.476923076923077,0.492307692307692,
0.507692307692308,0.523076923076923,0.538461538461538,0.553846153846154,
0.569230769230769,0.584615384615384,0.6,0.615384615384615,0.63076923076923,
0.646153846153846,0.661538461538461,0.676923076923076,0.692307692307692,
0.707692307692307,0.723076923076922,0.738461538461538,0.753846153846153,
0.769230769230768,0.784615384615384,0.799999999999999,0.815384615384614,
0.83076923076923,0.846153846153845,0.86153846153846,0.876923076923076,0.892307692307691,
0.907692307692306,0.923076923076922,0.938461538461537,0.953846153846152,
0.969230769230768,0.984615384615383,1.),.UNSPECIFIED.)
CURVE()
GEOMETRIC_REPRESENTATION_ITEM()
RATIONAL_B_SPLINE_CURVE((1.,1.,1.,1.,1.,1.,1.,1.,1.,1.,1.,1.,1.,1.,1.,1.,
1.,1.,1.,1.,1.,1.,1.,1.,1.,1.,1.,1.,1.,1.,1.,1.,1.,1.,1.,1.,1.,1.,1.,1.,
1.,1.,1.,1.,1.,1.,1.,1.,1.,1.,1.,1.,1.,1.,1.,1.,1.,1.,1.,1.,1.,1.,1.,1.,
1.,1.,1.,1.,1.,1.))
REPRESENTATION_ITEM('')
);
#386=(
BOUNDED_CURVE()
B_SPLINE_CURVE(5,(#53647,#53648,#53649,#53650,#53651,#53652,#53653,#53654,
#53655,#53656,#53657,#53658,#53659,#53660,#53661,#53662,#53663,#53664,#53665,
#53666,#53667,#53668,#53669,#53670,#53671,#53672,#53673,#53674,#53675,#53676,
#53677,#53678,#53679,#53680,#53681,#53682,#53683,#53684,#53685,#53686,#53687,
#53688,#53689,#53690,#53691,#53692,#53693,#53694,#53695,#53696,#53697,#53698,
#53699,#53700,#53701,#53702,#53703,#53704,#53705,#53706,#53707,#53708,#53709,
#53710,#53711,#53712,#53713,#53714,#53715,#53716),.UNSPECIFIED.,.F.,.F.)
B_SPLINE_CURVE_WITH_KNOTS((6,1,1,1,1,1,1,1,1,1,1,1,1,1,1,1,1,1,1,1,1,1,
1,1,1,1,1,1,1,1,1,1,1,1,1,1,1,1,1,1,1,1,1,1,1,1,1,1,1,1,1,1,1,1,1,1,1,1,
1,1,1,1,1,1,1,6),(0.,0.0153846153846154,0.0307692307692308,0.0461538461538462,
0.0615384615384615,0.0769230769230769,0.0923076923076923,0.107692307692308,
0.123076923076923,0.138461538461538,0.153846153846154,0.169230769230769,
0.184615384615385,0.2,0.215384615384615,0.230769230769231,0.246153846153846,
0.261538461538462,0.276923076923077,0.292307692307692,0.307692307692308,
0.323076923076923,0.338461538461538,0.353846153846154,0.369230769230769,
0.384615384615385,0.4,0.415384615384615,0.430769230769231,0.446153846153846,
0.461538461538462,0.476923076923077,0.492307692307692,0.507692307692308,
0.523076923076923,0.538461538461538,0.553846153846154,0.569230769230769,
0.584615384615384,0.6,0.615384615384615,0.63076923076923,0.646153846153846,
0.661538461538461,0.676923076923076,0.692307692307692,0.707692307692307,
0.723076923076922,0.738461538461538,0.753846153846153,0.769230769230768,
0.784615384615384,0.799999999999999,0.815384615384614,0.83076923076923,
0.846153846153845,0.86153846153846,0.876923076923076,0.892307692307691,
0.907692307692306,0.923076923076922,0.938461538461537,0.953846153846152,
0.969230769230768,0.984615384615383,0.994228156739698),.UNSPECIFIED.)
CURVE()
GEOMETRIC_REPRESENTATION_ITEM()
RATIONAL_B_SPLINE_CURVE((1.,1.,1.,1.,1.,1.,1.,1.,1.,1.,1.,1.,1.,1.,1.,1.,
1.,1.,1.,1.,1.,1.,1.,1.,1.,1.,1.,1.,1.,1.,1.,1.,1.,1.,1.,1.,1.,1.,1.,1.,
1.,1.,1.,1.,1.,1.,1.,1.,1.,1.,1.,1.,1.,1.,1.,1.,1.,1.,1.,1.,1.,1.,1.,1.,
1.,1.,1.,1.,1.,1.))
REPRESENTATION_ITEM('')
);
#387=(
BOUNDED_CURVE()
B_SPLINE_CURVE(5,(#53720,#53721,#53722,#53723,#53724,#53725,#53726,#53727,
#53728,#53729,#53730,#53731,#53732,#53733,#53734,#53735,#53736,#53737,#53738,
#53739,#53740,#53741,#53742,#53743,#53744,#53745,#53746,#53747,#53748,#53749,
#53750,#53751,#53752,#53753,#53754,#53755,#53756,#53757,#53758,#53759,#53760,
#53761,#53762,#53763,#53764,#53765,#53766,#53767,#53768,#53769,#53770,#53771,
#53772,#53773,#53774,#53775,#53776,#53777,#53778,#53779,#53780,#53781,#53782,
#53783,#53784,#53785,#53786,#53787,#53788,#53789),.UNSPECIFIED.,.F.,.F.)
B_SPLINE_CURVE_WITH_KNOTS((6,1,1,1,1,1,1,1,1,1,1,1,1,1,1,1,1,1,1,1,1,1,
1,1,1,1,1,1,1,1,1,1,1,1,1,1,1,1,1,1,1,1,1,1,1,1,1,1,1,1,1,1,1,1,1,1,1,1,
1,1,1,1,1,1,1,6),(0.00577184337451611,0.0153846153846154,0.0307692307692308,
0.0461538461538462,0.0615384615384615,0.0769230769230769,0.0923076923076923,
0.107692307692308,0.123076923076923,0.138461538461538,0.153846153846154,
0.169230769230769,0.184615384615385,0.2,0.215384615384615,0.230769230769231,
0.246153846153846,0.261538461538462,0.276923076923077,0.292307692307692,
0.307692307692308,0.323076923076923,0.338461538461538,0.353846153846154,
0.369230769230769,0.384615384615385,0.4,0.415384615384615,0.430769230769231,
0.446153846153846,0.461538461538462,0.476923076923077,0.492307692307692,
0.507692307692308,0.523076923076923,0.538461538461538,0.553846153846154,
0.569230769230769,0.584615384615384,0.6,0.615384615384615,0.63076923076923,
0.646153846153846,0.661538461538461,0.676923076923076,0.692307692307692,
0.707692307692307,0.723076923076922,0.738461538461538,0.753846153846153,
0.769230769230768,0.784615384615384,0.799999999999999,0.815384615384614,
0.83076923076923,0.846153846153845,0.86153846153846,0.876923076923076,0.892307692307691,
0.907692307692306,0.923076923076922,0.938461538461537,0.953846153846152,
0.969230769230768,0.984615384615383,1.),.UNSPECIFIED.)
CURVE()
GEOMETRIC_REPRESENTATION_ITEM()
RATIONAL_B_SPLINE_CURVE((1.,1.,1.,1.,1.,1.,1.,1.,1.,1.,1.,1.,1.,1.,1.,1.,
1.,1.,1.,1.,1.,1.,1.,1.,1.,1.,1.,1.,1.,1.,1.,1.,1.,1.,1.,1.,1.,1.,1.,1.,
1.,1.,1.,1.,1.,1.,1.,1.,1.,1.,1.,1.,1.,1.,1.,1.,1.,1.,1.,1.,1.,1.,1.,1.,
1.,1.,1.,1.,1.,1.))
REPRESENTATION_ITEM('')
);
#388=(
BOUNDED_CURVE()
B_SPLINE_CURVE(5,(#53793,#53794,#53795,#53796,#53797,#53798,#53799,#53800,
#53801,#53802,#53803,#53804,#53805,#53806,#53807,#53808,#53809,#53810,#53811,
#53812,#53813,#53814,#53815,#53816,#53817,#53818,#53819,#53820,#53821,#53822,
#53823,#53824,#53825,#53826,#53827,#53828,#53829,#53830,#53831,#53832,#53833,
#53834,#53835,#53836,#53837,#53838,#53839,#53840,#53841,#53842,#53843,#53844,
#53845,#53846,#53847,#53848,#53849,#53850,#53851,#53852,#53853,#53854,#53855,
#53856,#53857,#53858,#53859,#53860,#53861,#53862),.UNSPECIFIED.,.F.,.F.)
B_SPLINE_CURVE_WITH_KNOTS((6,1,1,1,1,1,1,1,1,1,1,1,1,1,1,1,1,1,1,1,1,1,
1,1,1,1,1,1,1,1,1,1,1,1,1,1,1,1,1,1,1,1,1,1,1,1,1,1,1,1,1,1,1,1,1,1,1,1,
1,1,1,1,1,1,1,6),(0.,0.0153846153846154,0.0307692307692308,0.0461538461538462,
0.0615384615384615,0.0769230769230769,0.0923076923076923,0.107692307692308,
0.123076923076923,0.138461538461538,0.153846153846154,0.169230769230769,
0.184615384615385,0.2,0.215384615384615,0.230769230769231,0.246153846153846,
0.261538461538462,0.276923076923077,0.292307692307692,0.307692307692308,
0.323076923076923,0.338461538461538,0.353846153846154,0.369230769230769,
0.384615384615385,0.4,0.415384615384615,0.430769230769231,0.446153846153846,
0.461538461538462,0.476923076923077,0.492307692307692,0.507692307692308,
0.523076923076923,0.538461538461538,0.553846153846154,0.569230769230769,
0.584615384615384,0.6,0.615384615384615,0.63076923076923,0.646153846153846,
0.661538461538461,0.676923076923076,0.692307692307692,0.707692307692307,
0.723076923076922,0.738461538461538,0.753846153846153,0.769230769230768,
0.784615384615384,0.799999999999999,0.815384615384614,0.83076923076923,
0.846153846153845,0.86153846153846,0.876923076923076,0.892307692307691,
0.907692307692306,0.923076923076922,0.938461538461537,0.953846153846152,
0.969230769230768,0.984615384615383,0.994228156739704),.UNSPECIFIED.)
CURVE()
GEOMETRIC_REPRESENTATION_ITEM()
RATIONAL_B_SPLINE_CURVE((1.,1.,1.,1.,1.,1.,1.,1.,1.,1.,1.,1.,1.,1.,1.,1.,
1.,1.,1.,1.,1.,1.,1.,1.,1.,1.,1.,1.,1.,1.,1.,1.,1.,1.,1.,1.,1.,1.,1.,1.,
1.,1.,1.,1.,1.,1.,1.,1.,1.,1.,1.,1.,1.,1.,1.,1.,1.,1.,1.,1.,1.,1.,1.,1.,
1.,1.,1.,1.,1.,1.))
REPRESENTATION_ITEM('')
);
#389=(
BOUNDED_CURVE()
B_SPLINE_CURVE(5,(#53866,#53867,#53868,#53869,#53870,#53871,#53872,#53873,
#53874,#53875,#53876,#53877,#53878,#53879,#53880,#53881,#53882,#53883,#53884,
#53885,#53886,#53887,#53888,#53889,#53890,#53891,#53892,#53893,#53894,#53895,
#53896,#53897,#53898,#53899,#53900,#53901,#53902,#53903,#53904,#53905,#53906,
#53907,#53908,#53909,#53910,#53911,#53912,#53913,#53914,#53915,#53916,#53917,
#53918,#53919,#53920,#53921,#53922,#53923,#53924,#53925,#53926,#53927,#53928,
#53929,#53930,#53931,#53932,#53933,#53934,#53935),.UNSPECIFIED.,.F.,.F.)
B_SPLINE_CURVE_WITH_KNOTS((6,1,1,1,1,1,1,1,1,1,1,1,1,1,1,1,1,1,1,1,1,1,
1,1,1,1,1,1,1,1,1,1,1,1,1,1,1,1,1,1,1,1,1,1,1,1,1,1,1,1,1,1,1,1,1,1,1,1,
1,1,1,1,1,1,1,6),(0.00577184337449682,0.0153846153846154,0.0307692307692308,
0.0461538461538462,0.0615384615384615,0.0769230769230769,0.0923076923076923,
0.107692307692308,0.123076923076923,0.138461538461538,0.153846153846154,
0.169230769230769,0.184615384615385,0.2,0.215384615384615,0.230769230769231,
0.246153846153846,0.261538461538462,0.276923076923077,0.292307692307692,
0.307692307692308,0.323076923076923,0.338461538461538,0.353846153846154,
0.369230769230769,0.384615384615385,0.4,0.415384615384615,0.430769230769231,
0.446153846153846,0.461538461538462,0.476923076923077,0.492307692307692,
0.507692307692308,0.523076923076923,0.538461538461538,0.553846153846154,
0.569230769230769,0.584615384615384,0.6,0.615384615384615,0.63076923076923,
0.646153846153846,0.661538461538461,0.676923076923076,0.692307692307692,
0.707692307692307,0.723076923076922,0.738461538461538,0.753846153846153,
0.769230769230768,0.784615384615384,0.799999999999999,0.815384615384614,
0.83076923076923,0.846153846153845,0.86153846153846,0.876923076923076,0.892307692307691,
0.907692307692306,0.923076923076922,0.938461538461537,0.953846153846152,
0.969230769230768,0.984615384615383,1.),.UNSPECIFIED.)
CURVE()
GEOMETRIC_REPRESENTATION_ITEM()
RATIONAL_B_SPLINE_CURVE((1.,1.,1.,1.,1.,1.,1.,1.,1.,1.,1.,1.,1.,1.,1.,1.,
1.,1.,1.,1.,1.,1.,1.,1.,1.,1.,1.,1.,1.,1.,1.,1.,1.,1.,1.,1.,1.,1.,1.,1.,
1.,1.,1.,1.,1.,1.,1.,1.,1.,1.,1.,1.,1.,1.,1.,1.,1.,1.,1.,1.,1.,1.,1.,1.,
1.,1.,1.,1.,1.,1.))
REPRESENTATION_ITEM('')
);
#390=(
BOUNDED_CURVE()
B_SPLINE_CURVE(5,(#53939,#53940,#53941,#53942,#53943,#53944,#53945,#53946,
#53947,#53948,#53949,#53950,#53951,#53952,#53953,#53954,#53955,#53956,#53957,
#53958,#53959,#53960,#53961,#53962,#53963,#53964,#53965,#53966,#53967,#53968,
#53969,#53970,#53971,#53972,#53973,#53974,#53975,#53976,#53977,#53978,#53979,
#53980,#53981,#53982,#53983,#53984,#53985,#53986,#53987,#53988,#53989,#53990,
#53991,#53992,#53993,#53994,#53995,#53996,#53997,#53998,#53999,#54000,#54001,
#54002,#54003,#54004,#54005,#54006,#54007,#54008),.UNSPECIFIED.,.F.,.F.)
B_SPLINE_CURVE_WITH_KNOTS((6,1,1,1,1,1,1,1,1,1,1,1,1,1,1,1,1,1,1,1,1,1,
1,1,1,1,1,1,1,1,1,1,1,1,1,1,1,1,1,1,1,1,1,1,1,1,1,1,1,1,1,1,1,1,1,1,1,1,
1,1,1,1,1,1,1,6),(0.,0.0153846153846154,0.0307692307692308,0.0461538461538462,
0.0615384615384615,0.0769230769230769,0.0923076923076923,0.107692307692308,
0.123076923076923,0.138461538461538,0.153846153846154,0.169230769230769,
0.184615384615385,0.2,0.215384615384615,0.230769230769231,0.246153846153846,
0.261538461538462,0.276923076923077,0.292307692307692,0.307692307692308,
0.323076923076923,0.338461538461538,0.353846153846154,0.369230769230769,
0.384615384615385,0.4,0.415384615384615,0.430769230769231,0.446153846153846,
0.461538461538462,0.476923076923077,0.492307692307692,0.507692307692308,
0.523076923076923,0.538461538461538,0.553846153846154,0.569230769230769,
0.584615384615384,0.6,0.615384615384615,0.63076923076923,0.646153846153846,
0.661538461538461,0.676923076923076,0.692307692307692,0.707692307692307,
0.723076923076922,0.738461538461538,0.753846153846153,0.769230769230768,
0.784615384615384,0.799999999999999,0.815384615384614,0.83076923076923,
0.846153846153845,0.86153846153846,0.876923076923076,0.892307692307691,
0.907692307692306,0.923076923076922,0.938461538461537,0.953846153846152,
0.969230769230768,0.984615384615383,0.994228156739711),.UNSPECIFIED.)
CURVE()
GEOMETRIC_REPRESENTATION_ITEM()
RATIONAL_B_SPLINE_CURVE((1.,1.,1.,1.,1.,1.,1.,1.,1.,1.,1.,1.,1.,1.,1.,1.,
1.,1.,1.,1.,1.,1.,1.,1.,1.,1.,1.,1.,1.,1.,1.,1.,1.,1.,1.,1.,1.,1.,1.,1.,
1.,1.,1.,1.,1.,1.,1.,1.,1.,1.,1.,1.,1.,1.,1.,1.,1.,1.,1.,1.,1.,1.,1.,1.,
1.,1.,1.,1.,1.,1.))
REPRESENTATION_ITEM('')
);
#391=(
BOUNDED_CURVE()
B_SPLINE_CURVE(5,(#54012,#54013,#54014,#54015,#54016,#54017,#54018,#54019,
#54020,#54021,#54022,#54023,#54024,#54025,#54026,#54027,#54028,#54029,#54030,
#54031,#54032,#54033,#54034,#54035,#54036,#54037,#54038,#54039,#54040,#54041,
#54042,#54043,#54044,#54045,#54046,#54047,#54048,#54049,#54050,#54051,#54052,
#54053,#54054,#54055,#54056,#54057,#54058,#54059,#54060,#54061,#54062,#54063,
#54064,#54065,#54066,#54067,#54068,#54069,#54070,#54071,#54072,#54073,#54074,
#54075,#54076,#54077,#54078,#54079,#54080,#54081),.UNSPECIFIED.,.F.,.F.)
B_SPLINE_CURVE_WITH_KNOTS((6,1,1,1,1,1,1,1,1,1,1,1,1,1,1,1,1,1,1,1,1,1,
1,1,1,1,1,1,1,1,1,1,1,1,1,1,1,1,1,1,1,1,1,1,1,1,1,1,1,1,1,1,1,1,1,1,1,1,
1,1,1,1,1,1,1,6),(0.00577184337449159,0.0153846153846154,0.0307692307692308,
0.0461538461538462,0.0615384615384615,0.0769230769230769,0.0923076923076923,
0.107692307692308,0.123076923076923,0.138461538461538,0.153846153846154,
0.169230769230769,0.184615384615385,0.2,0.215384615384615,0.230769230769231,
0.246153846153846,0.261538461538462,0.276923076923077,0.292307692307692,
0.307692307692308,0.323076923076923,0.338461538461538,0.353846153846154,
0.369230769230769,0.384615384615385,0.4,0.415384615384615,0.430769230769231,
0.446153846153846,0.461538461538462,0.476923076923077,0.492307692307692,
0.507692307692308,0.523076923076923,0.538461538461538,0.553846153846154,
0.569230769230769,0.584615384615384,0.6,0.615384615384615,0.63076923076923,
0.646153846153846,0.661538461538461,0.676923076923076,0.692307692307692,
0.707692307692307,0.723076923076922,0.738461538461538,0.753846153846153,
0.769230769230768,0.784615384615384,0.799999999999999,0.815384615384614,
0.83076923076923,0.846153846153845,0.86153846153846,0.876923076923076,0.892307692307691,
0.907692307692306,0.923076923076922,0.938461538461537,0.953846153846152,
0.969230769230768,0.984615384615383,1.),.UNSPECIFIED.)
CURVE()
GEOMETRIC_REPRESENTATION_ITEM()
RATIONAL_B_SPLINE_CURVE((1.,1.,1.,1.,1.,1.,1.,1.,1.,1.,1.,1.,1.,1.,1.,1.,
1.,1.,1.,1.,1.,1.,1.,1.,1.,1.,1.,1.,1.,1.,1.,1.,1.,1.,1.,1.,1.,1.,1.,1.,
1.,1.,1.,1.,1.,1.,1.,1.,1.,1.,1.,1.,1.,1.,1.,1.,1.,1.,1.,1.,1.,1.,1.,1.,
1.,1.,1.,1.,1.,1.))
REPRESENTATION_ITEM('')
);
#392=(
BOUNDED_CURVE()
B_SPLINE_CURVE(5,(#54085,#54086,#54087,#54088,#54089,#54090,#54091,#54092,
#54093,#54094,#54095,#54096,#54097,#54098,#54099,#54100,#54101,#54102,#54103,
#54104,#54105,#54106,#54107,#54108,#54109,#54110,#54111,#54112,#54113,#54114,
#54115,#54116,#54117,#54118,#54119,#54120,#54121,#54122,#54123,#54124,#54125,
#54126,#54127,#54128,#54129,#54130,#54131,#54132,#54133,#54134,#54135,#54136,
#54137,#54138,#54139,#54140,#54141,#54142,#54143,#54144,#54145,#54146,#54147,
#54148,#54149,#54150,#54151,#54152,#54153,#54154),.UNSPECIFIED.,.F.,.F.)
B_SPLINE_CURVE_WITH_KNOTS((6,1,1,1,1,1,1,1,1,1,1,1,1,1,1,1,1,1,1,1,1,1,
1,1,1,1,1,1,1,1,1,1,1,1,1,1,1,1,1,1,1,1,1,1,1,1,1,1,1,1,1,1,1,1,1,1,1,1,
1,1,1,1,1,1,1,6),(0.,0.0153846153846154,0.0307692307692308,0.0461538461538462,
0.0615384615384615,0.0769230769230769,0.0923076923076923,0.107692307692308,
0.123076923076923,0.138461538461538,0.153846153846154,0.169230769230769,
0.184615384615385,0.2,0.215384615384615,0.230769230769231,0.246153846153846,
0.261538461538462,0.276923076923077,0.292307692307692,0.307692307692308,
0.323076923076923,0.338461538461538,0.353846153846154,0.369230769230769,
0.384615384615385,0.4,0.415384615384615,0.430769230769231,0.446153846153846,
0.461538461538462,0.476923076923077,0.492307692307692,0.507692307692308,
0.523076923076923,0.538461538461538,0.553846153846154,0.569230769230769,
0.584615384615384,0.6,0.615384615384615,0.63076923076923,0.646153846153846,
0.661538461538461,0.676923076923076,0.692307692307692,0.707692307692307,
0.723076923076922,0.738461538461538,0.753846153846153,0.769230769230768,
0.784615384615384,0.799999999999999,0.815384615384614,0.83076923076923,
0.846153846153845,0.86153846153846,0.876923076923076,0.892307692307691,
0.907692307692306,0.923076923076922,0.938461538461537,0.953846153846152,
0.969230769230768,0.984615384615383,0.994228156739723),.UNSPECIFIED.)
CURVE()
GEOMETRIC_REPRESENTATION_ITEM()
RATIONAL_B_SPLINE_CURVE((1.,1.,1.,1.,1.,1.,1.,1.,1.,1.,1.,1.,1.,1.,1.,1.,
1.,1.,1.,1.,1.,1.,1.,1.,1.,1.,1.,1.,1.,1.,1.,1.,1.,1.,1.,1.,1.,1.,1.,1.,
1.,1.,1.,1.,1.,1.,1.,1.,1.,1.,1.,1.,1.,1.,1.,1.,1.,1.,1.,1.,1.,1.,1.,1.,
1.,1.,1.,1.,1.,1.))
REPRESENTATION_ITEM('')
);
#393=(
BOUNDED_CURVE()
B_SPLINE_CURVE(5,(#54158,#54159,#54160,#54161,#54162,#54163,#54164,#54165,
#54166,#54167,#54168,#54169,#54170,#54171,#54172,#54173,#54174,#54175,#54176,
#54177,#54178,#54179,#54180,#54181,#54182,#54183,#54184,#54185,#54186,#54187,
#54188,#54189,#54190,#54191,#54192,#54193,#54194,#54195,#54196,#54197,#54198,
#54199,#54200,#54201,#54202,#54203,#54204,#54205,#54206,#54207,#54208,#54209,
#54210,#54211,#54212,#54213,#54214,#54215,#54216,#54217,#54218,#54219,#54220,
#54221,#54222,#54223,#54224,#54225,#54226,#54227),.UNSPECIFIED.,.F.,.F.)
B_SPLINE_CURVE_WITH_KNOTS((6,1,1,1,1,1,1,1,1,1,1,1,1,1,1,1,1,1,1,1,1,1,
1,1,1,1,1,1,1,1,1,1,1,1,1,1,1,1,1,1,1,1,1,1,1,1,1,1,1,1,1,1,1,1,1,1,1,1,
1,1,1,1,1,1,1,6),(0.00577184337450718,0.0153846153846154,0.0307692307692308,
0.0461538461538462,0.0615384615384615,0.0769230769230769,0.0923076923076923,
0.107692307692308,0.123076923076923,0.138461538461538,0.153846153846154,
0.169230769230769,0.184615384615385,0.2,0.215384615384615,0.230769230769231,
0.246153846153846,0.261538461538462,0.276923076923077,0.292307692307692,
0.307692307692308,0.323076923076923,0.338461538461538,0.353846153846154,
0.369230769230769,0.384615384615385,0.4,0.415384615384615,0.430769230769231,
0.446153846153846,0.461538461538462,0.476923076923077,0.492307692307692,
0.507692307692308,0.523076923076923,0.538461538461538,0.553846153846154,
0.569230769230769,0.584615384615384,0.6,0.615384615384615,0.63076923076923,
0.646153846153846,0.661538461538461,0.676923076923076,0.692307692307692,
0.707692307692307,0.723076923076922,0.738461538461538,0.753846153846153,
0.769230769230768,0.784615384615384,0.799999999999999,0.815384615384614,
0.83076923076923,0.846153846153845,0.86153846153846,0.876923076923076,0.892307692307691,
0.907692307692306,0.923076923076922,0.938461538461537,0.953846153846152,
0.969230769230768,0.984615384615383,1.),.UNSPECIFIED.)
CURVE()
GEOMETRIC_REPRESENTATION_ITEM()
RATIONAL_B_SPLINE_CURVE((1.,1.,1.,1.,1.,1.,1.,1.,1.,1.,1.,1.,1.,1.,1.,1.,
1.,1.,1.,1.,1.,1.,1.,1.,1.,1.,1.,1.,1.,1.,1.,1.,1.,1.,1.,1.,1.,1.,1.,1.,
1.,1.,1.,1.,1.,1.,1.,1.,1.,1.,1.,1.,1.,1.,1.,1.,1.,1.,1.,1.,1.,1.,1.,1.,
1.,1.,1.,1.,1.,1.))
REPRESENTATION_ITEM('')
);
#394=(
BOUNDED_CURVE()
B_SPLINE_CURVE(5,(#54231,#54232,#54233,#54234,#54235,#54236,#54237,#54238,
#54239,#54240,#54241,#54242,#54243,#54244,#54245,#54246,#54247,#54248,#54249,
#54250,#54251,#54252,#54253,#54254,#54255,#54256,#54257,#54258,#54259,#54260,
#54261,#54262,#54263,#54264,#54265,#54266,#54267,#54268,#54269,#54270,#54271,
#54272,#54273,#54274,#54275,#54276,#54277,#54278,#54279,#54280,#54281,#54282,
#54283,#54284,#54285,#54286,#54287,#54288,#54289,#54290,#54291,#54292,#54293,
#54294,#54295,#54296,#54297,#54298,#54299,#54300),.UNSPECIFIED.,.F.,.F.)
B_SPLINE_CURVE_WITH_KNOTS((6,1,1,1,1,1,1,1,1,1,1,1,1,1,1,1,1,1,1,1,1,1,
1,1,1,1,1,1,1,1,1,1,1,1,1,1,1,1,1,1,1,1,1,1,1,1,1,1,1,1,1,1,1,1,1,1,1,1,
1,1,1,1,1,1,1,6),(0.,0.0153846153846154,0.0307692307692308,0.0461538461538462,
0.0615384615384615,0.0769230769230769,0.0923076923076923,0.107692307692308,
0.123076923076923,0.138461538461538,0.153846153846154,0.169230769230769,
0.184615384615385,0.2,0.215384615384615,0.230769230769231,0.246153846153846,
0.261538461538462,0.276923076923077,0.292307692307692,0.307692307692308,
0.323076923076923,0.338461538461538,0.353846153846154,0.369230769230769,
0.384615384615385,0.4,0.415384615384615,0.430769230769231,0.446153846153846,
0.461538461538462,0.476923076923077,0.492307692307692,0.507692307692308,
0.523076923076923,0.538461538461538,0.553846153846154,0.569230769230769,
0.584615384615384,0.6,0.615384615384615,0.63076923076923,0.646153846153846,
0.661538461538461,0.676923076923076,0.692307692307692,0.707692307692307,
0.723076923076922,0.738461538461538,0.753846153846153,0.769230769230768,
0.784615384615384,0.799999999999999,0.815384615384614,0.83076923076923,
0.846153846153845,0.86153846153846,0.876923076923076,0.892307692307691,
0.907692307692306,0.923076923076922,0.938461538461537,0.953846153846152,
0.969230769230768,0.984615384615383,0.994228156739716),.UNSPECIFIED.)
CURVE()
GEOMETRIC_REPRESENTATION_ITEM()
RATIONAL_B_SPLINE_CURVE((1.,1.,1.,1.,1.,1.,1.,1.,1.,1.,1.,1.,1.,1.,1.,1.,
1.,1.,1.,1.,1.,1.,1.,1.,1.,1.,1.,1.,1.,1.,1.,1.,1.,1.,1.,1.,1.,1.,1.,1.,
1.,1.,1.,1.,1.,1.,1.,1.,1.,1.,1.,1.,1.,1.,1.,1.,1.,1.,1.,1.,1.,1.,1.,1.,
1.,1.,1.,1.,1.,1.))
REPRESENTATION_ITEM('')
);
#395=(
BOUNDED_CURVE()
B_SPLINE_CURVE(5,(#54304,#54305,#54306,#54307,#54308,#54309,#54310,#54311,
#54312,#54313,#54314,#54315,#54316,#54317,#54318,#54319,#54320,#54321,#54322,
#54323,#54324,#54325,#54326,#54327,#54328,#54329,#54330,#54331,#54332,#54333,
#54334,#54335,#54336,#54337,#54338,#54339,#54340,#54341,#54342,#54343,#54344,
#54345,#54346,#54347,#54348,#54349,#54350,#54351,#54352,#54353,#54354,#54355,
#54356,#54357,#54358,#54359,#54360,#54361,#54362,#54363,#54364,#54365,#54366,
#54367,#54368,#54369,#54370,#54371,#54372,#54373),.UNSPECIFIED.,.F.,.F.)
B_SPLINE_CURVE_WITH_KNOTS((6,1,1,1,1,1,1,1,1,1,1,1,1,1,1,1,1,1,1,1,1,1,
1,1,1,1,1,1,1,1,1,1,1,1,1,1,1,1,1,1,1,1,1,1,1,1,1,1,1,1,1,1,1,1,1,1,1,1,
1,1,1,1,1,1,1,6),(0.00577184337450174,0.0153846153846154,0.0307692307692308,
0.0461538461538462,0.0615384615384615,0.0769230769230769,0.0923076923076923,
0.107692307692308,0.123076923076923,0.138461538461538,0.153846153846154,
0.169230769230769,0.184615384615385,0.2,0.215384615384615,0.230769230769231,
0.246153846153846,0.261538461538462,0.276923076923077,0.292307692307692,
0.307692307692308,0.323076923076923,0.338461538461538,0.353846153846154,
0.369230769230769,0.384615384615385,0.4,0.415384615384615,0.430769230769231,
0.446153846153846,0.461538461538462,0.476923076923077,0.492307692307692,
0.507692307692308,0.523076923076923,0.538461538461538,0.553846153846154,
0.569230769230769,0.584615384615384,0.6,0.615384615384615,0.63076923076923,
0.646153846153846,0.661538461538461,0.676923076923076,0.692307692307692,
0.707692307692307,0.723076923076922,0.738461538461538,0.753846153846153,
0.769230769230768,0.784615384615384,0.799999999999999,0.815384615384614,
0.83076923076923,0.846153846153845,0.86153846153846,0.876923076923076,0.892307692307691,
0.907692307692306,0.923076923076922,0.938461538461537,0.953846153846152,
0.969230769230768,0.984615384615383,1.),.UNSPECIFIED.)
CURVE()
GEOMETRIC_REPRESENTATION_ITEM()
RATIONAL_B_SPLINE_CURVE((1.,1.,1.,1.,1.,1.,1.,1.,1.,1.,1.,1.,1.,1.,1.,1.,
1.,1.,1.,1.,1.,1.,1.,1.,1.,1.,1.,1.,1.,1.,1.,1.,1.,1.,1.,1.,1.,1.,1.,1.,
1.,1.,1.,1.,1.,1.,1.,1.,1.,1.,1.,1.,1.,1.,1.,1.,1.,1.,1.,1.,1.,1.,1.,1.,
1.,1.,1.,1.,1.,1.))
REPRESENTATION_ITEM('')
);
#396=(
BOUNDED_CURVE()
B_SPLINE_CURVE(5,(#54377,#54378,#54379,#54380,#54381,#54382,#54383,#54384,
#54385,#54386,#54387,#54388,#54389,#54390,#54391,#54392,#54393,#54394,#54395,
#54396,#54397,#54398,#54399,#54400,#54401,#54402,#54403,#54404,#54405,#54406,
#54407,#54408,#54409,#54410,#54411,#54412,#54413,#54414,#54415,#54416,#54417,
#54418,#54419,#54420,#54421,#54422,#54423,#54424,#54425,#54426,#54427,#54428,
#54429,#54430,#54431,#54432,#54433,#54434,#54435,#54436,#54437,#54438,#54439,
#54440,#54441,#54442,#54443,#54444,#54445,#54446),.UNSPECIFIED.,.F.,.F.)
B_SPLINE_CURVE_WITH_KNOTS((6,1,1,1,1,1,1,1,1,1,1,1,1,1,1,1,1,1,1,1,1,1,
1,1,1,1,1,1,1,1,1,1,1,1,1,1,1,1,1,1,1,1,1,1,1,1,1,1,1,1,1,1,1,1,1,1,1,1,
1,1,1,1,1,1,1,6),(0.,0.0153846153846154,0.0307692307692308,0.0461538461538462,
0.0615384615384615,0.0769230769230769,0.0923076923076923,0.107692307692308,
0.123076923076923,0.138461538461538,0.153846153846154,0.169230769230769,
0.184615384615385,0.2,0.215384615384615,0.230769230769231,0.246153846153846,
0.261538461538462,0.276923076923077,0.292307692307692,0.307692307692308,
0.323076923076923,0.338461538461538,0.353846153846154,0.369230769230769,
0.384615384615385,0.4,0.415384615384615,0.430769230769231,0.446153846153846,
0.461538461538462,0.476923076923077,0.492307692307692,0.507692307692308,
0.523076923076923,0.538461538461538,0.553846153846154,0.569230769230769,
0.584615384615384,0.6,0.615384615384615,0.63076923076923,0.646153846153846,
0.661538461538461,0.676923076923076,0.692307692307692,0.707692307692307,
0.723076923076922,0.738461538461538,0.753846153846153,0.769230769230768,
0.784615384615384,0.799999999999999,0.815384615384614,0.83076923076923,
0.846153846153845,0.86153846153846,0.876923076923076,0.892307692307691,
0.907692307692306,0.923076923076922,0.938461538461537,0.953846153846152,
0.969230769230768,0.984615384615383,0.994228156739722),.UNSPECIFIED.)
CURVE()
GEOMETRIC_REPRESENTATION_ITEM()
RATIONAL_B_SPLINE_CURVE((1.,1.,1.,1.,1.,1.,1.,1.,1.,1.,1.,1.,1.,1.,1.,1.,
1.,1.,1.,1.,1.,1.,1.,1.,1.,1.,1.,1.,1.,1.,1.,1.,1.,1.,1.,1.,1.,1.,1.,1.,
1.,1.,1.,1.,1.,1.,1.,1.,1.,1.,1.,1.,1.,1.,1.,1.,1.,1.,1.,1.,1.,1.,1.,1.,
1.,1.,1.,1.,1.,1.))
REPRESENTATION_ITEM('')
);
#397=(
BOUNDED_CURVE()
B_SPLINE_CURVE(5,(#54450,#54451,#54452,#54453,#54454,#54455,#54456,#54457,
#54458,#54459,#54460,#54461,#54462,#54463,#54464,#54465,#54466,#54467,#54468,
#54469,#54470,#54471,#54472,#54473,#54474,#54475,#54476,#54477,#54478,#54479,
#54480,#54481,#54482,#54483,#54484,#54485,#54486,#54487,#54488,#54489,#54490,
#54491,#54492,#54493,#54494,#54495,#54496,#54497,#54498,#54499,#54500,#54501,
#54502,#54503,#54504,#54505,#54506,#54507,#54508,#54509,#54510,#54511,#54512,
#54513,#54514,#54515,#54516,#54517,#54518,#54519),.UNSPECIFIED.,.F.,.F.)
B_SPLINE_CURVE_WITH_KNOTS((6,1,1,1,1,1,1,1,1,1,1,1,1,1,1,1,1,1,1,1,1,1,
1,1,1,1,1,1,1,1,1,1,1,1,1,1,1,1,1,1,1,1,1,1,1,1,1,1,1,1,1,1,1,1,1,1,1,1,
1,1,1,1,1,1,1,6),(0.00577184337450943,0.0153846153846154,0.0307692307692308,
0.0461538461538462,0.0615384615384615,0.0769230769230769,0.0923076923076923,
0.107692307692308,0.123076923076923,0.138461538461538,0.153846153846154,
0.169230769230769,0.184615384615385,0.2,0.215384615384615,0.230769230769231,
0.246153846153846,0.261538461538462,0.276923076923077,0.292307692307692,
0.307692307692308,0.323076923076923,0.338461538461538,0.353846153846154,
0.369230769230769,0.384615384615385,0.4,0.415384615384615,0.430769230769231,
0.446153846153846,0.461538461538462,0.476923076923077,0.492307692307692,
0.507692307692308,0.523076923076923,0.538461538461538,0.553846153846154,
0.569230769230769,0.584615384615384,0.6,0.615384615384615,0.63076923076923,
0.646153846153846,0.661538461538461,0.676923076923076,0.692307692307692,
0.707692307692307,0.723076923076922,0.738461538461538,0.753846153846153,
0.769230769230768,0.784615384615384,0.799999999999999,0.815384615384614,
0.83076923076923,0.846153846153845,0.86153846153846,0.876923076923076,0.892307692307691,
0.907692307692306,0.923076923076922,0.938461538461537,0.953846153846152,
0.969230769230768,0.984615384615383,1.),.UNSPECIFIED.)
CURVE()
GEOMETRIC_REPRESENTATION_ITEM()
RATIONAL_B_SPLINE_CURVE((1.,1.,1.,1.,1.,1.,1.,1.,1.,1.,1.,1.,1.,1.,1.,1.,
1.,1.,1.,1.,1.,1.,1.,1.,1.,1.,1.,1.,1.,1.,1.,1.,1.,1.,1.,1.,1.,1.,1.,1.,
1.,1.,1.,1.,1.,1.,1.,1.,1.,1.,1.,1.,1.,1.,1.,1.,1.,1.,1.,1.,1.,1.,1.,1.,
1.,1.,1.,1.,1.,1.))
REPRESENTATION_ITEM('')
);
#398=(
BOUNDED_CURVE()
B_SPLINE_CURVE(5,(#54523,#54524,#54525,#54526,#54527,#54528,#54529,#54530,
#54531,#54532,#54533,#54534,#54535,#54536,#54537,#54538,#54539,#54540,#54541,
#54542,#54543,#54544,#54545,#54546,#54547,#54548,#54549,#54550,#54551,#54552,
#54553,#54554,#54555,#54556,#54557,#54558,#54559,#54560,#54561,#54562,#54563,
#54564,#54565,#54566,#54567,#54568,#54569,#54570,#54571,#54572,#54573,#54574,
#54575,#54576,#54577,#54578,#54579,#54580,#54581,#54582,#54583,#54584,#54585,
#54586,#54587,#54588,#54589,#54590,#54591,#54592),.UNSPECIFIED.,.F.,.F.)
B_SPLINE_CURVE_WITH_KNOTS((6,1,1,1,1,1,1,1,1,1,1,1,1,1,1,1,1,1,1,1,1,1,
1,1,1,1,1,1,1,1,1,1,1,1,1,1,1,1,1,1,1,1,1,1,1,1,1,1,1,1,1,1,1,1,1,1,1,1,
1,1,1,1,1,1,1,6),(0.,0.0153846153846154,0.0307692307692308,0.0461538461538462,
0.0615384615384615,0.0769230769230769,0.0923076923076923,0.107692307692308,
0.123076923076923,0.138461538461538,0.153846153846154,0.169230769230769,
0.184615384615385,0.2,0.215384615384615,0.230769230769231,0.246153846153846,
0.261538461538462,0.276923076923077,0.292307692307692,0.307692307692308,
0.323076923076923,0.338461538461538,0.353846153846154,0.369230769230769,
0.384615384615385,0.4,0.415384615384615,0.430769230769231,0.446153846153846,
0.461538461538462,0.476923076923077,0.492307692307692,0.507692307692308,
0.523076923076923,0.538461538461538,0.553846153846154,0.569230769230769,
0.584615384615384,0.6,0.615384615384615,0.63076923076923,0.646153846153846,
0.661538461538461,0.676923076923076,0.692307692307692,0.707692307692307,
0.723076923076922,0.738461538461538,0.753846153846153,0.769230769230768,
0.784615384615384,0.799999999999999,0.815384615384614,0.83076923076923,
0.846153846153845,0.86153846153846,0.876923076923076,0.892307692307691,
0.907692307692306,0.923076923076922,0.938461538461537,0.953846153846152,
0.969230769230768,0.984615384615383,0.994228156739699),.UNSPECIFIED.)
CURVE()
GEOMETRIC_REPRESENTATION_ITEM()
RATIONAL_B_SPLINE_CURVE((1.,1.,1.,1.,1.,1.,1.,1.,1.,1.,1.,1.,1.,1.,1.,1.,
1.,1.,1.,1.,1.,1.,1.,1.,1.,1.,1.,1.,1.,1.,1.,1.,1.,1.,1.,1.,1.,1.,1.,1.,
1.,1.,1.,1.,1.,1.,1.,1.,1.,1.,1.,1.,1.,1.,1.,1.,1.,1.,1.,1.,1.,1.,1.,1.,
1.,1.,1.,1.,1.,1.))
REPRESENTATION_ITEM('')
);
#399=(
BOUNDED_CURVE()
B_SPLINE_CURVE(5,(#54596,#54597,#54598,#54599,#54600,#54601,#54602,#54603,
#54604,#54605,#54606,#54607,#54608,#54609,#54610,#54611,#54612,#54613,#54614,
#54615,#54616,#54617,#54618,#54619,#54620,#54621,#54622,#54623,#54624,#54625,
#54626,#54627,#54628,#54629,#54630,#54631,#54632,#54633,#54634,#54635,#54636,
#54637,#54638,#54639,#54640,#54641,#54642,#54643,#54644,#54645,#54646,#54647,
#54648,#54649,#54650,#54651,#54652,#54653,#54654,#54655,#54656,#54657,#54658,
#54659,#54660,#54661,#54662,#54663,#54664,#54665),.UNSPECIFIED.,.F.,.F.)
B_SPLINE_CURVE_WITH_KNOTS((6,1,1,1,1,1,1,1,1,1,1,1,1,1,1,1,1,1,1,1,1,1,
1,1,1,1,1,1,1,1,1,1,1,1,1,1,1,1,1,1,1,1,1,1,1,1,1,1,1,1,1,1,1,1,1,1,1,1,
1,1,1,1,1,1,1,6),(0.00577184337450665,0.0153846153846154,0.0307692307692308,
0.0461538461538462,0.0615384615384615,0.0769230769230769,0.0923076923076923,
0.107692307692308,0.123076923076923,0.138461538461538,0.153846153846154,
0.169230769230769,0.184615384615385,0.2,0.215384615384615,0.230769230769231,
0.246153846153846,0.261538461538462,0.276923076923077,0.292307692307692,
0.307692307692308,0.323076923076923,0.338461538461538,0.353846153846154,
0.369230769230769,0.384615384615385,0.4,0.415384615384615,0.430769230769231,
0.446153846153846,0.461538461538462,0.476923076923077,0.492307692307692,
0.507692307692308,0.523076923076923,0.538461538461538,0.553846153846154,
0.569230769230769,0.584615384615384,0.6,0.615384615384615,0.63076923076923,
0.646153846153846,0.661538461538461,0.676923076923076,0.692307692307692,
0.707692307692307,0.723076923076922,0.738461538461538,0.753846153846153,
0.769230769230768,0.784615384615384,0.799999999999999,0.815384615384614,
0.83076923076923,0.846153846153845,0.86153846153846,0.876923076923076,0.892307692307691,
0.907692307692306,0.923076923076922,0.938461538461537,0.953846153846152,
0.969230769230768,0.984615384615383,1.),.UNSPECIFIED.)
CURVE()
GEOMETRIC_REPRESENTATION_ITEM()
RATIONAL_B_SPLINE_CURVE((1.,1.,1.,1.,1.,1.,1.,1.,1.,1.,1.,1.,1.,1.,1.,1.,
1.,1.,1.,1.,1.,1.,1.,1.,1.,1.,1.,1.,1.,1.,1.,1.,1.,1.,1.,1.,1.,1.,1.,1.,
1.,1.,1.,1.,1.,1.,1.,1.,1.,1.,1.,1.,1.,1.,1.,1.,1.,1.,1.,1.,1.,1.,1.,1.,
1.,1.,1.,1.,1.,1.))
REPRESENTATION_ITEM('')
);
#400=(
BOUNDED_CURVE()
B_SPLINE_CURVE(5,(#54669,#54670,#54671,#54672,#54673,#54674,#54675,#54676,
#54677,#54678,#54679,#54680,#54681,#54682,#54683,#54684,#54685,#54686,#54687,
#54688,#54689,#54690,#54691,#54692,#54693,#54694,#54695,#54696,#54697,#54698,
#54699,#54700,#54701,#54702,#54703,#54704,#54705,#54706,#54707,#54708,#54709,
#54710,#54711,#54712,#54713,#54714,#54715,#54716,#54717,#54718,#54719,#54720,
#54721,#54722,#54723,#54724,#54725,#54726,#54727,#54728,#54729,#54730,#54731,
#54732,#54733,#54734,#54735,#54736,#54737,#54738),.UNSPECIFIED.,.F.,.F.)
B_SPLINE_CURVE_WITH_KNOTS((6,1,1,1,1,1,1,1,1,1,1,1,1,1,1,1,1,1,1,1,1,1,
1,1,1,1,1,1,1,1,1,1,1,1,1,1,1,1,1,1,1,1,1,1,1,1,1,1,1,1,1,1,1,1,1,1,1,1,
1,1,1,1,1,1,1,6),(0.,0.0153846153846154,0.0307692307692308,0.0461538461538462,
0.0615384615384615,0.0769230769230769,0.0923076923076923,0.107692307692308,
0.123076923076923,0.138461538461538,0.153846153846154,0.169230769230769,
0.184615384615385,0.2,0.215384615384615,0.230769230769231,0.246153846153846,
0.261538461538462,0.276923076923077,0.292307692307692,0.307692307692308,
0.323076923076923,0.338461538461538,0.353846153846154,0.369230769230769,
0.384615384615385,0.4,0.415384615384615,0.430769230769231,0.446153846153846,
0.461538461538462,0.476923076923077,0.492307692307692,0.507692307692308,
0.523076923076923,0.538461538461538,0.553846153846154,0.569230769230769,
0.584615384615384,0.6,0.615384615384615,0.63076923076923,0.646153846153846,
0.661538461538461,0.676923076923076,0.692307692307692,0.707692307692307,
0.723076923076922,0.738461538461538,0.753846153846153,0.769230769230768,
0.784615384615384,0.799999999999999,0.815384615384614,0.83076923076923,
0.846153846153845,0.86153846153846,0.876923076923076,0.892307692307691,
0.907692307692306,0.923076923076922,0.938461538461537,0.953846153846152,
0.969230769230768,0.984615384615383,0.994228156739691),.UNSPECIFIED.)
CURVE()
GEOMETRIC_REPRESENTATION_ITEM()
RATIONAL_B_SPLINE_CURVE((1.,1.,1.,1.,1.,1.,1.,1.,1.,1.,1.,1.,1.,1.,1.,1.,
1.,1.,1.,1.,1.,1.,1.,1.,1.,1.,1.,1.,1.,1.,1.,1.,1.,1.,1.,1.,1.,1.,1.,1.,
1.,1.,1.,1.,1.,1.,1.,1.,1.,1.,1.,1.,1.,1.,1.,1.,1.,1.,1.,1.,1.,1.,1.,1.,
1.,1.,1.,1.,1.,1.))
REPRESENTATION_ITEM('')
);
#401=(
BOUNDED_CURVE()
B_SPLINE_CURVE(5,(#54742,#54743,#54744,#54745,#54746,#54747,#54748,#54749,
#54750,#54751,#54752,#54753,#54754,#54755,#54756,#54757,#54758,#54759,#54760,
#54761,#54762,#54763,#54764,#54765,#54766,#54767,#54768,#54769,#54770,#54771,
#54772,#54773,#54774,#54775,#54776,#54777,#54778,#54779,#54780,#54781,#54782,
#54783,#54784,#54785,#54786,#54787,#54788,#54789,#54790,#54791,#54792,#54793,
#54794,#54795,#54796,#54797,#54798,#54799,#54800,#54801,#54802,#54803,#54804,
#54805,#54806,#54807,#54808,#54809,#54810,#54811),.UNSPECIFIED.,.F.,.F.)
B_SPLINE_CURVE_WITH_KNOTS((6,1,1,1,1,1,1,1,1,1,1,1,1,1,1,1,1,1,1,1,1,1,
1,1,1,1,1,1,1,1,1,1,1,1,1,1,1,1,1,1,1,1,1,1,1,1,1,1,1,1,1,1,1,1,1,1,1,1,
1,1,1,1,1,1,1,6),(0.00577184337450785,0.0153846153846154,0.0307692307692308,
0.0461538461538462,0.0615384615384615,0.0769230769230769,0.0923076923076923,
0.107692307692308,0.123076923076923,0.138461538461538,0.153846153846154,
0.169230769230769,0.184615384615385,0.2,0.215384615384615,0.230769230769231,
0.246153846153846,0.261538461538462,0.276923076923077,0.292307692307692,
0.307692307692308,0.323076923076923,0.338461538461538,0.353846153846154,
0.369230769230769,0.384615384615385,0.4,0.415384615384615,0.430769230769231,
0.446153846153846,0.461538461538462,0.476923076923077,0.492307692307692,
0.507692307692308,0.523076923076923,0.538461538461538,0.553846153846154,
0.569230769230769,0.584615384615384,0.6,0.615384615384615,0.63076923076923,
0.646153846153846,0.661538461538461,0.676923076923076,0.692307692307692,
0.707692307692307,0.723076923076922,0.738461538461538,0.753846153846153,
0.769230769230768,0.784615384615384,0.799999999999999,0.815384615384614,
0.83076923076923,0.846153846153845,0.86153846153846,0.876923076923076,0.892307692307691,
0.907692307692306,0.923076923076922,0.938461538461537,0.953846153846152,
0.969230769230768,0.984615384615383,1.),.UNSPECIFIED.)
CURVE()
GEOMETRIC_REPRESENTATION_ITEM()
RATIONAL_B_SPLINE_CURVE((1.,1.,1.,1.,1.,1.,1.,1.,1.,1.,1.,1.,1.,1.,1.,1.,
1.,1.,1.,1.,1.,1.,1.,1.,1.,1.,1.,1.,1.,1.,1.,1.,1.,1.,1.,1.,1.,1.,1.,1.,
1.,1.,1.,1.,1.,1.,1.,1.,1.,1.,1.,1.,1.,1.,1.,1.,1.,1.,1.,1.,1.,1.,1.,1.,
1.,1.,1.,1.,1.,1.))
REPRESENTATION_ITEM('')
);
#402=(
BOUNDED_CURVE()
B_SPLINE_CURVE(5,(#54815,#54816,#54817,#54818,#54819,#54820,#54821,#54822,
#54823,#54824,#54825,#54826,#54827,#54828,#54829,#54830,#54831,#54832,#54833,
#54834,#54835,#54836,#54837,#54838,#54839,#54840,#54841,#54842,#54843,#54844,
#54845,#54846,#54847,#54848,#54849,#54850,#54851,#54852,#54853,#54854,#54855,
#54856,#54857,#54858,#54859,#54860,#54861,#54862,#54863,#54864,#54865,#54866,
#54867,#54868,#54869,#54870,#54871,#54872,#54873,#54874,#54875,#54876,#54877,
#54878,#54879,#54880,#54881,#54882,#54883,#54884),.UNSPECIFIED.,.F.,.F.)
B_SPLINE_CURVE_WITH_KNOTS((6,1,1,1,1,1,1,1,1,1,1,1,1,1,1,1,1,1,1,1,1,1,
1,1,1,1,1,1,1,1,1,1,1,1,1,1,1,1,1,1,1,1,1,1,1,1,1,1,1,1,1,1,1,1,1,1,1,1,
1,1,1,1,1,1,1,6),(0.,0.0153846153846154,0.0307692307692308,0.0461538461538462,
0.0615384615384615,0.0769230769230769,0.0923076923076923,0.107692307692308,
0.123076923076923,0.138461538461538,0.153846153846154,0.169230769230769,
0.184615384615385,0.2,0.215384615384615,0.230769230769231,0.246153846153846,
0.261538461538462,0.276923076923077,0.292307692307692,0.307692307692308,
0.323076923076923,0.338461538461538,0.353846153846154,0.369230769230769,
0.384615384615385,0.4,0.415384615384615,0.430769230769231,0.446153846153846,
0.461538461538462,0.476923076923077,0.492307692307692,0.507692307692308,
0.523076923076923,0.538461538461538,0.553846153846154,0.569230769230769,
0.584615384615384,0.6,0.615384615384615,0.63076923076923,0.646153846153846,
0.661538461538461,0.676923076923076,0.692307692307692,0.707692307692307,
0.723076923076922,0.738461538461538,0.753846153846153,0.769230769230768,
0.784615384615384,0.799999999999999,0.815384615384614,0.83076923076923,
0.846153846153845,0.86153846153846,0.876923076923076,0.892307692307691,
0.907692307692306,0.923076923076922,0.938461538461537,0.953846153846152,
0.969230769230768,0.984615384615383,0.994228156739708),.UNSPECIFIED.)
CURVE()
GEOMETRIC_REPRESENTATION_ITEM()
RATIONAL_B_SPLINE_CURVE((1.,1.,1.,1.,1.,1.,1.,1.,1.,1.,1.,1.,1.,1.,1.,1.,
1.,1.,1.,1.,1.,1.,1.,1.,1.,1.,1.,1.,1.,1.,1.,1.,1.,1.,1.,1.,1.,1.,1.,1.,
1.,1.,1.,1.,1.,1.,1.,1.,1.,1.,1.,1.,1.,1.,1.,1.,1.,1.,1.,1.,1.,1.,1.,1.,
1.,1.,1.,1.,1.,1.))
REPRESENTATION_ITEM('')
);
#403=(
BOUNDED_CURVE()
B_SPLINE_CURVE(5,(#54888,#54889,#54890,#54891,#54892,#54893,#54894,#54895,
#54896,#54897,#54898,#54899,#54900,#54901,#54902,#54903,#54904,#54905,#54906,
#54907,#54908,#54909,#54910,#54911,#54912,#54913,#54914,#54915,#54916,#54917,
#54918,#54919,#54920,#54921,#54922,#54923,#54924,#54925,#54926,#54927,#54928,
#54929,#54930,#54931,#54932,#54933,#54934,#54935,#54936,#54937,#54938,#54939,
#54940,#54941,#54942,#54943,#54944,#54945,#54946,#54947,#54948,#54949,#54950,
#54951,#54952,#54953,#54954,#54955,#54956,#54957),.UNSPECIFIED.,.F.,.F.)
B_SPLINE_CURVE_WITH_KNOTS((6,1,1,1,1,1,1,1,1,1,1,1,1,1,1,1,1,1,1,1,1,1,
1,1,1,1,1,1,1,1,1,1,1,1,1,1,1,1,1,1,1,1,1,1,1,1,1,1,1,1,1,1,1,1,1,1,1,1,
1,1,1,1,1,1,1,6),(0.00577184337450072,0.0153846153846154,0.0307692307692308,
0.0461538461538462,0.0615384615384615,0.0769230769230769,0.0923076923076923,
0.107692307692308,0.123076923076923,0.138461538461538,0.153846153846154,
0.169230769230769,0.184615384615385,0.2,0.215384615384615,0.230769230769231,
0.246153846153846,0.261538461538462,0.276923076923077,0.292307692307692,
0.307692307692308,0.323076923076923,0.338461538461538,0.353846153846154,
0.369230769230769,0.384615384615385,0.4,0.415384615384615,0.430769230769231,
0.446153846153846,0.461538461538462,0.476923076923077,0.492307692307692,
0.507692307692308,0.523076923076923,0.538461538461538,0.553846153846154,
0.569230769230769,0.584615384615384,0.6,0.615384615384615,0.63076923076923,
0.646153846153846,0.661538461538461,0.676923076923076,0.692307692307692,
0.707692307692307,0.723076923076922,0.738461538461538,0.753846153846153,
0.769230769230768,0.784615384615384,0.799999999999999,0.815384615384614,
0.83076923076923,0.846153846153845,0.86153846153846,0.876923076923076,0.892307692307691,
0.907692307692306,0.923076923076922,0.938461538461537,0.953846153846152,
0.969230769230768,0.984615384615383,1.),.UNSPECIFIED.)
CURVE()
GEOMETRIC_REPRESENTATION_ITEM()
RATIONAL_B_SPLINE_CURVE((1.,1.,1.,1.,1.,1.,1.,1.,1.,1.,1.,1.,1.,1.,1.,1.,
1.,1.,1.,1.,1.,1.,1.,1.,1.,1.,1.,1.,1.,1.,1.,1.,1.,1.,1.,1.,1.,1.,1.,1.,
1.,1.,1.,1.,1.,1.,1.,1.,1.,1.,1.,1.,1.,1.,1.,1.,1.,1.,1.,1.,1.,1.,1.,1.,
1.,1.,1.,1.,1.,1.))
REPRESENTATION_ITEM('')
);
#404=(
BOUNDED_CURVE()
B_SPLINE_CURVE(5,(#54961,#54962,#54963,#54964,#54965,#54966,#54967,#54968,
#54969,#54970,#54971,#54972,#54973,#54974,#54975,#54976,#54977,#54978,#54979,
#54980,#54981,#54982,#54983,#54984,#54985,#54986,#54987,#54988,#54989,#54990,
#54991,#54992,#54993,#54994,#54995,#54996,#54997,#54998,#54999,#55000,#55001,
#55002,#55003,#55004,#55005,#55006,#55007,#55008,#55009,#55010,#55011,#55012,
#55013,#55014,#55015,#55016,#55017,#55018,#55019,#55020,#55021,#55022,#55023,
#55024,#55025,#55026,#55027,#55028,#55029,#55030),.UNSPECIFIED.,.F.,.F.)
B_SPLINE_CURVE_WITH_KNOTS((6,1,1,1,1,1,1,1,1,1,1,1,1,1,1,1,1,1,1,1,1,1,
1,1,1,1,1,1,1,1,1,1,1,1,1,1,1,1,1,1,1,1,1,1,1,1,1,1,1,1,1,1,1,1,1,1,1,1,
1,1,1,1,1,1,1,6),(0.,0.0153846153846154,0.0307692307692308,0.0461538461538462,
0.0615384615384615,0.0769230769230769,0.0923076923076923,0.107692307692308,
0.123076923076923,0.138461538461538,0.153846153846154,0.169230769230769,
0.184615384615385,0.2,0.215384615384615,0.230769230769231,0.246153846153846,
0.261538461538462,0.276923076923077,0.292307692307692,0.307692307692308,
0.323076923076923,0.338461538461538,0.353846153846154,0.369230769230769,
0.384615384615385,0.4,0.415384615384615,0.430769230769231,0.446153846153846,
0.461538461538462,0.476923076923077,0.492307692307692,0.507692307692308,
0.523076923076923,0.538461538461538,0.553846153846154,0.569230769230769,
0.584615384615384,0.6,0.615384615384615,0.63076923076923,0.646153846153846,
0.661538461538461,0.676923076923076,0.692307692307692,0.707692307692307,
0.723076923076922,0.738461538461538,0.753846153846153,0.769230769230768,
0.784615384615384,0.799999999999999,0.815384615384614,0.83076923076923,
0.846153846153845,0.86153846153846,0.876923076923076,0.892307692307691,
0.907692307692306,0.923076923076922,0.938461538461537,0.953846153846152,
0.969230769230768,0.984615384615383,0.994228156739706),.UNSPECIFIED.)
CURVE()
GEOMETRIC_REPRESENTATION_ITEM()
RATIONAL_B_SPLINE_CURVE((1.,1.,1.,1.,1.,1.,1.,1.,1.,1.,1.,1.,1.,1.,1.,1.,
1.,1.,1.,1.,1.,1.,1.,1.,1.,1.,1.,1.,1.,1.,1.,1.,1.,1.,1.,1.,1.,1.,1.,1.,
1.,1.,1.,1.,1.,1.,1.,1.,1.,1.,1.,1.,1.,1.,1.,1.,1.,1.,1.,1.,1.,1.,1.,1.,
1.,1.,1.,1.,1.,1.))
REPRESENTATION_ITEM('')
);
#405=(
BOUNDED_CURVE()
B_SPLINE_CURVE(5,(#55034,#55035,#55036,#55037,#55038,#55039,#55040,#55041,
#55042,#55043,#55044,#55045,#55046,#55047,#55048,#55049,#55050,#55051,#55052,
#55053,#55054,#55055,#55056,#55057,#55058,#55059,#55060,#55061,#55062,#55063,
#55064,#55065,#55066,#55067,#55068,#55069,#55070,#55071,#55072,#55073,#55074,
#55075,#55076,#55077,#55078,#55079,#55080,#55081,#55082,#55083,#55084,#55085,
#55086,#55087,#55088,#55089,#55090,#55091,#55092,#55093,#55094,#55095,#55096,
#55097,#55098,#55099,#55100,#55101,#55102,#55103),.UNSPECIFIED.,.F.,.F.)
B_SPLINE_CURVE_WITH_KNOTS((6,1,1,1,1,1,1,1,1,1,1,1,1,1,1,1,1,1,1,1,1,1,
1,1,1,1,1,1,1,1,1,1,1,1,1,1,1,1,1,1,1,1,1,1,1,1,1,1,1,1,1,1,1,1,1,1,1,1,
1,1,1,1,1,1,1,6),(0.00577184337450902,0.0153846153846154,0.0307692307692308,
0.0461538461538462,0.0615384615384615,0.0769230769230769,0.0923076923076923,
0.107692307692308,0.123076923076923,0.138461538461538,0.153846153846154,
0.169230769230769,0.184615384615385,0.2,0.215384615384615,0.230769230769231,
0.246153846153846,0.261538461538462,0.276923076923077,0.292307692307692,
0.307692307692308,0.323076923076923,0.338461538461538,0.353846153846154,
0.369230769230769,0.384615384615385,0.4,0.415384615384615,0.430769230769231,
0.446153846153846,0.461538461538462,0.476923076923077,0.492307692307692,
0.507692307692308,0.523076923076923,0.538461538461538,0.553846153846154,
0.569230769230769,0.584615384615384,0.6,0.615384615384615,0.63076923076923,
0.646153846153846,0.661538461538461,0.676923076923076,0.692307692307692,
0.707692307692307,0.723076923076922,0.738461538461538,0.753846153846153,
0.769230769230768,0.784615384615384,0.799999999999999,0.815384615384614,
0.83076923076923,0.846153846153845,0.86153846153846,0.876923076923076,0.892307692307691,
0.907692307692306,0.923076923076922,0.938461538461537,0.953846153846152,
0.969230769230768,0.984615384615383,1.),.UNSPECIFIED.)
CURVE()
GEOMETRIC_REPRESENTATION_ITEM()
RATIONAL_B_SPLINE_CURVE((1.,1.,1.,1.,1.,1.,1.,1.,1.,1.,1.,1.,1.,1.,1.,1.,
1.,1.,1.,1.,1.,1.,1.,1.,1.,1.,1.,1.,1.,1.,1.,1.,1.,1.,1.,1.,1.,1.,1.,1.,
1.,1.,1.,1.,1.,1.,1.,1.,1.,1.,1.,1.,1.,1.,1.,1.,1.,1.,1.,1.,1.,1.,1.,1.,
1.,1.,1.,1.,1.,1.))
REPRESENTATION_ITEM('')
);
#406=(
BOUNDED_CURVE()
B_SPLINE_CURVE(5,(#55107,#55108,#55109,#55110,#55111,#55112,#55113,#55114,
#55115,#55116,#55117,#55118,#55119,#55120,#55121,#55122,#55123,#55124,#55125,
#55126,#55127,#55128,#55129,#55130,#55131,#55132,#55133,#55134,#55135,#55136,
#55137,#55138,#55139,#55140,#55141,#55142,#55143,#55144,#55145,#55146,#55147,
#55148,#55149,#55150,#55151,#55152,#55153,#55154,#55155,#55156,#55157,#55158,
#55159,#55160,#55161,#55162,#55163,#55164,#55165,#55166,#55167,#55168,#55169,
#55170,#55171,#55172,#55173,#55174,#55175,#55176),.UNSPECIFIED.,.F.,.F.)
B_SPLINE_CURVE_WITH_KNOTS((6,1,1,1,1,1,1,1,1,1,1,1,1,1,1,1,1,1,1,1,1,1,
1,1,1,1,1,1,1,1,1,1,1,1,1,1,1,1,1,1,1,1,1,1,1,1,1,1,1,1,1,1,1,1,1,1,1,1,
1,1,1,1,1,1,1,6),(0.,0.0153846153846154,0.0307692307692308,0.0461538461538462,
0.0615384615384615,0.0769230769230769,0.0923076923076923,0.107692307692308,
0.123076923076923,0.138461538461538,0.153846153846154,0.169230769230769,
0.184615384615385,0.2,0.215384615384615,0.230769230769231,0.246153846153846,
0.261538461538462,0.276923076923077,0.292307692307692,0.307692307692308,
0.323076923076923,0.338461538461538,0.353846153846154,0.369230769230769,
0.384615384615385,0.4,0.415384615384615,0.430769230769231,0.446153846153846,
0.461538461538462,0.476923076923077,0.492307692307692,0.507692307692308,
0.523076923076923,0.538461538461538,0.553846153846154,0.569230769230769,
0.584615384615384,0.6,0.615384615384615,0.63076923076923,0.646153846153846,
0.661538461538461,0.676923076923076,0.692307692307692,0.707692307692307,
0.723076923076922,0.738461538461538,0.753846153846153,0.769230769230768,
0.784615384615384,0.799999999999999,0.815384615384614,0.83076923076923,
0.846153846153845,0.86153846153846,0.876923076923076,0.892307692307691,
0.907692307692306,0.923076923076922,0.938461538461537,0.953846153846152,
0.969230769230768,0.984615384615383,0.994228156739698),.UNSPECIFIED.)
CURVE()
GEOMETRIC_REPRESENTATION_ITEM()
RATIONAL_B_SPLINE_CURVE((1.,1.,1.,1.,1.,1.,1.,1.,1.,1.,1.,1.,1.,1.,1.,1.,
1.,1.,1.,1.,1.,1.,1.,1.,1.,1.,1.,1.,1.,1.,1.,1.,1.,1.,1.,1.,1.,1.,1.,1.,
1.,1.,1.,1.,1.,1.,1.,1.,1.,1.,1.,1.,1.,1.,1.,1.,1.,1.,1.,1.,1.,1.,1.,1.,
1.,1.,1.,1.,1.,1.))
REPRESENTATION_ITEM('')
);
#407=(
BOUNDED_CURVE()
B_SPLINE_CURVE(5,(#55180,#55181,#55182,#55183,#55184,#55185,#55186,#55187,
#55188,#55189,#55190,#55191,#55192,#55193,#55194,#55195,#55196,#55197,#55198,
#55199,#55200,#55201,#55202,#55203,#55204,#55205,#55206,#55207,#55208,#55209,
#55210,#55211,#55212,#55213,#55214,#55215,#55216,#55217,#55218,#55219,#55220,
#55221,#55222,#55223,#55224,#55225,#55226,#55227,#55228,#55229,#55230,#55231,
#55232,#55233,#55234,#55235,#55236,#55237,#55238,#55239,#55240,#55241,#55242,
#55243,#55244,#55245,#55246,#55247,#55248,#55249),.UNSPECIFIED.,.F.,.F.)
B_SPLINE_CURVE_WITH_KNOTS((6,1,1,1,1,1,1,1,1,1,1,1,1,1,1,1,1,1,1,1,1,1,
1,1,1,1,1,1,1,1,1,1,1,1,1,1,1,1,1,1,1,1,1,1,1,1,1,1,1,1,1,1,1,1,1,1,1,1,
1,1,1,1,1,1,1,6),(0.00577184337451611,0.0153846153846154,0.0307692307692308,
0.0461538461538462,0.0615384615384615,0.0769230769230769,0.0923076923076923,
0.107692307692308,0.123076923076923,0.138461538461538,0.153846153846154,
0.169230769230769,0.184615384615385,0.2,0.215384615384615,0.230769230769231,
0.246153846153846,0.261538461538462,0.276923076923077,0.292307692307692,
0.307692307692308,0.323076923076923,0.338461538461538,0.353846153846154,
0.369230769230769,0.384615384615385,0.4,0.415384615384615,0.430769230769231,
0.446153846153846,0.461538461538462,0.476923076923077,0.492307692307692,
0.507692307692308,0.523076923076923,0.538461538461538,0.553846153846154,
0.569230769230769,0.584615384615384,0.6,0.615384615384615,0.63076923076923,
0.646153846153846,0.661538461538461,0.676923076923076,0.692307692307692,
0.707692307692307,0.723076923076922,0.738461538461538,0.753846153846153,
0.769230769230768,0.784615384615384,0.799999999999999,0.815384615384614,
0.83076923076923,0.846153846153845,0.86153846153846,0.876923076923076,0.892307692307691,
0.907692307692306,0.923076923076922,0.938461538461537,0.953846153846152,
0.969230769230768,0.984615384615383,1.),.UNSPECIFIED.)
CURVE()
GEOMETRIC_REPRESENTATION_ITEM()
RATIONAL_B_SPLINE_CURVE((1.,1.,1.,1.,1.,1.,1.,1.,1.,1.,1.,1.,1.,1.,1.,1.,
1.,1.,1.,1.,1.,1.,1.,1.,1.,1.,1.,1.,1.,1.,1.,1.,1.,1.,1.,1.,1.,1.,1.,1.,
1.,1.,1.,1.,1.,1.,1.,1.,1.,1.,1.,1.,1.,1.,1.,1.,1.,1.,1.,1.,1.,1.,1.,1.,
1.,1.,1.,1.,1.,1.))
REPRESENTATION_ITEM('')
);
#408=(
BOUNDED_CURVE()
B_SPLINE_CURVE(5,(#55253,#55254,#55255,#55256,#55257,#55258,#55259,#55260,
#55261,#55262,#55263,#55264,#55265,#55266,#55267,#55268,#55269,#55270,#55271,
#55272,#55273,#55274,#55275,#55276,#55277,#55278,#55279,#55280,#55281,#55282,
#55283,#55284,#55285,#55286,#55287,#55288,#55289,#55290,#55291,#55292,#55293,
#55294,#55295,#55296,#55297,#55298,#55299,#55300,#55301,#55302,#55303,#55304,
#55305,#55306,#55307,#55308,#55309,#55310,#55311,#55312,#55313,#55314,#55315,
#55316,#55317,#55318,#55319,#55320,#55321,#55322),.UNSPECIFIED.,.F.,.F.)
B_SPLINE_CURVE_WITH_KNOTS((6,1,1,1,1,1,1,1,1,1,1,1,1,1,1,1,1,1,1,1,1,1,
1,1,1,1,1,1,1,1,1,1,1,1,1,1,1,1,1,1,1,1,1,1,1,1,1,1,1,1,1,1,1,1,1,1,1,1,
1,1,1,1,1,1,1,6),(0.,0.0153846153846154,0.0307692307692308,0.0461538461538462,
0.0615384615384615,0.0769230769230769,0.0923076923076923,0.107692307692308,
0.123076923076923,0.138461538461538,0.153846153846154,0.169230769230769,
0.184615384615385,0.2,0.215384615384615,0.230769230769231,0.246153846153846,
0.261538461538462,0.276923076923077,0.292307692307692,0.307692307692308,
0.323076923076923,0.338461538461538,0.353846153846154,0.369230769230769,
0.384615384615385,0.4,0.415384615384615,0.430769230769231,0.446153846153846,
0.461538461538462,0.476923076923077,0.492307692307692,0.507692307692308,
0.523076923076923,0.538461538461538,0.553846153846154,0.569230769230769,
0.584615384615384,0.6,0.615384615384615,0.63076923076923,0.646153846153846,
0.661538461538461,0.676923076923076,0.692307692307692,0.707692307692307,
0.723076923076922,0.738461538461538,0.753846153846153,0.769230769230768,
0.784615384615384,0.799999999999999,0.815384615384614,0.83076923076923,
0.846153846153845,0.86153846153846,0.876923076923076,0.892307692307691,
0.907692307692306,0.923076923076922,0.938461538461537,0.953846153846152,
0.969230769230768,0.984615384615383,0.994228156739704),.UNSPECIFIED.)
CURVE()
GEOMETRIC_REPRESENTATION_ITEM()
RATIONAL_B_SPLINE_CURVE((1.,1.,1.,1.,1.,1.,1.,1.,1.,1.,1.,1.,1.,1.,1.,1.,
1.,1.,1.,1.,1.,1.,1.,1.,1.,1.,1.,1.,1.,1.,1.,1.,1.,1.,1.,1.,1.,1.,1.,1.,
1.,1.,1.,1.,1.,1.,1.,1.,1.,1.,1.,1.,1.,1.,1.,1.,1.,1.,1.,1.,1.,1.,1.,1.,
1.,1.,1.,1.,1.,1.))
REPRESENTATION_ITEM('')
);
#409=(
BOUNDED_CURVE()
B_SPLINE_CURVE(5,(#55326,#55327,#55328,#55329,#55330,#55331,#55332,#55333,
#55334,#55335,#55336,#55337,#55338,#55339,#55340,#55341,#55342,#55343,#55344,
#55345,#55346,#55347,#55348,#55349,#55350,#55351,#55352,#55353,#55354,#55355,
#55356,#55357,#55358,#55359,#55360,#55361,#55362,#55363,#55364,#55365,#55366,
#55367,#55368,#55369,#55370,#55371,#55372,#55373,#55374,#55375,#55376,#55377,
#55378,#55379,#55380,#55381,#55382,#55383,#55384,#55385,#55386,#55387,#55388,
#55389,#55390,#55391,#55392,#55393,#55394,#55395),.UNSPECIFIED.,.F.,.F.)
B_SPLINE_CURVE_WITH_KNOTS((6,1,1,1,1,1,1,1,1,1,1,1,1,1,1,1,1,1,1,1,1,1,
1,1,1,1,1,1,1,1,1,1,1,1,1,1,1,1,1,1,1,1,1,1,1,1,1,1,1,1,1,1,1,1,1,1,1,1,
1,1,1,1,1,1,1,6),(0.00577184337449692,0.0153846153846154,0.0307692307692308,
0.0461538461538462,0.0615384615384615,0.0769230769230769,0.0923076923076923,
0.107692307692308,0.123076923076923,0.138461538461538,0.153846153846154,
0.169230769230769,0.184615384615385,0.2,0.215384615384615,0.230769230769231,
0.246153846153846,0.261538461538462,0.276923076923077,0.292307692307692,
0.307692307692308,0.323076923076923,0.338461538461538,0.353846153846154,
0.369230769230769,0.384615384615385,0.4,0.415384615384615,0.430769230769231,
0.446153846153846,0.461538461538462,0.476923076923077,0.492307692307692,
0.507692307692308,0.523076923076923,0.538461538461538,0.553846153846154,
0.569230769230769,0.584615384615384,0.6,0.615384615384615,0.63076923076923,
0.646153846153846,0.661538461538461,0.676923076923076,0.692307692307692,
0.707692307692307,0.723076923076922,0.738461538461538,0.753846153846153,
0.769230769230768,0.784615384615384,0.799999999999999,0.815384615384614,
0.83076923076923,0.846153846153845,0.86153846153846,0.876923076923076,0.892307692307691,
0.907692307692306,0.923076923076922,0.938461538461537,0.953846153846152,
0.969230769230768,0.984615384615383,1.),.UNSPECIFIED.)
CURVE()
GEOMETRIC_REPRESENTATION_ITEM()
RATIONAL_B_SPLINE_CURVE((1.,1.,1.,1.,1.,1.,1.,1.,1.,1.,1.,1.,1.,1.,1.,1.,
1.,1.,1.,1.,1.,1.,1.,1.,1.,1.,1.,1.,1.,1.,1.,1.,1.,1.,1.,1.,1.,1.,1.,1.,
1.,1.,1.,1.,1.,1.,1.,1.,1.,1.,1.,1.,1.,1.,1.,1.,1.,1.,1.,1.,1.,1.,1.,1.,
1.,1.,1.,1.,1.,1.))
REPRESENTATION_ITEM('')
);
#410=(
BOUNDED_CURVE()
B_SPLINE_CURVE(5,(#55398,#55399,#55400,#55401,#55402,#55403,#55404,#55405,
#55406,#55407,#55408,#55409,#55410,#55411,#55412,#55413,#55414,#55415,#55416,
#55417,#55418,#55419,#55420,#55421,#55422,#55423,#55424,#55425,#55426,#55427,
#55428,#55429,#55430,#55431,#55432,#55433,#55434,#55435,#55436,#55437,#55438,
#55439,#55440,#55441,#55442,#55443,#55444,#55445,#55446,#55447,#55448,#55449,
#55450,#55451,#55452,#55453,#55454,#55455,#55456,#55457,#55458,#55459,#55460,
#55461,#55462,#55463,#55464,#55465,#55466,#55467),.UNSPECIFIED.,.F.,.F.)
B_SPLINE_CURVE_WITH_KNOTS((6,1,1,1,1,1,1,1,1,1,1,1,1,1,1,1,1,1,1,1,1,1,
1,1,1,1,1,1,1,1,1,1,1,1,1,1,1,1,1,1,1,1,1,1,1,1,1,1,1,1,1,1,1,1,1,1,1,1,
1,1,1,1,1,1,1,6),(0.,0.0153846153846154,0.0307692307692308,0.0461538461538462,
0.0615384615384615,0.0769230769230769,0.0923076923076923,0.107692307692308,
0.123076923076923,0.138461538461538,0.153846153846154,0.169230769230769,
0.184615384615385,0.2,0.215384615384615,0.230769230769231,0.246153846153846,
0.261538461538462,0.276923076923077,0.292307692307692,0.307692307692308,
0.323076923076923,0.338461538461538,0.353846153846154,0.369230769230769,
0.384615384615385,0.4,0.415384615384615,0.430769230769231,0.446153846153846,
0.461538461538462,0.476923076923077,0.492307692307692,0.507692307692308,
0.523076923076923,0.538461538461538,0.553846153846154,0.569230769230769,
0.584615384615384,0.6,0.615384615384615,0.63076923076923,0.646153846153846,
0.661538461538461,0.676923076923076,0.692307692307692,0.707692307692307,
0.723076923076922,0.738461538461538,0.753846153846153,0.769230769230768,
0.784615384615384,0.799999999999999,0.815384615384614,0.83076923076923,
0.846153846153845,0.86153846153846,0.876923076923076,0.892307692307691,
0.907692307692306,0.923076923076922,0.938461538461537,0.953846153846152,
0.969230769230768,0.984615384615383,0.994228156739723),.UNSPECIFIED.)
CURVE()
GEOMETRIC_REPRESENTATION_ITEM()
RATIONAL_B_SPLINE_CURVE((1.,1.,1.,1.,1.,1.,1.,1.,1.,1.,1.,1.,1.,1.,1.,1.,
1.,1.,1.,1.,1.,1.,1.,1.,1.,1.,1.,1.,1.,1.,1.,1.,1.,1.,1.,1.,1.,1.,1.,1.,
1.,1.,1.,1.,1.,1.,1.,1.,1.,1.,1.,1.,1.,1.,1.,1.,1.,1.,1.,1.,1.,1.,1.,1.,
1.,1.,1.,1.,1.,1.))
REPRESENTATION_ITEM('')
);
#411=(
BOUNDED_CURVE()
B_SPLINE_CURVE(5,(#55626,#55627,#55628,#55629,#55630,#55631,#55632,#55633,
#55634,#55635,#55636,#55637,#55638,#55639,#55640,#55641,#55642,#55643,#55644,
#55645,#55646,#55647,#55648,#55649,#55650,#55651,#55652,#55653,#55654,#55655,
#55656,#55657,#55658,#55659,#55660,#55661,#55662,#55663,#55664,#55665,#55666,
#55667,#55668,#55669,#55670,#55671,#55672,#55673,#55674,#55675,#55676,#55677,
#55678,#55679,#55680,#55681,#55682,#55683,#55684,#55685,#55686,#55687,#55688,
#55689,#55690,#55691,#55692,#55693,#55694,#55695),.UNSPECIFIED.,.F.,.F.)
B_SPLINE_CURVE_WITH_KNOTS((6,1,1,1,1,1,1,1,1,1,1,1,1,1,1,1,1,1,1,1,1,1,
1,1,1,1,1,1,1,1,1,1,1,1,1,1,1,1,1,1,1,1,1,1,1,1,1,1,1,1,1,1,1,1,1,1,1,1,
1,1,1,1,1,1,1,6),(-1.,-0.984615384615383,-0.969230769230768,-0.953846153846152,
-0.938461538461537,-0.923076923076922,-0.907692307692306,-0.892307692307691,
-0.876923076923076,-0.86153846153846,-0.846153846153845,-0.83076923076923,
-0.815384615384614,-0.799999999999999,-0.784615384615384,-0.769230769230768,
-0.753846153846153,-0.738461538461538,-0.723076923076922,-0.707692307692307,
-0.692307692307692,-0.676923076923076,-0.661538461538461,-0.646153846153846,
-0.63076923076923,-0.615384615384615,-0.6,-0.584615384615384,-0.569230769230769,
-0.553846153846154,-0.538461538461538,-0.523076923076923,-0.507692307692308,
-0.492307692307692,-0.476923076923077,-0.461538461538462,-0.446153846153846,
-0.430769230769231,-0.415384615384615,-0.4,-0.384615384615385,-0.369230769230769,
-0.353846153846154,-0.338461538461538,-0.323076923076923,-0.307692307692308,
-0.292307692307692,-0.276923076923077,-0.261538461538462,-0.246153846153846,
-0.230769230769231,-0.215384615384615,-0.2,-0.184615384615385,-0.169230769230769,
-0.153846153846154,-0.138461538461538,-0.123076923076923,-0.107692307692308,
-0.0923076923076923,-0.0769230769230769,-0.0615384615384615,-0.0461538461538462,
-0.0307692307692308,-0.0153846153846154,-0.00577184337448906),
 .UNSPECIFIED.)
CURVE()
GEOMETRIC_REPRESENTATION_ITEM()
RATIONAL_B_SPLINE_CURVE((1.,1.,1.,1.,1.,1.,1.,1.,1.,1.,1.,1.,1.,1.,1.,1.,
1.,1.,1.,1.,1.,1.,1.,1.,1.,1.,1.,1.,1.,1.,1.,1.,1.,1.,1.,1.,1.,1.,1.,1.,
1.,1.,1.,1.,1.,1.,1.,1.,1.,1.,1.,1.,1.,1.,1.,1.,1.,1.,1.,1.,1.,1.,1.,1.,
1.,1.,1.,1.,1.,1.))
REPRESENTATION_ITEM('')
);
#412=(
BOUNDED_CURVE()
B_SPLINE_CURVE(5,(#55846,#55847,#55848,#55849,#55850,#55851,#55852,#55853,
#55854,#55855,#55856,#55857,#55858,#55859,#55860,#55861,#55862,#55863,#55864,
#55865,#55866,#55867,#55868,#55869,#55870,#55871,#55872,#55873,#55874,#55875,
#55876,#55877,#55878,#55879,#55880,#55881,#55882,#55883,#55884,#55885,#55886,
#55887,#55888,#55889,#55890,#55891,#55892,#55893,#55894,#55895,#55896,#55897,
#55898,#55899,#55900,#55901,#55902,#55903,#55904,#55905,#55906,#55907,#55908,
#55909,#55910,#55911,#55912,#55913,#55914,#55915),.UNSPECIFIED.,.F.,.F.)
B_SPLINE_CURVE_WITH_KNOTS((6,1,1,1,1,1,1,1,1,1,1,1,1,1,1,1,1,1,1,1,1,1,
1,1,1,1,1,1,1,1,1,1,1,1,1,1,1,1,1,1,1,1,1,1,1,1,1,1,1,1,1,1,1,1,1,1,1,1,
1,1,1,1,1,1,1,6),(-0.994228156739728,-0.984615384615383,-0.969230769230768,
-0.953846153846152,-0.938461538461537,-0.923076923076922,-0.907692307692306,
-0.892307692307691,-0.876923076923076,-0.86153846153846,-0.846153846153845,
-0.83076923076923,-0.815384615384614,-0.799999999999999,-0.784615384615384,
-0.769230769230768,-0.753846153846153,-0.738461538461538,-0.723076923076922,
-0.707692307692307,-0.692307692307692,-0.676923076923076,-0.661538461538461,
-0.646153846153846,-0.63076923076923,-0.615384615384615,-0.6,-0.584615384615384,
-0.569230769230769,-0.553846153846154,-0.538461538461538,-0.523076923076923,
-0.507692307692308,-0.492307692307692,-0.476923076923077,-0.461538461538462,
-0.446153846153846,-0.430769230769231,-0.415384615384615,-0.4,-0.384615384615385,
-0.369230769230769,-0.353846153846154,-0.338461538461538,-0.323076923076923,
-0.307692307692308,-0.292307692307692,-0.276923076923077,-0.261538461538462,
-0.246153846153846,-0.230769230769231,-0.215384615384615,-0.2,-0.184615384615385,
-0.169230769230769,-0.153846153846154,-0.138461538461538,-0.123076923076923,
-0.107692307692308,-0.0923076923076923,-0.0769230769230769,-0.0615384615384615,
-0.0461538461538462,-0.0307692307692308,-0.0153846153846154,0.),
 .UNSPECIFIED.)
CURVE()
GEOMETRIC_REPRESENTATION_ITEM()
RATIONAL_B_SPLINE_CURVE((1.,1.,1.,1.,1.,1.,1.,1.,1.,1.,1.,1.,1.,1.,1.,1.,
1.,1.,1.,1.,1.,1.,1.,1.,1.,1.,1.,1.,1.,1.,1.,1.,1.,1.,1.,1.,1.,1.,1.,1.,
1.,1.,1.,1.,1.,1.,1.,1.,1.,1.,1.,1.,1.,1.,1.,1.,1.,1.,1.,1.,1.,1.,1.,1.,
1.,1.,1.,1.,1.,1.))
REPRESENTATION_ITEM('')
);
#413=(
BOUNDED_CURVE()
B_SPLINE_CURVE(5,(#56068,#56069,#56070,#56071,#56072,#56073,#56074,#56075,
#56076,#56077,#56078,#56079,#56080,#56081,#56082,#56083,#56084,#56085,#56086,
#56087,#56088,#56089,#56090,#56091,#56092,#56093,#56094,#56095,#56096,#56097,
#56098,#56099,#56100,#56101,#56102,#56103,#56104,#56105,#56106,#56107,#56108,
#56109,#56110,#56111,#56112,#56113,#56114,#56115,#56116,#56117,#56118,#56119,
#56120,#56121,#56122,#56123,#56124,#56125,#56126,#56127,#56128,#56129,#56130,
#56131,#56132,#56133,#56134,#56135,#56136,#56137),.UNSPECIFIED.,.F.,.F.)
B_SPLINE_CURVE_WITH_KNOTS((6,1,1,1,1,1,1,1,1,1,1,1,1,1,1,1,1,1,1,1,1,1,
1,1,1,1,1,1,1,1,1,1,1,1,1,1,1,1,1,1,1,1,1,1,1,1,1,1,1,1,1,1,1,1,1,1,1,1,
1,1,1,1,1,1,1,6),(-1.,-0.984615384615383,-0.969230769230768,-0.953846153846152,
-0.938461538461537,-0.923076923076922,-0.907692307692306,-0.892307692307691,
-0.876923076923076,-0.86153846153846,-0.846153846153845,-0.83076923076923,
-0.815384615384614,-0.799999999999999,-0.784615384615384,-0.769230769230768,
-0.753846153846153,-0.738461538461538,-0.723076923076922,-0.707692307692307,
-0.692307692307692,-0.676923076923076,-0.661538461538461,-0.646153846153846,
-0.63076923076923,-0.615384615384615,-0.6,-0.584615384615384,-0.569230769230769,
-0.553846153846154,-0.538461538461538,-0.523076923076923,-0.507692307692308,
-0.492307692307692,-0.476923076923077,-0.461538461538462,-0.446153846153846,
-0.430769230769231,-0.415384615384615,-0.4,-0.384615384615385,-0.369230769230769,
-0.353846153846154,-0.338461538461538,-0.323076923076923,-0.307692307692308,
-0.292307692307692,-0.276923076923077,-0.261538461538462,-0.246153846153846,
-0.230769230769231,-0.215384615384615,-0.2,-0.184615384615385,-0.169230769230769,
-0.153846153846154,-0.138461538461538,-0.123076923076923,-0.107692307692308,
-0.0923076923076923,-0.0769230769230769,-0.0615384615384615,-0.0461538461538462,
-0.0307692307692308,-0.0153846153846154,-0.0057718433744926),
 .UNSPECIFIED.)
CURVE()
GEOMETRIC_REPRESENTATION_ITEM()
RATIONAL_B_SPLINE_CURVE((1.,1.,1.,1.,1.,1.,1.,1.,1.,1.,1.,1.,1.,1.,1.,1.,
1.,1.,1.,1.,1.,1.,1.,1.,1.,1.,1.,1.,1.,1.,1.,1.,1.,1.,1.,1.,1.,1.,1.,1.,
1.,1.,1.,1.,1.,1.,1.,1.,1.,1.,1.,1.,1.,1.,1.,1.,1.,1.,1.,1.,1.,1.,1.,1.,
1.,1.,1.,1.,1.,1.))
REPRESENTATION_ITEM('')
);
#414=(
BOUNDED_CURVE()
B_SPLINE_CURVE(5,(#56288,#56289,#56290,#56291,#56292,#56293,#56294,#56295,
#56296,#56297,#56298,#56299,#56300,#56301,#56302,#56303,#56304,#56305,#56306,
#56307,#56308,#56309,#56310,#56311,#56312,#56313,#56314,#56315,#56316,#56317,
#56318,#56319,#56320,#56321,#56322,#56323,#56324,#56325,#56326,#56327,#56328,
#56329,#56330,#56331,#56332,#56333,#56334,#56335,#56336,#56337,#56338,#56339,
#56340,#56341,#56342,#56343,#56344,#56345,#56346,#56347,#56348,#56349,#56350,
#56351,#56352,#56353,#56354,#56355,#56356,#56357),.UNSPECIFIED.,.F.,.F.)
B_SPLINE_CURVE_WITH_KNOTS((6,1,1,1,1,1,1,1,1,1,1,1,1,1,1,1,1,1,1,1,1,1,
1,1,1,1,1,1,1,1,1,1,1,1,1,1,1,1,1,1,1,1,1,1,1,1,1,1,1,1,1,1,1,1,1,1,1,1,
1,1,1,1,1,1,1,6),(-0.994228156739718,-0.984615384615383,-0.969230769230768,
-0.953846153846152,-0.938461538461537,-0.923076923076922,-0.907692307692306,
-0.892307692307691,-0.876923076923076,-0.86153846153846,-0.846153846153845,
-0.83076923076923,-0.815384615384614,-0.799999999999999,-0.784615384615384,
-0.769230769230768,-0.753846153846153,-0.738461538461538,-0.723076923076922,
-0.707692307692307,-0.692307692307692,-0.676923076923076,-0.661538461538461,
-0.646153846153846,-0.63076923076923,-0.615384615384615,-0.6,-0.584615384615384,
-0.569230769230769,-0.553846153846154,-0.538461538461538,-0.523076923076923,
-0.507692307692308,-0.492307692307692,-0.476923076923077,-0.461538461538462,
-0.446153846153846,-0.430769230769231,-0.415384615384615,-0.4,-0.384615384615385,
-0.369230769230769,-0.353846153846154,-0.338461538461538,-0.323076923076923,
-0.307692307692308,-0.292307692307692,-0.276923076923077,-0.261538461538462,
-0.246153846153846,-0.230769230769231,-0.215384615384615,-0.2,-0.184615384615385,
-0.169230769230769,-0.153846153846154,-0.138461538461538,-0.123076923076923,
-0.107692307692308,-0.0923076923076923,-0.0769230769230769,-0.0615384615384615,
-0.0461538461538462,-0.0307692307692308,-0.0153846153846154,0.),
 .UNSPECIFIED.)
CURVE()
GEOMETRIC_REPRESENTATION_ITEM()
RATIONAL_B_SPLINE_CURVE((1.,1.,1.,1.,1.,1.,1.,1.,1.,1.,1.,1.,1.,1.,1.,1.,
1.,1.,1.,1.,1.,1.,1.,1.,1.,1.,1.,1.,1.,1.,1.,1.,1.,1.,1.,1.,1.,1.,1.,1.,
1.,1.,1.,1.,1.,1.,1.,1.,1.,1.,1.,1.,1.,1.,1.,1.,1.,1.,1.,1.,1.,1.,1.,1.,
1.,1.,1.,1.,1.,1.))
REPRESENTATION_ITEM('')
);
#415=(
BOUNDED_CURVE()
B_SPLINE_CURVE(5,(#56510,#56511,#56512,#56513,#56514,#56515,#56516,#56517,
#56518,#56519,#56520,#56521,#56522,#56523,#56524,#56525,#56526,#56527,#56528,
#56529,#56530,#56531,#56532,#56533,#56534,#56535,#56536,#56537,#56538,#56539,
#56540,#56541,#56542,#56543,#56544,#56545,#56546,#56547,#56548,#56549,#56550,
#56551,#56552,#56553,#56554,#56555,#56556,#56557,#56558,#56559,#56560,#56561,
#56562,#56563,#56564,#56565,#56566,#56567,#56568,#56569,#56570,#56571,#56572,
#56573,#56574,#56575,#56576,#56577,#56578,#56579),.UNSPECIFIED.,.F.,.F.)
B_SPLINE_CURVE_WITH_KNOTS((6,1,1,1,1,1,1,1,1,1,1,1,1,1,1,1,1,1,1,1,1,1,
1,1,1,1,1,1,1,1,1,1,1,1,1,1,1,1,1,1,1,1,1,1,1,1,1,1,1,1,1,1,1,1,1,1,1,1,
1,1,1,1,1,1,1,6),(-1.,-0.984615384615383,-0.969230769230768,-0.953846153846152,
-0.938461538461537,-0.923076923076922,-0.907692307692306,-0.892307692307691,
-0.876923076923076,-0.86153846153846,-0.846153846153845,-0.83076923076923,
-0.815384615384614,-0.799999999999999,-0.784615384615384,-0.769230769230768,
-0.753846153846153,-0.738461538461538,-0.723076923076922,-0.707692307692307,
-0.692307692307692,-0.676923076923076,-0.661538461538461,-0.646153846153846,
-0.63076923076923,-0.615384615384615,-0.6,-0.584615384615384,-0.569230769230769,
-0.553846153846154,-0.538461538461538,-0.523076923076923,-0.507692307692308,
-0.492307692307692,-0.476923076923077,-0.461538461538462,-0.446153846153846,
-0.430769230769231,-0.415384615384615,-0.4,-0.384615384615385,-0.369230769230769,
-0.353846153846154,-0.338461538461538,-0.323076923076923,-0.307692307692308,
-0.292307692307692,-0.276923076923077,-0.261538461538462,-0.246153846153846,
-0.230769230769231,-0.215384615384615,-0.2,-0.184615384615385,-0.169230769230769,
-0.153846153846154,-0.138461538461538,-0.123076923076923,-0.107692307692308,
-0.0923076923076923,-0.0769230769230769,-0.0615384615384615,-0.0461538461538462,
-0.0307692307692308,-0.0153846153846154,-0.00577184337449396),
 .UNSPECIFIED.)
CURVE()
GEOMETRIC_REPRESENTATION_ITEM()
RATIONAL_B_SPLINE_CURVE((1.,1.,1.,1.,1.,1.,1.,1.,1.,1.,1.,1.,1.,1.,1.,1.,
1.,1.,1.,1.,1.,1.,1.,1.,1.,1.,1.,1.,1.,1.,1.,1.,1.,1.,1.,1.,1.,1.,1.,1.,
1.,1.,1.,1.,1.,1.,1.,1.,1.,1.,1.,1.,1.,1.,1.,1.,1.,1.,1.,1.,1.,1.,1.,1.,
1.,1.,1.,1.,1.,1.))
REPRESENTATION_ITEM('')
);
#416=(
BOUNDED_CURVE()
B_SPLINE_CURVE(5,(#56730,#56731,#56732,#56733,#56734,#56735,#56736,#56737,
#56738,#56739,#56740,#56741,#56742,#56743,#56744,#56745,#56746,#56747,#56748,
#56749,#56750,#56751,#56752,#56753,#56754,#56755,#56756,#56757,#56758,#56759,
#56760,#56761,#56762,#56763,#56764,#56765,#56766,#56767,#56768,#56769,#56770,
#56771,#56772,#56773,#56774,#56775,#56776,#56777,#56778,#56779,#56780,#56781,
#56782,#56783,#56784,#56785,#56786,#56787,#56788,#56789,#56790,#56791,#56792,
#56793,#56794,#56795,#56796,#56797,#56798,#56799),.UNSPECIFIED.,.F.,.F.)
B_SPLINE_CURVE_WITH_KNOTS((6,1,1,1,1,1,1,1,1,1,1,1,1,1,1,1,1,1,1,1,1,1,
1,1,1,1,1,1,1,1,1,1,1,1,1,1,1,1,1,1,1,1,1,1,1,1,1,1,1,1,1,1,1,1,1,1,1,1,
1,1,1,1,1,1,1,6),(-0.994228156739702,-0.984615384615383,-0.969230769230768,
-0.953846153846152,-0.938461538461537,-0.923076923076922,-0.907692307692306,
-0.892307692307691,-0.876923076923076,-0.86153846153846,-0.846153846153845,
-0.83076923076923,-0.815384615384614,-0.799999999999999,-0.784615384615384,
-0.769230769230768,-0.753846153846153,-0.738461538461538,-0.723076923076922,
-0.707692307692307,-0.692307692307692,-0.676923076923076,-0.661538461538461,
-0.646153846153846,-0.63076923076923,-0.615384615384615,-0.6,-0.584615384615384,
-0.569230769230769,-0.553846153846154,-0.538461538461538,-0.523076923076923,
-0.507692307692308,-0.492307692307692,-0.476923076923077,-0.461538461538462,
-0.446153846153846,-0.430769230769231,-0.415384615384615,-0.4,-0.384615384615385,
-0.369230769230769,-0.353846153846154,-0.338461538461538,-0.323076923076923,
-0.307692307692308,-0.292307692307692,-0.276923076923077,-0.261538461538462,
-0.246153846153846,-0.230769230769231,-0.215384615384615,-0.2,-0.184615384615385,
-0.169230769230769,-0.153846153846154,-0.138461538461538,-0.123076923076923,
-0.107692307692308,-0.0923076923076923,-0.0769230769230769,-0.0615384615384615,
-0.0461538461538462,-0.0307692307692308,-0.0153846153846154,0.),
 .UNSPECIFIED.)
CURVE()
GEOMETRIC_REPRESENTATION_ITEM()
RATIONAL_B_SPLINE_CURVE((1.,1.,1.,1.,1.,1.,1.,1.,1.,1.,1.,1.,1.,1.,1.,1.,
1.,1.,1.,1.,1.,1.,1.,1.,1.,1.,1.,1.,1.,1.,1.,1.,1.,1.,1.,1.,1.,1.,1.,1.,
1.,1.,1.,1.,1.,1.,1.,1.,1.,1.,1.,1.,1.,1.,1.,1.,1.,1.,1.,1.,1.,1.,1.,1.,
1.,1.,1.,1.,1.,1.))
REPRESENTATION_ITEM('')
);
#417=(
BOUNDED_CURVE()
B_SPLINE_CURVE(5,(#56952,#56953,#56954,#56955,#56956,#56957,#56958,#56959,
#56960,#56961,#56962,#56963,#56964,#56965,#56966,#56967,#56968,#56969,#56970,
#56971,#56972,#56973,#56974,#56975,#56976,#56977,#56978,#56979,#56980,#56981,
#56982,#56983,#56984,#56985,#56986,#56987,#56988,#56989,#56990,#56991,#56992,
#56993,#56994,#56995,#56996,#56997,#56998,#56999,#57000,#57001,#57002,#57003,
#57004,#57005,#57006,#57007,#57008,#57009,#57010,#57011,#57012,#57013,#57014,
#57015,#57016,#57017,#57018,#57019,#57020,#57021),.UNSPECIFIED.,.F.,.F.)
B_SPLINE_CURVE_WITH_KNOTS((6,1,1,1,1,1,1,1,1,1,1,1,1,1,1,1,1,1,1,1,1,1,
1,1,1,1,1,1,1,1,1,1,1,1,1,1,1,1,1,1,1,1,1,1,1,1,1,1,1,1,1,1,1,1,1,1,1,1,
1,1,1,1,1,1,1,6),(-1.,-0.984615384615383,-0.969230769230768,-0.953846153846152,
-0.938461538461537,-0.923076923076922,-0.907692307692306,-0.892307692307691,
-0.876923076923076,-0.86153846153846,-0.846153846153845,-0.83076923076923,
-0.815384615384614,-0.799999999999999,-0.784615384615384,-0.769230769230768,
-0.753846153846153,-0.738461538461538,-0.723076923076922,-0.707692307692307,
-0.692307692307692,-0.676923076923076,-0.661538461538461,-0.646153846153846,
-0.63076923076923,-0.615384615384615,-0.6,-0.584615384615384,-0.569230769230769,
-0.553846153846154,-0.538461538461538,-0.523076923076923,-0.507692307692308,
-0.492307692307692,-0.476923076923077,-0.461538461538462,-0.446153846153846,
-0.430769230769231,-0.415384615384615,-0.4,-0.384615384615385,-0.369230769230769,
-0.353846153846154,-0.338461538461538,-0.323076923076923,-0.307692307692308,
-0.292307692307692,-0.276923076923077,-0.261538461538462,-0.246153846153846,
-0.230769230769231,-0.215384615384615,-0.2,-0.184615384615385,-0.169230769230769,
-0.153846153846154,-0.138461538461538,-0.123076923076923,-0.107692307692308,
-0.0923076923076923,-0.0769230769230769,-0.0615384615384615,-0.0461538461538462,
-0.0307692307692308,-0.0153846153846154,-0.00577184337450989),
 .UNSPECIFIED.)
CURVE()
GEOMETRIC_REPRESENTATION_ITEM()
RATIONAL_B_SPLINE_CURVE((1.,1.,1.,1.,1.,1.,1.,1.,1.,1.,1.,1.,1.,1.,1.,1.,
1.,1.,1.,1.,1.,1.,1.,1.,1.,1.,1.,1.,1.,1.,1.,1.,1.,1.,1.,1.,1.,1.,1.,1.,
1.,1.,1.,1.,1.,1.,1.,1.,1.,1.,1.,1.,1.,1.,1.,1.,1.,1.,1.,1.,1.,1.,1.,1.,
1.,1.,1.,1.,1.,1.))
REPRESENTATION_ITEM('')
);
#418=(
BOUNDED_CURVE()
B_SPLINE_CURVE(5,(#57172,#57173,#57174,#57175,#57176,#57177,#57178,#57179,
#57180,#57181,#57182,#57183,#57184,#57185,#57186,#57187,#57188,#57189,#57190,
#57191,#57192,#57193,#57194,#57195,#57196,#57197,#57198,#57199,#57200,#57201,
#57202,#57203,#57204,#57205,#57206,#57207,#57208,#57209,#57210,#57211,#57212,
#57213,#57214,#57215,#57216,#57217,#57218,#57219,#57220,#57221,#57222,#57223,
#57224,#57225,#57226,#57227,#57228,#57229,#57230,#57231,#57232,#57233,#57234,
#57235,#57236,#57237,#57238,#57239,#57240,#57241),.UNSPECIFIED.,.F.,.F.)
B_SPLINE_CURVE_WITH_KNOTS((6,1,1,1,1,1,1,1,1,1,1,1,1,1,1,1,1,1,1,1,1,1,
1,1,1,1,1,1,1,1,1,1,1,1,1,1,1,1,1,1,1,1,1,1,1,1,1,1,1,1,1,1,1,1,1,1,1,1,
1,1,1,1,1,1,1,6),(-0.994228156739736,-0.984615384615383,-0.969230769230768,
-0.953846153846152,-0.938461538461537,-0.923076923076922,-0.907692307692306,
-0.892307692307691,-0.876923076923076,-0.86153846153846,-0.846153846153845,
-0.83076923076923,-0.815384615384614,-0.799999999999999,-0.784615384615384,
-0.769230769230768,-0.753846153846153,-0.738461538461538,-0.723076923076922,
-0.707692307692307,-0.692307692307692,-0.676923076923076,-0.661538461538461,
-0.646153846153846,-0.63076923076923,-0.615384615384615,-0.6,-0.584615384615384,
-0.569230769230769,-0.553846153846154,-0.538461538461538,-0.523076923076923,
-0.507692307692308,-0.492307692307692,-0.476923076923077,-0.461538461538462,
-0.446153846153846,-0.430769230769231,-0.415384615384615,-0.4,-0.384615384615385,
-0.369230769230769,-0.353846153846154,-0.338461538461538,-0.323076923076923,
-0.307692307692308,-0.292307692307692,-0.276923076923077,-0.261538461538462,
-0.246153846153846,-0.230769230769231,-0.215384615384615,-0.2,-0.184615384615385,
-0.169230769230769,-0.153846153846154,-0.138461538461538,-0.123076923076923,
-0.107692307692308,-0.0923076923076923,-0.0769230769230769,-0.0615384615384615,
-0.0461538461538462,-0.0307692307692308,-0.0153846153846154,0.),
 .UNSPECIFIED.)
CURVE()
GEOMETRIC_REPRESENTATION_ITEM()
RATIONAL_B_SPLINE_CURVE((1.,1.,1.,1.,1.,1.,1.,1.,1.,1.,1.,1.,1.,1.,1.,1.,
1.,1.,1.,1.,1.,1.,1.,1.,1.,1.,1.,1.,1.,1.,1.,1.,1.,1.,1.,1.,1.,1.,1.,1.,
1.,1.,1.,1.,1.,1.,1.,1.,1.,1.,1.,1.,1.,1.,1.,1.,1.,1.,1.,1.,1.,1.,1.,1.,
1.,1.,1.,1.,1.,1.))
REPRESENTATION_ITEM('')
);
#419=(
BOUNDED_CURVE()
B_SPLINE_CURVE(5,(#57394,#57395,#57396,#57397,#57398,#57399,#57400,#57401,
#57402,#57403,#57404,#57405,#57406,#57407,#57408,#57409,#57410,#57411,#57412,
#57413,#57414,#57415,#57416,#57417,#57418,#57419,#57420,#57421,#57422,#57423,
#57424,#57425,#57426,#57427,#57428,#57429,#57430,#57431,#57432,#57433,#57434,
#57435,#57436,#57437,#57438,#57439,#57440,#57441,#57442,#57443,#57444,#57445,
#57446,#57447,#57448,#57449,#57450,#57451,#57452,#57453,#57454,#57455,#57456,
#57457,#57458,#57459,#57460,#57461,#57462,#57463),.UNSPECIFIED.,.F.,.F.)
B_SPLINE_CURVE_WITH_KNOTS((6,1,1,1,1,1,1,1,1,1,1,1,1,1,1,1,1,1,1,1,1,1,
1,1,1,1,1,1,1,1,1,1,1,1,1,1,1,1,1,1,1,1,1,1,1,1,1,1,1,1,1,1,1,1,1,1,1,1,
1,1,1,1,1,1,1,6),(-1.,-0.984615384615383,-0.969230769230768,-0.953846153846152,
-0.938461538461537,-0.923076923076922,-0.907692307692306,-0.892307692307691,
-0.876923076923076,-0.86153846153846,-0.846153846153845,-0.83076923076923,
-0.815384615384614,-0.799999999999999,-0.784615384615384,-0.769230769230768,
-0.753846153846153,-0.738461538461538,-0.723076923076922,-0.707692307692307,
-0.692307692307692,-0.676923076923076,-0.661538461538461,-0.646153846153846,
-0.63076923076923,-0.615384615384615,-0.6,-0.584615384615384,-0.569230769230769,
-0.553846153846154,-0.538461538461538,-0.523076923076923,-0.507692307692308,
-0.492307692307692,-0.476923076923077,-0.461538461538462,-0.446153846153846,
-0.430769230769231,-0.415384615384615,-0.4,-0.384615384615385,-0.369230769230769,
-0.353846153846154,-0.338461538461538,-0.323076923076923,-0.307692307692308,
-0.292307692307692,-0.276923076923077,-0.261538461538462,-0.246153846153846,
-0.230769230769231,-0.215384615384615,-0.2,-0.184615384615385,-0.169230769230769,
-0.153846153846154,-0.138461538461538,-0.123076923076923,-0.107692307692308,
-0.0923076923076923,-0.0769230769230769,-0.0615384615384615,-0.0461538461538462,
-0.0307692307692308,-0.0153846153846154,-0.00577184337452469),
 .UNSPECIFIED.)
CURVE()
GEOMETRIC_REPRESENTATION_ITEM()
RATIONAL_B_SPLINE_CURVE((1.,1.,1.,1.,1.,1.,1.,1.,1.,1.,1.,1.,1.,1.,1.,1.,
1.,1.,1.,1.,1.,1.,1.,1.,1.,1.,1.,1.,1.,1.,1.,1.,1.,1.,1.,1.,1.,1.,1.,1.,
1.,1.,1.,1.,1.,1.,1.,1.,1.,1.,1.,1.,1.,1.,1.,1.,1.,1.,1.,1.,1.,1.,1.,1.,
1.,1.,1.,1.,1.,1.))
REPRESENTATION_ITEM('')
);
#420=(
BOUNDED_CURVE()
B_SPLINE_CURVE(5,(#57614,#57615,#57616,#57617,#57618,#57619,#57620,#57621,
#57622,#57623,#57624,#57625,#57626,#57627,#57628,#57629,#57630,#57631,#57632,
#57633,#57634,#57635,#57636,#57637,#57638,#57639,#57640,#57641,#57642,#57643,
#57644,#57645,#57646,#57647,#57648,#57649,#57650,#57651,#57652,#57653,#57654,
#57655,#57656,#57657,#57658,#57659,#57660,#57661,#57662,#57663,#57664,#57665,
#57666,#57667,#57668,#57669,#57670,#57671,#57672,#57673,#57674,#57675,#57676,
#57677,#57678,#57679,#57680,#57681,#57682,#57683),.UNSPECIFIED.,.F.,.F.)
B_SPLINE_CURVE_WITH_KNOTS((6,1,1,1,1,1,1,1,1,1,1,1,1,1,1,1,1,1,1,1,1,1,
1,1,1,1,1,1,1,1,1,1,1,1,1,1,1,1,1,1,1,1,1,1,1,1,1,1,1,1,1,1,1,1,1,1,1,1,
1,1,1,1,1,1,1,6),(-0.994228156739717,-0.984615384615383,-0.969230769230768,
-0.953846153846152,-0.938461538461537,-0.923076923076922,-0.907692307692306,
-0.892307692307691,-0.876923076923076,-0.86153846153846,-0.846153846153845,
-0.83076923076923,-0.815384615384614,-0.799999999999999,-0.784615384615384,
-0.769230769230768,-0.753846153846153,-0.738461538461538,-0.723076923076922,
-0.707692307692307,-0.692307692307692,-0.676923076923076,-0.661538461538461,
-0.646153846153846,-0.63076923076923,-0.615384615384615,-0.6,-0.584615384615384,
-0.569230769230769,-0.553846153846154,-0.538461538461538,-0.523076923076923,
-0.507692307692308,-0.492307692307692,-0.476923076923077,-0.461538461538462,
-0.446153846153846,-0.430769230769231,-0.415384615384615,-0.4,-0.384615384615385,
-0.369230769230769,-0.353846153846154,-0.338461538461538,-0.323076923076923,
-0.307692307692308,-0.292307692307692,-0.276923076923077,-0.261538461538462,
-0.246153846153846,-0.230769230769231,-0.215384615384615,-0.2,-0.184615384615385,
-0.169230769230769,-0.153846153846154,-0.138461538461538,-0.123076923076923,
-0.107692307692308,-0.0923076923076923,-0.0769230769230769,-0.0615384615384615,
-0.0461538461538462,-0.0307692307692308,-0.0153846153846154,0.),
 .UNSPECIFIED.)
CURVE()
GEOMETRIC_REPRESENTATION_ITEM()
RATIONAL_B_SPLINE_CURVE((1.,1.,1.,1.,1.,1.,1.,1.,1.,1.,1.,1.,1.,1.,1.,1.,
1.,1.,1.,1.,1.,1.,1.,1.,1.,1.,1.,1.,1.,1.,1.,1.,1.,1.,1.,1.,1.,1.,1.,1.,
1.,1.,1.,1.,1.,1.,1.,1.,1.,1.,1.,1.,1.,1.,1.,1.,1.,1.,1.,1.,1.,1.,1.,1.,
1.,1.,1.,1.,1.,1.))
REPRESENTATION_ITEM('')
);
#421=(
BOUNDED_CURVE()
B_SPLINE_CURVE(5,(#57836,#57837,#57838,#57839,#57840,#57841,#57842,#57843,
#57844,#57845,#57846,#57847,#57848,#57849,#57850,#57851,#57852,#57853,#57854,
#57855,#57856,#57857,#57858,#57859,#57860,#57861,#57862,#57863,#57864,#57865,
#57866,#57867,#57868,#57869,#57870,#57871,#57872,#57873,#57874,#57875,#57876,
#57877,#57878,#57879,#57880,#57881,#57882,#57883,#57884,#57885,#57886,#57887,
#57888,#57889,#57890,#57891,#57892,#57893,#57894,#57895,#57896,#57897,#57898,
#57899,#57900,#57901,#57902,#57903,#57904,#57905),.UNSPECIFIED.,.F.,.F.)
B_SPLINE_CURVE_WITH_KNOTS((6,1,1,1,1,1,1,1,1,1,1,1,1,1,1,1,1,1,1,1,1,1,
1,1,1,1,1,1,1,1,1,1,1,1,1,1,1,1,1,1,1,1,1,1,1,1,1,1,1,1,1,1,1,1,1,1,1,1,
1,1,1,1,1,1,1,6),(-1.,-0.984615384615383,-0.969230769230768,-0.953846153846152,
-0.938461538461537,-0.923076923076922,-0.907692307692306,-0.892307692307691,
-0.876923076923076,-0.86153846153846,-0.846153846153845,-0.83076923076923,
-0.815384615384614,-0.799999999999999,-0.784615384615384,-0.769230769230768,
-0.753846153846153,-0.738461538461538,-0.723076923076922,-0.707692307692307,
-0.692307692307692,-0.676923076923076,-0.661538461538461,-0.646153846153846,
-0.63076923076923,-0.615384615384615,-0.6,-0.584615384615384,-0.569230769230769,
-0.553846153846154,-0.538461538461538,-0.523076923076923,-0.507692307692308,
-0.492307692307692,-0.476923076923077,-0.461538461538462,-0.446153846153846,
-0.430769230769231,-0.415384615384615,-0.4,-0.384615384615385,-0.369230769230769,
-0.353846153846154,-0.338461538461538,-0.323076923076923,-0.307692307692308,
-0.292307692307692,-0.276923076923077,-0.261538461538462,-0.246153846153846,
-0.230769230769231,-0.215384615384615,-0.2,-0.184615384615385,-0.169230769230769,
-0.153846153846154,-0.138461538461538,-0.123076923076923,-0.107692307692308,
-0.0923076923076923,-0.0769230769230769,-0.0615384615384615,-0.0461538461538462,
-0.0307692307692308,-0.0153846153846154,-0.00577184337453472),
 .UNSPECIFIED.)
CURVE()
GEOMETRIC_REPRESENTATION_ITEM()
RATIONAL_B_SPLINE_CURVE((1.,1.,1.,1.,1.,1.,1.,1.,1.,1.,1.,1.,1.,1.,1.,1.,
1.,1.,1.,1.,1.,1.,1.,1.,1.,1.,1.,1.,1.,1.,1.,1.,1.,1.,1.,1.,1.,1.,1.,1.,
1.,1.,1.,1.,1.,1.,1.,1.,1.,1.,1.,1.,1.,1.,1.,1.,1.,1.,1.,1.,1.,1.,1.,1.,
1.,1.,1.,1.,1.,1.))
REPRESENTATION_ITEM('')
);
#422=(
BOUNDED_CURVE()
B_SPLINE_CURVE(5,(#58056,#58057,#58058,#58059,#58060,#58061,#58062,#58063,
#58064,#58065,#58066,#58067,#58068,#58069,#58070,#58071,#58072,#58073,#58074,
#58075,#58076,#58077,#58078,#58079,#58080,#58081,#58082,#58083,#58084,#58085,
#58086,#58087,#58088,#58089,#58090,#58091,#58092,#58093,#58094,#58095,#58096,
#58097,#58098,#58099,#58100,#58101,#58102,#58103,#58104,#58105,#58106,#58107,
#58108,#58109,#58110,#58111,#58112,#58113,#58114,#58115,#58116,#58117,#58118,
#58119,#58120,#58121,#58122,#58123,#58124,#58125),.UNSPECIFIED.,.F.,.F.)
B_SPLINE_CURVE_WITH_KNOTS((6,1,1,1,1,1,1,1,1,1,1,1,1,1,1,1,1,1,1,1,1,1,
1,1,1,1,1,1,1,1,1,1,1,1,1,1,1,1,1,1,1,1,1,1,1,1,1,1,1,1,1,1,1,1,1,1,1,1,
1,1,1,1,1,1,1,6),(-0.994228156739652,-0.984615384615383,-0.969230769230768,
-0.953846153846152,-0.938461538461537,-0.923076923076922,-0.907692307692306,
-0.892307692307691,-0.876923076923076,-0.86153846153846,-0.846153846153845,
-0.83076923076923,-0.815384615384614,-0.799999999999999,-0.784615384615384,
-0.769230769230768,-0.753846153846153,-0.738461538461538,-0.723076923076922,
-0.707692307692307,-0.692307692307692,-0.676923076923076,-0.661538461538461,
-0.646153846153846,-0.63076923076923,-0.615384615384615,-0.6,-0.584615384615384,
-0.569230769230769,-0.553846153846154,-0.538461538461538,-0.523076923076923,
-0.507692307692308,-0.492307692307692,-0.476923076923077,-0.461538461538462,
-0.446153846153846,-0.430769230769231,-0.415384615384615,-0.4,-0.384615384615385,
-0.369230769230769,-0.353846153846154,-0.338461538461538,-0.323076923076923,
-0.307692307692308,-0.292307692307692,-0.276923076923077,-0.261538461538462,
-0.246153846153846,-0.230769230769231,-0.215384615384615,-0.2,-0.184615384615385,
-0.169230769230769,-0.153846153846154,-0.138461538461538,-0.123076923076923,
-0.107692307692308,-0.0923076923076923,-0.0769230769230769,-0.0615384615384615,
-0.0461538461538462,-0.0307692307692308,-0.0153846153846154,0.),
 .UNSPECIFIED.)
CURVE()
GEOMETRIC_REPRESENTATION_ITEM()
RATIONAL_B_SPLINE_CURVE((1.,1.,1.,1.,1.,1.,1.,1.,1.,1.,1.,1.,1.,1.,1.,1.,
1.,1.,1.,1.,1.,1.,1.,1.,1.,1.,1.,1.,1.,1.,1.,1.,1.,1.,1.,1.,1.,1.,1.,1.,
1.,1.,1.,1.,1.,1.,1.,1.,1.,1.,1.,1.,1.,1.,1.,1.,1.,1.,1.,1.,1.,1.,1.,1.,
1.,1.,1.,1.,1.,1.))
REPRESENTATION_ITEM('')
);
#423=(
BOUNDED_CURVE()
B_SPLINE_CURVE(5,(#58278,#58279,#58280,#58281,#58282,#58283,#58284,#58285,
#58286,#58287,#58288,#58289,#58290,#58291,#58292,#58293,#58294,#58295,#58296,
#58297,#58298,#58299,#58300,#58301,#58302,#58303,#58304,#58305,#58306,#58307,
#58308,#58309,#58310,#58311,#58312,#58313,#58314,#58315,#58316,#58317,#58318,
#58319,#58320,#58321,#58322,#58323,#58324,#58325,#58326,#58327,#58328,#58329,
#58330,#58331,#58332,#58333,#58334,#58335,#58336,#58337,#58338,#58339,#58340,
#58341,#58342,#58343,#58344,#58345,#58346,#58347),.UNSPECIFIED.,.F.,.F.)
B_SPLINE_CURVE_WITH_KNOTS((6,1,1,1,1,1,1,1,1,1,1,1,1,1,1,1,1,1,1,1,1,1,
1,1,1,1,1,1,1,1,1,1,1,1,1,1,1,1,1,1,1,1,1,1,1,1,1,1,1,1,1,1,1,1,1,1,1,1,
1,1,1,1,1,1,1,6),(-1.,-0.984615384615383,-0.969230769230768,-0.953846153846152,
-0.938461538461537,-0.923076923076922,-0.907692307692306,-0.892307692307691,
-0.876923076923076,-0.86153846153846,-0.846153846153845,-0.83076923076923,
-0.815384615384614,-0.799999999999999,-0.784615384615384,-0.769230769230768,
-0.753846153846153,-0.738461538461538,-0.723076923076922,-0.707692307692307,
-0.692307692307692,-0.676923076923076,-0.661538461538461,-0.646153846153846,
-0.63076923076923,-0.615384615384615,-0.6,-0.584615384615384,-0.569230769230769,
-0.553846153846154,-0.538461538461538,-0.523076923076923,-0.507692307692308,
-0.492307692307692,-0.476923076923077,-0.461538461538462,-0.446153846153846,
-0.430769230769231,-0.415384615384615,-0.4,-0.384615384615385,-0.369230769230769,
-0.353846153846154,-0.338461538461538,-0.323076923076923,-0.307692307692308,
-0.292307692307692,-0.276923076923077,-0.261538461538462,-0.246153846153846,
-0.230769230769231,-0.215384615384615,-0.2,-0.184615384615385,-0.169230769230769,
-0.153846153846154,-0.138461538461538,-0.123076923076923,-0.107692307692308,
-0.0923076923076923,-0.0769230769230769,-0.0615384615384615,-0.0461538461538462,
-0.0307692307692308,-0.0153846153846154,-0.00577184337450876),
 .UNSPECIFIED.)
CURVE()
GEOMETRIC_REPRESENTATION_ITEM()
RATIONAL_B_SPLINE_CURVE((1.,1.,1.,1.,1.,1.,1.,1.,1.,1.,1.,1.,1.,1.,1.,1.,
1.,1.,1.,1.,1.,1.,1.,1.,1.,1.,1.,1.,1.,1.,1.,1.,1.,1.,1.,1.,1.,1.,1.,1.,
1.,1.,1.,1.,1.,1.,1.,1.,1.,1.,1.,1.,1.,1.,1.,1.,1.,1.,1.,1.,1.,1.,1.,1.,
1.,1.,1.,1.,1.,1.))
REPRESENTATION_ITEM('')
);
#424=(
BOUNDED_CURVE()
B_SPLINE_CURVE(5,(#58498,#58499,#58500,#58501,#58502,#58503,#58504,#58505,
#58506,#58507,#58508,#58509,#58510,#58511,#58512,#58513,#58514,#58515,#58516,
#58517,#58518,#58519,#58520,#58521,#58522,#58523,#58524,#58525,#58526,#58527,
#58528,#58529,#58530,#58531,#58532,#58533,#58534,#58535,#58536,#58537,#58538,
#58539,#58540,#58541,#58542,#58543,#58544,#58545,#58546,#58547,#58548,#58549,
#58550,#58551,#58552,#58553,#58554,#58555,#58556,#58557,#58558,#58559,#58560,
#58561,#58562,#58563,#58564,#58565,#58566,#58567),.UNSPECIFIED.,.F.,.F.)
B_SPLINE_CURVE_WITH_KNOTS((6,1,1,1,1,1,1,1,1,1,1,1,1,1,1,1,1,1,1,1,1,1,
1,1,1,1,1,1,1,1,1,1,1,1,1,1,1,1,1,1,1,1,1,1,1,1,1,1,1,1,1,1,1,1,1,1,1,1,
1,1,1,1,1,1,1,6),(-0.994228156739683,-0.984615384615383,-0.969230769230768,
-0.953846153846152,-0.938461538461537,-0.923076923076922,-0.907692307692306,
-0.892307692307691,-0.876923076923076,-0.86153846153846,-0.846153846153845,
-0.83076923076923,-0.815384615384614,-0.799999999999999,-0.784615384615384,
-0.769230769230768,-0.753846153846153,-0.738461538461538,-0.723076923076922,
-0.707692307692307,-0.692307692307692,-0.676923076923076,-0.661538461538461,
-0.646153846153846,-0.63076923076923,-0.615384615384615,-0.6,-0.584615384615384,
-0.569230769230769,-0.553846153846154,-0.538461538461538,-0.523076923076923,
-0.507692307692308,-0.492307692307692,-0.476923076923077,-0.461538461538462,
-0.446153846153846,-0.430769230769231,-0.415384615384615,-0.4,-0.384615384615385,
-0.369230769230769,-0.353846153846154,-0.338461538461538,-0.323076923076923,
-0.307692307692308,-0.292307692307692,-0.276923076923077,-0.261538461538462,
-0.246153846153846,-0.230769230769231,-0.215384615384615,-0.2,-0.184615384615385,
-0.169230769230769,-0.153846153846154,-0.138461538461538,-0.123076923076923,
-0.107692307692308,-0.0923076923076923,-0.0769230769230769,-0.0615384615384615,
-0.0461538461538462,-0.0307692307692308,-0.0153846153846154,0.),
 .UNSPECIFIED.)
CURVE()
GEOMETRIC_REPRESENTATION_ITEM()
RATIONAL_B_SPLINE_CURVE((1.,1.,1.,1.,1.,1.,1.,1.,1.,1.,1.,1.,1.,1.,1.,1.,
1.,1.,1.,1.,1.,1.,1.,1.,1.,1.,1.,1.,1.,1.,1.,1.,1.,1.,1.,1.,1.,1.,1.,1.,
1.,1.,1.,1.,1.,1.,1.,1.,1.,1.,1.,1.,1.,1.,1.,1.,1.,1.,1.,1.,1.,1.,1.,1.,
1.,1.,1.,1.,1.,1.))
REPRESENTATION_ITEM('')
);
#425=(
BOUNDED_CURVE()
B_SPLINE_CURVE(5,(#58720,#58721,#58722,#58723,#58724,#58725,#58726,#58727,
#58728,#58729,#58730,#58731,#58732,#58733,#58734,#58735,#58736,#58737,#58738,
#58739,#58740,#58741,#58742,#58743,#58744,#58745,#58746,#58747,#58748,#58749,
#58750,#58751,#58752,#58753,#58754,#58755,#58756,#58757,#58758,#58759,#58760,
#58761,#58762,#58763,#58764,#58765,#58766,#58767,#58768,#58769,#58770,#58771,
#58772,#58773,#58774,#58775,#58776,#58777,#58778,#58779,#58780,#58781,#58782,
#58783,#58784,#58785,#58786,#58787,#58788,#58789),.UNSPECIFIED.,.F.,.F.)
B_SPLINE_CURVE_WITH_KNOTS((6,1,1,1,1,1,1,1,1,1,1,1,1,1,1,1,1,1,1,1,1,1,
1,1,1,1,1,1,1,1,1,1,1,1,1,1,1,1,1,1,1,1,1,1,1,1,1,1,1,1,1,1,1,1,1,1,1,1,
1,1,1,1,1,1,1,6),(-1.,-0.984615384615383,-0.969230769230768,-0.953846153846152,
-0.938461538461537,-0.923076923076922,-0.907692307692306,-0.892307692307691,
-0.876923076923076,-0.86153846153846,-0.846153846153845,-0.83076923076923,
-0.815384615384614,-0.799999999999999,-0.784615384615384,-0.769230769230768,
-0.753846153846153,-0.738461538461538,-0.723076923076922,-0.707692307692307,
-0.692307692307692,-0.676923076923076,-0.661538461538461,-0.646153846153846,
-0.63076923076923,-0.615384615384615,-0.6,-0.584615384615384,-0.569230769230769,
-0.553846153846154,-0.538461538461538,-0.523076923076923,-0.507692307692308,
-0.492307692307692,-0.476923076923077,-0.461538461538462,-0.446153846153846,
-0.430769230769231,-0.415384615384615,-0.4,-0.384615384615385,-0.369230769230769,
-0.353846153846154,-0.338461538461538,-0.323076923076923,-0.307692307692308,
-0.292307692307692,-0.276923076923077,-0.261538461538462,-0.246153846153846,
-0.230769230769231,-0.215384615384615,-0.2,-0.184615384615385,-0.169230769230769,
-0.153846153846154,-0.138461538461538,-0.123076923076923,-0.107692307692308,
-0.0923076923076923,-0.0769230769230769,-0.0615384615384615,-0.0461538461538462,
-0.0307692307692308,-0.0153846153846154,-0.00577184337450277),
 .UNSPECIFIED.)
CURVE()
GEOMETRIC_REPRESENTATION_ITEM()
RATIONAL_B_SPLINE_CURVE((1.,1.,1.,1.,1.,1.,1.,1.,1.,1.,1.,1.,1.,1.,1.,1.,
1.,1.,1.,1.,1.,1.,1.,1.,1.,1.,1.,1.,1.,1.,1.,1.,1.,1.,1.,1.,1.,1.,1.,1.,
1.,1.,1.,1.,1.,1.,1.,1.,1.,1.,1.,1.,1.,1.,1.,1.,1.,1.,1.,1.,1.,1.,1.,1.,
1.,1.,1.,1.,1.,1.))
REPRESENTATION_ITEM('')
);
#426=(
BOUNDED_CURVE()
B_SPLINE_CURVE(5,(#58940,#58941,#58942,#58943,#58944,#58945,#58946,#58947,
#58948,#58949,#58950,#58951,#58952,#58953,#58954,#58955,#58956,#58957,#58958,
#58959,#58960,#58961,#58962,#58963,#58964,#58965,#58966,#58967,#58968,#58969,
#58970,#58971,#58972,#58973,#58974,#58975,#58976,#58977,#58978,#58979,#58980,
#58981,#58982,#58983,#58984,#58985,#58986,#58987,#58988,#58989,#58990,#58991,
#58992,#58993,#58994,#58995,#58996,#58997,#58998,#58999,#59000,#59001,#59002,
#59003,#59004,#59005,#59006,#59007,#59008,#59009),.UNSPECIFIED.,.F.,.F.)
B_SPLINE_CURVE_WITH_KNOTS((6,1,1,1,1,1,1,1,1,1,1,1,1,1,1,1,1,1,1,1,1,1,
1,1,1,1,1,1,1,1,1,1,1,1,1,1,1,1,1,1,1,1,1,1,1,1,1,1,1,1,1,1,1,1,1,1,1,1,
1,1,1,1,1,1,1,6),(-0.994228156739689,-0.984615384615383,-0.969230769230768,
-0.953846153846152,-0.938461538461537,-0.923076923076922,-0.907692307692306,
-0.892307692307691,-0.876923076923076,-0.86153846153846,-0.846153846153845,
-0.83076923076923,-0.815384615384614,-0.799999999999999,-0.784615384615384,
-0.769230769230768,-0.753846153846153,-0.738461538461538,-0.723076923076922,
-0.707692307692307,-0.692307692307692,-0.676923076923076,-0.661538461538461,
-0.646153846153846,-0.63076923076923,-0.615384615384615,-0.6,-0.584615384615384,
-0.569230769230769,-0.553846153846154,-0.538461538461538,-0.523076923076923,
-0.507692307692308,-0.492307692307692,-0.476923076923077,-0.461538461538462,
-0.446153846153846,-0.430769230769231,-0.415384615384615,-0.4,-0.384615384615385,
-0.369230769230769,-0.353846153846154,-0.338461538461538,-0.323076923076923,
-0.307692307692308,-0.292307692307692,-0.276923076923077,-0.261538461538462,
-0.246153846153846,-0.230769230769231,-0.215384615384615,-0.2,-0.184615384615385,
-0.169230769230769,-0.153846153846154,-0.138461538461538,-0.123076923076923,
-0.107692307692308,-0.0923076923076923,-0.0769230769230769,-0.0615384615384615,
-0.0461538461538462,-0.0307692307692308,-0.0153846153846154,0.),
 .UNSPECIFIED.)
CURVE()
GEOMETRIC_REPRESENTATION_ITEM()
RATIONAL_B_SPLINE_CURVE((1.,1.,1.,1.,1.,1.,1.,1.,1.,1.,1.,1.,1.,1.,1.,1.,
1.,1.,1.,1.,1.,1.,1.,1.,1.,1.,1.,1.,1.,1.,1.,1.,1.,1.,1.,1.,1.,1.,1.,1.,
1.,1.,1.,1.,1.,1.,1.,1.,1.,1.,1.,1.,1.,1.,1.,1.,1.,1.,1.,1.,1.,1.,1.,1.,
1.,1.,1.,1.,1.,1.))
REPRESENTATION_ITEM('')
);
#427=(
BOUNDED_CURVE()
B_SPLINE_CURVE(5,(#59162,#59163,#59164,#59165,#59166,#59167,#59168,#59169,
#59170,#59171,#59172,#59173,#59174,#59175,#59176,#59177,#59178,#59179,#59180,
#59181,#59182,#59183,#59184,#59185,#59186,#59187,#59188,#59189,#59190,#59191,
#59192,#59193,#59194,#59195,#59196,#59197,#59198,#59199,#59200,#59201,#59202,
#59203,#59204,#59205,#59206,#59207,#59208,#59209,#59210,#59211,#59212,#59213,
#59214,#59215,#59216,#59217,#59218,#59219,#59220,#59221,#59222,#59223,#59224,
#59225,#59226,#59227,#59228,#59229,#59230,#59231),.UNSPECIFIED.,.F.,.F.)
B_SPLINE_CURVE_WITH_KNOTS((6,1,1,1,1,1,1,1,1,1,1,1,1,1,1,1,1,1,1,1,1,1,
1,1,1,1,1,1,1,1,1,1,1,1,1,1,1,1,1,1,1,1,1,1,1,1,1,1,1,1,1,1,1,1,1,1,1,1,
1,1,1,1,1,1,1,6),(-1.,-0.984615384615383,-0.969230769230768,-0.953846153846152,
-0.938461538461537,-0.923076923076922,-0.907692307692306,-0.892307692307691,
-0.876923076923076,-0.86153846153846,-0.846153846153845,-0.83076923076923,
-0.815384615384614,-0.799999999999999,-0.784615384615384,-0.769230769230768,
-0.753846153846153,-0.738461538461538,-0.723076923076922,-0.707692307692307,
-0.692307692307692,-0.676923076923076,-0.661538461538461,-0.646153846153846,
-0.63076923076923,-0.615384615384615,-0.6,-0.584615384615384,-0.569230769230769,
-0.553846153846154,-0.538461538461538,-0.523076923076923,-0.507692307692308,
-0.492307692307692,-0.476923076923077,-0.461538461538462,-0.446153846153846,
-0.430769230769231,-0.415384615384615,-0.4,-0.384615384615385,-0.369230769230769,
-0.353846153846154,-0.338461538461538,-0.323076923076923,-0.307692307692308,
-0.292307692307692,-0.276923076923077,-0.261538461538462,-0.246153846153846,
-0.230769230769231,-0.215384615384615,-0.2,-0.184615384615385,-0.169230769230769,
-0.153846153846154,-0.138461538461538,-0.123076923076923,-0.107692307692308,
-0.0923076923076923,-0.0769230769230769,-0.0615384615384615,-0.0461538461538462,
-0.0307692307692308,-0.0153846153846154,-0.00577184337451766),
 .UNSPECIFIED.)
CURVE()
GEOMETRIC_REPRESENTATION_ITEM()
RATIONAL_B_SPLINE_CURVE((1.,1.,1.,1.,1.,1.,1.,1.,1.,1.,1.,1.,1.,1.,1.,1.,
1.,1.,1.,1.,1.,1.,1.,1.,1.,1.,1.,1.,1.,1.,1.,1.,1.,1.,1.,1.,1.,1.,1.,1.,
1.,1.,1.,1.,1.,1.,1.,1.,1.,1.,1.,1.,1.,1.,1.,1.,1.,1.,1.,1.,1.,1.,1.,1.,
1.,1.,1.,1.,1.,1.))
REPRESENTATION_ITEM('')
);
#428=(
BOUNDED_CURVE()
B_SPLINE_CURVE(5,(#59382,#59383,#59384,#59385,#59386,#59387,#59388,#59389,
#59390,#59391,#59392,#59393,#59394,#59395,#59396,#59397,#59398,#59399,#59400,
#59401,#59402,#59403,#59404,#59405,#59406,#59407,#59408,#59409,#59410,#59411,
#59412,#59413,#59414,#59415,#59416,#59417,#59418,#59419,#59420,#59421,#59422,
#59423,#59424,#59425,#59426,#59427,#59428,#59429,#59430,#59431,#59432,#59433,
#59434,#59435,#59436,#59437,#59438,#59439,#59440,#59441,#59442,#59443,#59444,
#59445,#59446,#59447,#59448,#59449,#59450,#59451),.UNSPECIFIED.,.F.,.F.)
B_SPLINE_CURVE_WITH_KNOTS((6,1,1,1,1,1,1,1,1,1,1,1,1,1,1,1,1,1,1,1,1,1,
1,1,1,1,1,1,1,1,1,1,1,1,1,1,1,1,1,1,1,1,1,1,1,1,1,1,1,1,1,1,1,1,1,1,1,1,
1,1,1,1,1,1,1,6),(-0.994228156739687,-0.984615384615383,-0.969230769230768,
-0.953846153846152,-0.938461538461537,-0.923076923076922,-0.907692307692306,
-0.892307692307691,-0.876923076923076,-0.86153846153846,-0.846153846153845,
-0.83076923076923,-0.815384615384614,-0.799999999999999,-0.784615384615384,
-0.769230769230768,-0.753846153846153,-0.738461538461538,-0.723076923076922,
-0.707692307692307,-0.692307692307692,-0.676923076923076,-0.661538461538461,
-0.646153846153846,-0.63076923076923,-0.615384615384615,-0.6,-0.584615384615384,
-0.569230769230769,-0.553846153846154,-0.538461538461538,-0.523076923076923,
-0.507692307692308,-0.492307692307692,-0.476923076923077,-0.461538461538462,
-0.446153846153846,-0.430769230769231,-0.415384615384615,-0.4,-0.384615384615385,
-0.369230769230769,-0.353846153846154,-0.338461538461538,-0.323076923076923,
-0.307692307692308,-0.292307692307692,-0.276923076923077,-0.261538461538462,
-0.246153846153846,-0.230769230769231,-0.215384615384615,-0.2,-0.184615384615385,
-0.169230769230769,-0.153846153846154,-0.138461538461538,-0.123076923076923,
-0.107692307692308,-0.0923076923076923,-0.0769230769230769,-0.0615384615384615,
-0.0461538461538462,-0.0307692307692308,-0.0153846153846154,0.),
 .UNSPECIFIED.)
CURVE()
GEOMETRIC_REPRESENTATION_ITEM()
RATIONAL_B_SPLINE_CURVE((1.,1.,1.,1.,1.,1.,1.,1.,1.,1.,1.,1.,1.,1.,1.,1.,
1.,1.,1.,1.,1.,1.,1.,1.,1.,1.,1.,1.,1.,1.,1.,1.,1.,1.,1.,1.,1.,1.,1.,1.,
1.,1.,1.,1.,1.,1.,1.,1.,1.,1.,1.,1.,1.,1.,1.,1.,1.,1.,1.,1.,1.,1.,1.,1.,
1.,1.,1.,1.,1.,1.))
REPRESENTATION_ITEM('')
);
#429=(
BOUNDED_CURVE()
B_SPLINE_CURVE(5,(#59604,#59605,#59606,#59607,#59608,#59609,#59610,#59611,
#59612,#59613,#59614,#59615,#59616,#59617,#59618,#59619,#59620,#59621,#59622,
#59623,#59624,#59625,#59626,#59627,#59628,#59629,#59630,#59631,#59632,#59633,
#59634,#59635,#59636,#59637,#59638,#59639,#59640,#59641,#59642,#59643,#59644,
#59645,#59646,#59647,#59648,#59649,#59650,#59651,#59652,#59653,#59654,#59655,
#59656,#59657,#59658,#59659,#59660,#59661,#59662,#59663,#59664,#59665,#59666,
#59667,#59668,#59669,#59670,#59671,#59672,#59673),.UNSPECIFIED.,.F.,.F.)
B_SPLINE_CURVE_WITH_KNOTS((6,1,1,1,1,1,1,1,1,1,1,1,1,1,1,1,1,1,1,1,1,1,
1,1,1,1,1,1,1,1,1,1,1,1,1,1,1,1,1,1,1,1,1,1,1,1,1,1,1,1,1,1,1,1,1,1,1,1,
1,1,1,1,1,1,1,6),(-1.,-0.984615384615383,-0.969230769230768,-0.953846153846152,
-0.938461538461537,-0.923076923076922,-0.907692307692306,-0.892307692307691,
-0.876923076923076,-0.86153846153846,-0.846153846153845,-0.83076923076923,
-0.815384615384614,-0.799999999999999,-0.784615384615384,-0.769230769230768,
-0.753846153846153,-0.738461538461538,-0.723076923076922,-0.707692307692307,
-0.692307692307692,-0.676923076923076,-0.661538461538461,-0.646153846153846,
-0.63076923076923,-0.615384615384615,-0.6,-0.584615384615384,-0.569230769230769,
-0.553846153846154,-0.538461538461538,-0.523076923076923,-0.507692307692308,
-0.492307692307692,-0.476923076923077,-0.461538461538462,-0.446153846153846,
-0.430769230769231,-0.415384615384615,-0.4,-0.384615384615385,-0.369230769230769,
-0.353846153846154,-0.338461538461538,-0.323076923076923,-0.307692307692308,
-0.292307692307692,-0.276923076923077,-0.261538461538462,-0.246153846153846,
-0.230769230769231,-0.215384615384615,-0.2,-0.184615384615385,-0.169230769230769,
-0.153846153846154,-0.138461538461538,-0.123076923076923,-0.107692307692308,
-0.0923076923076923,-0.0769230769230769,-0.0615384615384615,-0.0461538461538462,
-0.0307692307692308,-0.0153846153846154,-0.00577184337452512),
 .UNSPECIFIED.)
CURVE()
GEOMETRIC_REPRESENTATION_ITEM()
RATIONAL_B_SPLINE_CURVE((1.,1.,1.,1.,1.,1.,1.,1.,1.,1.,1.,1.,1.,1.,1.,1.,
1.,1.,1.,1.,1.,1.,1.,1.,1.,1.,1.,1.,1.,1.,1.,1.,1.,1.,1.,1.,1.,1.,1.,1.,
1.,1.,1.,1.,1.,1.,1.,1.,1.,1.,1.,1.,1.,1.,1.,1.,1.,1.,1.,1.,1.,1.,1.,1.,
1.,1.,1.,1.,1.,1.))
REPRESENTATION_ITEM('')
);
#430=(
BOUNDED_CURVE()
B_SPLINE_CURVE(5,(#59824,#59825,#59826,#59827,#59828,#59829,#59830,#59831,
#59832,#59833,#59834,#59835,#59836,#59837,#59838,#59839,#59840,#59841,#59842,
#59843,#59844,#59845,#59846,#59847,#59848,#59849,#59850,#59851,#59852,#59853,
#59854,#59855,#59856,#59857,#59858,#59859,#59860,#59861,#59862,#59863,#59864,
#59865,#59866,#59867,#59868,#59869,#59870,#59871,#59872,#59873,#59874,#59875,
#59876,#59877,#59878,#59879,#59880,#59881,#59882,#59883,#59884,#59885,#59886,
#59887,#59888,#59889,#59890,#59891,#59892,#59893),.UNSPECIFIED.,.F.,.F.)
B_SPLINE_CURVE_WITH_KNOTS((6,1,1,1,1,1,1,1,1,1,1,1,1,1,1,1,1,1,1,1,1,1,
1,1,1,1,1,1,1,1,1,1,1,1,1,1,1,1,1,1,1,1,1,1,1,1,1,1,1,1,1,1,1,1,1,1,1,1,
1,1,1,1,1,1,1,6),(-0.994228156739691,-0.984615384615383,-0.969230769230768,
-0.953846153846152,-0.938461538461537,-0.923076923076922,-0.907692307692306,
-0.892307692307691,-0.876923076923076,-0.86153846153846,-0.846153846153845,
-0.83076923076923,-0.815384615384614,-0.799999999999999,-0.784615384615384,
-0.769230769230768,-0.753846153846153,-0.738461538461538,-0.723076923076922,
-0.707692307692307,-0.692307692307692,-0.676923076923076,-0.661538461538461,
-0.646153846153846,-0.63076923076923,-0.615384615384615,-0.6,-0.584615384615384,
-0.569230769230769,-0.553846153846154,-0.538461538461538,-0.523076923076923,
-0.507692307692308,-0.492307692307692,-0.476923076923077,-0.461538461538462,
-0.446153846153846,-0.430769230769231,-0.415384615384615,-0.4,-0.384615384615385,
-0.369230769230769,-0.353846153846154,-0.338461538461538,-0.323076923076923,
-0.307692307692308,-0.292307692307692,-0.276923076923077,-0.261538461538462,
-0.246153846153846,-0.230769230769231,-0.215384615384615,-0.2,-0.184615384615385,
-0.169230769230769,-0.153846153846154,-0.138461538461538,-0.123076923076923,
-0.107692307692308,-0.0923076923076923,-0.0769230769230769,-0.0615384615384615,
-0.0461538461538462,-0.0307692307692308,-0.0153846153846154,0.),
 .UNSPECIFIED.)
CURVE()
GEOMETRIC_REPRESENTATION_ITEM()
RATIONAL_B_SPLINE_CURVE((1.,1.,1.,1.,1.,1.,1.,1.,1.,1.,1.,1.,1.,1.,1.,1.,
1.,1.,1.,1.,1.,1.,1.,1.,1.,1.,1.,1.,1.,1.,1.,1.,1.,1.,1.,1.,1.,1.,1.,1.,
1.,1.,1.,1.,1.,1.,1.,1.,1.,1.,1.,1.,1.,1.,1.,1.,1.,1.,1.,1.,1.,1.,1.,1.,
1.,1.,1.,1.,1.,1.))
REPRESENTATION_ITEM('')
);
#431=(
BOUNDED_CURVE()
B_SPLINE_CURVE(5,(#60046,#60047,#60048,#60049,#60050,#60051,#60052,#60053,
#60054,#60055,#60056,#60057,#60058,#60059,#60060,#60061,#60062,#60063,#60064,
#60065,#60066,#60067,#60068,#60069,#60070,#60071,#60072,#60073,#60074,#60075,
#60076,#60077,#60078,#60079,#60080,#60081,#60082,#60083,#60084,#60085,#60086,
#60087,#60088,#60089,#60090,#60091,#60092,#60093,#60094,#60095,#60096,#60097,
#60098,#60099,#60100,#60101,#60102,#60103,#60104,#60105,#60106,#60107,#60108,
#60109,#60110,#60111,#60112,#60113,#60114,#60115),.UNSPECIFIED.,.F.,.F.)
B_SPLINE_CURVE_WITH_KNOTS((6,1,1,1,1,1,1,1,1,1,1,1,1,1,1,1,1,1,1,1,1,1,
1,1,1,1,1,1,1,1,1,1,1,1,1,1,1,1,1,1,1,1,1,1,1,1,1,1,1,1,1,1,1,1,1,1,1,1,
1,1,1,1,1,1,1,6),(-1.,-0.984615384615383,-0.969230769230768,-0.953846153846152,
-0.938461538461537,-0.923076923076922,-0.907692307692306,-0.892307692307691,
-0.876923076923076,-0.86153846153846,-0.846153846153845,-0.83076923076923,
-0.815384615384614,-0.799999999999999,-0.784615384615384,-0.769230769230768,
-0.753846153846153,-0.738461538461538,-0.723076923076922,-0.707692307692307,
-0.692307692307692,-0.676923076923076,-0.661538461538461,-0.646153846153846,
-0.63076923076923,-0.615384615384615,-0.6,-0.584615384615384,-0.569230769230769,
-0.553846153846154,-0.538461538461538,-0.523076923076923,-0.507692307692308,
-0.492307692307692,-0.476923076923077,-0.461538461538462,-0.446153846153846,
-0.430769230769231,-0.415384615384615,-0.4,-0.384615384615385,-0.369230769230769,
-0.353846153846154,-0.338461538461538,-0.323076923076923,-0.307692307692308,
-0.292307692307692,-0.276923076923077,-0.261538461538462,-0.246153846153846,
-0.230769230769231,-0.215384615384615,-0.2,-0.184615384615385,-0.169230769230769,
-0.153846153846154,-0.138461538461538,-0.123076923076923,-0.107692307692308,
-0.0923076923076923,-0.0769230769230769,-0.0615384615384615,-0.0461538461538462,
-0.0307692307692308,-0.0153846153846154,-0.00577184337448448),
 .UNSPECIFIED.)
CURVE()
GEOMETRIC_REPRESENTATION_ITEM()
RATIONAL_B_SPLINE_CURVE((1.,1.,1.,1.,1.,1.,1.,1.,1.,1.,1.,1.,1.,1.,1.,1.,
1.,1.,1.,1.,1.,1.,1.,1.,1.,1.,1.,1.,1.,1.,1.,1.,1.,1.,1.,1.,1.,1.,1.,1.,
1.,1.,1.,1.,1.,1.,1.,1.,1.,1.,1.,1.,1.,1.,1.,1.,1.,1.,1.,1.,1.,1.,1.,1.,
1.,1.,1.,1.,1.,1.))
REPRESENTATION_ITEM('')
);
#432=(
BOUNDED_CURVE()
B_SPLINE_CURVE(5,(#60266,#60267,#60268,#60269,#60270,#60271,#60272,#60273,
#60274,#60275,#60276,#60277,#60278,#60279,#60280,#60281,#60282,#60283,#60284,
#60285,#60286,#60287,#60288,#60289,#60290,#60291,#60292,#60293,#60294,#60295,
#60296,#60297,#60298,#60299,#60300,#60301,#60302,#60303,#60304,#60305,#60306,
#60307,#60308,#60309,#60310,#60311,#60312,#60313,#60314,#60315,#60316,#60317,
#60318,#60319,#60320,#60321,#60322,#60323,#60324,#60325,#60326,#60327,#60328,
#60329,#60330,#60331,#60332,#60333,#60334,#60335),.UNSPECIFIED.,.F.,.F.)
B_SPLINE_CURVE_WITH_KNOTS((6,1,1,1,1,1,1,1,1,1,1,1,1,1,1,1,1,1,1,1,1,1,
1,1,1,1,1,1,1,1,1,1,1,1,1,1,1,1,1,1,1,1,1,1,1,1,1,1,1,1,1,1,1,1,1,1,1,1,
1,1,1,1,1,1,1,6),(-0.99422815673972,-0.984615384615383,-0.969230769230768,
-0.953846153846152,-0.938461538461537,-0.923076923076922,-0.907692307692306,
-0.892307692307691,-0.876923076923076,-0.86153846153846,-0.846153846153845,
-0.83076923076923,-0.815384615384614,-0.799999999999999,-0.784615384615384,
-0.769230769230768,-0.753846153846153,-0.738461538461538,-0.723076923076922,
-0.707692307692307,-0.692307692307692,-0.676923076923076,-0.661538461538461,
-0.646153846153846,-0.63076923076923,-0.615384615384615,-0.6,-0.584615384615384,
-0.569230769230769,-0.553846153846154,-0.538461538461538,-0.523076923076923,
-0.507692307692308,-0.492307692307692,-0.476923076923077,-0.461538461538462,
-0.446153846153846,-0.430769230769231,-0.415384615384615,-0.4,-0.384615384615385,
-0.369230769230769,-0.353846153846154,-0.338461538461538,-0.323076923076923,
-0.307692307692308,-0.292307692307692,-0.276923076923077,-0.261538461538462,
-0.246153846153846,-0.230769230769231,-0.215384615384615,-0.2,-0.184615384615385,
-0.169230769230769,-0.153846153846154,-0.138461538461538,-0.123076923076923,
-0.107692307692308,-0.0923076923076923,-0.0769230769230769,-0.0615384615384615,
-0.0461538461538462,-0.0307692307692308,-0.0153846153846154,0.),
 .UNSPECIFIED.)
CURVE()
GEOMETRIC_REPRESENTATION_ITEM()
RATIONAL_B_SPLINE_CURVE((1.,1.,1.,1.,1.,1.,1.,1.,1.,1.,1.,1.,1.,1.,1.,1.,
1.,1.,1.,1.,1.,1.,1.,1.,1.,1.,1.,1.,1.,1.,1.,1.,1.,1.,1.,1.,1.,1.,1.,1.,
1.,1.,1.,1.,1.,1.,1.,1.,1.,1.,1.,1.,1.,1.,1.,1.,1.,1.,1.,1.,1.,1.,1.,1.,
1.,1.,1.,1.,1.,1.))
REPRESENTATION_ITEM('')
);
#433=(
BOUNDED_CURVE()
B_SPLINE_CURVE(5,(#60488,#60489,#60490,#60491,#60492,#60493,#60494,#60495,
#60496,#60497,#60498,#60499,#60500,#60501,#60502,#60503,#60504,#60505,#60506,
#60507,#60508,#60509,#60510,#60511,#60512,#60513,#60514,#60515,#60516,#60517,
#60518,#60519,#60520,#60521,#60522,#60523,#60524,#60525,#60526,#60527,#60528,
#60529,#60530,#60531,#60532,#60533,#60534,#60535,#60536,#60537,#60538,#60539,
#60540,#60541,#60542,#60543,#60544,#60545,#60546,#60547,#60548,#60549,#60550,
#60551,#60552,#60553,#60554,#60555,#60556,#60557),.UNSPECIFIED.,.F.,.F.)
B_SPLINE_CURVE_WITH_KNOTS((6,1,1,1,1,1,1,1,1,1,1,1,1,1,1,1,1,1,1,1,1,1,
1,1,1,1,1,1,1,1,1,1,1,1,1,1,1,1,1,1,1,1,1,1,1,1,1,1,1,1,1,1,1,1,1,1,1,1,
1,1,1,1,1,1,1,6),(-1.,-0.984615384615383,-0.969230769230768,-0.953846153846152,
-0.938461538461537,-0.923076923076922,-0.907692307692306,-0.892307692307691,
-0.876923076923076,-0.86153846153846,-0.846153846153845,-0.83076923076923,
-0.815384615384614,-0.799999999999999,-0.784615384615384,-0.769230769230768,
-0.753846153846153,-0.738461538461538,-0.723076923076922,-0.707692307692307,
-0.692307692307692,-0.676923076923076,-0.661538461538461,-0.646153846153846,
-0.63076923076923,-0.615384615384615,-0.6,-0.584615384615384,-0.569230769230769,
-0.553846153846154,-0.538461538461538,-0.523076923076923,-0.507692307692308,
-0.492307692307692,-0.476923076923077,-0.461538461538462,-0.446153846153846,
-0.430769230769231,-0.415384615384615,-0.4,-0.384615384615385,-0.369230769230769,
-0.353846153846154,-0.338461538461538,-0.323076923076923,-0.307692307692308,
-0.292307692307692,-0.276923076923077,-0.261538461538462,-0.246153846153846,
-0.230769230769231,-0.215384615384615,-0.2,-0.184615384615385,-0.169230769230769,
-0.153846153846154,-0.138461538461538,-0.123076923076923,-0.107692307692308,
-0.0923076923076923,-0.0769230769230769,-0.0615384615384615,-0.0461538461538462,
-0.0307692307692308,-0.0153846153846154,-0.00577184337448251),
 .UNSPECIFIED.)
CURVE()
GEOMETRIC_REPRESENTATION_ITEM()
RATIONAL_B_SPLINE_CURVE((1.,1.,1.,1.,1.,1.,1.,1.,1.,1.,1.,1.,1.,1.,1.,1.,
1.,1.,1.,1.,1.,1.,1.,1.,1.,1.,1.,1.,1.,1.,1.,1.,1.,1.,1.,1.,1.,1.,1.,1.,
1.,1.,1.,1.,1.,1.,1.,1.,1.,1.,1.,1.,1.,1.,1.,1.,1.,1.,1.,1.,1.,1.,1.,1.,
1.,1.,1.,1.,1.,1.))
REPRESENTATION_ITEM('')
);
#434=(
BOUNDED_CURVE()
B_SPLINE_CURVE(5,(#60708,#60709,#60710,#60711,#60712,#60713,#60714,#60715,
#60716,#60717,#60718,#60719,#60720,#60721,#60722,#60723,#60724,#60725,#60726,
#60727,#60728,#60729,#60730,#60731,#60732,#60733,#60734,#60735,#60736,#60737,
#60738,#60739,#60740,#60741,#60742,#60743,#60744,#60745,#60746,#60747,#60748,
#60749,#60750,#60751,#60752,#60753,#60754,#60755,#60756,#60757,#60758,#60759,
#60760,#60761,#60762,#60763,#60764,#60765,#60766,#60767,#60768,#60769,#60770,
#60771,#60772,#60773,#60774,#60775,#60776,#60777),.UNSPECIFIED.,.F.,.F.)
B_SPLINE_CURVE_WITH_KNOTS((6,1,1,1,1,1,1,1,1,1,1,1,1,1,1,1,1,1,1,1,1,1,
1,1,1,1,1,1,1,1,1,1,1,1,1,1,1,1,1,1,1,1,1,1,1,1,1,1,1,1,1,1,1,1,1,1,1,1,
1,1,1,1,1,1,1,6),(-0.994228156739703,-0.984615384615383,-0.969230769230768,
-0.953846153846152,-0.938461538461537,-0.923076923076922,-0.907692307692306,
-0.892307692307691,-0.876923076923076,-0.86153846153846,-0.846153846153845,
-0.83076923076923,-0.815384615384614,-0.799999999999999,-0.784615384615384,
-0.769230769230768,-0.753846153846153,-0.738461538461538,-0.723076923076922,
-0.707692307692307,-0.692307692307692,-0.676923076923076,-0.661538461538461,
-0.646153846153846,-0.63076923076923,-0.615384615384615,-0.6,-0.584615384615384,
-0.569230769230769,-0.553846153846154,-0.538461538461538,-0.523076923076923,
-0.507692307692308,-0.492307692307692,-0.476923076923077,-0.461538461538462,
-0.446153846153846,-0.430769230769231,-0.415384615384615,-0.4,-0.384615384615385,
-0.369230769230769,-0.353846153846154,-0.338461538461538,-0.323076923076923,
-0.307692307692308,-0.292307692307692,-0.276923076923077,-0.261538461538462,
-0.246153846153846,-0.230769230769231,-0.215384615384615,-0.2,-0.184615384615385,
-0.169230769230769,-0.153846153846154,-0.138461538461538,-0.123076923076923,
-0.107692307692308,-0.0923076923076923,-0.0769230769230769,-0.0615384615384615,
-0.0461538461538462,-0.0307692307692308,-0.0153846153846154,0.),
 .UNSPECIFIED.)
CURVE()
GEOMETRIC_REPRESENTATION_ITEM()
RATIONAL_B_SPLINE_CURVE((1.,1.,1.,1.,1.,1.,1.,1.,1.,1.,1.,1.,1.,1.,1.,1.,
1.,1.,1.,1.,1.,1.,1.,1.,1.,1.,1.,1.,1.,1.,1.,1.,1.,1.,1.,1.,1.,1.,1.,1.,
1.,1.,1.,1.,1.,1.,1.,1.,1.,1.,1.,1.,1.,1.,1.,1.,1.,1.,1.,1.,1.,1.,1.,1.,
1.,1.,1.,1.,1.,1.))
REPRESENTATION_ITEM('')
);
#435=(
BOUNDED_CURVE()
B_SPLINE_CURVE(5,(#60930,#60931,#60932,#60933,#60934,#60935,#60936,#60937,
#60938,#60939,#60940,#60941,#60942,#60943,#60944,#60945,#60946,#60947,#60948,
#60949,#60950,#60951,#60952,#60953,#60954,#60955,#60956,#60957,#60958,#60959,
#60960,#60961,#60962,#60963,#60964,#60965,#60966,#60967,#60968,#60969,#60970,
#60971,#60972,#60973,#60974,#60975,#60976,#60977,#60978,#60979,#60980,#60981,
#60982,#60983,#60984,#60985,#60986,#60987,#60988,#60989,#60990,#60991,#60992,
#60993,#60994,#60995,#60996,#60997,#60998,#60999),.UNSPECIFIED.,.F.,.F.)
B_SPLINE_CURVE_WITH_KNOTS((6,1,1,1,1,1,1,1,1,1,1,1,1,1,1,1,1,1,1,1,1,1,
1,1,1,1,1,1,1,1,1,1,1,1,1,1,1,1,1,1,1,1,1,1,1,1,1,1,1,1,1,1,1,1,1,1,1,1,
1,1,1,1,1,1,1,6),(-1.,-0.984615384615383,-0.969230769230768,-0.953846153846152,
-0.938461538461537,-0.923076923076922,-0.907692307692306,-0.892307692307691,
-0.876923076923076,-0.86153846153846,-0.846153846153845,-0.83076923076923,
-0.815384615384614,-0.799999999999999,-0.784615384615384,-0.769230769230768,
-0.753846153846153,-0.738461538461538,-0.723076923076922,-0.707692307692307,
-0.692307692307692,-0.676923076923076,-0.661538461538461,-0.646153846153846,
-0.63076923076923,-0.615384615384615,-0.6,-0.584615384615384,-0.569230769230769,
-0.553846153846154,-0.538461538461538,-0.523076923076923,-0.507692307692308,
-0.492307692307692,-0.476923076923077,-0.461538461538462,-0.446153846153846,
-0.430769230769231,-0.415384615384615,-0.4,-0.384615384615385,-0.369230769230769,
-0.353846153846154,-0.338461538461538,-0.323076923076923,-0.307692307692308,
-0.292307692307692,-0.276923076923077,-0.261538461538462,-0.246153846153846,
-0.230769230769231,-0.215384615384615,-0.2,-0.184615384615385,-0.169230769230769,
-0.153846153846154,-0.138461538461538,-0.123076923076923,-0.107692307692308,
-0.0923076923076923,-0.0769230769230769,-0.0615384615384615,-0.0461538461538462,
-0.0307692307692308,-0.0153846153846154,-0.00577184337449602),
 .UNSPECIFIED.)
CURVE()
GEOMETRIC_REPRESENTATION_ITEM()
RATIONAL_B_SPLINE_CURVE((1.,1.,1.,1.,1.,1.,1.,1.,1.,1.,1.,1.,1.,1.,1.,1.,
1.,1.,1.,1.,1.,1.,1.,1.,1.,1.,1.,1.,1.,1.,1.,1.,1.,1.,1.,1.,1.,1.,1.,1.,
1.,1.,1.,1.,1.,1.,1.,1.,1.,1.,1.,1.,1.,1.,1.,1.,1.,1.,1.,1.,1.,1.,1.,1.,
1.,1.,1.,1.,1.,1.))
REPRESENTATION_ITEM('')
);
#436=(
BOUNDED_CURVE()
B_SPLINE_CURVE(5,(#61150,#61151,#61152,#61153,#61154,#61155,#61156,#61157,
#61158,#61159,#61160,#61161,#61162,#61163,#61164,#61165,#61166,#61167,#61168,
#61169,#61170,#61171,#61172,#61173,#61174,#61175,#61176,#61177,#61178,#61179,
#61180,#61181,#61182,#61183,#61184,#61185,#61186,#61187,#61188,#61189,#61190,
#61191,#61192,#61193,#61194,#61195,#61196,#61197,#61198,#61199,#61200,#61201,
#61202,#61203,#61204,#61205,#61206,#61207,#61208,#61209,#61210,#61211,#61212,
#61213,#61214,#61215,#61216,#61217,#61218,#61219),.UNSPECIFIED.,.F.,.F.)
B_SPLINE_CURVE_WITH_KNOTS((6,1,1,1,1,1,1,1,1,1,1,1,1,1,1,1,1,1,1,1,1,1,
1,1,1,1,1,1,1,1,1,1,1,1,1,1,1,1,1,1,1,1,1,1,1,1,1,1,1,1,1,1,1,1,1,1,1,1,
1,1,1,1,1,1,1,6),(-0.994228156739695,-0.984615384615383,-0.969230769230768,
-0.953846153846152,-0.938461538461537,-0.923076923076922,-0.907692307692306,
-0.892307692307691,-0.876923076923076,-0.86153846153846,-0.846153846153845,
-0.83076923076923,-0.815384615384614,-0.799999999999999,-0.784615384615384,
-0.769230769230768,-0.753846153846153,-0.738461538461538,-0.723076923076922,
-0.707692307692307,-0.692307692307692,-0.676923076923076,-0.661538461538461,
-0.646153846153846,-0.63076923076923,-0.615384615384615,-0.6,-0.584615384615384,
-0.569230769230769,-0.553846153846154,-0.538461538461538,-0.523076923076923,
-0.507692307692308,-0.492307692307692,-0.476923076923077,-0.461538461538462,
-0.446153846153846,-0.430769230769231,-0.415384615384615,-0.4,-0.384615384615385,
-0.369230769230769,-0.353846153846154,-0.338461538461538,-0.323076923076923,
-0.307692307692308,-0.292307692307692,-0.276923076923077,-0.261538461538462,
-0.246153846153846,-0.230769230769231,-0.215384615384615,-0.2,-0.184615384615385,
-0.169230769230769,-0.153846153846154,-0.138461538461538,-0.123076923076923,
-0.107692307692308,-0.0923076923076923,-0.0769230769230769,-0.0615384615384615,
-0.0461538461538462,-0.0307692307692308,-0.0153846153846154,0.),
 .UNSPECIFIED.)
CURVE()
GEOMETRIC_REPRESENTATION_ITEM()
RATIONAL_B_SPLINE_CURVE((1.,1.,1.,1.,1.,1.,1.,1.,1.,1.,1.,1.,1.,1.,1.,1.,
1.,1.,1.,1.,1.,1.,1.,1.,1.,1.,1.,1.,1.,1.,1.,1.,1.,1.,1.,1.,1.,1.,1.,1.,
1.,1.,1.,1.,1.,1.,1.,1.,1.,1.,1.,1.,1.,1.,1.,1.,1.,1.,1.,1.,1.,1.,1.,1.,
1.,1.,1.,1.,1.,1.))
REPRESENTATION_ITEM('')
);
#437=(
BOUNDED_CURVE()
B_SPLINE_CURVE(5,(#61372,#61373,#61374,#61375,#61376,#61377,#61378,#61379,
#61380,#61381,#61382,#61383,#61384,#61385,#61386,#61387,#61388,#61389,#61390,
#61391,#61392,#61393,#61394,#61395,#61396,#61397,#61398,#61399,#61400,#61401,
#61402,#61403,#61404,#61405,#61406,#61407,#61408,#61409,#61410,#61411,#61412,
#61413,#61414,#61415,#61416,#61417,#61418,#61419,#61420,#61421,#61422,#61423,
#61424,#61425,#61426,#61427,#61428,#61429,#61430,#61431,#61432,#61433,#61434,
#61435,#61436,#61437,#61438,#61439,#61440,#61441),.UNSPECIFIED.,.F.,.F.)
B_SPLINE_CURVE_WITH_KNOTS((6,1,1,1,1,1,1,1,1,1,1,1,1,1,1,1,1,1,1,1,1,1,
1,1,1,1,1,1,1,1,1,1,1,1,1,1,1,1,1,1,1,1,1,1,1,1,1,1,1,1,1,1,1,1,1,1,1,1,
1,1,1,1,1,1,1,6),(-1.,-0.984615384615383,-0.969230769230768,-0.953846153846152,
-0.938461538461537,-0.923076923076922,-0.907692307692306,-0.892307692307691,
-0.876923076923076,-0.86153846153846,-0.846153846153845,-0.83076923076923,
-0.815384615384614,-0.799999999999999,-0.784615384615384,-0.769230769230768,
-0.753846153846153,-0.738461538461538,-0.723076923076922,-0.707692307692307,
-0.692307692307692,-0.676923076923076,-0.661538461538461,-0.646153846153846,
-0.63076923076923,-0.615384615384615,-0.6,-0.584615384615384,-0.569230769230769,
-0.553846153846154,-0.538461538461538,-0.523076923076923,-0.507692307692308,
-0.492307692307692,-0.476923076923077,-0.461538461538462,-0.446153846153846,
-0.430769230769231,-0.415384615384615,-0.4,-0.384615384615385,-0.369230769230769,
-0.353846153846154,-0.338461538461538,-0.323076923076923,-0.307692307692308,
-0.292307692307692,-0.276923076923077,-0.261538461538462,-0.246153846153846,
-0.230769230769231,-0.215384615384615,-0.2,-0.184615384615385,-0.169230769230769,
-0.153846153846154,-0.138461538461538,-0.123076923076923,-0.107692307692308,
-0.0923076923076923,-0.0769230769230769,-0.0615384615384615,-0.0461538461538462,
-0.0307692307692308,-0.0153846153846154,-0.00577184337450911),
 .UNSPECIFIED.)
CURVE()
GEOMETRIC_REPRESENTATION_ITEM()
RATIONAL_B_SPLINE_CURVE((1.,1.,1.,1.,1.,1.,1.,1.,1.,1.,1.,1.,1.,1.,1.,1.,
1.,1.,1.,1.,1.,1.,1.,1.,1.,1.,1.,1.,1.,1.,1.,1.,1.,1.,1.,1.,1.,1.,1.,1.,
1.,1.,1.,1.,1.,1.,1.,1.,1.,1.,1.,1.,1.,1.,1.,1.,1.,1.,1.,1.,1.,1.,1.,1.,
1.,1.,1.,1.,1.,1.))
REPRESENTATION_ITEM('')
);
#438=(
BOUNDED_CURVE()
B_SPLINE_CURVE(5,(#61592,#61593,#61594,#61595,#61596,#61597,#61598,#61599,
#61600,#61601,#61602,#61603,#61604,#61605,#61606,#61607,#61608,#61609,#61610,
#61611,#61612,#61613,#61614,#61615,#61616,#61617,#61618,#61619,#61620,#61621,
#61622,#61623,#61624,#61625,#61626,#61627,#61628,#61629,#61630,#61631,#61632,
#61633,#61634,#61635,#61636,#61637,#61638,#61639,#61640,#61641,#61642,#61643,
#61644,#61645,#61646,#61647,#61648,#61649,#61650,#61651,#61652,#61653,#61654,
#61655,#61656,#61657,#61658,#61659,#61660,#61661),.UNSPECIFIED.,.F.,.F.)
B_SPLINE_CURVE_WITH_KNOTS((6,1,1,1,1,1,1,1,1,1,1,1,1,1,1,1,1,1,1,1,1,1,
1,1,1,1,1,1,1,1,1,1,1,1,1,1,1,1,1,1,1,1,1,1,1,1,1,1,1,1,1,1,1,1,1,1,1,1,
1,1,1,1,1,1,1,6),(-0.994228156739712,-0.984615384615383,-0.969230769230768,
-0.953846153846152,-0.938461538461537,-0.923076923076922,-0.907692307692306,
-0.892307692307691,-0.876923076923076,-0.86153846153846,-0.846153846153845,
-0.83076923076923,-0.815384615384614,-0.799999999999999,-0.784615384615384,
-0.769230769230768,-0.753846153846153,-0.738461538461538,-0.723076923076922,
-0.707692307692307,-0.692307692307692,-0.676923076923076,-0.661538461538461,
-0.646153846153846,-0.63076923076923,-0.615384615384615,-0.6,-0.584615384615384,
-0.569230769230769,-0.553846153846154,-0.538461538461538,-0.523076923076923,
-0.507692307692308,-0.492307692307692,-0.476923076923077,-0.461538461538462,
-0.446153846153846,-0.430769230769231,-0.415384615384615,-0.4,-0.384615384615385,
-0.369230769230769,-0.353846153846154,-0.338461538461538,-0.323076923076923,
-0.307692307692308,-0.292307692307692,-0.276923076923077,-0.261538461538462,
-0.246153846153846,-0.230769230769231,-0.215384615384615,-0.2,-0.184615384615385,
-0.169230769230769,-0.153846153846154,-0.138461538461538,-0.123076923076923,
-0.107692307692308,-0.0923076923076923,-0.0769230769230769,-0.0615384615384615,
-0.0461538461538462,-0.0307692307692308,-0.0153846153846154,0.),
 .UNSPECIFIED.)
CURVE()
GEOMETRIC_REPRESENTATION_ITEM()
RATIONAL_B_SPLINE_CURVE((1.,1.,1.,1.,1.,1.,1.,1.,1.,1.,1.,1.,1.,1.,1.,1.,
1.,1.,1.,1.,1.,1.,1.,1.,1.,1.,1.,1.,1.,1.,1.,1.,1.,1.,1.,1.,1.,1.,1.,1.,
1.,1.,1.,1.,1.,1.,1.,1.,1.,1.,1.,1.,1.,1.,1.,1.,1.,1.,1.,1.,1.,1.,1.,1.,
1.,1.,1.,1.,1.,1.))
REPRESENTATION_ITEM('')
);
#439=(
BOUNDED_CURVE()
B_SPLINE_CURVE(5,(#61814,#61815,#61816,#61817,#61818,#61819,#61820,#61821,
#61822,#61823,#61824,#61825,#61826,#61827,#61828,#61829,#61830,#61831,#61832,
#61833,#61834,#61835,#61836,#61837,#61838,#61839,#61840,#61841,#61842,#61843,
#61844,#61845,#61846,#61847,#61848,#61849,#61850,#61851,#61852,#61853,#61854,
#61855,#61856,#61857,#61858,#61859,#61860,#61861,#61862,#61863,#61864,#61865,
#61866,#61867,#61868,#61869,#61870,#61871,#61872,#61873,#61874,#61875,#61876,
#61877,#61878,#61879,#61880,#61881,#61882,#61883),.UNSPECIFIED.,.F.,.F.)
B_SPLINE_CURVE_WITH_KNOTS((6,1,1,1,1,1,1,1,1,1,1,1,1,1,1,1,1,1,1,1,1,1,
1,1,1,1,1,1,1,1,1,1,1,1,1,1,1,1,1,1,1,1,1,1,1,1,1,1,1,1,1,1,1,1,1,1,1,1,
1,1,1,1,1,1,1,6),(-1.,-0.984615384615383,-0.969230769230768,-0.953846153846152,
-0.938461538461537,-0.923076923076922,-0.907692307692306,-0.892307692307691,
-0.876923076923076,-0.86153846153846,-0.846153846153845,-0.83076923076923,
-0.815384615384614,-0.799999999999999,-0.784615384615384,-0.769230769230768,
-0.753846153846153,-0.738461538461538,-0.723076923076922,-0.707692307692307,
-0.692307692307692,-0.676923076923076,-0.661538461538461,-0.646153846153846,
-0.63076923076923,-0.615384615384615,-0.6,-0.584615384615384,-0.569230769230769,
-0.553846153846154,-0.538461538461538,-0.523076923076923,-0.507692307692308,
-0.492307692307692,-0.476923076923077,-0.461538461538462,-0.446153846153846,
-0.430769230769231,-0.415384615384615,-0.4,-0.384615384615385,-0.369230769230769,
-0.353846153846154,-0.338461538461538,-0.323076923076923,-0.307692307692308,
-0.292307692307692,-0.276923076923077,-0.261538461538462,-0.246153846153846,
-0.230769230769231,-0.215384615384615,-0.2,-0.184615384615385,-0.169230769230769,
-0.153846153846154,-0.138461538461538,-0.123076923076923,-0.107692307692308,
-0.0923076923076923,-0.0769230769230769,-0.0615384615384615,-0.0461538461538462,
-0.0307692307692308,-0.0153846153846154,-0.00577184337451206),
 .UNSPECIFIED.)
CURVE()
GEOMETRIC_REPRESENTATION_ITEM()
RATIONAL_B_SPLINE_CURVE((1.,1.,1.,1.,1.,1.,1.,1.,1.,1.,1.,1.,1.,1.,1.,1.,
1.,1.,1.,1.,1.,1.,1.,1.,1.,1.,1.,1.,1.,1.,1.,1.,1.,1.,1.,1.,1.,1.,1.,1.,
1.,1.,1.,1.,1.,1.,1.,1.,1.,1.,1.,1.,1.,1.,1.,1.,1.,1.,1.,1.,1.,1.,1.,1.,
1.,1.,1.,1.,1.,1.))
REPRESENTATION_ITEM('')
);
#440=(
BOUNDED_CURVE()
B_SPLINE_CURVE(5,(#62034,#62035,#62036,#62037,#62038,#62039,#62040,#62041,
#62042,#62043,#62044,#62045,#62046,#62047,#62048,#62049,#62050,#62051,#62052,
#62053,#62054,#62055,#62056,#62057,#62058,#62059,#62060,#62061,#62062,#62063,
#62064,#62065,#62066,#62067,#62068,#62069,#62070,#62071,#62072,#62073,#62074,
#62075,#62076,#62077,#62078,#62079,#62080,#62081,#62082,#62083,#62084,#62085,
#62086,#62087,#62088,#62089,#62090,#62091,#62092,#62093,#62094,#62095,#62096,
#62097,#62098,#62099,#62100,#62101,#62102,#62103),.UNSPECIFIED.,.F.,.F.)
B_SPLINE_CURVE_WITH_KNOTS((6,1,1,1,1,1,1,1,1,1,1,1,1,1,1,1,1,1,1,1,1,1,
1,1,1,1,1,1,1,1,1,1,1,1,1,1,1,1,1,1,1,1,1,1,1,1,1,1,1,1,1,1,1,1,1,1,1,1,
1,1,1,1,1,1,1,6),(-0.994228156739717,-0.984615384615383,-0.969230769230768,
-0.953846153846152,-0.938461538461537,-0.923076923076922,-0.907692307692306,
-0.892307692307691,-0.876923076923076,-0.86153846153846,-0.846153846153845,
-0.83076923076923,-0.815384615384614,-0.799999999999999,-0.784615384615384,
-0.769230769230768,-0.753846153846153,-0.738461538461538,-0.723076923076922,
-0.707692307692307,-0.692307692307692,-0.676923076923076,-0.661538461538461,
-0.646153846153846,-0.63076923076923,-0.615384615384615,-0.6,-0.584615384615384,
-0.569230769230769,-0.553846153846154,-0.538461538461538,-0.523076923076923,
-0.507692307692308,-0.492307692307692,-0.476923076923077,-0.461538461538462,
-0.446153846153846,-0.430769230769231,-0.415384615384615,-0.4,-0.384615384615385,
-0.369230769230769,-0.353846153846154,-0.338461538461538,-0.323076923076923,
-0.307692307692308,-0.292307692307692,-0.276923076923077,-0.261538461538462,
-0.246153846153846,-0.230769230769231,-0.215384615384615,-0.2,-0.184615384615385,
-0.169230769230769,-0.153846153846154,-0.138461538461538,-0.123076923076923,
-0.107692307692308,-0.0923076923076923,-0.0769230769230769,-0.0615384615384615,
-0.0461538461538462,-0.0307692307692308,-0.0153846153846154,0.),
 .UNSPECIFIED.)
CURVE()
GEOMETRIC_REPRESENTATION_ITEM()
RATIONAL_B_SPLINE_CURVE((1.,1.,1.,1.,1.,1.,1.,1.,1.,1.,1.,1.,1.,1.,1.,1.,
1.,1.,1.,1.,1.,1.,1.,1.,1.,1.,1.,1.,1.,1.,1.,1.,1.,1.,1.,1.,1.,1.,1.,1.,
1.,1.,1.,1.,1.,1.,1.,1.,1.,1.,1.,1.,1.,1.,1.,1.,1.,1.,1.,1.,1.,1.,1.,1.,
1.,1.,1.,1.,1.,1.))
REPRESENTATION_ITEM('')
);
#441=(
BOUNDED_CURVE()
B_SPLINE_CURVE(5,(#62256,#62257,#62258,#62259,#62260,#62261,#62262,#62263,
#62264,#62265,#62266,#62267,#62268,#62269,#62270,#62271,#62272,#62273,#62274,
#62275,#62276,#62277,#62278,#62279,#62280,#62281,#62282,#62283,#62284,#62285,
#62286,#62287,#62288,#62289,#62290,#62291,#62292,#62293,#62294,#62295,#62296,
#62297,#62298,#62299,#62300,#62301,#62302,#62303,#62304,#62305,#62306,#62307,
#62308,#62309,#62310,#62311,#62312,#62313,#62314,#62315,#62316,#62317,#62318,
#62319,#62320,#62321,#62322,#62323,#62324,#62325),.UNSPECIFIED.,.F.,.F.)
B_SPLINE_CURVE_WITH_KNOTS((6,1,1,1,1,1,1,1,1,1,1,1,1,1,1,1,1,1,1,1,1,1,
1,1,1,1,1,1,1,1,1,1,1,1,1,1,1,1,1,1,1,1,1,1,1,1,1,1,1,1,1,1,1,1,1,1,1,1,
1,1,1,1,1,1,1,6),(-1.,-0.984615384615383,-0.969230769230768,-0.953846153846152,
-0.938461538461537,-0.923076923076922,-0.907692307692306,-0.892307692307691,
-0.876923076923076,-0.86153846153846,-0.846153846153845,-0.83076923076923,
-0.815384615384614,-0.799999999999999,-0.784615384615384,-0.769230769230768,
-0.753846153846153,-0.738461538461538,-0.723076923076922,-0.707692307692307,
-0.692307692307692,-0.676923076923076,-0.661538461538461,-0.646153846153846,
-0.63076923076923,-0.615384615384615,-0.6,-0.584615384615384,-0.569230769230769,
-0.553846153846154,-0.538461538461538,-0.523076923076923,-0.507692307692308,
-0.492307692307692,-0.476923076923077,-0.461538461538462,-0.446153846153846,
-0.430769230769231,-0.415384615384615,-0.4,-0.384615384615385,-0.369230769230769,
-0.353846153846154,-0.338461538461538,-0.323076923076923,-0.307692307692308,
-0.292307692307692,-0.276923076923077,-0.261538461538462,-0.246153846153846,
-0.230769230769231,-0.215384615384615,-0.2,-0.184615384615385,-0.169230769230769,
-0.153846153846154,-0.138461538461538,-0.123076923076923,-0.107692307692308,
-0.0923076923076923,-0.0769230769230769,-0.0615384615384615,-0.0461538461538462,
-0.0307692307692308,-0.0153846153846154,-0.00577184337448646),
 .UNSPECIFIED.)
CURVE()
GEOMETRIC_REPRESENTATION_ITEM()
RATIONAL_B_SPLINE_CURVE((1.,1.,1.,1.,1.,1.,1.,1.,1.,1.,1.,1.,1.,1.,1.,1.,
1.,1.,1.,1.,1.,1.,1.,1.,1.,1.,1.,1.,1.,1.,1.,1.,1.,1.,1.,1.,1.,1.,1.,1.,
1.,1.,1.,1.,1.,1.,1.,1.,1.,1.,1.,1.,1.,1.,1.,1.,1.,1.,1.,1.,1.,1.,1.,1.,
1.,1.,1.,1.,1.,1.))
REPRESENTATION_ITEM('')
);
#442=(
BOUNDED_CURVE()
B_SPLINE_CURVE(5,(#62476,#62477,#62478,#62479,#62480,#62481,#62482,#62483,
#62484,#62485,#62486,#62487,#62488,#62489,#62490,#62491,#62492,#62493,#62494,
#62495,#62496,#62497,#62498,#62499,#62500,#62501,#62502,#62503,#62504,#62505,
#62506,#62507,#62508,#62509,#62510,#62511,#62512,#62513,#62514,#62515,#62516,
#62517,#62518,#62519,#62520,#62521,#62522,#62523,#62524,#62525,#62526,#62527,
#62528,#62529,#62530,#62531,#62532,#62533,#62534,#62535,#62536,#62537,#62538,
#62539,#62540,#62541,#62542,#62543,#62544,#62545),.UNSPECIFIED.,.F.,.F.)
B_SPLINE_CURVE_WITH_KNOTS((6,1,1,1,1,1,1,1,1,1,1,1,1,1,1,1,1,1,1,1,1,1,
1,1,1,1,1,1,1,1,1,1,1,1,1,1,1,1,1,1,1,1,1,1,1,1,1,1,1,1,1,1,1,1,1,1,1,1,
1,1,1,1,1,1,1,6),(-0.994228156739708,-0.984615384615383,-0.969230769230768,
-0.953846153846152,-0.938461538461537,-0.923076923076922,-0.907692307692306,
-0.892307692307691,-0.876923076923076,-0.86153846153846,-0.846153846153845,
-0.83076923076923,-0.815384615384614,-0.799999999999999,-0.784615384615384,
-0.769230769230768,-0.753846153846153,-0.738461538461538,-0.723076923076922,
-0.707692307692307,-0.692307692307692,-0.676923076923076,-0.661538461538461,
-0.646153846153846,-0.63076923076923,-0.615384615384615,-0.6,-0.584615384615384,
-0.569230769230769,-0.553846153846154,-0.538461538461538,-0.523076923076923,
-0.507692307692308,-0.492307692307692,-0.476923076923077,-0.461538461538462,
-0.446153846153846,-0.430769230769231,-0.415384615384615,-0.4,-0.384615384615385,
-0.369230769230769,-0.353846153846154,-0.338461538461538,-0.323076923076923,
-0.307692307692308,-0.292307692307692,-0.276923076923077,-0.261538461538462,
-0.246153846153846,-0.230769230769231,-0.215384615384615,-0.2,-0.184615384615385,
-0.169230769230769,-0.153846153846154,-0.138461538461538,-0.123076923076923,
-0.107692307692308,-0.0923076923076923,-0.0769230769230769,-0.0615384615384615,
-0.0461538461538462,-0.0307692307692308,-0.0153846153846154,0.),
 .UNSPECIFIED.)
CURVE()
GEOMETRIC_REPRESENTATION_ITEM()
RATIONAL_B_SPLINE_CURVE((1.,1.,1.,1.,1.,1.,1.,1.,1.,1.,1.,1.,1.,1.,1.,1.,
1.,1.,1.,1.,1.,1.,1.,1.,1.,1.,1.,1.,1.,1.,1.,1.,1.,1.,1.,1.,1.,1.,1.,1.,
1.,1.,1.,1.,1.,1.,1.,1.,1.,1.,1.,1.,1.,1.,1.,1.,1.,1.,1.,1.,1.,1.,1.,1.,
1.,1.,1.,1.,1.,1.))
REPRESENTATION_ITEM('')
);
#443=(
BOUNDED_CURVE()
B_SPLINE_CURVE(5,(#62698,#62699,#62700,#62701,#62702,#62703,#62704,#62705,
#62706,#62707,#62708,#62709,#62710,#62711,#62712,#62713,#62714,#62715,#62716,
#62717,#62718,#62719,#62720,#62721,#62722,#62723,#62724,#62725,#62726,#62727,
#62728,#62729,#62730,#62731,#62732,#62733,#62734,#62735,#62736,#62737,#62738,
#62739,#62740,#62741,#62742,#62743,#62744,#62745,#62746,#62747,#62748,#62749,
#62750,#62751,#62752,#62753,#62754,#62755,#62756,#62757,#62758,#62759,#62760,
#62761,#62762,#62763,#62764,#62765,#62766,#62767),.UNSPECIFIED.,.F.,.F.)
B_SPLINE_CURVE_WITH_KNOTS((6,1,1,1,1,1,1,1,1,1,1,1,1,1,1,1,1,1,1,1,1,1,
1,1,1,1,1,1,1,1,1,1,1,1,1,1,1,1,1,1,1,1,1,1,1,1,1,1,1,1,1,1,1,1,1,1,1,1,
1,1,1,1,1,1,1,6),(-1.,-0.984615384615383,-0.969230769230768,-0.953846153846152,
-0.938461538461537,-0.923076923076922,-0.907692307692306,-0.892307692307691,
-0.876923076923076,-0.86153846153846,-0.846153846153845,-0.83076923076923,
-0.815384615384614,-0.799999999999999,-0.784615384615384,-0.769230769230768,
-0.753846153846153,-0.738461538461538,-0.723076923076922,-0.707692307692307,
-0.692307692307692,-0.676923076923076,-0.661538461538461,-0.646153846153846,
-0.63076923076923,-0.615384615384615,-0.6,-0.584615384615384,-0.569230769230769,
-0.553846153846154,-0.538461538461538,-0.523076923076923,-0.507692307692308,
-0.492307692307692,-0.476923076923077,-0.461538461538462,-0.446153846153846,
-0.430769230769231,-0.415384615384615,-0.4,-0.384615384615385,-0.369230769230769,
-0.353846153846154,-0.338461538461538,-0.323076923076923,-0.307692307692308,
-0.292307692307692,-0.276923076923077,-0.261538461538462,-0.246153846153846,
-0.230769230769231,-0.215384615384615,-0.2,-0.184615384615385,-0.169230769230769,
-0.153846153846154,-0.138461538461538,-0.123076923076923,-0.107692307692308,
-0.0923076923076923,-0.0769230769230769,-0.0615384615384615,-0.0461538461538462,
-0.0307692307692308,-0.0153846153846154,-0.00577184337451626),
 .UNSPECIFIED.)
CURVE()
GEOMETRIC_REPRESENTATION_ITEM()
RATIONAL_B_SPLINE_CURVE((1.,1.,1.,1.,1.,1.,1.,1.,1.,1.,1.,1.,1.,1.,1.,1.,
1.,1.,1.,1.,1.,1.,1.,1.,1.,1.,1.,1.,1.,1.,1.,1.,1.,1.,1.,1.,1.,1.,1.,1.,
1.,1.,1.,1.,1.,1.,1.,1.,1.,1.,1.,1.,1.,1.,1.,1.,1.,1.,1.,1.,1.,1.,1.,1.,
1.,1.,1.,1.,1.,1.))
REPRESENTATION_ITEM('')
);
#444=(
BOUNDED_CURVE()
B_SPLINE_CURVE(5,(#62918,#62919,#62920,#62921,#62922,#62923,#62924,#62925,
#62926,#62927,#62928,#62929,#62930,#62931,#62932,#62933,#62934,#62935,#62936,
#62937,#62938,#62939,#62940,#62941,#62942,#62943,#62944,#62945,#62946,#62947,
#62948,#62949,#62950,#62951,#62952,#62953,#62954,#62955,#62956,#62957,#62958,
#62959,#62960,#62961,#62962,#62963,#62964,#62965,#62966,#62967,#62968,#62969,
#62970,#62971,#62972,#62973,#62974,#62975,#62976,#62977,#62978,#62979,#62980,
#62981,#62982,#62983,#62984,#62985,#62986,#62987),.UNSPECIFIED.,.F.,.F.)
B_SPLINE_CURVE_WITH_KNOTS((6,1,1,1,1,1,1,1,1,1,1,1,1,1,1,1,1,1,1,1,1,1,
1,1,1,1,1,1,1,1,1,1,1,1,1,1,1,1,1,1,1,1,1,1,1,1,1,1,1,1,1,1,1,1,1,1,1,1,
1,1,1,1,1,1,1,6),(-0.994228156739708,-0.984615384615383,-0.969230769230768,
-0.953846153846152,-0.938461538461537,-0.923076923076922,-0.907692307692306,
-0.892307692307691,-0.876923076923076,-0.86153846153846,-0.846153846153845,
-0.83076923076923,-0.815384615384614,-0.799999999999999,-0.784615384615384,
-0.769230769230768,-0.753846153846153,-0.738461538461538,-0.723076923076922,
-0.707692307692307,-0.692307692307692,-0.676923076923076,-0.661538461538461,
-0.646153846153846,-0.63076923076923,-0.615384615384615,-0.6,-0.584615384615384,
-0.569230769230769,-0.553846153846154,-0.538461538461538,-0.523076923076923,
-0.507692307692308,-0.492307692307692,-0.476923076923077,-0.461538461538462,
-0.446153846153846,-0.430769230769231,-0.415384615384615,-0.4,-0.384615384615385,
-0.369230769230769,-0.353846153846154,-0.338461538461538,-0.323076923076923,
-0.307692307692308,-0.292307692307692,-0.276923076923077,-0.261538461538462,
-0.246153846153846,-0.230769230769231,-0.215384615384615,-0.2,-0.184615384615385,
-0.169230769230769,-0.153846153846154,-0.138461538461538,-0.123076923076923,
-0.107692307692308,-0.0923076923076923,-0.0769230769230769,-0.0615384615384615,
-0.0461538461538462,-0.0307692307692308,-0.0153846153846154,0.),
 .UNSPECIFIED.)
CURVE()
GEOMETRIC_REPRESENTATION_ITEM()
RATIONAL_B_SPLINE_CURVE((1.,1.,1.,1.,1.,1.,1.,1.,1.,1.,1.,1.,1.,1.,1.,1.,
1.,1.,1.,1.,1.,1.,1.,1.,1.,1.,1.,1.,1.,1.,1.,1.,1.,1.,1.,1.,1.,1.,1.,1.,
1.,1.,1.,1.,1.,1.,1.,1.,1.,1.,1.,1.,1.,1.,1.,1.,1.,1.,1.,1.,1.,1.,1.,1.,
1.,1.,1.,1.,1.,1.))
REPRESENTATION_ITEM('')
);
#445=(
BOUNDED_CURVE()
B_SPLINE_CURVE(5,(#63140,#63141,#63142,#63143,#63144,#63145,#63146,#63147,
#63148,#63149,#63150,#63151,#63152,#63153,#63154,#63155,#63156,#63157,#63158,
#63159,#63160,#63161,#63162,#63163,#63164,#63165,#63166,#63167,#63168,#63169,
#63170,#63171,#63172,#63173,#63174,#63175,#63176,#63177,#63178,#63179,#63180,
#63181,#63182,#63183,#63184,#63185,#63186,#63187,#63188,#63189,#63190,#63191,
#63192,#63193,#63194,#63195,#63196,#63197,#63198,#63199,#63200,#63201,#63202,
#63203,#63204,#63205,#63206,#63207,#63208,#63209),.UNSPECIFIED.,.F.,.F.)
B_SPLINE_CURVE_WITH_KNOTS((6,1,1,1,1,1,1,1,1,1,1,1,1,1,1,1,1,1,1,1,1,1,
1,1,1,1,1,1,1,1,1,1,1,1,1,1,1,1,1,1,1,1,1,1,1,1,1,1,1,1,1,1,1,1,1,1,1,1,
1,1,1,1,1,1,1,6),(-1.,-0.984615384615383,-0.969230769230768,-0.953846153846152,
-0.938461538461537,-0.923076923076922,-0.907692307692306,-0.892307692307691,
-0.876923076923076,-0.86153846153846,-0.846153846153845,-0.83076923076923,
-0.815384615384614,-0.799999999999999,-0.784615384615384,-0.769230769230768,
-0.753846153846153,-0.738461538461538,-0.723076923076922,-0.707692307692307,
-0.692307692307692,-0.676923076923076,-0.661538461538461,-0.646153846153846,
-0.63076923076923,-0.615384615384615,-0.6,-0.584615384615384,-0.569230769230769,
-0.553846153846154,-0.538461538461538,-0.523076923076923,-0.507692307692308,
-0.492307692307692,-0.476923076923077,-0.461538461538462,-0.446153846153846,
-0.430769230769231,-0.415384615384615,-0.4,-0.384615384615385,-0.369230769230769,
-0.353846153846154,-0.338461538461538,-0.323076923076923,-0.307692307692308,
-0.292307692307692,-0.276923076923077,-0.261538461538462,-0.246153846153846,
-0.230769230769231,-0.215384615384615,-0.2,-0.184615384615385,-0.169230769230769,
-0.153846153846154,-0.138461538461538,-0.123076923076923,-0.107692307692308,
-0.0923076923076923,-0.0769230769230769,-0.0615384615384615,-0.0461538461538462,
-0.0307692307692308,-0.0153846153846154,-0.00577184337451372),
 .UNSPECIFIED.)
CURVE()
GEOMETRIC_REPRESENTATION_ITEM()
RATIONAL_B_SPLINE_CURVE((1.,1.,1.,1.,1.,1.,1.,1.,1.,1.,1.,1.,1.,1.,1.,1.,
1.,1.,1.,1.,1.,1.,1.,1.,1.,1.,1.,1.,1.,1.,1.,1.,1.,1.,1.,1.,1.,1.,1.,1.,
1.,1.,1.,1.,1.,1.,1.,1.,1.,1.,1.,1.,1.,1.,1.,1.,1.,1.,1.,1.,1.,1.,1.,1.,
1.,1.,1.,1.,1.,1.))
REPRESENTATION_ITEM('')
);
#446=(
BOUNDED_CURVE()
B_SPLINE_CURVE(5,(#63360,#63361,#63362,#63363,#63364,#63365,#63366,#63367,
#63368,#63369,#63370,#63371,#63372,#63373,#63374,#63375,#63376,#63377,#63378,
#63379,#63380,#63381,#63382,#63383,#63384,#63385,#63386,#63387,#63388,#63389,
#63390,#63391,#63392,#63393,#63394,#63395,#63396,#63397,#63398,#63399,#63400,
#63401,#63402,#63403,#63404,#63405,#63406,#63407,#63408,#63409,#63410,#63411,
#63412,#63413,#63414,#63415,#63416,#63417,#63418,#63419,#63420,#63421,#63422,
#63423,#63424,#63425,#63426,#63427,#63428,#63429),.UNSPECIFIED.,.F.,.F.)
B_SPLINE_CURVE_WITH_KNOTS((6,1,1,1,1,1,1,1,1,1,1,1,1,1,1,1,1,1,1,1,1,1,
1,1,1,1,1,1,1,1,1,1,1,1,1,1,1,1,1,1,1,1,1,1,1,1,1,1,1,1,1,1,1,1,1,1,1,1,
1,1,1,1,1,1,1,6),(-0.994228156739703,-0.984615384615383,-0.969230769230768,
-0.953846153846152,-0.938461538461537,-0.923076923076922,-0.907692307692306,
-0.892307692307691,-0.876923076923076,-0.86153846153846,-0.846153846153845,
-0.83076923076923,-0.815384615384614,-0.799999999999999,-0.784615384615384,
-0.769230769230768,-0.753846153846153,-0.738461538461538,-0.723076923076922,
-0.707692307692307,-0.692307692307692,-0.676923076923076,-0.661538461538461,
-0.646153846153846,-0.63076923076923,-0.615384615384615,-0.6,-0.584615384615384,
-0.569230769230769,-0.553846153846154,-0.538461538461538,-0.523076923076923,
-0.507692307692308,-0.492307692307692,-0.476923076923077,-0.461538461538462,
-0.446153846153846,-0.430769230769231,-0.415384615384615,-0.4,-0.384615384615385,
-0.369230769230769,-0.353846153846154,-0.338461538461538,-0.323076923076923,
-0.307692307692308,-0.292307692307692,-0.276923076923077,-0.261538461538462,
-0.246153846153846,-0.230769230769231,-0.215384615384615,-0.2,-0.184615384615385,
-0.169230769230769,-0.153846153846154,-0.138461538461538,-0.123076923076923,
-0.107692307692308,-0.0923076923076923,-0.0769230769230769,-0.0615384615384615,
-0.0461538461538462,-0.0307692307692308,-0.0153846153846154,0.),
 .UNSPECIFIED.)
CURVE()
GEOMETRIC_REPRESENTATION_ITEM()
RATIONAL_B_SPLINE_CURVE((1.,1.,1.,1.,1.,1.,1.,1.,1.,1.,1.,1.,1.,1.,1.,1.,
1.,1.,1.,1.,1.,1.,1.,1.,1.,1.,1.,1.,1.,1.,1.,1.,1.,1.,1.,1.,1.,1.,1.,1.,
1.,1.,1.,1.,1.,1.,1.,1.,1.,1.,1.,1.,1.,1.,1.,1.,1.,1.,1.,1.,1.,1.,1.,1.,
1.,1.,1.,1.,1.,1.))
REPRESENTATION_ITEM('')
);
#447=(
BOUNDED_CURVE()
B_SPLINE_CURVE(5,(#63582,#63583,#63584,#63585,#63586,#63587,#63588,#63589,
#63590,#63591,#63592,#63593,#63594,#63595,#63596,#63597,#63598,#63599,#63600,
#63601,#63602,#63603,#63604,#63605,#63606,#63607,#63608,#63609,#63610,#63611,
#63612,#63613,#63614,#63615,#63616,#63617,#63618,#63619,#63620,#63621,#63622,
#63623,#63624,#63625,#63626,#63627,#63628,#63629,#63630,#63631,#63632,#63633,
#63634,#63635,#63636,#63637,#63638,#63639,#63640,#63641,#63642,#63643,#63644,
#63645,#63646,#63647,#63648,#63649,#63650,#63651),.UNSPECIFIED.,.F.,.F.)
B_SPLINE_CURVE_WITH_KNOTS((6,1,1,1,1,1,1,1,1,1,1,1,1,1,1,1,1,1,1,1,1,1,
1,1,1,1,1,1,1,1,1,1,1,1,1,1,1,1,1,1,1,1,1,1,1,1,1,1,1,1,1,1,1,1,1,1,1,1,
1,1,1,1,1,1,1,6),(-1.,-0.984615384615383,-0.969230769230768,-0.953846153846152,
-0.938461538461537,-0.923076923076922,-0.907692307692306,-0.892307692307691,
-0.876923076923076,-0.86153846153846,-0.846153846153845,-0.83076923076923,
-0.815384615384614,-0.799999999999999,-0.784615384615384,-0.769230769230768,
-0.753846153846153,-0.738461538461538,-0.723076923076922,-0.707692307692307,
-0.692307692307692,-0.676923076923076,-0.661538461538461,-0.646153846153846,
-0.63076923076923,-0.615384615384615,-0.6,-0.584615384615384,-0.569230769230769,
-0.553846153846154,-0.538461538461538,-0.523076923076923,-0.507692307692308,
-0.492307692307692,-0.476923076923077,-0.461538461538462,-0.446153846153846,
-0.430769230769231,-0.415384615384615,-0.4,-0.384615384615385,-0.369230769230769,
-0.353846153846154,-0.338461538461538,-0.323076923076923,-0.307692307692308,
-0.292307692307692,-0.276923076923077,-0.261538461538462,-0.246153846153846,
-0.230769230769231,-0.215384615384615,-0.2,-0.184615384615385,-0.169230769230769,
-0.153846153846154,-0.138461538461538,-0.123076923076923,-0.107692307692308,
-0.0923076923076923,-0.0769230769230769,-0.0615384615384615,-0.0461538461538462,
-0.0307692307692308,-0.0153846153846154,-0.00577184337451698),
 .UNSPECIFIED.)
CURVE()
GEOMETRIC_REPRESENTATION_ITEM()
RATIONAL_B_SPLINE_CURVE((1.,1.,1.,1.,1.,1.,1.,1.,1.,1.,1.,1.,1.,1.,1.,1.,
1.,1.,1.,1.,1.,1.,1.,1.,1.,1.,1.,1.,1.,1.,1.,1.,1.,1.,1.,1.,1.,1.,1.,1.,
1.,1.,1.,1.,1.,1.,1.,1.,1.,1.,1.,1.,1.,1.,1.,1.,1.,1.,1.,1.,1.,1.,1.,1.,
1.,1.,1.,1.,1.,1.))
REPRESENTATION_ITEM('')
);
#448=(
BOUNDED_CURVE()
B_SPLINE_CURVE(5,(#63802,#63803,#63804,#63805,#63806,#63807,#63808,#63809,
#63810,#63811,#63812,#63813,#63814,#63815,#63816,#63817,#63818,#63819,#63820,
#63821,#63822,#63823,#63824,#63825,#63826,#63827,#63828,#63829,#63830,#63831,
#63832,#63833,#63834,#63835,#63836,#63837,#63838,#63839,#63840,#63841,#63842,
#63843,#63844,#63845,#63846,#63847,#63848,#63849,#63850,#63851,#63852,#63853,
#63854,#63855,#63856,#63857,#63858,#63859,#63860,#63861,#63862,#63863,#63864,
#63865,#63866,#63867,#63868,#63869,#63870,#63871),.UNSPECIFIED.,.F.,.F.)
B_SPLINE_CURVE_WITH_KNOTS((6,1,1,1,1,1,1,1,1,1,1,1,1,1,1,1,1,1,1,1,1,1,
1,1,1,1,1,1,1,1,1,1,1,1,1,1,1,1,1,1,1,1,1,1,1,1,1,1,1,1,1,1,1,1,1,1,1,1,
1,1,1,1,1,1,1,6),(-0.994228156739706,-0.984615384615383,-0.969230769230768,
-0.953846153846152,-0.938461538461537,-0.923076923076922,-0.907692307692306,
-0.892307692307691,-0.876923076923076,-0.86153846153846,-0.846153846153845,
-0.83076923076923,-0.815384615384614,-0.799999999999999,-0.784615384615384,
-0.769230769230768,-0.753846153846153,-0.738461538461538,-0.723076923076922,
-0.707692307692307,-0.692307692307692,-0.676923076923076,-0.661538461538461,
-0.646153846153846,-0.63076923076923,-0.615384615384615,-0.6,-0.584615384615384,
-0.569230769230769,-0.553846153846154,-0.538461538461538,-0.523076923076923,
-0.507692307692308,-0.492307692307692,-0.476923076923077,-0.461538461538462,
-0.446153846153846,-0.430769230769231,-0.415384615384615,-0.4,-0.384615384615385,
-0.369230769230769,-0.353846153846154,-0.338461538461538,-0.323076923076923,
-0.307692307692308,-0.292307692307692,-0.276923076923077,-0.261538461538462,
-0.246153846153846,-0.230769230769231,-0.215384615384615,-0.2,-0.184615384615385,
-0.169230769230769,-0.153846153846154,-0.138461538461538,-0.123076923076923,
-0.107692307692308,-0.0923076923076923,-0.0769230769230769,-0.0615384615384615,
-0.0461538461538462,-0.0307692307692308,-0.0153846153846154,0.),
 .UNSPECIFIED.)
CURVE()
GEOMETRIC_REPRESENTATION_ITEM()
RATIONAL_B_SPLINE_CURVE((1.,1.,1.,1.,1.,1.,1.,1.,1.,1.,1.,1.,1.,1.,1.,1.,
1.,1.,1.,1.,1.,1.,1.,1.,1.,1.,1.,1.,1.,1.,1.,1.,1.,1.,1.,1.,1.,1.,1.,1.,
1.,1.,1.,1.,1.,1.,1.,1.,1.,1.,1.,1.,1.,1.,1.,1.,1.,1.,1.,1.,1.,1.,1.,1.,
1.,1.,1.,1.,1.,1.))
REPRESENTATION_ITEM('')
);
#449=(
BOUNDED_CURVE()
B_SPLINE_CURVE(5,(#64024,#64025,#64026,#64027,#64028,#64029,#64030,#64031,
#64032,#64033,#64034,#64035,#64036,#64037,#64038,#64039,#64040,#64041,#64042,
#64043,#64044,#64045,#64046,#64047,#64048,#64049,#64050,#64051,#64052,#64053,
#64054,#64055,#64056,#64057,#64058,#64059,#64060,#64061,#64062,#64063,#64064,
#64065,#64066,#64067,#64068,#64069,#64070,#64071,#64072,#64073,#64074,#64075,
#64076,#64077,#64078,#64079,#64080,#64081,#64082,#64083,#64084,#64085,#64086,
#64087,#64088,#64089,#64090,#64091,#64092,#64093),.UNSPECIFIED.,.F.,.F.)
B_SPLINE_CURVE_WITH_KNOTS((6,1,1,1,1,1,1,1,1,1,1,1,1,1,1,1,1,1,1,1,1,1,
1,1,1,1,1,1,1,1,1,1,1,1,1,1,1,1,1,1,1,1,1,1,1,1,1,1,1,1,1,1,1,1,1,1,1,1,
1,1,1,1,1,1,1,6),(-1.,-0.984615384615383,-0.969230769230768,-0.953846153846152,
-0.938461538461537,-0.923076923076922,-0.907692307692306,-0.892307692307691,
-0.876923076923076,-0.86153846153846,-0.846153846153845,-0.83076923076923,
-0.815384615384614,-0.799999999999999,-0.784615384615384,-0.769230769230768,
-0.753846153846153,-0.738461538461538,-0.723076923076922,-0.707692307692307,
-0.692307692307692,-0.676923076923076,-0.661538461538461,-0.646153846153846,
-0.63076923076923,-0.615384615384615,-0.6,-0.584615384615384,-0.569230769230769,
-0.553846153846154,-0.538461538461538,-0.523076923076923,-0.507692307692308,
-0.492307692307692,-0.476923076923077,-0.461538461538462,-0.446153846153846,
-0.430769230769231,-0.415384615384615,-0.4,-0.384615384615385,-0.369230769230769,
-0.353846153846154,-0.338461538461538,-0.323076923076923,-0.307692307692308,
-0.292307692307692,-0.276923076923077,-0.261538461538462,-0.246153846153846,
-0.230769230769231,-0.215384615384615,-0.2,-0.184615384615385,-0.169230769230769,
-0.153846153846154,-0.138461538461538,-0.123076923076923,-0.107692307692308,
-0.0923076923076923,-0.0769230769230769,-0.0615384615384615,-0.0461538461538462,
-0.0307692307692308,-0.0153846153846154,-0.00577184337452512),
 .UNSPECIFIED.)
CURVE()
GEOMETRIC_REPRESENTATION_ITEM()
RATIONAL_B_SPLINE_CURVE((1.,1.,1.,1.,1.,1.,1.,1.,1.,1.,1.,1.,1.,1.,1.,1.,
1.,1.,1.,1.,1.,1.,1.,1.,1.,1.,1.,1.,1.,1.,1.,1.,1.,1.,1.,1.,1.,1.,1.,1.,
1.,1.,1.,1.,1.,1.,1.,1.,1.,1.,1.,1.,1.,1.,1.,1.,1.,1.,1.,1.,1.,1.,1.,1.,
1.,1.,1.,1.,1.,1.))
REPRESENTATION_ITEM('')
);
#450=(
BOUNDED_CURVE()
B_SPLINE_CURVE(5,(#64244,#64245,#64246,#64247,#64248,#64249,#64250,#64251,
#64252,#64253,#64254,#64255,#64256,#64257,#64258,#64259,#64260,#64261,#64262,
#64263,#64264,#64265,#64266,#64267,#64268,#64269,#64270,#64271,#64272,#64273,
#64274,#64275,#64276,#64277,#64278,#64279,#64280,#64281,#64282,#64283,#64284,
#64285,#64286,#64287,#64288,#64289,#64290,#64291,#64292,#64293,#64294,#64295,
#64296,#64297,#64298,#64299,#64300,#64301,#64302,#64303,#64304,#64305,#64306,
#64307,#64308,#64309,#64310,#64311,#64312,#64313),.UNSPECIFIED.,.F.,.F.)
B_SPLINE_CURVE_WITH_KNOTS((6,1,1,1,1,1,1,1,1,1,1,1,1,1,1,1,1,1,1,1,1,1,
1,1,1,1,1,1,1,1,1,1,1,1,1,1,1,1,1,1,1,1,1,1,1,1,1,1,1,1,1,1,1,1,1,1,1,1,
1,1,1,1,1,1,1,6),(-0.994228156739713,-0.984615384615383,-0.969230769230768,
-0.953846153846152,-0.938461538461537,-0.923076923076922,-0.907692307692306,
-0.892307692307691,-0.876923076923076,-0.86153846153846,-0.846153846153845,
-0.83076923076923,-0.815384615384614,-0.799999999999999,-0.784615384615384,
-0.769230769230768,-0.753846153846153,-0.738461538461538,-0.723076923076922,
-0.707692307692307,-0.692307692307692,-0.676923076923076,-0.661538461538461,
-0.646153846153846,-0.63076923076923,-0.615384615384615,-0.6,-0.584615384615384,
-0.569230769230769,-0.553846153846154,-0.538461538461538,-0.523076923076923,
-0.507692307692308,-0.492307692307692,-0.476923076923077,-0.461538461538462,
-0.446153846153846,-0.430769230769231,-0.415384615384615,-0.4,-0.384615384615385,
-0.369230769230769,-0.353846153846154,-0.338461538461538,-0.323076923076923,
-0.307692307692308,-0.292307692307692,-0.276923076923077,-0.261538461538462,
-0.246153846153846,-0.230769230769231,-0.215384615384615,-0.2,-0.184615384615385,
-0.169230769230769,-0.153846153846154,-0.138461538461538,-0.123076923076923,
-0.107692307692308,-0.0923076923076923,-0.0769230769230769,-0.0615384615384615,
-0.0461538461538462,-0.0307692307692308,-0.0153846153846154,0.),
 .UNSPECIFIED.)
CURVE()
GEOMETRIC_REPRESENTATION_ITEM()
RATIONAL_B_SPLINE_CURVE((1.,1.,1.,1.,1.,1.,1.,1.,1.,1.,1.,1.,1.,1.,1.,1.,
1.,1.,1.,1.,1.,1.,1.,1.,1.,1.,1.,1.,1.,1.,1.,1.,1.,1.,1.,1.,1.,1.,1.,1.,
1.,1.,1.,1.,1.,1.,1.,1.,1.,1.,1.,1.,1.,1.,1.,1.,1.,1.,1.,1.,1.,1.,1.,1.,
1.,1.,1.,1.,1.,1.))
REPRESENTATION_ITEM('')
);
#451=(
BOUNDED_CURVE()
B_SPLINE_CURVE(5,(#64466,#64467,#64468,#64469,#64470,#64471,#64472,#64473,
#64474,#64475,#64476,#64477,#64478,#64479,#64480,#64481,#64482,#64483,#64484,
#64485,#64486,#64487,#64488,#64489,#64490,#64491,#64492,#64493,#64494,#64495,
#64496,#64497,#64498,#64499,#64500,#64501,#64502,#64503,#64504,#64505,#64506,
#64507,#64508,#64509,#64510,#64511,#64512,#64513,#64514,#64515,#64516,#64517,
#64518,#64519,#64520,#64521,#64522,#64523,#64524,#64525,#64526,#64527,#64528,
#64529,#64530,#64531,#64532,#64533,#64534,#64535),.UNSPECIFIED.,.F.,.F.)
B_SPLINE_CURVE_WITH_KNOTS((6,1,1,1,1,1,1,1,1,1,1,1,1,1,1,1,1,1,1,1,1,1,
1,1,1,1,1,1,1,1,1,1,1,1,1,1,1,1,1,1,1,1,1,1,1,1,1,1,1,1,1,1,1,1,1,1,1,1,
1,1,1,1,1,1,1,6),(-1.,-0.984615384615383,-0.969230769230768,-0.953846153846152,
-0.938461538461537,-0.923076923076922,-0.907692307692306,-0.892307692307691,
-0.876923076923076,-0.86153846153846,-0.846153846153845,-0.83076923076923,
-0.815384615384614,-0.799999999999999,-0.784615384615384,-0.769230769230768,
-0.753846153846153,-0.738461538461538,-0.723076923076922,-0.707692307692307,
-0.692307692307692,-0.676923076923076,-0.661538461538461,-0.646153846153846,
-0.63076923076923,-0.615384615384615,-0.6,-0.584615384615384,-0.569230769230769,
-0.553846153846154,-0.538461538461538,-0.523076923076923,-0.507692307692308,
-0.492307692307692,-0.476923076923077,-0.461538461538462,-0.446153846153846,
-0.430769230769231,-0.415384615384615,-0.4,-0.384615384615385,-0.369230769230769,
-0.353846153846154,-0.338461538461538,-0.323076923076923,-0.307692307692308,
-0.292307692307692,-0.276923076923077,-0.261538461538462,-0.246153846153846,
-0.230769230769231,-0.215384615384615,-0.2,-0.184615384615385,-0.169230769230769,
-0.153846153846154,-0.138461538461538,-0.123076923076923,-0.107692307692308,
-0.0923076923076923,-0.0769230769230769,-0.0615384615384615,-0.0461538461538462,
-0.0307692307692308,-0.0153846153846154,-0.00577184337450204),
 .UNSPECIFIED.)
CURVE()
GEOMETRIC_REPRESENTATION_ITEM()
RATIONAL_B_SPLINE_CURVE((1.,1.,1.,1.,1.,1.,1.,1.,1.,1.,1.,1.,1.,1.,1.,1.,
1.,1.,1.,1.,1.,1.,1.,1.,1.,1.,1.,1.,1.,1.,1.,1.,1.,1.,1.,1.,1.,1.,1.,1.,
1.,1.,1.,1.,1.,1.,1.,1.,1.,1.,1.,1.,1.,1.,1.,1.,1.,1.,1.,1.,1.,1.,1.,1.,
1.,1.,1.,1.,1.,1.))
REPRESENTATION_ITEM('')
);
#452=(
BOUNDED_CURVE()
B_SPLINE_CURVE(5,(#64686,#64687,#64688,#64689,#64690,#64691,#64692,#64693,
#64694,#64695,#64696,#64697,#64698,#64699,#64700,#64701,#64702,#64703,#64704,
#64705,#64706,#64707,#64708,#64709,#64710,#64711,#64712,#64713,#64714,#64715,
#64716,#64717,#64718,#64719,#64720,#64721,#64722,#64723,#64724,#64725,#64726,
#64727,#64728,#64729,#64730,#64731,#64732,#64733,#64734,#64735,#64736,#64737,
#64738,#64739,#64740,#64741,#64742,#64743,#64744,#64745,#64746,#64747,#64748,
#64749,#64750,#64751,#64752,#64753,#64754,#64755),.UNSPECIFIED.,.F.,.F.)
B_SPLINE_CURVE_WITH_KNOTS((6,1,1,1,1,1,1,1,1,1,1,1,1,1,1,1,1,1,1,1,1,1,
1,1,1,1,1,1,1,1,1,1,1,1,1,1,1,1,1,1,1,1,1,1,1,1,1,1,1,1,1,1,1,1,1,1,1,1,
1,1,1,1,1,1,1,6),(-0.99422815673972,-0.984615384615383,-0.969230769230768,
-0.953846153846152,-0.938461538461537,-0.923076923076922,-0.907692307692306,
-0.892307692307691,-0.876923076923076,-0.86153846153846,-0.846153846153845,
-0.83076923076923,-0.815384615384614,-0.799999999999999,-0.784615384615384,
-0.769230769230768,-0.753846153846153,-0.738461538461538,-0.723076923076922,
-0.707692307692307,-0.692307692307692,-0.676923076923076,-0.661538461538461,
-0.646153846153846,-0.63076923076923,-0.615384615384615,-0.6,-0.584615384615384,
-0.569230769230769,-0.553846153846154,-0.538461538461538,-0.523076923076923,
-0.507692307692308,-0.492307692307692,-0.476923076923077,-0.461538461538462,
-0.446153846153846,-0.430769230769231,-0.415384615384615,-0.4,-0.384615384615385,
-0.369230769230769,-0.353846153846154,-0.338461538461538,-0.323076923076923,
-0.307692307692308,-0.292307692307692,-0.276923076923077,-0.261538461538462,
-0.246153846153846,-0.230769230769231,-0.215384615384615,-0.2,-0.184615384615385,
-0.169230769230769,-0.153846153846154,-0.138461538461538,-0.123076923076923,
-0.107692307692308,-0.0923076923076923,-0.0769230769230769,-0.0615384615384615,
-0.0461538461538462,-0.0307692307692308,-0.0153846153846154,0.),
 .UNSPECIFIED.)
CURVE()
GEOMETRIC_REPRESENTATION_ITEM()
RATIONAL_B_SPLINE_CURVE((1.,1.,1.,1.,1.,1.,1.,1.,1.,1.,1.,1.,1.,1.,1.,1.,
1.,1.,1.,1.,1.,1.,1.,1.,1.,1.,1.,1.,1.,1.,1.,1.,1.,1.,1.,1.,1.,1.,1.,1.,
1.,1.,1.,1.,1.,1.,1.,1.,1.,1.,1.,1.,1.,1.,1.,1.,1.,1.,1.,1.,1.,1.,1.,1.,
1.,1.,1.,1.,1.,1.))
REPRESENTATION_ITEM('')
);
#453=(
BOUNDED_CURVE()
B_SPLINE_CURVE(5,(#64908,#64909,#64910,#64911,#64912,#64913,#64914,#64915,
#64916,#64917,#64918,#64919,#64920,#64921,#64922,#64923,#64924,#64925,#64926,
#64927,#64928,#64929,#64930,#64931,#64932,#64933,#64934,#64935,#64936,#64937,
#64938,#64939,#64940,#64941,#64942,#64943,#64944,#64945,#64946,#64947,#64948,
#64949,#64950,#64951,#64952,#64953,#64954,#64955,#64956,#64957,#64958,#64959,
#64960,#64961,#64962,#64963,#64964,#64965,#64966,#64967,#64968,#64969,#64970,
#64971,#64972,#64973,#64974,#64975,#64976,#64977),.UNSPECIFIED.,.F.,.F.)
B_SPLINE_CURVE_WITH_KNOTS((6,1,1,1,1,1,1,1,1,1,1,1,1,1,1,1,1,1,1,1,1,1,
1,1,1,1,1,1,1,1,1,1,1,1,1,1,1,1,1,1,1,1,1,1,1,1,1,1,1,1,1,1,1,1,1,1,1,1,
1,1,1,1,1,1,1,6),(-1.,-0.984615384615383,-0.969230769230768,-0.953846153846152,
-0.938461538461537,-0.923076923076922,-0.907692307692306,-0.892307692307691,
-0.876923076923076,-0.86153846153846,-0.846153846153845,-0.83076923076923,
-0.815384615384614,-0.799999999999999,-0.784615384615384,-0.769230769230768,
-0.753846153846153,-0.738461538461538,-0.723076923076922,-0.707692307692307,
-0.692307692307692,-0.676923076923076,-0.661538461538461,-0.646153846153846,
-0.63076923076923,-0.615384615384615,-0.6,-0.584615384615384,-0.569230769230769,
-0.553846153846154,-0.538461538461538,-0.523076923076923,-0.507692307692308,
-0.492307692307692,-0.476923076923077,-0.461538461538462,-0.446153846153846,
-0.430769230769231,-0.415384615384615,-0.4,-0.384615384615385,-0.369230769230769,
-0.353846153846154,-0.338461538461538,-0.323076923076923,-0.307692307692308,
-0.292307692307692,-0.276923076923077,-0.261538461538462,-0.246153846153846,
-0.230769230769231,-0.215384615384615,-0.2,-0.184615384615385,-0.169230769230769,
-0.153846153846154,-0.138461538461538,-0.123076923076923,-0.107692307692308,
-0.0923076923076923,-0.0769230769230769,-0.0615384615384615,-0.0461538461538462,
-0.0307692307692308,-0.0153846153846154,-0.0057718433745107),
 .UNSPECIFIED.)
CURVE()
GEOMETRIC_REPRESENTATION_ITEM()
RATIONAL_B_SPLINE_CURVE((1.,1.,1.,1.,1.,1.,1.,1.,1.,1.,1.,1.,1.,1.,1.,1.,
1.,1.,1.,1.,1.,1.,1.,1.,1.,1.,1.,1.,1.,1.,1.,1.,1.,1.,1.,1.,1.,1.,1.,1.,
1.,1.,1.,1.,1.,1.,1.,1.,1.,1.,1.,1.,1.,1.,1.,1.,1.,1.,1.,1.,1.,1.,1.,1.,
1.,1.,1.,1.,1.,1.))
REPRESENTATION_ITEM('')
);
#454=(
BOUNDED_CURVE()
B_SPLINE_CURVE(5,(#65128,#65129,#65130,#65131,#65132,#65133,#65134,#65135,
#65136,#65137,#65138,#65139,#65140,#65141,#65142,#65143,#65144,#65145,#65146,
#65147,#65148,#65149,#65150,#65151,#65152,#65153,#65154,#65155,#65156,#65157,
#65158,#65159,#65160,#65161,#65162,#65163,#65164,#65165,#65166,#65167,#65168,
#65169,#65170,#65171,#65172,#65173,#65174,#65175,#65176,#65177,#65178,#65179,
#65180,#65181,#65182,#65183,#65184,#65185,#65186,#65187,#65188,#65189,#65190,
#65191,#65192,#65193,#65194,#65195,#65196,#65197),.UNSPECIFIED.,.F.,.F.)
B_SPLINE_CURVE_WITH_KNOTS((6,1,1,1,1,1,1,1,1,1,1,1,1,1,1,1,1,1,1,1,1,1,
1,1,1,1,1,1,1,1,1,1,1,1,1,1,1,1,1,1,1,1,1,1,1,1,1,1,1,1,1,1,1,1,1,1,1,1,
1,1,1,1,1,1,1,6),(-0.994228156739708,-0.984615384615383,-0.969230769230768,
-0.953846153846152,-0.938461538461537,-0.923076923076922,-0.907692307692306,
-0.892307692307691,-0.876923076923076,-0.86153846153846,-0.846153846153845,
-0.83076923076923,-0.815384615384614,-0.799999999999999,-0.784615384615384,
-0.769230769230768,-0.753846153846153,-0.738461538461538,-0.723076923076922,
-0.707692307692307,-0.692307692307692,-0.676923076923076,-0.661538461538461,
-0.646153846153846,-0.63076923076923,-0.615384615384615,-0.6,-0.584615384615384,
-0.569230769230769,-0.553846153846154,-0.538461538461538,-0.523076923076923,
-0.507692307692308,-0.492307692307692,-0.476923076923077,-0.461538461538462,
-0.446153846153846,-0.430769230769231,-0.415384615384615,-0.4,-0.384615384615385,
-0.369230769230769,-0.353846153846154,-0.338461538461538,-0.323076923076923,
-0.307692307692308,-0.292307692307692,-0.276923076923077,-0.261538461538462,
-0.246153846153846,-0.230769230769231,-0.215384615384615,-0.2,-0.184615384615385,
-0.169230769230769,-0.153846153846154,-0.138461538461538,-0.123076923076923,
-0.107692307692308,-0.0923076923076923,-0.0769230769230769,-0.0615384615384615,
-0.0461538461538462,-0.0307692307692308,-0.0153846153846154,0.),
 .UNSPECIFIED.)
CURVE()
GEOMETRIC_REPRESENTATION_ITEM()
RATIONAL_B_SPLINE_CURVE((1.,1.,1.,1.,1.,1.,1.,1.,1.,1.,1.,1.,1.,1.,1.,1.,
1.,1.,1.,1.,1.,1.,1.,1.,1.,1.,1.,1.,1.,1.,1.,1.,1.,1.,1.,1.,1.,1.,1.,1.,
1.,1.,1.,1.,1.,1.,1.,1.,1.,1.,1.,1.,1.,1.,1.,1.,1.,1.,1.,1.,1.,1.,1.,1.,
1.,1.,1.,1.,1.,1.))
REPRESENTATION_ITEM('')
);
#455=(
BOUNDED_CURVE()
B_SPLINE_CURVE(5,(#65350,#65351,#65352,#65353,#65354,#65355,#65356,#65357,
#65358,#65359,#65360,#65361,#65362,#65363,#65364,#65365,#65366,#65367,#65368,
#65369,#65370,#65371,#65372,#65373,#65374,#65375,#65376,#65377,#65378,#65379,
#65380,#65381,#65382,#65383,#65384,#65385,#65386,#65387,#65388,#65389,#65390,
#65391,#65392,#65393,#65394,#65395,#65396,#65397,#65398,#65399,#65400,#65401,
#65402,#65403,#65404,#65405,#65406,#65407,#65408,#65409,#65410,#65411,#65412,
#65413,#65414,#65415,#65416,#65417,#65418,#65419),.UNSPECIFIED.,.F.,.F.)
B_SPLINE_CURVE_WITH_KNOTS((6,1,1,1,1,1,1,1,1,1,1,1,1,1,1,1,1,1,1,1,1,1,
1,1,1,1,1,1,1,1,1,1,1,1,1,1,1,1,1,1,1,1,1,1,1,1,1,1,1,1,1,1,1,1,1,1,1,1,
1,1,1,1,1,1,1,6),(-1.,-0.984615384615383,-0.969230769230768,-0.953846153846152,
-0.938461538461537,-0.923076923076922,-0.907692307692306,-0.892307692307691,
-0.876923076923076,-0.86153846153846,-0.846153846153845,-0.83076923076923,
-0.815384615384614,-0.799999999999999,-0.784615384615384,-0.769230769230768,
-0.753846153846153,-0.738461538461538,-0.723076923076922,-0.707692307692307,
-0.692307692307692,-0.676923076923076,-0.661538461538461,-0.646153846153846,
-0.63076923076923,-0.615384615384615,-0.6,-0.584615384615384,-0.569230769230769,
-0.553846153846154,-0.538461538461538,-0.523076923076923,-0.507692307692308,
-0.492307692307692,-0.476923076923077,-0.461538461538462,-0.446153846153846,
-0.430769230769231,-0.415384615384615,-0.4,-0.384615384615385,-0.369230769230769,
-0.353846153846154,-0.338461538461538,-0.323076923076923,-0.307692307692308,
-0.292307692307692,-0.276923076923077,-0.261538461538462,-0.246153846153846,
-0.230769230769231,-0.215384615384615,-0.2,-0.184615384615385,-0.169230769230769,
-0.153846153846154,-0.138461538461538,-0.123076923076923,-0.107692307692308,
-0.0923076923076923,-0.0769230769230769,-0.0615384615384615,-0.0461538461538462,
-0.0307692307692308,-0.0153846153846154,-0.00577184337451708),
 .UNSPECIFIED.)
CURVE()
GEOMETRIC_REPRESENTATION_ITEM()
RATIONAL_B_SPLINE_CURVE((1.,1.,1.,1.,1.,1.,1.,1.,1.,1.,1.,1.,1.,1.,1.,1.,
1.,1.,1.,1.,1.,1.,1.,1.,1.,1.,1.,1.,1.,1.,1.,1.,1.,1.,1.,1.,1.,1.,1.,1.,
1.,1.,1.,1.,1.,1.,1.,1.,1.,1.,1.,1.,1.,1.,1.,1.,1.,1.,1.,1.,1.,1.,1.,1.,
1.,1.,1.,1.,1.,1.))
REPRESENTATION_ITEM('')
);
#456=(
BOUNDED_CURVE()
B_SPLINE_CURVE(5,(#65570,#65571,#65572,#65573,#65574,#65575,#65576,#65577,
#65578,#65579,#65580,#65581,#65582,#65583,#65584,#65585,#65586,#65587,#65588,
#65589,#65590,#65591,#65592,#65593,#65594,#65595,#65596,#65597,#65598,#65599,
#65600,#65601,#65602,#65603,#65604,#65605,#65606,#65607,#65608,#65609,#65610,
#65611,#65612,#65613,#65614,#65615,#65616,#65617,#65618,#65619,#65620,#65621,
#65622,#65623,#65624,#65625,#65626,#65627,#65628,#65629,#65630,#65631,#65632,
#65633,#65634,#65635,#65636,#65637,#65638,#65639),.UNSPECIFIED.,.F.,.F.)
B_SPLINE_CURVE_WITH_KNOTS((6,1,1,1,1,1,1,1,1,1,1,1,1,1,1,1,1,1,1,1,1,1,
1,1,1,1,1,1,1,1,1,1,1,1,1,1,1,1,1,1,1,1,1,1,1,1,1,1,1,1,1,1,1,1,1,1,1,1,
1,1,1,1,1,1,1,6),(-0.994228156739669,-0.984615384615383,-0.969230769230768,
-0.953846153846152,-0.938461538461537,-0.923076923076922,-0.907692307692306,
-0.892307692307691,-0.876923076923076,-0.86153846153846,-0.846153846153845,
-0.83076923076923,-0.815384615384614,-0.799999999999999,-0.784615384615384,
-0.769230769230768,-0.753846153846153,-0.738461538461538,-0.723076923076922,
-0.707692307692307,-0.692307692307692,-0.676923076923076,-0.661538461538461,
-0.646153846153846,-0.63076923076923,-0.615384615384615,-0.6,-0.584615384615384,
-0.569230769230769,-0.553846153846154,-0.538461538461538,-0.523076923076923,
-0.507692307692308,-0.492307692307692,-0.476923076923077,-0.461538461538462,
-0.446153846153846,-0.430769230769231,-0.415384615384615,-0.4,-0.384615384615385,
-0.369230769230769,-0.353846153846154,-0.338461538461538,-0.323076923076923,
-0.307692307692308,-0.292307692307692,-0.276923076923077,-0.261538461538462,
-0.246153846153846,-0.230769230769231,-0.215384615384615,-0.2,-0.184615384615385,
-0.169230769230769,-0.153846153846154,-0.138461538461538,-0.123076923076923,
-0.107692307692308,-0.0923076923076923,-0.0769230769230769,-0.0615384615384615,
-0.0461538461538462,-0.0307692307692308,-0.0153846153846154,0.),
 .UNSPECIFIED.)
CURVE()
GEOMETRIC_REPRESENTATION_ITEM()
RATIONAL_B_SPLINE_CURVE((1.,1.,1.,1.,1.,1.,1.,1.,1.,1.,1.,1.,1.,1.,1.,1.,
1.,1.,1.,1.,1.,1.,1.,1.,1.,1.,1.,1.,1.,1.,1.,1.,1.,1.,1.,1.,1.,1.,1.,1.,
1.,1.,1.,1.,1.,1.,1.,1.,1.,1.,1.,1.,1.,1.,1.,1.,1.,1.,1.,1.,1.,1.,1.,1.,
1.,1.,1.,1.,1.,1.))
REPRESENTATION_ITEM('')
);
#457=(
BOUNDED_CURVE()
B_SPLINE_CURVE(5,(#65792,#65793,#65794,#65795,#65796,#65797,#65798,#65799,
#65800,#65801,#65802,#65803,#65804,#65805,#65806,#65807,#65808,#65809,#65810,
#65811,#65812,#65813,#65814,#65815,#65816,#65817,#65818,#65819,#65820,#65821,
#65822,#65823,#65824,#65825,#65826,#65827,#65828,#65829,#65830,#65831,#65832,
#65833,#65834,#65835,#65836,#65837,#65838,#65839,#65840,#65841,#65842,#65843,
#65844,#65845,#65846,#65847,#65848,#65849,#65850,#65851,#65852,#65853,#65854,
#65855,#65856,#65857,#65858,#65859,#65860,#65861),.UNSPECIFIED.,.F.,.F.)
B_SPLINE_CURVE_WITH_KNOTS((6,1,1,1,1,1,1,1,1,1,1,1,1,1,1,1,1,1,1,1,1,1,
1,1,1,1,1,1,1,1,1,1,1,1,1,1,1,1,1,1,1,1,1,1,1,1,1,1,1,1,1,1,1,1,1,1,1,1,
1,1,1,1,1,1,1,6),(-1.,-0.984615384615383,-0.969230769230768,-0.953846153846152,
-0.938461538461537,-0.923076923076922,-0.907692307692306,-0.892307692307691,
-0.876923076923076,-0.86153846153846,-0.846153846153845,-0.83076923076923,
-0.815384615384614,-0.799999999999999,-0.784615384615384,-0.769230769230768,
-0.753846153846153,-0.738461538461538,-0.723076923076922,-0.707692307692307,
-0.692307692307692,-0.676923076923076,-0.661538461538461,-0.646153846153846,
-0.63076923076923,-0.615384615384615,-0.6,-0.584615384615384,-0.569230769230769,
-0.553846153846154,-0.538461538461538,-0.523076923076923,-0.507692307692308,
-0.492307692307692,-0.476923076923077,-0.461538461538462,-0.446153846153846,
-0.430769230769231,-0.415384615384615,-0.4,-0.384615384615385,-0.369230769230769,
-0.353846153846154,-0.338461538461538,-0.323076923076923,-0.307692307692308,
-0.292307692307692,-0.276923076923077,-0.261538461538462,-0.246153846153846,
-0.230769230769231,-0.215384615384615,-0.2,-0.184615384615385,-0.169230769230769,
-0.153846153846154,-0.138461538461538,-0.123076923076923,-0.107692307692308,
-0.0923076923076923,-0.0769230769230769,-0.0615384615384615,-0.0461538461538462,
-0.0307692307692308,-0.0153846153846154,-0.0057718433744903),
 .UNSPECIFIED.)
CURVE()
GEOMETRIC_REPRESENTATION_ITEM()
RATIONAL_B_SPLINE_CURVE((1.,1.,1.,1.,1.,1.,1.,1.,1.,1.,1.,1.,1.,1.,1.,1.,
1.,1.,1.,1.,1.,1.,1.,1.,1.,1.,1.,1.,1.,1.,1.,1.,1.,1.,1.,1.,1.,1.,1.,1.,
1.,1.,1.,1.,1.,1.,1.,1.,1.,1.,1.,1.,1.,1.,1.,1.,1.,1.,1.,1.,1.,1.,1.,1.,
1.,1.,1.,1.,1.,1.))
REPRESENTATION_ITEM('')
);
#458=(
BOUNDED_CURVE()
B_SPLINE_CURVE(5,(#66012,#66013,#66014,#66015,#66016,#66017,#66018,#66019,
#66020,#66021,#66022,#66023,#66024,#66025,#66026,#66027,#66028,#66029,#66030,
#66031,#66032,#66033,#66034,#66035,#66036,#66037,#66038,#66039,#66040,#66041,
#66042,#66043,#66044,#66045,#66046,#66047,#66048,#66049,#66050,#66051,#66052,
#66053,#66054,#66055,#66056,#66057,#66058,#66059,#66060,#66061,#66062,#66063,
#66064,#66065,#66066,#66067,#66068,#66069,#66070,#66071,#66072,#66073,#66074,
#66075,#66076,#66077,#66078,#66079,#66080,#66081),.UNSPECIFIED.,.F.,.F.)
B_SPLINE_CURVE_WITH_KNOTS((6,1,1,1,1,1,1,1,1,1,1,1,1,1,1,1,1,1,1,1,1,1,
1,1,1,1,1,1,1,1,1,1,1,1,1,1,1,1,1,1,1,1,1,1,1,1,1,1,1,1,1,1,1,1,1,1,1,1,
1,1,1,1,1,1,1,6),(-0.994228156739712,-0.984615384615383,-0.969230769230768,
-0.953846153846152,-0.938461538461537,-0.923076923076922,-0.907692307692306,
-0.892307692307691,-0.876923076923076,-0.86153846153846,-0.846153846153845,
-0.83076923076923,-0.815384615384614,-0.799999999999999,-0.784615384615384,
-0.769230769230768,-0.753846153846153,-0.738461538461538,-0.723076923076922,
-0.707692307692307,-0.692307692307692,-0.676923076923076,-0.661538461538461,
-0.646153846153846,-0.63076923076923,-0.615384615384615,-0.6,-0.584615384615384,
-0.569230769230769,-0.553846153846154,-0.538461538461538,-0.523076923076923,
-0.507692307692308,-0.492307692307692,-0.476923076923077,-0.461538461538462,
-0.446153846153846,-0.430769230769231,-0.415384615384615,-0.4,-0.384615384615385,
-0.369230769230769,-0.353846153846154,-0.338461538461538,-0.323076923076923,
-0.307692307692308,-0.292307692307692,-0.276923076923077,-0.261538461538462,
-0.246153846153846,-0.230769230769231,-0.215384615384615,-0.2,-0.184615384615385,
-0.169230769230769,-0.153846153846154,-0.138461538461538,-0.123076923076923,
-0.107692307692308,-0.0923076923076923,-0.0769230769230769,-0.0615384615384615,
-0.0461538461538462,-0.0307692307692308,-0.0153846153846154,0.),
 .UNSPECIFIED.)
CURVE()
GEOMETRIC_REPRESENTATION_ITEM()
RATIONAL_B_SPLINE_CURVE((1.,1.,1.,1.,1.,1.,1.,1.,1.,1.,1.,1.,1.,1.,1.,1.,
1.,1.,1.,1.,1.,1.,1.,1.,1.,1.,1.,1.,1.,1.,1.,1.,1.,1.,1.,1.,1.,1.,1.,1.,
1.,1.,1.,1.,1.,1.,1.,1.,1.,1.,1.,1.,1.,1.,1.,1.,1.,1.,1.,1.,1.,1.,1.,1.,
1.,1.,1.,1.,1.,1.))
REPRESENTATION_ITEM('')
);
#459=(
BOUNDED_CURVE()
B_SPLINE_CURVE(5,(#66234,#66235,#66236,#66237,#66238,#66239,#66240,#66241,
#66242,#66243,#66244,#66245,#66246,#66247,#66248,#66249,#66250,#66251,#66252,
#66253,#66254,#66255,#66256,#66257,#66258,#66259,#66260,#66261,#66262,#66263,
#66264,#66265,#66266,#66267,#66268,#66269,#66270,#66271,#66272,#66273,#66274,
#66275,#66276,#66277,#66278,#66279,#66280,#66281,#66282,#66283,#66284,#66285,
#66286,#66287,#66288,#66289,#66290,#66291,#66292,#66293,#66294,#66295,#66296,
#66297,#66298,#66299,#66300,#66301,#66302,#66303),.UNSPECIFIED.,.F.,.F.)
B_SPLINE_CURVE_WITH_KNOTS((6,1,1,1,1,1,1,1,1,1,1,1,1,1,1,1,1,1,1,1,1,1,
1,1,1,1,1,1,1,1,1,1,1,1,1,1,1,1,1,1,1,1,1,1,1,1,1,1,1,1,1,1,1,1,1,1,1,1,
1,1,1,1,1,1,1,6),(-1.,-0.984615384615383,-0.969230769230768,-0.953846153846152,
-0.938461538461537,-0.923076923076922,-0.907692307692306,-0.892307692307691,
-0.876923076923076,-0.86153846153846,-0.846153846153845,-0.83076923076923,
-0.815384615384614,-0.799999999999999,-0.784615384615384,-0.769230769230768,
-0.753846153846153,-0.738461538461538,-0.723076923076922,-0.707692307692307,
-0.692307692307692,-0.676923076923076,-0.661538461538461,-0.646153846153846,
-0.63076923076923,-0.615384615384615,-0.6,-0.584615384615384,-0.569230769230769,
-0.553846153846154,-0.538461538461538,-0.523076923076923,-0.507692307692308,
-0.492307692307692,-0.476923076923077,-0.461538461538462,-0.446153846153846,
-0.430769230769231,-0.415384615384615,-0.4,-0.384615384615385,-0.369230769230769,
-0.353846153846154,-0.338461538461538,-0.323076923076923,-0.307692307692308,
-0.292307692307692,-0.276923076923077,-0.261538461538462,-0.246153846153846,
-0.230769230769231,-0.215384615384615,-0.2,-0.184615384615385,-0.169230769230769,
-0.153846153846154,-0.138461538461538,-0.123076923076923,-0.107692307692308,
-0.0923076923076923,-0.0769230769230769,-0.0615384615384615,-0.0461538461538462,
-0.0307692307692308,-0.0153846153846154,-0.0057718433745291),
 .UNSPECIFIED.)
CURVE()
GEOMETRIC_REPRESENTATION_ITEM()
RATIONAL_B_SPLINE_CURVE((1.,1.,1.,1.,1.,1.,1.,1.,1.,1.,1.,1.,1.,1.,1.,1.,
1.,1.,1.,1.,1.,1.,1.,1.,1.,1.,1.,1.,1.,1.,1.,1.,1.,1.,1.,1.,1.,1.,1.,1.,
1.,1.,1.,1.,1.,1.,1.,1.,1.,1.,1.,1.,1.,1.,1.,1.,1.,1.,1.,1.,1.,1.,1.,1.,
1.,1.,1.,1.,1.,1.))
REPRESENTATION_ITEM('')
);
#460=(
BOUNDED_CURVE()
B_SPLINE_CURVE(5,(#66454,#66455,#66456,#66457,#66458,#66459,#66460,#66461,
#66462,#66463,#66464,#66465,#66466,#66467,#66468,#66469,#66470,#66471,#66472,
#66473,#66474,#66475,#66476,#66477,#66478,#66479,#66480,#66481,#66482,#66483,
#66484,#66485,#66486,#66487,#66488,#66489,#66490,#66491,#66492,#66493,#66494,
#66495,#66496,#66497,#66498,#66499,#66500,#66501,#66502,#66503,#66504,#66505,
#66506,#66507,#66508,#66509,#66510,#66511,#66512,#66513,#66514,#66515,#66516,
#66517,#66518,#66519,#66520,#66521,#66522,#66523),.UNSPECIFIED.,.F.,.F.)
B_SPLINE_CURVE_WITH_KNOTS((6,1,1,1,1,1,1,1,1,1,1,1,1,1,1,1,1,1,1,1,1,1,
1,1,1,1,1,1,1,1,1,1,1,1,1,1,1,1,1,1,1,1,1,1,1,1,1,1,1,1,1,1,1,1,1,1,1,1,
1,1,1,1,1,1,1,6),(-0.994228156739695,-0.984615384615383,-0.969230769230768,
-0.953846153846152,-0.938461538461537,-0.923076923076922,-0.907692307692306,
-0.892307692307691,-0.876923076923076,-0.86153846153846,-0.846153846153845,
-0.83076923076923,-0.815384615384614,-0.799999999999999,-0.784615384615384,
-0.769230769230768,-0.753846153846153,-0.738461538461538,-0.723076923076922,
-0.707692307692307,-0.692307692307692,-0.676923076923076,-0.661538461538461,
-0.646153846153846,-0.63076923076923,-0.615384615384615,-0.6,-0.584615384615384,
-0.569230769230769,-0.553846153846154,-0.538461538461538,-0.523076923076923,
-0.507692307692308,-0.492307692307692,-0.476923076923077,-0.461538461538462,
-0.446153846153846,-0.430769230769231,-0.415384615384615,-0.4,-0.384615384615385,
-0.369230769230769,-0.353846153846154,-0.338461538461538,-0.323076923076923,
-0.307692307692308,-0.292307692307692,-0.276923076923077,-0.261538461538462,
-0.246153846153846,-0.230769230769231,-0.215384615384615,-0.2,-0.184615384615385,
-0.169230769230769,-0.153846153846154,-0.138461538461538,-0.123076923076923,
-0.107692307692308,-0.0923076923076923,-0.0769230769230769,-0.0615384615384615,
-0.0461538461538462,-0.0307692307692308,-0.0153846153846154,0.),
 .UNSPECIFIED.)
CURVE()
GEOMETRIC_REPRESENTATION_ITEM()
RATIONAL_B_SPLINE_CURVE((1.,1.,1.,1.,1.,1.,1.,1.,1.,1.,1.,1.,1.,1.,1.,1.,
1.,1.,1.,1.,1.,1.,1.,1.,1.,1.,1.,1.,1.,1.,1.,1.,1.,1.,1.,1.,1.,1.,1.,1.,
1.,1.,1.,1.,1.,1.,1.,1.,1.,1.,1.,1.,1.,1.,1.,1.,1.,1.,1.,1.,1.,1.,1.,1.,
1.,1.,1.,1.,1.,1.))
REPRESENTATION_ITEM('')
);
#461=(
BOUNDED_CURVE()
B_SPLINE_CURVE(5,(#66676,#66677,#66678,#66679,#66680,#66681,#66682,#66683,
#66684,#66685,#66686,#66687,#66688,#66689,#66690,#66691,#66692,#66693,#66694,
#66695,#66696,#66697,#66698,#66699,#66700,#66701,#66702,#66703,#66704,#66705,
#66706,#66707,#66708,#66709,#66710,#66711,#66712,#66713,#66714,#66715,#66716,
#66717,#66718,#66719,#66720,#66721,#66722,#66723,#66724,#66725,#66726,#66727,
#66728,#66729,#66730,#66731,#66732,#66733,#66734,#66735,#66736,#66737,#66738,
#66739,#66740,#66741,#66742,#66743,#66744,#66745),.UNSPECIFIED.,.F.,.F.)
B_SPLINE_CURVE_WITH_KNOTS((6,1,1,1,1,1,1,1,1,1,1,1,1,1,1,1,1,1,1,1,1,1,
1,1,1,1,1,1,1,1,1,1,1,1,1,1,1,1,1,1,1,1,1,1,1,1,1,1,1,1,1,1,1,1,1,1,1,1,
1,1,1,1,1,1,1,6),(-1.,-0.984615384615383,-0.969230769230768,-0.953846153846152,
-0.938461538461537,-0.923076923076922,-0.907692307692306,-0.892307692307691,
-0.876923076923076,-0.86153846153846,-0.846153846153845,-0.83076923076923,
-0.815384615384614,-0.799999999999999,-0.784615384615384,-0.769230769230768,
-0.753846153846153,-0.738461538461538,-0.723076923076922,-0.707692307692307,
-0.692307692307692,-0.676923076923076,-0.661538461538461,-0.646153846153846,
-0.63076923076923,-0.615384615384615,-0.6,-0.584615384615384,-0.569230769230769,
-0.553846153846154,-0.538461538461538,-0.523076923076923,-0.507692307692308,
-0.492307692307692,-0.476923076923077,-0.461538461538462,-0.446153846153846,
-0.430769230769231,-0.415384615384615,-0.4,-0.384615384615385,-0.369230769230769,
-0.353846153846154,-0.338461538461538,-0.323076923076923,-0.307692307692308,
-0.292307692307692,-0.276923076923077,-0.261538461538462,-0.246153846153846,
-0.230769230769231,-0.215384615384615,-0.2,-0.184615384615385,-0.169230769230769,
-0.153846153846154,-0.138461538461538,-0.123076923076923,-0.107692307692308,
-0.0923076923076923,-0.0769230769230769,-0.0615384615384615,-0.0461538461538462,
-0.0307692307692308,-0.0153846153846154,-0.00577184337450344),
 .UNSPECIFIED.)
CURVE()
GEOMETRIC_REPRESENTATION_ITEM()
RATIONAL_B_SPLINE_CURVE((1.,1.,1.,1.,1.,1.,1.,1.,1.,1.,1.,1.,1.,1.,1.,1.,
1.,1.,1.,1.,1.,1.,1.,1.,1.,1.,1.,1.,1.,1.,1.,1.,1.,1.,1.,1.,1.,1.,1.,1.,
1.,1.,1.,1.,1.,1.,1.,1.,1.,1.,1.,1.,1.,1.,1.,1.,1.,1.,1.,1.,1.,1.,1.,1.,
1.,1.,1.,1.,1.,1.))
REPRESENTATION_ITEM('')
);
#462=(
BOUNDED_CURVE()
B_SPLINE_CURVE(5,(#66896,#66897,#66898,#66899,#66900,#66901,#66902,#66903,
#66904,#66905,#66906,#66907,#66908,#66909,#66910,#66911,#66912,#66913,#66914,
#66915,#66916,#66917,#66918,#66919,#66920,#66921,#66922,#66923,#66924,#66925,
#66926,#66927,#66928,#66929,#66930,#66931,#66932,#66933,#66934,#66935,#66936,
#66937,#66938,#66939,#66940,#66941,#66942,#66943,#66944,#66945,#66946,#66947,
#66948,#66949,#66950,#66951,#66952,#66953,#66954,#66955,#66956,#66957,#66958,
#66959,#66960,#66961,#66962,#66963,#66964,#66965),.UNSPECIFIED.,.F.,.F.)
B_SPLINE_CURVE_WITH_KNOTS((6,1,1,1,1,1,1,1,1,1,1,1,1,1,1,1,1,1,1,1,1,1,
1,1,1,1,1,1,1,1,1,1,1,1,1,1,1,1,1,1,1,1,1,1,1,1,1,1,1,1,1,1,1,1,1,1,1,1,
1,1,1,1,1,1,1,6),(-0.994228156739669,-0.984615384615383,-0.969230769230768,
-0.953846153846152,-0.938461538461537,-0.923076923076922,-0.907692307692306,
-0.892307692307691,-0.876923076923076,-0.86153846153846,-0.846153846153845,
-0.83076923076923,-0.815384615384614,-0.799999999999999,-0.784615384615384,
-0.769230769230768,-0.753846153846153,-0.738461538461538,-0.723076923076922,
-0.707692307692307,-0.692307692307692,-0.676923076923076,-0.661538461538461,
-0.646153846153846,-0.63076923076923,-0.615384615384615,-0.6,-0.584615384615384,
-0.569230769230769,-0.553846153846154,-0.538461538461538,-0.523076923076923,
-0.507692307692308,-0.492307692307692,-0.476923076923077,-0.461538461538462,
-0.446153846153846,-0.430769230769231,-0.415384615384615,-0.4,-0.384615384615385,
-0.369230769230769,-0.353846153846154,-0.338461538461538,-0.323076923076923,
-0.307692307692308,-0.292307692307692,-0.276923076923077,-0.261538461538462,
-0.246153846153846,-0.230769230769231,-0.215384615384615,-0.2,-0.184615384615385,
-0.169230769230769,-0.153846153846154,-0.138461538461538,-0.123076923076923,
-0.107692307692308,-0.0923076923076923,-0.0769230769230769,-0.0615384615384615,
-0.0461538461538462,-0.0307692307692308,-0.0153846153846154,0.),
 .UNSPECIFIED.)
CURVE()
GEOMETRIC_REPRESENTATION_ITEM()
RATIONAL_B_SPLINE_CURVE((1.,1.,1.,1.,1.,1.,1.,1.,1.,1.,1.,1.,1.,1.,1.,1.,
1.,1.,1.,1.,1.,1.,1.,1.,1.,1.,1.,1.,1.,1.,1.,1.,1.,1.,1.,1.,1.,1.,1.,1.,
1.,1.,1.,1.,1.,1.,1.,1.,1.,1.,1.,1.,1.,1.,1.,1.,1.,1.,1.,1.,1.,1.,1.,1.,
1.,1.,1.,1.,1.,1.))
REPRESENTATION_ITEM('')
);
#463=(
BOUNDED_CURVE()
B_SPLINE_CURVE(5,(#67118,#67119,#67120,#67121,#67122,#67123,#67124,#67125,
#67126,#67127,#67128,#67129,#67130,#67131,#67132,#67133,#67134,#67135,#67136,
#67137,#67138,#67139,#67140,#67141,#67142,#67143,#67144,#67145,#67146,#67147,
#67148,#67149,#67150,#67151,#67152,#67153,#67154,#67155,#67156,#67157,#67158,
#67159,#67160,#67161,#67162,#67163,#67164,#67165,#67166,#67167,#67168,#67169,
#67170,#67171,#67172,#67173,#67174,#67175,#67176,#67177,#67178,#67179,#67180,
#67181,#67182,#67183,#67184,#67185,#67186,#67187),.UNSPECIFIED.,.F.,.F.)
B_SPLINE_CURVE_WITH_KNOTS((6,1,1,1,1,1,1,1,1,1,1,1,1,1,1,1,1,1,1,1,1,1,
1,1,1,1,1,1,1,1,1,1,1,1,1,1,1,1,1,1,1,1,1,1,1,1,1,1,1,1,1,1,1,1,1,1,1,1,
1,1,1,1,1,1,1,6),(-1.,-0.984615384615383,-0.969230769230768,-0.953846153846152,
-0.938461538461537,-0.923076923076922,-0.907692307692306,-0.892307692307691,
-0.876923076923076,-0.86153846153846,-0.846153846153845,-0.83076923076923,
-0.815384615384614,-0.799999999999999,-0.784615384615384,-0.769230769230768,
-0.753846153846153,-0.738461538461538,-0.723076923076922,-0.707692307692307,
-0.692307692307692,-0.676923076923076,-0.661538461538461,-0.646153846153846,
-0.63076923076923,-0.615384615384615,-0.6,-0.584615384615384,-0.569230769230769,
-0.553846153846154,-0.538461538461538,-0.523076923076923,-0.507692307692308,
-0.492307692307692,-0.476923076923077,-0.461538461538462,-0.446153846153846,
-0.430769230769231,-0.415384615384615,-0.4,-0.384615384615385,-0.369230769230769,
-0.353846153846154,-0.338461538461538,-0.323076923076923,-0.307692307692308,
-0.292307692307692,-0.276923076923077,-0.261538461538462,-0.246153846153846,
-0.230769230769231,-0.215384615384615,-0.2,-0.184615384615385,-0.169230769230769,
-0.153846153846154,-0.138461538461538,-0.123076923076923,-0.107692307692308,
-0.0923076923076923,-0.0769230769230769,-0.0615384615384615,-0.0461538461538462,
-0.0307692307692308,-0.0153846153846154,-0.00577184337450876),
 .UNSPECIFIED.)
CURVE()
GEOMETRIC_REPRESENTATION_ITEM()
RATIONAL_B_SPLINE_CURVE((1.,1.,1.,1.,1.,1.,1.,1.,1.,1.,1.,1.,1.,1.,1.,1.,
1.,1.,1.,1.,1.,1.,1.,1.,1.,1.,1.,1.,1.,1.,1.,1.,1.,1.,1.,1.,1.,1.,1.,1.,
1.,1.,1.,1.,1.,1.,1.,1.,1.,1.,1.,1.,1.,1.,1.,1.,1.,1.,1.,1.,1.,1.,1.,1.,
1.,1.,1.,1.,1.,1.))
REPRESENTATION_ITEM('')
);
#464=(
BOUNDED_CURVE()
B_SPLINE_CURVE(5,(#67338,#67339,#67340,#67341,#67342,#67343,#67344,#67345,
#67346,#67347,#67348,#67349,#67350,#67351,#67352,#67353,#67354,#67355,#67356,
#67357,#67358,#67359,#67360,#67361,#67362,#67363,#67364,#67365,#67366,#67367,
#67368,#67369,#67370,#67371,#67372,#67373,#67374,#67375,#67376,#67377,#67378,
#67379,#67380,#67381,#67382,#67383,#67384,#67385,#67386,#67387,#67388,#67389,
#67390,#67391,#67392,#67393,#67394,#67395,#67396,#67397,#67398,#67399,#67400,
#67401,#67402,#67403,#67404,#67405,#67406,#67407),.UNSPECIFIED.,.F.,.F.)
B_SPLINE_CURVE_WITH_KNOTS((6,1,1,1,1,1,1,1,1,1,1,1,1,1,1,1,1,1,1,1,1,1,
1,1,1,1,1,1,1,1,1,1,1,1,1,1,1,1,1,1,1,1,1,1,1,1,1,1,1,1,1,1,1,1,1,1,1,1,
1,1,1,1,1,1,1,6),(-0.99422815673966,-0.984615384615383,-0.969230769230768,
-0.953846153846152,-0.938461538461537,-0.923076923076922,-0.907692307692306,
-0.892307692307691,-0.876923076923076,-0.86153846153846,-0.846153846153845,
-0.83076923076923,-0.815384615384614,-0.799999999999999,-0.784615384615384,
-0.769230769230768,-0.753846153846153,-0.738461538461538,-0.723076923076922,
-0.707692307692307,-0.692307692307692,-0.676923076923076,-0.661538461538461,
-0.646153846153846,-0.63076923076923,-0.615384615384615,-0.6,-0.584615384615384,
-0.569230769230769,-0.553846153846154,-0.538461538461538,-0.523076923076923,
-0.507692307692308,-0.492307692307692,-0.476923076923077,-0.461538461538462,
-0.446153846153846,-0.430769230769231,-0.415384615384615,-0.4,-0.384615384615385,
-0.369230769230769,-0.353846153846154,-0.338461538461538,-0.323076923076923,
-0.307692307692308,-0.292307692307692,-0.276923076923077,-0.261538461538462,
-0.246153846153846,-0.230769230769231,-0.215384615384615,-0.2,-0.184615384615385,
-0.169230769230769,-0.153846153846154,-0.138461538461538,-0.123076923076923,
-0.107692307692308,-0.0923076923076923,-0.0769230769230769,-0.0615384615384615,
-0.0461538461538462,-0.0307692307692308,-0.0153846153846154,0.),
 .UNSPECIFIED.)
CURVE()
GEOMETRIC_REPRESENTATION_ITEM()
RATIONAL_B_SPLINE_CURVE((1.,1.,1.,1.,1.,1.,1.,1.,1.,1.,1.,1.,1.,1.,1.,1.,
1.,1.,1.,1.,1.,1.,1.,1.,1.,1.,1.,1.,1.,1.,1.,1.,1.,1.,1.,1.,1.,1.,1.,1.,
1.,1.,1.,1.,1.,1.,1.,1.,1.,1.,1.,1.,1.,1.,1.,1.,1.,1.,1.,1.,1.,1.,1.,1.,
1.,1.,1.,1.,1.,1.))
REPRESENTATION_ITEM('')
);
#465=(
BOUNDED_CURVE()
B_SPLINE_CURVE(5,(#67560,#67561,#67562,#67563,#67564,#67565,#67566,#67567,
#67568,#67569,#67570,#67571,#67572,#67573,#67574,#67575,#67576,#67577,#67578,
#67579,#67580,#67581,#67582,#67583,#67584,#67585,#67586,#67587,#67588,#67589,
#67590,#67591,#67592,#67593,#67594,#67595,#67596,#67597,#67598,#67599,#67600,
#67601,#67602,#67603,#67604,#67605,#67606,#67607,#67608,#67609,#67610,#67611,
#67612,#67613,#67614,#67615,#67616,#67617,#67618,#67619,#67620,#67621,#67622,
#67623,#67624,#67625,#67626,#67627,#67628,#67629),.UNSPECIFIED.,.F.,.F.)
B_SPLINE_CURVE_WITH_KNOTS((6,1,1,1,1,1,1,1,1,1,1,1,1,1,1,1,1,1,1,1,1,1,
1,1,1,1,1,1,1,1,1,1,1,1,1,1,1,1,1,1,1,1,1,1,1,1,1,1,1,1,1,1,1,1,1,1,1,1,
1,1,1,1,1,1,1,6),(-1.,-0.984615384615383,-0.969230769230768,-0.953846153846152,
-0.938461538461537,-0.923076923076922,-0.907692307692306,-0.892307692307691,
-0.876923076923076,-0.86153846153846,-0.846153846153845,-0.83076923076923,
-0.815384615384614,-0.799999999999999,-0.784615384615384,-0.769230769230768,
-0.753846153846153,-0.738461538461538,-0.723076923076922,-0.707692307692307,
-0.692307692307692,-0.676923076923076,-0.661538461538461,-0.646153846153846,
-0.63076923076923,-0.615384615384615,-0.6,-0.584615384615384,-0.569230769230769,
-0.553846153846154,-0.538461538461538,-0.523076923076923,-0.507692307692308,
-0.492307692307692,-0.476923076923077,-0.461538461538462,-0.446153846153846,
-0.430769230769231,-0.415384615384615,-0.4,-0.384615384615385,-0.369230769230769,
-0.353846153846154,-0.338461538461538,-0.323076923076923,-0.307692307692308,
-0.292307692307692,-0.276923076923077,-0.261538461538462,-0.246153846153846,
-0.230769230769231,-0.215384615384615,-0.2,-0.184615384615385,-0.169230769230769,
-0.153846153846154,-0.138461538461538,-0.123076923076923,-0.107692307692308,
-0.0923076923076923,-0.0769230769230769,-0.0615384615384615,-0.0461538461538462,
-0.0307692307692308,-0.0153846153846154,-0.00577184337451051),
 .UNSPECIFIED.)
CURVE()
GEOMETRIC_REPRESENTATION_ITEM()
RATIONAL_B_SPLINE_CURVE((1.,1.,1.,1.,1.,1.,1.,1.,1.,1.,1.,1.,1.,1.,1.,1.,
1.,1.,1.,1.,1.,1.,1.,1.,1.,1.,1.,1.,1.,1.,1.,1.,1.,1.,1.,1.,1.,1.,1.,1.,
1.,1.,1.,1.,1.,1.,1.,1.,1.,1.,1.,1.,1.,1.,1.,1.,1.,1.,1.,1.,1.,1.,1.,1.,
1.,1.,1.,1.,1.,1.))
REPRESENTATION_ITEM('')
);
#466=(
BOUNDED_CURVE()
B_SPLINE_CURVE(5,(#67780,#67781,#67782,#67783,#67784,#67785,#67786,#67787,
#67788,#67789,#67790,#67791,#67792,#67793,#67794,#67795,#67796,#67797,#67798,
#67799,#67800,#67801,#67802,#67803,#67804,#67805,#67806,#67807,#67808,#67809,
#67810,#67811,#67812,#67813,#67814,#67815,#67816,#67817,#67818,#67819,#67820,
#67821,#67822,#67823,#67824,#67825,#67826,#67827,#67828,#67829,#67830,#67831,
#67832,#67833,#67834,#67835,#67836,#67837,#67838,#67839,#67840,#67841,#67842,
#67843,#67844,#67845,#67846,#67847,#67848,#67849),.UNSPECIFIED.,.F.,.F.)
B_SPLINE_CURVE_WITH_KNOTS((6,1,1,1,1,1,1,1,1,1,1,1,1,1,1,1,1,1,1,1,1,1,
1,1,1,1,1,1,1,1,1,1,1,1,1,1,1,1,1,1,1,1,1,1,1,1,1,1,1,1,1,1,1,1,1,1,1,1,
1,1,1,1,1,1,1,6),(-0.994228156739678,-0.984615384615383,-0.969230769230768,
-0.953846153846152,-0.938461538461537,-0.923076923076922,-0.907692307692306,
-0.892307692307691,-0.876923076923076,-0.86153846153846,-0.846153846153845,
-0.83076923076923,-0.815384615384614,-0.799999999999999,-0.784615384615384,
-0.769230769230768,-0.753846153846153,-0.738461538461538,-0.723076923076922,
-0.707692307692307,-0.692307692307692,-0.676923076923076,-0.661538461538461,
-0.646153846153846,-0.63076923076923,-0.615384615384615,-0.6,-0.584615384615384,
-0.569230769230769,-0.553846153846154,-0.538461538461538,-0.523076923076923,
-0.507692307692308,-0.492307692307692,-0.476923076923077,-0.461538461538462,
-0.446153846153846,-0.430769230769231,-0.415384615384615,-0.4,-0.384615384615385,
-0.369230769230769,-0.353846153846154,-0.338461538461538,-0.323076923076923,
-0.307692307692308,-0.292307692307692,-0.276923076923077,-0.261538461538462,
-0.246153846153846,-0.230769230769231,-0.215384615384615,-0.2,-0.184615384615385,
-0.169230769230769,-0.153846153846154,-0.138461538461538,-0.123076923076923,
-0.107692307692308,-0.0923076923076923,-0.0769230769230769,-0.0615384615384615,
-0.0461538461538462,-0.0307692307692308,-0.0153846153846154,0.),
 .UNSPECIFIED.)
CURVE()
GEOMETRIC_REPRESENTATION_ITEM()
RATIONAL_B_SPLINE_CURVE((1.,1.,1.,1.,1.,1.,1.,1.,1.,1.,1.,1.,1.,1.,1.,1.,
1.,1.,1.,1.,1.,1.,1.,1.,1.,1.,1.,1.,1.,1.,1.,1.,1.,1.,1.,1.,1.,1.,1.,1.,
1.,1.,1.,1.,1.,1.,1.,1.,1.,1.,1.,1.,1.,1.,1.,1.,1.,1.,1.,1.,1.,1.,1.,1.,
1.,1.,1.,1.,1.,1.))
REPRESENTATION_ITEM('')
);
#467=(
BOUNDED_CURVE()
B_SPLINE_CURVE(5,(#68002,#68003,#68004,#68005,#68006,#68007,#68008,#68009,
#68010,#68011,#68012,#68013,#68014,#68015,#68016,#68017,#68018,#68019,#68020,
#68021,#68022,#68023,#68024,#68025,#68026,#68027,#68028,#68029,#68030,#68031,
#68032,#68033,#68034,#68035,#68036,#68037,#68038,#68039,#68040,#68041,#68042,
#68043,#68044,#68045,#68046,#68047,#68048,#68049,#68050,#68051,#68052,#68053,
#68054,#68055,#68056,#68057,#68058,#68059,#68060,#68061,#68062,#68063,#68064,
#68065,#68066,#68067,#68068,#68069,#68070,#68071),.UNSPECIFIED.,.F.,.F.)
B_SPLINE_CURVE_WITH_KNOTS((6,1,1,1,1,1,1,1,1,1,1,1,1,1,1,1,1,1,1,1,1,1,
1,1,1,1,1,1,1,1,1,1,1,1,1,1,1,1,1,1,1,1,1,1,1,1,1,1,1,1,1,1,1,1,1,1,1,1,
1,1,1,1,1,1,1,6),(-1.,-0.984615384615383,-0.969230769230768,-0.953846153846152,
-0.938461538461537,-0.923076923076922,-0.907692307692306,-0.892307692307691,
-0.876923076923076,-0.86153846153846,-0.846153846153845,-0.83076923076923,
-0.815384615384614,-0.799999999999999,-0.784615384615384,-0.769230769230768,
-0.753846153846153,-0.738461538461538,-0.723076923076922,-0.707692307692307,
-0.692307692307692,-0.676923076923076,-0.661538461538461,-0.646153846153846,
-0.63076923076923,-0.615384615384615,-0.6,-0.584615384615384,-0.569230769230769,
-0.553846153846154,-0.538461538461538,-0.523076923076923,-0.507692307692308,
-0.492307692307692,-0.476923076923077,-0.461538461538462,-0.446153846153846,
-0.430769230769231,-0.415384615384615,-0.4,-0.384615384615385,-0.369230769230769,
-0.353846153846154,-0.338461538461538,-0.323076923076923,-0.307692307692308,
-0.292307692307692,-0.276923076923077,-0.261538461538462,-0.246153846153846,
-0.230769230769231,-0.215384615384615,-0.2,-0.184615384615385,-0.169230769230769,
-0.153846153846154,-0.138461538461538,-0.123076923076923,-0.107692307692308,
-0.0923076923076923,-0.0769230769230769,-0.0615384615384615,-0.0461538461538462,
-0.0307692307692308,-0.0153846153846154,-0.0057718433745179),
 .UNSPECIFIED.)
CURVE()
GEOMETRIC_REPRESENTATION_ITEM()
RATIONAL_B_SPLINE_CURVE((1.,1.,1.,1.,1.,1.,1.,1.,1.,1.,1.,1.,1.,1.,1.,1.,
1.,1.,1.,1.,1.,1.,1.,1.,1.,1.,1.,1.,1.,1.,1.,1.,1.,1.,1.,1.,1.,1.,1.,1.,
1.,1.,1.,1.,1.,1.,1.,1.,1.,1.,1.,1.,1.,1.,1.,1.,1.,1.,1.,1.,1.,1.,1.,1.,
1.,1.,1.,1.,1.,1.))
REPRESENTATION_ITEM('')
);
#468=(
BOUNDED_CURVE()
B_SPLINE_CURVE(5,(#68222,#68223,#68224,#68225,#68226,#68227,#68228,#68229,
#68230,#68231,#68232,#68233,#68234,#68235,#68236,#68237,#68238,#68239,#68240,
#68241,#68242,#68243,#68244,#68245,#68246,#68247,#68248,#68249,#68250,#68251,
#68252,#68253,#68254,#68255,#68256,#68257,#68258,#68259,#68260,#68261,#68262,
#68263,#68264,#68265,#68266,#68267,#68268,#68269,#68270,#68271,#68272,#68273,
#68274,#68275,#68276,#68277,#68278,#68279,#68280,#68281,#68282,#68283,#68284,
#68285,#68286,#68287,#68288,#68289,#68290,#68291),.UNSPECIFIED.,.F.,.F.)
B_SPLINE_CURVE_WITH_KNOTS((6,1,1,1,1,1,1,1,1,1,1,1,1,1,1,1,1,1,1,1,1,1,
1,1,1,1,1,1,1,1,1,1,1,1,1,1,1,1,1,1,1,1,1,1,1,1,1,1,1,1,1,1,1,1,1,1,1,1,
1,1,1,1,1,1,1,6),(-0.99422815673967,-0.984615384615383,-0.969230769230768,
-0.953846153846152,-0.938461538461537,-0.923076923076922,-0.907692307692306,
-0.892307692307691,-0.876923076923076,-0.86153846153846,-0.846153846153845,
-0.83076923076923,-0.815384615384614,-0.799999999999999,-0.784615384615384,
-0.769230769230768,-0.753846153846153,-0.738461538461538,-0.723076923076922,
-0.707692307692307,-0.692307692307692,-0.676923076923076,-0.661538461538461,
-0.646153846153846,-0.63076923076923,-0.615384615384615,-0.6,-0.584615384615384,
-0.569230769230769,-0.553846153846154,-0.538461538461538,-0.523076923076923,
-0.507692307692308,-0.492307692307692,-0.476923076923077,-0.461538461538462,
-0.446153846153846,-0.430769230769231,-0.415384615384615,-0.4,-0.384615384615385,
-0.369230769230769,-0.353846153846154,-0.338461538461538,-0.323076923076923,
-0.307692307692308,-0.292307692307692,-0.276923076923077,-0.261538461538462,
-0.246153846153846,-0.230769230769231,-0.215384615384615,-0.2,-0.184615384615385,
-0.169230769230769,-0.153846153846154,-0.138461538461538,-0.123076923076923,
-0.107692307692308,-0.0923076923076923,-0.0769230769230769,-0.0615384615384615,
-0.0461538461538462,-0.0307692307692308,-0.0153846153846154,0.),
 .UNSPECIFIED.)
CURVE()
GEOMETRIC_REPRESENTATION_ITEM()
RATIONAL_B_SPLINE_CURVE((1.,1.,1.,1.,1.,1.,1.,1.,1.,1.,1.,1.,1.,1.,1.,1.,
1.,1.,1.,1.,1.,1.,1.,1.,1.,1.,1.,1.,1.,1.,1.,1.,1.,1.,1.,1.,1.,1.,1.,1.,
1.,1.,1.,1.,1.,1.,1.,1.,1.,1.,1.,1.,1.,1.,1.,1.,1.,1.,1.,1.,1.,1.,1.,1.,
1.,1.,1.,1.,1.,1.))
REPRESENTATION_ITEM('')
);
#469=(
BOUNDED_CURVE()
B_SPLINE_CURVE(5,(#68444,#68445,#68446,#68447,#68448,#68449,#68450,#68451,
#68452,#68453,#68454,#68455,#68456,#68457,#68458,#68459,#68460,#68461,#68462,
#68463,#68464,#68465,#68466,#68467,#68468,#68469,#68470,#68471,#68472,#68473,
#68474,#68475,#68476,#68477,#68478,#68479,#68480,#68481,#68482,#68483,#68484,
#68485,#68486,#68487,#68488,#68489,#68490,#68491,#68492,#68493,#68494,#68495,
#68496,#68497,#68498,#68499,#68500,#68501,#68502,#68503,#68504,#68505,#68506,
#68507,#68508,#68509,#68510,#68511,#68512,#68513),.UNSPECIFIED.,.F.,.F.)
B_SPLINE_CURVE_WITH_KNOTS((6,1,1,1,1,1,1,1,1,1,1,1,1,1,1,1,1,1,1,1,1,1,
1,1,1,1,1,1,1,1,1,1,1,1,1,1,1,1,1,1,1,1,1,1,1,1,1,1,1,1,1,1,1,1,1,1,1,1,
1,1,1,1,1,1,1,6),(-1.,-0.984615384615383,-0.969230769230768,-0.953846153846152,
-0.938461538461537,-0.923076923076922,-0.907692307692306,-0.892307692307691,
-0.876923076923076,-0.86153846153846,-0.846153846153845,-0.83076923076923,
-0.815384615384614,-0.799999999999999,-0.784615384615384,-0.769230769230768,
-0.753846153846153,-0.738461538461538,-0.723076923076922,-0.707692307692307,
-0.692307692307692,-0.676923076923076,-0.661538461538461,-0.646153846153846,
-0.63076923076923,-0.615384615384615,-0.6,-0.584615384615384,-0.569230769230769,
-0.553846153846154,-0.538461538461538,-0.523076923076923,-0.507692307692308,
-0.492307692307692,-0.476923076923077,-0.461538461538462,-0.446153846153846,
-0.430769230769231,-0.415384615384615,-0.4,-0.384615384615385,-0.369230769230769,
-0.353846153846154,-0.338461538461538,-0.323076923076923,-0.307692307692308,
-0.292307692307692,-0.276923076923077,-0.261538461538462,-0.246153846153846,
-0.230769230769231,-0.215384615384615,-0.2,-0.184615384615385,-0.169230769230769,
-0.153846153846154,-0.138461538461538,-0.123076923076923,-0.107692307692308,
-0.0923076923076923,-0.0769230769230769,-0.0615384615384615,-0.0461538461538462,
-0.0307692307692308,-0.0153846153846154,-0.00577184337452479),
 .UNSPECIFIED.)
CURVE()
GEOMETRIC_REPRESENTATION_ITEM()
RATIONAL_B_SPLINE_CURVE((1.,1.,1.,1.,1.,1.,1.,1.,1.,1.,1.,1.,1.,1.,1.,1.,
1.,1.,1.,1.,1.,1.,1.,1.,1.,1.,1.,1.,1.,1.,1.,1.,1.,1.,1.,1.,1.,1.,1.,1.,
1.,1.,1.,1.,1.,1.,1.,1.,1.,1.,1.,1.,1.,1.,1.,1.,1.,1.,1.,1.,1.,1.,1.,1.,
1.,1.,1.,1.,1.,1.))
REPRESENTATION_ITEM('')
);
#470=(
BOUNDED_CURVE()
B_SPLINE_CURVE(5,(#68664,#68665,#68666,#68667,#68668,#68669,#68670,#68671,
#68672,#68673,#68674,#68675,#68676,#68677,#68678,#68679,#68680,#68681,#68682,
#68683,#68684,#68685,#68686,#68687,#68688,#68689,#68690,#68691,#68692,#68693,
#68694,#68695,#68696,#68697,#68698,#68699,#68700,#68701,#68702,#68703,#68704,
#68705,#68706,#68707,#68708,#68709,#68710,#68711,#68712,#68713,#68714,#68715,
#68716,#68717,#68718,#68719,#68720,#68721,#68722,#68723,#68724,#68725,#68726,
#68727,#68728,#68729,#68730,#68731,#68732,#68733),.UNSPECIFIED.,.F.,.F.)
B_SPLINE_CURVE_WITH_KNOTS((6,1,1,1,1,1,1,1,1,1,1,1,1,1,1,1,1,1,1,1,1,1,
1,1,1,1,1,1,1,1,1,1,1,1,1,1,1,1,1,1,1,1,1,1,1,1,1,1,1,1,1,1,1,1,1,1,1,1,
1,1,1,1,1,1,1,6),(-0.99422815673967,-0.984615384615383,-0.969230769230768,
-0.953846153846152,-0.938461538461537,-0.923076923076922,-0.907692307692306,
-0.892307692307691,-0.876923076923076,-0.86153846153846,-0.846153846153845,
-0.83076923076923,-0.815384615384614,-0.799999999999999,-0.784615384615384,
-0.769230769230768,-0.753846153846153,-0.738461538461538,-0.723076923076922,
-0.707692307692307,-0.692307692307692,-0.676923076923076,-0.661538461538461,
-0.646153846153846,-0.63076923076923,-0.615384615384615,-0.6,-0.584615384615384,
-0.569230769230769,-0.553846153846154,-0.538461538461538,-0.523076923076923,
-0.507692307692308,-0.492307692307692,-0.476923076923077,-0.461538461538462,
-0.446153846153846,-0.430769230769231,-0.415384615384615,-0.4,-0.384615384615385,
-0.369230769230769,-0.353846153846154,-0.338461538461538,-0.323076923076923,
-0.307692307692308,-0.292307692307692,-0.276923076923077,-0.261538461538462,
-0.246153846153846,-0.230769230769231,-0.215384615384615,-0.2,-0.184615384615385,
-0.169230769230769,-0.153846153846154,-0.138461538461538,-0.123076923076923,
-0.107692307692308,-0.0923076923076923,-0.0769230769230769,-0.0615384615384615,
-0.0461538461538462,-0.0307692307692308,-0.0153846153846154,0.),
 .UNSPECIFIED.)
CURVE()
GEOMETRIC_REPRESENTATION_ITEM()
RATIONAL_B_SPLINE_CURVE((1.,1.,1.,1.,1.,1.,1.,1.,1.,1.,1.,1.,1.,1.,1.,1.,
1.,1.,1.,1.,1.,1.,1.,1.,1.,1.,1.,1.,1.,1.,1.,1.,1.,1.,1.,1.,1.,1.,1.,1.,
1.,1.,1.,1.,1.,1.,1.,1.,1.,1.,1.,1.,1.,1.,1.,1.,1.,1.,1.,1.,1.,1.,1.,1.,
1.,1.,1.,1.,1.,1.))
REPRESENTATION_ITEM('')
);
#471=(
BOUNDED_CURVE()
B_SPLINE_CURVE(5,(#68886,#68887,#68888,#68889,#68890,#68891,#68892,#68893,
#68894,#68895,#68896,#68897,#68898,#68899,#68900,#68901,#68902,#68903,#68904,
#68905,#68906,#68907,#68908,#68909,#68910,#68911,#68912,#68913,#68914,#68915,
#68916,#68917,#68918,#68919,#68920,#68921,#68922,#68923,#68924,#68925,#68926,
#68927,#68928,#68929,#68930,#68931,#68932,#68933,#68934,#68935,#68936,#68937,
#68938,#68939,#68940,#68941,#68942,#68943,#68944,#68945,#68946,#68947,#68948,
#68949,#68950,#68951,#68952,#68953,#68954,#68955),.UNSPECIFIED.,.F.,.F.)
B_SPLINE_CURVE_WITH_KNOTS((6,1,1,1,1,1,1,1,1,1,1,1,1,1,1,1,1,1,1,1,1,1,
1,1,1,1,1,1,1,1,1,1,1,1,1,1,1,1,1,1,1,1,1,1,1,1,1,1,1,1,1,1,1,1,1,1,1,1,
1,1,1,1,1,1,1,6),(-1.,-0.984615384615383,-0.969230769230768,-0.953846153846152,
-0.938461538461537,-0.923076923076922,-0.907692307692306,-0.892307692307691,
-0.876923076923076,-0.86153846153846,-0.846153846153845,-0.83076923076923,
-0.815384615384614,-0.799999999999999,-0.784615384615384,-0.769230769230768,
-0.753846153846153,-0.738461538461538,-0.723076923076922,-0.707692307692307,
-0.692307692307692,-0.676923076923076,-0.661538461538461,-0.646153846153846,
-0.63076923076923,-0.615384615384615,-0.6,-0.584615384615384,-0.569230769230769,
-0.553846153846154,-0.538461538461538,-0.523076923076923,-0.507692307692308,
-0.492307692307692,-0.476923076923077,-0.461538461538462,-0.446153846153846,
-0.430769230769231,-0.415384615384615,-0.4,-0.384615384615385,-0.369230769230769,
-0.353846153846154,-0.338461538461538,-0.323076923076923,-0.307692307692308,
-0.292307692307692,-0.276923076923077,-0.261538461538462,-0.246153846153846,
-0.230769230769231,-0.215384615384615,-0.2,-0.184615384615385,-0.169230769230769,
-0.153846153846154,-0.138461538461538,-0.123076923076923,-0.107692307692308,
-0.0923076923076923,-0.0769230769230769,-0.0615384615384615,-0.0461538461538462,
-0.0307692307692308,-0.0153846153846154,-0.0057718433745009),
 .UNSPECIFIED.)
CURVE()
GEOMETRIC_REPRESENTATION_ITEM()
RATIONAL_B_SPLINE_CURVE((1.,1.,1.,1.,1.,1.,1.,1.,1.,1.,1.,1.,1.,1.,1.,1.,
1.,1.,1.,1.,1.,1.,1.,1.,1.,1.,1.,1.,1.,1.,1.,1.,1.,1.,1.,1.,1.,1.,1.,1.,
1.,1.,1.,1.,1.,1.,1.,1.,1.,1.,1.,1.,1.,1.,1.,1.,1.,1.,1.,1.,1.,1.,1.,1.,
1.,1.,1.,1.,1.,1.))
REPRESENTATION_ITEM('')
);
#472=(
BOUNDED_CURVE()
B_SPLINE_CURVE(5,(#69106,#69107,#69108,#69109,#69110,#69111,#69112,#69113,
#69114,#69115,#69116,#69117,#69118,#69119,#69120,#69121,#69122,#69123,#69124,
#69125,#69126,#69127,#69128,#69129,#69130,#69131,#69132,#69133,#69134,#69135,
#69136,#69137,#69138,#69139,#69140,#69141,#69142,#69143,#69144,#69145,#69146,
#69147,#69148,#69149,#69150,#69151,#69152,#69153,#69154,#69155,#69156,#69157,
#69158,#69159,#69160,#69161,#69162,#69163,#69164,#69165,#69166,#69167,#69168,
#69169,#69170,#69171,#69172,#69173,#69174,#69175),.UNSPECIFIED.,.F.,.F.)
B_SPLINE_CURVE_WITH_KNOTS((6,1,1,1,1,1,1,1,1,1,1,1,1,1,1,1,1,1,1,1,1,1,
1,1,1,1,1,1,1,1,1,1,1,1,1,1,1,1,1,1,1,1,1,1,1,1,1,1,1,1,1,1,1,1,1,1,1,1,
1,1,1,1,1,1,1,6),(-0.99422815673967,-0.984615384615383,-0.969230769230768,
-0.953846153846152,-0.938461538461537,-0.923076923076922,-0.907692307692306,
-0.892307692307691,-0.876923076923076,-0.86153846153846,-0.846153846153845,
-0.83076923076923,-0.815384615384614,-0.799999999999999,-0.784615384615384,
-0.769230769230768,-0.753846153846153,-0.738461538461538,-0.723076923076922,
-0.707692307692307,-0.692307692307692,-0.676923076923076,-0.661538461538461,
-0.646153846153846,-0.63076923076923,-0.615384615384615,-0.6,-0.584615384615384,
-0.569230769230769,-0.553846153846154,-0.538461538461538,-0.523076923076923,
-0.507692307692308,-0.492307692307692,-0.476923076923077,-0.461538461538462,
-0.446153846153846,-0.430769230769231,-0.415384615384615,-0.4,-0.384615384615385,
-0.369230769230769,-0.353846153846154,-0.338461538461538,-0.323076923076923,
-0.307692307692308,-0.292307692307692,-0.276923076923077,-0.261538461538462,
-0.246153846153846,-0.230769230769231,-0.215384615384615,-0.2,-0.184615384615385,
-0.169230769230769,-0.153846153846154,-0.138461538461538,-0.123076923076923,
-0.107692307692308,-0.0923076923076923,-0.0769230769230769,-0.0615384615384615,
-0.0461538461538462,-0.0307692307692308,-0.0153846153846154,0.),
 .UNSPECIFIED.)
CURVE()
GEOMETRIC_REPRESENTATION_ITEM()
RATIONAL_B_SPLINE_CURVE((1.,1.,1.,1.,1.,1.,1.,1.,1.,1.,1.,1.,1.,1.,1.,1.,
1.,1.,1.,1.,1.,1.,1.,1.,1.,1.,1.,1.,1.,1.,1.,1.,1.,1.,1.,1.,1.,1.,1.,1.,
1.,1.,1.,1.,1.,1.,1.,1.,1.,1.,1.,1.,1.,1.,1.,1.,1.,1.,1.,1.,1.,1.,1.,1.,
1.,1.,1.,1.,1.,1.))
REPRESENTATION_ITEM('')
);
#473=(
BOUNDED_CURVE()
B_SPLINE_CURVE(5,(#69328,#69329,#69330,#69331,#69332,#69333,#69334,#69335,
#69336,#69337,#69338,#69339,#69340,#69341,#69342,#69343,#69344,#69345,#69346,
#69347,#69348,#69349,#69350,#69351,#69352,#69353,#69354,#69355,#69356,#69357,
#69358,#69359,#69360,#69361,#69362,#69363,#69364,#69365,#69366,#69367,#69368,
#69369,#69370,#69371,#69372,#69373,#69374,#69375,#69376,#69377,#69378,#69379,
#69380,#69381,#69382,#69383,#69384,#69385,#69386,#69387,#69388,#69389,#69390,
#69391,#69392,#69393,#69394,#69395,#69396,#69397),.UNSPECIFIED.,.F.,.F.)
B_SPLINE_CURVE_WITH_KNOTS((6,1,1,1,1,1,1,1,1,1,1,1,1,1,1,1,1,1,1,1,1,1,
1,1,1,1,1,1,1,1,1,1,1,1,1,1,1,1,1,1,1,1,1,1,1,1,1,1,1,1,1,1,1,1,1,1,1,1,
1,1,1,1,1,1,1,6),(-1.,-0.984615384615383,-0.969230769230768,-0.953846153846152,
-0.938461538461537,-0.923076923076922,-0.907692307692306,-0.892307692307691,
-0.876923076923076,-0.86153846153846,-0.846153846153845,-0.83076923076923,
-0.815384615384614,-0.799999999999999,-0.784615384615384,-0.769230769230768,
-0.753846153846153,-0.738461538461538,-0.723076923076922,-0.707692307692307,
-0.692307692307692,-0.676923076923076,-0.661538461538461,-0.646153846153846,
-0.63076923076923,-0.615384615384615,-0.6,-0.584615384615384,-0.569230769230769,
-0.553846153846154,-0.538461538461538,-0.523076923076923,-0.507692307692308,
-0.492307692307692,-0.476923076923077,-0.461538461538462,-0.446153846153846,
-0.430769230769231,-0.415384615384615,-0.4,-0.384615384615385,-0.369230769230769,
-0.353846153846154,-0.338461538461538,-0.323076923076923,-0.307692307692308,
-0.292307692307692,-0.276923076923077,-0.261538461538462,-0.246153846153846,
-0.230769230769231,-0.215384615384615,-0.2,-0.184615384615385,-0.169230769230769,
-0.153846153846154,-0.138461538461538,-0.123076923076923,-0.107692307692308,
-0.0923076923076923,-0.0769230769230769,-0.0615384615384615,-0.0461538461538462,
-0.0307692307692308,-0.0153846153846154,-0.00577184337450701),
 .UNSPECIFIED.)
CURVE()
GEOMETRIC_REPRESENTATION_ITEM()
RATIONAL_B_SPLINE_CURVE((1.,1.,1.,1.,1.,1.,1.,1.,1.,1.,1.,1.,1.,1.,1.,1.,
1.,1.,1.,1.,1.,1.,1.,1.,1.,1.,1.,1.,1.,1.,1.,1.,1.,1.,1.,1.,1.,1.,1.,1.,
1.,1.,1.,1.,1.,1.,1.,1.,1.,1.,1.,1.,1.,1.,1.,1.,1.,1.,1.,1.,1.,1.,1.,1.,
1.,1.,1.,1.,1.,1.))
REPRESENTATION_ITEM('')
);
#474=(
BOUNDED_CURVE()
B_SPLINE_CURVE(5,(#69548,#69549,#69550,#69551,#69552,#69553,#69554,#69555,
#69556,#69557,#69558,#69559,#69560,#69561,#69562,#69563,#69564,#69565,#69566,
#69567,#69568,#69569,#69570,#69571,#69572,#69573,#69574,#69575,#69576,#69577,
#69578,#69579,#69580,#69581,#69582,#69583,#69584,#69585,#69586,#69587,#69588,
#69589,#69590,#69591,#69592,#69593,#69594,#69595,#69596,#69597,#69598,#69599,
#69600,#69601,#69602,#69603,#69604,#69605,#69606,#69607,#69608,#69609,#69610,
#69611,#69612,#69613,#69614,#69615,#69616,#69617),.UNSPECIFIED.,.F.,.F.)
B_SPLINE_CURVE_WITH_KNOTS((6,1,1,1,1,1,1,1,1,1,1,1,1,1,1,1,1,1,1,1,1,1,
1,1,1,1,1,1,1,1,1,1,1,1,1,1,1,1,1,1,1,1,1,1,1,1,1,1,1,1,1,1,1,1,1,1,1,1,
1,1,1,1,1,1,1,6),(-0.994228156739689,-0.984615384615383,-0.969230769230768,
-0.953846153846152,-0.938461538461537,-0.923076923076922,-0.907692307692306,
-0.892307692307691,-0.876923076923076,-0.86153846153846,-0.846153846153845,
-0.83076923076923,-0.815384615384614,-0.799999999999999,-0.784615384615384,
-0.769230769230768,-0.753846153846153,-0.738461538461538,-0.723076923076922,
-0.707692307692307,-0.692307692307692,-0.676923076923076,-0.661538461538461,
-0.646153846153846,-0.63076923076923,-0.615384615384615,-0.6,-0.584615384615384,
-0.569230769230769,-0.553846153846154,-0.538461538461538,-0.523076923076923,
-0.507692307692308,-0.492307692307692,-0.476923076923077,-0.461538461538462,
-0.446153846153846,-0.430769230769231,-0.415384615384615,-0.4,-0.384615384615385,
-0.369230769230769,-0.353846153846154,-0.338461538461538,-0.323076923076923,
-0.307692307692308,-0.292307692307692,-0.276923076923077,-0.261538461538462,
-0.246153846153846,-0.230769230769231,-0.215384615384615,-0.2,-0.184615384615385,
-0.169230769230769,-0.153846153846154,-0.138461538461538,-0.123076923076923,
-0.107692307692308,-0.0923076923076923,-0.0769230769230769,-0.0615384615384615,
-0.0461538461538462,-0.0307692307692308,-0.0153846153846154,0.),
 .UNSPECIFIED.)
CURVE()
GEOMETRIC_REPRESENTATION_ITEM()
RATIONAL_B_SPLINE_CURVE((1.,1.,1.,1.,1.,1.,1.,1.,1.,1.,1.,1.,1.,1.,1.,1.,
1.,1.,1.,1.,1.,1.,1.,1.,1.,1.,1.,1.,1.,1.,1.,1.,1.,1.,1.,1.,1.,1.,1.,1.,
1.,1.,1.,1.,1.,1.,1.,1.,1.,1.,1.,1.,1.,1.,1.,1.,1.,1.,1.,1.,1.,1.,1.,1.,
1.,1.,1.,1.,1.,1.))
REPRESENTATION_ITEM('')
);
#475=(
BOUNDED_CURVE()
B_SPLINE_CURVE(5,(#69770,#69771,#69772,#69773,#69774,#69775,#69776,#69777,
#69778,#69779,#69780,#69781,#69782,#69783,#69784,#69785,#69786,#69787,#69788,
#69789,#69790,#69791,#69792,#69793,#69794,#69795,#69796,#69797,#69798,#69799,
#69800,#69801,#69802,#69803,#69804,#69805,#69806,#69807,#69808,#69809,#69810,
#69811,#69812,#69813,#69814,#69815,#69816,#69817,#69818,#69819,#69820,#69821,
#69822,#69823,#69824,#69825,#69826,#69827,#69828,#69829,#69830,#69831,#69832,
#69833,#69834,#69835,#69836,#69837,#69838,#69839),.UNSPECIFIED.,.F.,.F.)
B_SPLINE_CURVE_WITH_KNOTS((6,1,1,1,1,1,1,1,1,1,1,1,1,1,1,1,1,1,1,1,1,1,
1,1,1,1,1,1,1,1,1,1,1,1,1,1,1,1,1,1,1,1,1,1,1,1,1,1,1,1,1,1,1,1,1,1,1,1,
1,1,1,1,1,1,1,6),(-1.,-0.984615384615383,-0.969230769230768,-0.953846153846152,
-0.938461538461537,-0.923076923076922,-0.907692307692306,-0.892307692307691,
-0.876923076923076,-0.86153846153846,-0.846153846153845,-0.83076923076923,
-0.815384615384614,-0.799999999999999,-0.784615384615384,-0.769230769230768,
-0.753846153846153,-0.738461538461538,-0.723076923076922,-0.707692307692307,
-0.692307692307692,-0.676923076923076,-0.661538461538461,-0.646153846153846,
-0.63076923076923,-0.615384615384615,-0.6,-0.584615384615384,-0.569230769230769,
-0.553846153846154,-0.538461538461538,-0.523076923076923,-0.507692307692308,
-0.492307692307692,-0.476923076923077,-0.461538461538462,-0.446153846153846,
-0.430769230769231,-0.415384615384615,-0.4,-0.384615384615385,-0.369230769230769,
-0.353846153846154,-0.338461538461538,-0.323076923076923,-0.307692307692308,
-0.292307692307692,-0.276923076923077,-0.261538461538462,-0.246153846153846,
-0.230769230769231,-0.215384615384615,-0.2,-0.184615384615385,-0.169230769230769,
-0.153846153846154,-0.138461538461538,-0.123076923076923,-0.107692307692308,
-0.0923076923076923,-0.0769230769230769,-0.0615384615384615,-0.0461538461538462,
-0.0307692307692308,-0.0153846153846154,-0.00577184337452382),
 .UNSPECIFIED.)
CURVE()
GEOMETRIC_REPRESENTATION_ITEM()
RATIONAL_B_SPLINE_CURVE((1.,1.,1.,1.,1.,1.,1.,1.,1.,1.,1.,1.,1.,1.,1.,1.,
1.,1.,1.,1.,1.,1.,1.,1.,1.,1.,1.,1.,1.,1.,1.,1.,1.,1.,1.,1.,1.,1.,1.,1.,
1.,1.,1.,1.,1.,1.,1.,1.,1.,1.,1.,1.,1.,1.,1.,1.,1.,1.,1.,1.,1.,1.,1.,1.,
1.,1.,1.,1.,1.,1.))
REPRESENTATION_ITEM('')
);
#476=(
BOUNDED_CURVE()
B_SPLINE_CURVE(5,(#69990,#69991,#69992,#69993,#69994,#69995,#69996,#69997,
#69998,#69999,#70000,#70001,#70002,#70003,#70004,#70005,#70006,#70007,#70008,
#70009,#70010,#70011,#70012,#70013,#70014,#70015,#70016,#70017,#70018,#70019,
#70020,#70021,#70022,#70023,#70024,#70025,#70026,#70027,#70028,#70029,#70030,
#70031,#70032,#70033,#70034,#70035,#70036,#70037,#70038,#70039,#70040,#70041,
#70042,#70043,#70044,#70045,#70046,#70047,#70048,#70049,#70050,#70051,#70052,
#70053,#70054,#70055,#70056,#70057,#70058,#70059),.UNSPECIFIED.,.F.,.F.)
B_SPLINE_CURVE_WITH_KNOTS((6,1,1,1,1,1,1,1,1,1,1,1,1,1,1,1,1,1,1,1,1,1,
1,1,1,1,1,1,1,1,1,1,1,1,1,1,1,1,1,1,1,1,1,1,1,1,1,1,1,1,1,1,1,1,1,1,1,1,
1,1,1,1,1,1,1,6),(-0.994228156739677,-0.984615384615383,-0.969230769230768,
-0.953846153846152,-0.938461538461537,-0.923076923076922,-0.907692307692306,
-0.892307692307691,-0.876923076923076,-0.86153846153846,-0.846153846153845,
-0.83076923076923,-0.815384615384614,-0.799999999999999,-0.784615384615384,
-0.769230769230768,-0.753846153846153,-0.738461538461538,-0.723076923076922,
-0.707692307692307,-0.692307692307692,-0.676923076923076,-0.661538461538461,
-0.646153846153846,-0.63076923076923,-0.615384615384615,-0.6,-0.584615384615384,
-0.569230769230769,-0.553846153846154,-0.538461538461538,-0.523076923076923,
-0.507692307692308,-0.492307692307692,-0.476923076923077,-0.461538461538462,
-0.446153846153846,-0.430769230769231,-0.415384615384615,-0.4,-0.384615384615385,
-0.369230769230769,-0.353846153846154,-0.338461538461538,-0.323076923076923,
-0.307692307692308,-0.292307692307692,-0.276923076923077,-0.261538461538462,
-0.246153846153846,-0.230769230769231,-0.215384615384615,-0.2,-0.184615384615385,
-0.169230769230769,-0.153846153846154,-0.138461538461538,-0.123076923076923,
-0.107692307692308,-0.0923076923076923,-0.0769230769230769,-0.0615384615384615,
-0.0461538461538462,-0.0307692307692308,-0.0153846153846154,0.),
 .UNSPECIFIED.)
CURVE()
GEOMETRIC_REPRESENTATION_ITEM()
RATIONAL_B_SPLINE_CURVE((1.,1.,1.,1.,1.,1.,1.,1.,1.,1.,1.,1.,1.,1.,1.,1.,
1.,1.,1.,1.,1.,1.,1.,1.,1.,1.,1.,1.,1.,1.,1.,1.,1.,1.,1.,1.,1.,1.,1.,1.,
1.,1.,1.,1.,1.,1.,1.,1.,1.,1.,1.,1.,1.,1.,1.,1.,1.,1.,1.,1.,1.,1.,1.,1.,
1.,1.,1.,1.,1.,1.))
REPRESENTATION_ITEM('')
);
#477=(
BOUNDED_CURVE()
B_SPLINE_CURVE(5,(#70212,#70213,#70214,#70215,#70216,#70217,#70218,#70219,
#70220,#70221,#70222,#70223,#70224,#70225,#70226,#70227,#70228,#70229,#70230,
#70231,#70232,#70233,#70234,#70235,#70236,#70237,#70238,#70239,#70240,#70241,
#70242,#70243,#70244,#70245,#70246,#70247,#70248,#70249,#70250,#70251,#70252,
#70253,#70254,#70255,#70256,#70257,#70258,#70259,#70260,#70261,#70262,#70263,
#70264,#70265,#70266,#70267,#70268,#70269,#70270,#70271,#70272,#70273,#70274,
#70275,#70276,#70277,#70278,#70279,#70280,#70281),.UNSPECIFIED.,.F.,.F.)
B_SPLINE_CURVE_WITH_KNOTS((6,1,1,1,1,1,1,1,1,1,1,1,1,1,1,1,1,1,1,1,1,1,
1,1,1,1,1,1,1,1,1,1,1,1,1,1,1,1,1,1,1,1,1,1,1,1,1,1,1,1,1,1,1,1,1,1,1,1,
1,1,1,1,1,1,1,6),(-1.,-0.984615384615383,-0.969230769230768,-0.953846153846152,
-0.938461538461537,-0.923076923076922,-0.907692307692306,-0.892307692307691,
-0.876923076923076,-0.86153846153846,-0.846153846153845,-0.83076923076923,
-0.815384615384614,-0.799999999999999,-0.784615384615384,-0.769230769230768,
-0.753846153846153,-0.738461538461538,-0.723076923076922,-0.707692307692307,
-0.692307692307692,-0.676923076923076,-0.661538461538461,-0.646153846153846,
-0.63076923076923,-0.615384615384615,-0.6,-0.584615384615384,-0.569230769230769,
-0.553846153846154,-0.538461538461538,-0.523076923076923,-0.507692307692308,
-0.492307692307692,-0.476923076923077,-0.461538461538462,-0.446153846153846,
-0.430769230769231,-0.415384615384615,-0.4,-0.384615384615385,-0.369230769230769,
-0.353846153846154,-0.338461538461538,-0.323076923076923,-0.307692307692308,
-0.292307692307692,-0.276923076923077,-0.261538461538462,-0.246153846153846,
-0.230769230769231,-0.215384615384615,-0.2,-0.184615384615385,-0.169230769230769,
-0.153846153846154,-0.138461538461538,-0.123076923076923,-0.107692307692308,
-0.0923076923076923,-0.0769230769230769,-0.0615384615384615,-0.0461538461538462,
-0.0307692307692308,-0.0153846153846154,-0.0057718433744938),
 .UNSPECIFIED.)
CURVE()
GEOMETRIC_REPRESENTATION_ITEM()
RATIONAL_B_SPLINE_CURVE((1.,1.,1.,1.,1.,1.,1.,1.,1.,1.,1.,1.,1.,1.,1.,1.,
1.,1.,1.,1.,1.,1.,1.,1.,1.,1.,1.,1.,1.,1.,1.,1.,1.,1.,1.,1.,1.,1.,1.,1.,
1.,1.,1.,1.,1.,1.,1.,1.,1.,1.,1.,1.,1.,1.,1.,1.,1.,1.,1.,1.,1.,1.,1.,1.,
1.,1.,1.,1.,1.,1.))
REPRESENTATION_ITEM('')
);
#478=(
BOUNDED_CURVE()
B_SPLINE_CURVE(5,(#70432,#70433,#70434,#70435,#70436,#70437,#70438,#70439,
#70440,#70441,#70442,#70443,#70444,#70445,#70446,#70447,#70448,#70449,#70450,
#70451,#70452,#70453,#70454,#70455,#70456,#70457,#70458,#70459,#70460,#70461,
#70462,#70463,#70464,#70465,#70466,#70467,#70468,#70469,#70470,#70471,#70472,
#70473,#70474,#70475,#70476,#70477,#70478,#70479,#70480,#70481,#70482,#70483,
#70484,#70485,#70486,#70487,#70488,#70489,#70490,#70491,#70492,#70493,#70494,
#70495,#70496,#70497,#70498,#70499,#70500,#70501),.UNSPECIFIED.,.F.,.F.)
B_SPLINE_CURVE_WITH_KNOTS((6,1,1,1,1,1,1,1,1,1,1,1,1,1,1,1,1,1,1,1,1,1,
1,1,1,1,1,1,1,1,1,1,1,1,1,1,1,1,1,1,1,1,1,1,1,1,1,1,1,1,1,1,1,1,1,1,1,1,
1,1,1,1,1,1,1,6),(-0.994228156739743,-0.984615384615383,-0.969230769230768,
-0.953846153846152,-0.938461538461537,-0.923076923076922,-0.907692307692306,
-0.892307692307691,-0.876923076923076,-0.86153846153846,-0.846153846153845,
-0.83076923076923,-0.815384615384614,-0.799999999999999,-0.784615384615384,
-0.769230769230768,-0.753846153846153,-0.738461538461538,-0.723076923076922,
-0.707692307692307,-0.692307692307692,-0.676923076923076,-0.661538461538461,
-0.646153846153846,-0.63076923076923,-0.615384615384615,-0.6,-0.584615384615384,
-0.569230769230769,-0.553846153846154,-0.538461538461538,-0.523076923076923,
-0.507692307692308,-0.492307692307692,-0.476923076923077,-0.461538461538462,
-0.446153846153846,-0.430769230769231,-0.415384615384615,-0.4,-0.384615384615385,
-0.369230769230769,-0.353846153846154,-0.338461538461538,-0.323076923076923,
-0.307692307692308,-0.292307692307692,-0.276923076923077,-0.261538461538462,
-0.246153846153846,-0.230769230769231,-0.215384615384615,-0.2,-0.184615384615385,
-0.169230769230769,-0.153846153846154,-0.138461538461538,-0.123076923076923,
-0.107692307692308,-0.0923076923076923,-0.0769230769230769,-0.0615384615384615,
-0.0461538461538462,-0.0307692307692308,-0.0153846153846154,0.),
 .UNSPECIFIED.)
CURVE()
GEOMETRIC_REPRESENTATION_ITEM()
RATIONAL_B_SPLINE_CURVE((1.,1.,1.,1.,1.,1.,1.,1.,1.,1.,1.,1.,1.,1.,1.,1.,
1.,1.,1.,1.,1.,1.,1.,1.,1.,1.,1.,1.,1.,1.,1.,1.,1.,1.,1.,1.,1.,1.,1.,1.,
1.,1.,1.,1.,1.,1.,1.,1.,1.,1.,1.,1.,1.,1.,1.,1.,1.,1.,1.,1.,1.,1.,1.,1.,
1.,1.,1.,1.,1.,1.))
REPRESENTATION_ITEM('')
);
#479=(
BOUNDED_CURVE()
B_SPLINE_CURVE(5,(#70654,#70655,#70656,#70657,#70658,#70659,#70660,#70661,
#70662,#70663,#70664,#70665,#70666,#70667,#70668,#70669,#70670,#70671,#70672,
#70673,#70674,#70675,#70676,#70677,#70678,#70679,#70680,#70681,#70682,#70683,
#70684,#70685,#70686,#70687,#70688,#70689,#70690,#70691,#70692,#70693,#70694,
#70695,#70696,#70697,#70698,#70699,#70700,#70701,#70702,#70703,#70704,#70705,
#70706,#70707,#70708,#70709,#70710,#70711,#70712,#70713,#70714,#70715,#70716,
#70717,#70718,#70719,#70720,#70721,#70722,#70723),.UNSPECIFIED.,.F.,.F.)
B_SPLINE_CURVE_WITH_KNOTS((6,1,1,1,1,1,1,1,1,1,1,1,1,1,1,1,1,1,1,1,1,1,
1,1,1,1,1,1,1,1,1,1,1,1,1,1,1,1,1,1,1,1,1,1,1,1,1,1,1,1,1,1,1,1,1,1,1,1,
1,1,1,1,1,1,1,6),(-1.,-0.984615384615383,-0.969230769230768,-0.953846153846152,
-0.938461538461537,-0.923076923076922,-0.907692307692306,-0.892307692307691,
-0.876923076923076,-0.86153846153846,-0.846153846153845,-0.83076923076923,
-0.815384615384614,-0.799999999999999,-0.784615384615384,-0.769230769230768,
-0.753846153846153,-0.738461538461538,-0.723076923076922,-0.707692307692307,
-0.692307692307692,-0.676923076923076,-0.661538461538461,-0.646153846153846,
-0.63076923076923,-0.615384615384615,-0.6,-0.584615384615384,-0.569230769230769,
-0.553846153846154,-0.538461538461538,-0.523076923076923,-0.507692307692308,
-0.492307692307692,-0.476923076923077,-0.461538461538462,-0.446153846153846,
-0.430769230769231,-0.415384615384615,-0.4,-0.384615384615385,-0.369230769230769,
-0.353846153846154,-0.338461538461538,-0.323076923076923,-0.307692307692308,
-0.292307692307692,-0.276923076923077,-0.261538461538462,-0.246153846153846,
-0.230769230769231,-0.215384615384615,-0.2,-0.184615384615385,-0.169230769230769,
-0.153846153846154,-0.138461538461538,-0.123076923076923,-0.107692307692308,
-0.0923076923076923,-0.0769230769230769,-0.0615384615384615,-0.0461538461538462,
-0.0307692307692308,-0.0153846153846154,-0.0057718433745291),
 .UNSPECIFIED.)
CURVE()
GEOMETRIC_REPRESENTATION_ITEM()
RATIONAL_B_SPLINE_CURVE((1.,1.,1.,1.,1.,1.,1.,1.,1.,1.,1.,1.,1.,1.,1.,1.,
1.,1.,1.,1.,1.,1.,1.,1.,1.,1.,1.,1.,1.,1.,1.,1.,1.,1.,1.,1.,1.,1.,1.,1.,
1.,1.,1.,1.,1.,1.,1.,1.,1.,1.,1.,1.,1.,1.,1.,1.,1.,1.,1.,1.,1.,1.,1.,1.,
1.,1.,1.,1.,1.,1.))
REPRESENTATION_ITEM('')
);
#480=(
BOUNDED_CURVE()
B_SPLINE_CURVE(5,(#70874,#70875,#70876,#70877,#70878,#70879,#70880,#70881,
#70882,#70883,#70884,#70885,#70886,#70887,#70888,#70889,#70890,#70891,#70892,
#70893,#70894,#70895,#70896,#70897,#70898,#70899,#70900,#70901,#70902,#70903,
#70904,#70905,#70906,#70907,#70908,#70909,#70910,#70911,#70912,#70913,#70914,
#70915,#70916,#70917,#70918,#70919,#70920,#70921,#70922,#70923,#70924,#70925,
#70926,#70927,#70928,#70929,#70930,#70931,#70932,#70933,#70934,#70935,#70936,
#70937,#70938,#70939,#70940,#70941,#70942,#70943),.UNSPECIFIED.,.F.,.F.)
B_SPLINE_CURVE_WITH_KNOTS((6,1,1,1,1,1,1,1,1,1,1,1,1,1,1,1,1,1,1,1,1,1,
1,1,1,1,1,1,1,1,1,1,1,1,1,1,1,1,1,1,1,1,1,1,1,1,1,1,1,1,1,1,1,1,1,1,1,1,
1,1,1,1,1,1,1,6),(-0.994228156739665,-0.984615384615383,-0.969230769230768,
-0.953846153846152,-0.938461538461537,-0.923076923076922,-0.907692307692306,
-0.892307692307691,-0.876923076923076,-0.86153846153846,-0.846153846153845,
-0.83076923076923,-0.815384615384614,-0.799999999999999,-0.784615384615384,
-0.769230769230768,-0.753846153846153,-0.738461538461538,-0.723076923076922,
-0.707692307692307,-0.692307692307692,-0.676923076923076,-0.661538461538461,
-0.646153846153846,-0.63076923076923,-0.615384615384615,-0.6,-0.584615384615384,
-0.569230769230769,-0.553846153846154,-0.538461538461538,-0.523076923076923,
-0.507692307692308,-0.492307692307692,-0.476923076923077,-0.461538461538462,
-0.446153846153846,-0.430769230769231,-0.415384615384615,-0.4,-0.384615384615385,
-0.369230769230769,-0.353846153846154,-0.338461538461538,-0.323076923076923,
-0.307692307692308,-0.292307692307692,-0.276923076923077,-0.261538461538462,
-0.246153846153846,-0.230769230769231,-0.215384615384615,-0.2,-0.184615384615385,
-0.169230769230769,-0.153846153846154,-0.138461538461538,-0.123076923076923,
-0.107692307692308,-0.0923076923076923,-0.0769230769230769,-0.0615384615384615,
-0.0461538461538462,-0.0307692307692308,-0.0153846153846154,0.),
 .UNSPECIFIED.)
CURVE()
GEOMETRIC_REPRESENTATION_ITEM()
RATIONAL_B_SPLINE_CURVE((1.,1.,1.,1.,1.,1.,1.,1.,1.,1.,1.,1.,1.,1.,1.,1.,
1.,1.,1.,1.,1.,1.,1.,1.,1.,1.,1.,1.,1.,1.,1.,1.,1.,1.,1.,1.,1.,1.,1.,1.,
1.,1.,1.,1.,1.,1.,1.,1.,1.,1.,1.,1.,1.,1.,1.,1.,1.,1.,1.,1.,1.,1.,1.,1.,
1.,1.,1.,1.,1.,1.))
REPRESENTATION_ITEM('')
);
#481=(
BOUNDED_CURVE()
B_SPLINE_CURVE(5,(#71096,#71097,#71098,#71099,#71100,#71101,#71102,#71103,
#71104,#71105,#71106,#71107,#71108,#71109,#71110,#71111,#71112,#71113,#71114,
#71115,#71116,#71117,#71118,#71119,#71120,#71121,#71122,#71123,#71124,#71125,
#71126,#71127,#71128,#71129,#71130,#71131,#71132,#71133,#71134,#71135,#71136,
#71137,#71138,#71139,#71140,#71141,#71142,#71143,#71144,#71145,#71146,#71147,
#71148,#71149,#71150,#71151,#71152,#71153,#71154,#71155,#71156,#71157,#71158,
#71159,#71160,#71161,#71162,#71163,#71164,#71165),.UNSPECIFIED.,.F.,.F.)
B_SPLINE_CURVE_WITH_KNOTS((6,1,1,1,1,1,1,1,1,1,1,1,1,1,1,1,1,1,1,1,1,1,
1,1,1,1,1,1,1,1,1,1,1,1,1,1,1,1,1,1,1,1,1,1,1,1,1,1,1,1,1,1,1,1,1,1,1,1,
1,1,1,1,1,1,1,6),(-1.,-0.984615384615383,-0.969230769230768,-0.953846153846152,
-0.938461538461537,-0.923076923076922,-0.907692307692306,-0.892307692307691,
-0.876923076923076,-0.86153846153846,-0.846153846153845,-0.83076923076923,
-0.815384615384614,-0.799999999999999,-0.784615384615384,-0.769230769230768,
-0.753846153846153,-0.738461538461538,-0.723076923076922,-0.707692307692307,
-0.692307692307692,-0.676923076923076,-0.661538461538461,-0.646153846153846,
-0.63076923076923,-0.615384615384615,-0.6,-0.584615384615384,-0.569230769230769,
-0.553846153846154,-0.538461538461538,-0.523076923076923,-0.507692307692308,
-0.492307692307692,-0.476923076923077,-0.461538461538462,-0.446153846153846,
-0.430769230769231,-0.415384615384615,-0.4,-0.384615384615385,-0.369230769230769,
-0.353846153846154,-0.338461538461538,-0.323076923076923,-0.307692307692308,
-0.292307692307692,-0.276923076923077,-0.261538461538462,-0.246153846153846,
-0.230769230769231,-0.215384615384615,-0.2,-0.184615384615385,-0.169230769230769,
-0.153846153846154,-0.138461538461538,-0.123076923076923,-0.107692307692308,
-0.0923076923076923,-0.0769230769230769,-0.0615384615384615,-0.0461538461538462,
-0.0307692307692308,-0.0153846153846154,-0.00577184337450666),
 .UNSPECIFIED.)
CURVE()
GEOMETRIC_REPRESENTATION_ITEM()
RATIONAL_B_SPLINE_CURVE((1.,1.,1.,1.,1.,1.,1.,1.,1.,1.,1.,1.,1.,1.,1.,1.,
1.,1.,1.,1.,1.,1.,1.,1.,1.,1.,1.,1.,1.,1.,1.,1.,1.,1.,1.,1.,1.,1.,1.,1.,
1.,1.,1.,1.,1.,1.,1.,1.,1.,1.,1.,1.,1.,1.,1.,1.,1.,1.,1.,1.,1.,1.,1.,1.,
1.,1.,1.,1.,1.,1.))
REPRESENTATION_ITEM('')
);
#482=(
BOUNDED_CURVE()
B_SPLINE_CURVE(5,(#71316,#71317,#71318,#71319,#71320,#71321,#71322,#71323,
#71324,#71325,#71326,#71327,#71328,#71329,#71330,#71331,#71332,#71333,#71334,
#71335,#71336,#71337,#71338,#71339,#71340,#71341,#71342,#71343,#71344,#71345,
#71346,#71347,#71348,#71349,#71350,#71351,#71352,#71353,#71354,#71355,#71356,
#71357,#71358,#71359,#71360,#71361,#71362,#71363,#71364,#71365,#71366,#71367,
#71368,#71369,#71370,#71371,#71372,#71373,#71374,#71375,#71376,#71377,#71378,
#71379,#71380,#71381,#71382,#71383,#71384,#71385),.UNSPECIFIED.,.F.,.F.)
B_SPLINE_CURVE_WITH_KNOTS((6,1,1,1,1,1,1,1,1,1,1,1,1,1,1,1,1,1,1,1,1,1,
1,1,1,1,1,1,1,1,1,1,1,1,1,1,1,1,1,1,1,1,1,1,1,1,1,1,1,1,1,1,1,1,1,1,1,1,
1,1,1,1,1,1,1,6),(-0.994228156739758,-0.984615384615383,-0.969230769230768,
-0.953846153846152,-0.938461538461537,-0.923076923076922,-0.907692307692306,
-0.892307692307691,-0.876923076923076,-0.86153846153846,-0.846153846153845,
-0.83076923076923,-0.815384615384614,-0.799999999999999,-0.784615384615384,
-0.769230769230768,-0.753846153846153,-0.738461538461538,-0.723076923076922,
-0.707692307692307,-0.692307692307692,-0.676923076923076,-0.661538461538461,
-0.646153846153846,-0.63076923076923,-0.615384615384615,-0.6,-0.584615384615384,
-0.569230769230769,-0.553846153846154,-0.538461538461538,-0.523076923076923,
-0.507692307692308,-0.492307692307692,-0.476923076923077,-0.461538461538462,
-0.446153846153846,-0.430769230769231,-0.415384615384615,-0.4,-0.384615384615385,
-0.369230769230769,-0.353846153846154,-0.338461538461538,-0.323076923076923,
-0.307692307692308,-0.292307692307692,-0.276923076923077,-0.261538461538462,
-0.246153846153846,-0.230769230769231,-0.215384615384615,-0.2,-0.184615384615385,
-0.169230769230769,-0.153846153846154,-0.138461538461538,-0.123076923076923,
-0.107692307692308,-0.0923076923076923,-0.0769230769230769,-0.0615384615384615,
-0.0461538461538462,-0.0307692307692308,-0.0153846153846154,0.),
 .UNSPECIFIED.)
CURVE()
GEOMETRIC_REPRESENTATION_ITEM()
RATIONAL_B_SPLINE_CURVE((1.,1.,1.,1.,1.,1.,1.,1.,1.,1.,1.,1.,1.,1.,1.,1.,
1.,1.,1.,1.,1.,1.,1.,1.,1.,1.,1.,1.,1.,1.,1.,1.,1.,1.,1.,1.,1.,1.,1.,1.,
1.,1.,1.,1.,1.,1.,1.,1.,1.,1.,1.,1.,1.,1.,1.,1.,1.,1.,1.,1.,1.,1.,1.,1.,
1.,1.,1.,1.,1.,1.))
REPRESENTATION_ITEM('')
);
#483=(
BOUNDED_CURVE()
B_SPLINE_CURVE(5,(#71538,#71539,#71540,#71541,#71542,#71543,#71544,#71545,
#71546,#71547,#71548,#71549,#71550,#71551,#71552,#71553,#71554,#71555,#71556,
#71557,#71558,#71559,#71560,#71561,#71562,#71563,#71564,#71565,#71566,#71567,
#71568,#71569,#71570,#71571,#71572,#71573,#71574,#71575,#71576,#71577,#71578,
#71579,#71580,#71581,#71582,#71583,#71584,#71585,#71586,#71587,#71588,#71589,
#71590,#71591,#71592,#71593,#71594,#71595,#71596,#71597,#71598,#71599,#71600,
#71601,#71602,#71603,#71604,#71605,#71606,#71607),.UNSPECIFIED.,.F.,.F.)
B_SPLINE_CURVE_WITH_KNOTS((6,1,1,1,1,1,1,1,1,1,1,1,1,1,1,1,1,1,1,1,1,1,
1,1,1,1,1,1,1,1,1,1,1,1,1,1,1,1,1,1,1,1,1,1,1,1,1,1,1,1,1,1,1,1,1,1,1,1,
1,1,1,1,1,1,1,6),(-1.,-0.984615384615383,-0.969230769230768,-0.953846153846152,
-0.938461538461537,-0.923076923076922,-0.907692307692306,-0.892307692307691,
-0.876923076923076,-0.86153846153846,-0.846153846153845,-0.83076923076923,
-0.815384615384614,-0.799999999999999,-0.784615384615384,-0.769230769230768,
-0.753846153846153,-0.738461538461538,-0.723076923076922,-0.707692307692307,
-0.692307692307692,-0.676923076923076,-0.661538461538461,-0.646153846153846,
-0.63076923076923,-0.615384615384615,-0.6,-0.584615384615384,-0.569230769230769,
-0.553846153846154,-0.538461538461538,-0.523076923076923,-0.507692307692308,
-0.492307692307692,-0.476923076923077,-0.461538461538462,-0.446153846153846,
-0.430769230769231,-0.415384615384615,-0.4,-0.384615384615385,-0.369230769230769,
-0.353846153846154,-0.338461538461538,-0.323076923076923,-0.307692307692308,
-0.292307692307692,-0.276923076923077,-0.261538461538462,-0.246153846153846,
-0.230769230769231,-0.215384615384615,-0.2,-0.184615384615385,-0.169230769230769,
-0.153846153846154,-0.138461538461538,-0.123076923076923,-0.107692307692308,
-0.0923076923076923,-0.0769230769230769,-0.0615384615384615,-0.0461538461538462,
-0.0307692307692308,-0.0153846153846154,-0.00577184337451981),
 .UNSPECIFIED.)
CURVE()
GEOMETRIC_REPRESENTATION_ITEM()
RATIONAL_B_SPLINE_CURVE((1.,1.,1.,1.,1.,1.,1.,1.,1.,1.,1.,1.,1.,1.,1.,1.,
1.,1.,1.,1.,1.,1.,1.,1.,1.,1.,1.,1.,1.,1.,1.,1.,1.,1.,1.,1.,1.,1.,1.,1.,
1.,1.,1.,1.,1.,1.,1.,1.,1.,1.,1.,1.,1.,1.,1.,1.,1.,1.,1.,1.,1.,1.,1.,1.,
1.,1.,1.,1.,1.,1.))
REPRESENTATION_ITEM('')
);
#484=(
BOUNDED_CURVE()
B_SPLINE_CURVE(5,(#71758,#71759,#71760,#71761,#71762,#71763,#71764,#71765,
#71766,#71767,#71768,#71769,#71770,#71771,#71772,#71773,#71774,#71775,#71776,
#71777,#71778,#71779,#71780,#71781,#71782,#71783,#71784,#71785,#71786,#71787,
#71788,#71789,#71790,#71791,#71792,#71793,#71794,#71795,#71796,#71797,#71798,
#71799,#71800,#71801,#71802,#71803,#71804,#71805,#71806,#71807,#71808,#71809,
#71810,#71811,#71812,#71813,#71814,#71815,#71816,#71817,#71818,#71819,#71820,
#71821,#71822,#71823,#71824,#71825,#71826,#71827),.UNSPECIFIED.,.F.,.F.)
B_SPLINE_CURVE_WITH_KNOTS((6,1,1,1,1,1,1,1,1,1,1,1,1,1,1,1,1,1,1,1,1,1,
1,1,1,1,1,1,1,1,1,1,1,1,1,1,1,1,1,1,1,1,1,1,1,1,1,1,1,1,1,1,1,1,1,1,1,1,
1,1,1,1,1,1,1,6),(-0.994228156739659,-0.984615384615383,-0.969230769230768,
-0.953846153846152,-0.938461538461537,-0.923076923076922,-0.907692307692306,
-0.892307692307691,-0.876923076923076,-0.86153846153846,-0.846153846153845,
-0.83076923076923,-0.815384615384614,-0.799999999999999,-0.784615384615384,
-0.769230769230768,-0.753846153846153,-0.738461538461538,-0.723076923076922,
-0.707692307692307,-0.692307692307692,-0.676923076923076,-0.661538461538461,
-0.646153846153846,-0.63076923076923,-0.615384615384615,-0.6,-0.584615384615384,
-0.569230769230769,-0.553846153846154,-0.538461538461538,-0.523076923076923,
-0.507692307692308,-0.492307692307692,-0.476923076923077,-0.461538461538462,
-0.446153846153846,-0.430769230769231,-0.415384615384615,-0.4,-0.384615384615385,
-0.369230769230769,-0.353846153846154,-0.338461538461538,-0.323076923076923,
-0.307692307692308,-0.292307692307692,-0.276923076923077,-0.261538461538462,
-0.246153846153846,-0.230769230769231,-0.215384615384615,-0.2,-0.184615384615385,
-0.169230769230769,-0.153846153846154,-0.138461538461538,-0.123076923076923,
-0.107692307692308,-0.0923076923076923,-0.0769230769230769,-0.0615384615384615,
-0.0461538461538462,-0.0307692307692308,-0.0153846153846154,0.),
 .UNSPECIFIED.)
CURVE()
GEOMETRIC_REPRESENTATION_ITEM()
RATIONAL_B_SPLINE_CURVE((1.,1.,1.,1.,1.,1.,1.,1.,1.,1.,1.,1.,1.,1.,1.,1.,
1.,1.,1.,1.,1.,1.,1.,1.,1.,1.,1.,1.,1.,1.,1.,1.,1.,1.,1.,1.,1.,1.,1.,1.,
1.,1.,1.,1.,1.,1.,1.,1.,1.,1.,1.,1.,1.,1.,1.,1.,1.,1.,1.,1.,1.,1.,1.,1.,
1.,1.,1.,1.,1.,1.))
REPRESENTATION_ITEM('')
);
#485=(
BOUNDED_CURVE()
B_SPLINE_CURVE(5,(#71980,#71981,#71982,#71983,#71984,#71985,#71986,#71987,
#71988,#71989,#71990,#71991,#71992,#71993,#71994,#71995,#71996,#71997,#71998,
#71999,#72000,#72001,#72002,#72003,#72004,#72005,#72006,#72007,#72008,#72009,
#72010,#72011,#72012,#72013,#72014,#72015,#72016,#72017,#72018,#72019,#72020,
#72021,#72022,#72023,#72024,#72025,#72026,#72027,#72028,#72029,#72030,#72031,
#72032,#72033,#72034,#72035,#72036,#72037,#72038,#72039,#72040,#72041,#72042,
#72043,#72044,#72045,#72046,#72047,#72048,#72049),.UNSPECIFIED.,.F.,.F.)
B_SPLINE_CURVE_WITH_KNOTS((6,1,1,1,1,1,1,1,1,1,1,1,1,1,1,1,1,1,1,1,1,1,
1,1,1,1,1,1,1,1,1,1,1,1,1,1,1,1,1,1,1,1,1,1,1,1,1,1,1,1,1,1,1,1,1,1,1,1,
1,1,1,1,1,1,1,6),(-1.,-0.984615384615383,-0.969230769230768,-0.953846153846152,
-0.938461538461537,-0.923076923076922,-0.907692307692306,-0.892307692307691,
-0.876923076923076,-0.86153846153846,-0.846153846153845,-0.83076923076923,
-0.815384615384614,-0.799999999999999,-0.784615384615384,-0.769230769230768,
-0.753846153846153,-0.738461538461538,-0.723076923076922,-0.707692307692307,
-0.692307692307692,-0.676923076923076,-0.661538461538461,-0.646153846153846,
-0.63076923076923,-0.615384615384615,-0.6,-0.584615384615384,-0.569230769230769,
-0.553846153846154,-0.538461538461538,-0.523076923076923,-0.507692307692308,
-0.492307692307692,-0.476923076923077,-0.461538461538462,-0.446153846153846,
-0.430769230769231,-0.415384615384615,-0.4,-0.384615384615385,-0.369230769230769,
-0.353846153846154,-0.338461538461538,-0.323076923076923,-0.307692307692308,
-0.292307692307692,-0.276923076923077,-0.261538461538462,-0.246153846153846,
-0.230769230769231,-0.215384615384615,-0.2,-0.184615384615385,-0.169230769230769,
-0.153846153846154,-0.138461538461538,-0.123076923076923,-0.107692307692308,
-0.0923076923076923,-0.0769230769230769,-0.0615384615384615,-0.0461538461538462,
-0.0307692307692308,-0.0153846153846154,-0.00577184337450306),
 .UNSPECIFIED.)
CURVE()
GEOMETRIC_REPRESENTATION_ITEM()
RATIONAL_B_SPLINE_CURVE((1.,1.,1.,1.,1.,1.,1.,1.,1.,1.,1.,1.,1.,1.,1.,1.,
1.,1.,1.,1.,1.,1.,1.,1.,1.,1.,1.,1.,1.,1.,1.,1.,1.,1.,1.,1.,1.,1.,1.,1.,
1.,1.,1.,1.,1.,1.,1.,1.,1.,1.,1.,1.,1.,1.,1.,1.,1.,1.,1.,1.,1.,1.,1.,1.,
1.,1.,1.,1.,1.,1.))
REPRESENTATION_ITEM('')
);
#486=(
BOUNDED_CURVE()
B_SPLINE_CURVE(5,(#72200,#72201,#72202,#72203,#72204,#72205,#72206,#72207,
#72208,#72209,#72210,#72211,#72212,#72213,#72214,#72215,#72216,#72217,#72218,
#72219,#72220,#72221,#72222,#72223,#72224,#72225,#72226,#72227,#72228,#72229,
#72230,#72231,#72232,#72233,#72234,#72235,#72236,#72237,#72238,#72239,#72240,
#72241,#72242,#72243,#72244,#72245,#72246,#72247,#72248,#72249,#72250,#72251,
#72252,#72253,#72254,#72255,#72256,#72257,#72258,#72259,#72260,#72261,#72262,
#72263,#72264,#72265,#72266,#72267,#72268,#72269),.UNSPECIFIED.,.F.,.F.)
B_SPLINE_CURVE_WITH_KNOTS((6,1,1,1,1,1,1,1,1,1,1,1,1,1,1,1,1,1,1,1,1,1,
1,1,1,1,1,1,1,1,1,1,1,1,1,1,1,1,1,1,1,1,1,1,1,1,1,1,1,1,1,1,1,1,1,1,1,1,
1,1,1,1,1,1,1,6),(-0.994228156739675,-0.984615384615383,-0.969230769230768,
-0.953846153846152,-0.938461538461537,-0.923076923076922,-0.907692307692306,
-0.892307692307691,-0.876923076923076,-0.86153846153846,-0.846153846153845,
-0.83076923076923,-0.815384615384614,-0.799999999999999,-0.784615384615384,
-0.769230769230768,-0.753846153846153,-0.738461538461538,-0.723076923076922,
-0.707692307692307,-0.692307692307692,-0.676923076923076,-0.661538461538461,
-0.646153846153846,-0.63076923076923,-0.615384615384615,-0.6,-0.584615384615384,
-0.569230769230769,-0.553846153846154,-0.538461538461538,-0.523076923076923,
-0.507692307692308,-0.492307692307692,-0.476923076923077,-0.461538461538462,
-0.446153846153846,-0.430769230769231,-0.415384615384615,-0.4,-0.384615384615385,
-0.369230769230769,-0.353846153846154,-0.338461538461538,-0.323076923076923,
-0.307692307692308,-0.292307692307692,-0.276923076923077,-0.261538461538462,
-0.246153846153846,-0.230769230769231,-0.215384615384615,-0.2,-0.184615384615385,
-0.169230769230769,-0.153846153846154,-0.138461538461538,-0.123076923076923,
-0.107692307692308,-0.0923076923076923,-0.0769230769230769,-0.0615384615384615,
-0.0461538461538462,-0.0307692307692308,-0.0153846153846154,0.),
 .UNSPECIFIED.)
CURVE()
GEOMETRIC_REPRESENTATION_ITEM()
RATIONAL_B_SPLINE_CURVE((1.,1.,1.,1.,1.,1.,1.,1.,1.,1.,1.,1.,1.,1.,1.,1.,
1.,1.,1.,1.,1.,1.,1.,1.,1.,1.,1.,1.,1.,1.,1.,1.,1.,1.,1.,1.,1.,1.,1.,1.,
1.,1.,1.,1.,1.,1.,1.,1.,1.,1.,1.,1.,1.,1.,1.,1.,1.,1.,1.,1.,1.,1.,1.,1.,
1.,1.,1.,1.,1.,1.))
REPRESENTATION_ITEM('')
);
#487=(
BOUNDED_CURVE()
B_SPLINE_CURVE(5,(#72422,#72423,#72424,#72425,#72426,#72427,#72428,#72429,
#72430,#72431,#72432,#72433,#72434,#72435,#72436,#72437,#72438,#72439,#72440,
#72441,#72442,#72443,#72444,#72445,#72446,#72447,#72448,#72449,#72450,#72451,
#72452,#72453,#72454,#72455,#72456,#72457,#72458,#72459,#72460,#72461,#72462,
#72463,#72464,#72465,#72466,#72467,#72468,#72469,#72470,#72471,#72472,#72473,
#72474,#72475,#72476,#72477,#72478,#72479,#72480,#72481,#72482,#72483,#72484,
#72485,#72486,#72487,#72488,#72489,#72490,#72491),.UNSPECIFIED.,.F.,.F.)
B_SPLINE_CURVE_WITH_KNOTS((6,1,1,1,1,1,1,1,1,1,1,1,1,1,1,1,1,1,1,1,1,1,
1,1,1,1,1,1,1,1,1,1,1,1,1,1,1,1,1,1,1,1,1,1,1,1,1,1,1,1,1,1,1,1,1,1,1,1,
1,1,1,1,1,1,1,6),(-1.,-0.984615384615383,-0.969230769230768,-0.953846153846152,
-0.938461538461537,-0.923076923076922,-0.907692307692306,-0.892307692307691,
-0.876923076923076,-0.86153846153846,-0.846153846153845,-0.83076923076923,
-0.815384615384614,-0.799999999999999,-0.784615384615384,-0.769230769230768,
-0.753846153846153,-0.738461538461538,-0.723076923076922,-0.707692307692307,
-0.692307692307692,-0.676923076923076,-0.661538461538461,-0.646153846153846,
-0.63076923076923,-0.615384615384615,-0.6,-0.584615384615384,-0.569230769230769,
-0.553846153846154,-0.538461538461538,-0.523076923076923,-0.507692307692308,
-0.492307692307692,-0.476923076923077,-0.461538461538462,-0.446153846153846,
-0.430769230769231,-0.415384615384615,-0.4,-0.384615384615385,-0.369230769230769,
-0.353846153846154,-0.338461538461538,-0.323076923076923,-0.307692307692308,
-0.292307692307692,-0.276923076923077,-0.261538461538462,-0.246153846153846,
-0.230769230769231,-0.215384615384615,-0.2,-0.184615384615385,-0.169230769230769,
-0.153846153846154,-0.138461538461538,-0.123076923076923,-0.107692307692308,
-0.0923076923076923,-0.0769230769230769,-0.0615384615384615,-0.0461538461538462,
-0.0307692307692308,-0.0153846153846154,-0.00577184337450328),
 .UNSPECIFIED.)
CURVE()
GEOMETRIC_REPRESENTATION_ITEM()
RATIONAL_B_SPLINE_CURVE((1.,1.,1.,1.,1.,1.,1.,1.,1.,1.,1.,1.,1.,1.,1.,1.,
1.,1.,1.,1.,1.,1.,1.,1.,1.,1.,1.,1.,1.,1.,1.,1.,1.,1.,1.,1.,1.,1.,1.,1.,
1.,1.,1.,1.,1.,1.,1.,1.,1.,1.,1.,1.,1.,1.,1.,1.,1.,1.,1.,1.,1.,1.,1.,1.,
1.,1.,1.,1.,1.,1.))
REPRESENTATION_ITEM('')
);
#488=(
BOUNDED_CURVE()
B_SPLINE_CURVE(5,(#72644,#72645,#72646,#72647,#72648,#72649,#72650,#72651,
#72652,#72653,#72654,#72655,#72656,#72657,#72658,#72659,#72660,#72661,#72662,
#72663,#72664,#72665,#72666,#72667,#72668,#72669,#72670,#72671,#72672,#72673,
#72674,#72675,#72676,#72677,#72678,#72679,#72680,#72681,#72682,#72683,#72684,
#72685,#72686,#72687,#72688,#72689,#72690,#72691,#72692,#72693,#72694,#72695,
#72696,#72697,#72698,#72699,#72700,#72701,#72702,#72703,#72704,#72705,#72706,
#72707,#72708,#72709,#72710,#72711,#72712,#72713),.UNSPECIFIED.,.F.,.F.)
B_SPLINE_CURVE_WITH_KNOTS((6,1,1,1,1,1,1,1,1,1,1,1,1,1,1,1,1,1,1,1,1,1,
1,1,1,1,1,1,1,1,1,1,1,1,1,1,1,1,1,1,1,1,1,1,1,1,1,1,1,1,1,1,1,1,1,1,1,1,
1,1,1,1,1,1,1,6),(-0.994228156739672,-0.984615384615383,-0.969230769230768,
-0.953846153846152,-0.938461538461537,-0.923076923076922,-0.907692307692306,
-0.892307692307691,-0.876923076923076,-0.86153846153846,-0.846153846153845,
-0.83076923076923,-0.815384615384614,-0.799999999999999,-0.784615384615384,
-0.769230769230768,-0.753846153846153,-0.738461538461538,-0.723076923076922,
-0.707692307692307,-0.692307692307692,-0.676923076923076,-0.661538461538461,
-0.646153846153846,-0.63076923076923,-0.615384615384615,-0.6,-0.584615384615384,
-0.569230769230769,-0.553846153846154,-0.538461538461538,-0.523076923076923,
-0.507692307692308,-0.492307692307692,-0.476923076923077,-0.461538461538462,
-0.446153846153846,-0.430769230769231,-0.415384615384615,-0.4,-0.384615384615385,
-0.369230769230769,-0.353846153846154,-0.338461538461538,-0.323076923076923,
-0.307692307692308,-0.292307692307692,-0.276923076923077,-0.261538461538462,
-0.246153846153846,-0.230769230769231,-0.215384615384615,-0.2,-0.184615384615385,
-0.169230769230769,-0.153846153846154,-0.138461538461538,-0.123076923076923,
-0.107692307692308,-0.0923076923076923,-0.0769230769230769,-0.0615384615384615,
-0.0461538461538462,-0.0307692307692308,-0.0153846153846154,0.),
 .UNSPECIFIED.)
CURVE()
GEOMETRIC_REPRESENTATION_ITEM()
RATIONAL_B_SPLINE_CURVE((1.,1.,1.,1.,1.,1.,1.,1.,1.,1.,1.,1.,1.,1.,1.,1.,
1.,1.,1.,1.,1.,1.,1.,1.,1.,1.,1.,1.,1.,1.,1.,1.,1.,1.,1.,1.,1.,1.,1.,1.,
1.,1.,1.,1.,1.,1.,1.,1.,1.,1.,1.,1.,1.,1.,1.,1.,1.,1.,1.,1.,1.,1.,1.,1.,
1.,1.,1.,1.,1.,1.))
REPRESENTATION_ITEM('')
);
#489=(
BOUNDED_CURVE()
B_SPLINE_CURVE(5,(#72872,#72873,#72874,#72875,#72876,#72877,#72878,#72879,
#72880,#72881,#72882,#72883,#72884,#72885,#72886,#72887,#72888,#72889,#72890,
#72891,#72892,#72893,#72894,#72895,#72896,#72897,#72898,#72899,#72900,#72901,
#72902,#72903,#72904,#72905,#72906,#72907,#72908,#72909,#72910,#72911,#72912,
#72913,#72914,#72915,#72916,#72917,#72918,#72919,#72920,#72921,#72922,#72923,
#72924,#72925,#72926,#72927,#72928,#72929,#72930,#72931,#72932,#72933,#72934,
#72935,#72936,#72937,#72938,#72939,#72940,#72941),.UNSPECIFIED.,.F.,.F.)
B_SPLINE_CURVE_WITH_KNOTS((6,1,1,1,1,1,1,1,1,1,1,1,1,1,1,1,1,1,1,1,1,1,
1,1,1,1,1,1,1,1,1,1,1,1,1,1,1,1,1,1,1,1,1,1,1,1,1,1,1,1,1,1,1,1,1,1,1,1,
1,1,1,1,1,1,1,6),(-0.994228156739704,-0.984615384615383,-0.969230769230768,
-0.953846153846152,-0.938461538461537,-0.923076923076922,-0.907692307692306,
-0.892307692307691,-0.876923076923076,-0.86153846153846,-0.846153846153845,
-0.83076923076923,-0.815384615384614,-0.799999999999999,-0.784615384615384,
-0.769230769230768,-0.753846153846153,-0.738461538461538,-0.723076923076922,
-0.707692307692307,-0.692307692307692,-0.676923076923076,-0.661538461538461,
-0.646153846153846,-0.63076923076923,-0.615384615384615,-0.6,-0.584615384615384,
-0.569230769230769,-0.553846153846154,-0.538461538461538,-0.523076923076923,
-0.507692307692308,-0.492307692307692,-0.476923076923077,-0.461538461538462,
-0.446153846153846,-0.430769230769231,-0.415384615384615,-0.4,-0.384615384615385,
-0.369230769230769,-0.353846153846154,-0.338461538461538,-0.323076923076923,
-0.307692307692308,-0.292307692307692,-0.276923076923077,-0.261538461538462,
-0.246153846153846,-0.230769230769231,-0.215384615384615,-0.2,-0.184615384615385,
-0.169230769230769,-0.153846153846154,-0.138461538461538,-0.123076923076923,
-0.107692307692308,-0.0923076923076923,-0.0769230769230769,-0.0615384615384615,
-0.0461538461538462,-0.0307692307692308,-0.0153846153846154,0.),
 .UNSPECIFIED.)
CURVE()
GEOMETRIC_REPRESENTATION_ITEM()
RATIONAL_B_SPLINE_CURVE((1.,1.,1.,1.,1.,1.,1.,1.,1.,1.,1.,1.,1.,1.,1.,1.,
1.,1.,1.,1.,1.,1.,1.,1.,1.,1.,1.,1.,1.,1.,1.,1.,1.,1.,1.,1.,1.,1.,1.,1.,
1.,1.,1.,1.,1.,1.,1.,1.,1.,1.,1.,1.,1.,1.,1.,1.,1.,1.,1.,1.,1.,1.,1.,1.,
1.,1.,1.,1.,1.,1.))
REPRESENTATION_ITEM('')
);
#490=(
BOUNDED_CURVE()
B_SPLINE_CURVE(5,(#73083,#73084,#73085,#73086,#73087,#73088,#73089,#73090,
#73091,#73092,#73093,#73094,#73095,#73096,#73097,#73098,#73099,#73100,#73101,
#73102,#73103,#73104,#73105,#73106,#73107,#73108,#73109,#73110,#73111,#73112,
#73113,#73114,#73115,#73116,#73117,#73118,#73119,#73120,#73121,#73122,#73123,
#73124,#73125,#73126,#73127,#73128,#73129,#73130,#73131,#73132,#73133,#73134,
#73135,#73136,#73137,#73138,#73139,#73140,#73141,#73142,#73143,#73144,#73145,
#73146,#73147,#73148,#73149,#73150,#73151,#73152),.UNSPECIFIED.,.F.,.F.)
B_SPLINE_CURVE_WITH_KNOTS((6,1,1,1,1,1,1,1,1,1,1,1,1,1,1,1,1,1,1,1,1,1,
1,1,1,1,1,1,1,1,1,1,1,1,1,1,1,1,1,1,1,1,1,1,1,1,1,1,1,1,1,1,1,1,1,1,1,1,
1,1,1,1,1,1,1,6),(-1.,-0.984615384615383,-0.969230769230768,-0.953846153846152,
-0.938461538461537,-0.923076923076922,-0.907692307692306,-0.892307692307691,
-0.876923076923076,-0.86153846153846,-0.846153846153845,-0.83076923076923,
-0.815384615384614,-0.799999999999999,-0.784615384615384,-0.769230769230768,
-0.753846153846153,-0.738461538461538,-0.723076923076922,-0.707692307692307,
-0.692307692307692,-0.676923076923076,-0.661538461538461,-0.646153846153846,
-0.63076923076923,-0.615384615384615,-0.6,-0.584615384615384,-0.569230769230769,
-0.553846153846154,-0.538461538461538,-0.523076923076923,-0.507692307692308,
-0.492307692307692,-0.476923076923077,-0.461538461538462,-0.446153846153846,
-0.430769230769231,-0.415384615384615,-0.4,-0.384615384615385,-0.369230769230769,
-0.353846153846154,-0.338461538461538,-0.323076923076923,-0.307692307692308,
-0.292307692307692,-0.276923076923077,-0.261538461538462,-0.246153846153846,
-0.230769230769231,-0.215384615384615,-0.2,-0.184615384615385,-0.169230769230769,
-0.153846153846154,-0.138461538461538,-0.123076923076923,-0.107692307692308,
-0.0923076923076923,-0.0769230769230769,-0.0615384615384615,-0.0461538461538462,
-0.0307692307692308,-0.0153846153846154,-0.00577184337451611),
 .UNSPECIFIED.)
CURVE()
GEOMETRIC_REPRESENTATION_ITEM()
RATIONAL_B_SPLINE_CURVE((1.,1.,1.,1.,1.,1.,1.,1.,1.,1.,1.,1.,1.,1.,1.,1.,
1.,1.,1.,1.,1.,1.,1.,1.,1.,1.,1.,1.,1.,1.,1.,1.,1.,1.,1.,1.,1.,1.,1.,1.,
1.,1.,1.,1.,1.,1.,1.,1.,1.,1.,1.,1.,1.,1.,1.,1.,1.,1.,1.,1.,1.,1.,1.,1.,
1.,1.,1.,1.,1.,1.))
REPRESENTATION_ITEM('')
);
#491=ITEM_DEFINED_TRANSFORMATION($,$,#17417,#17539);
#492=ITEM_DEFINED_TRANSFORMATION($,$,#17437,#17540);
#493=ITEM_DEFINED_TRANSFORMATION($,$,#17457,#17541);
#494=ITEM_DEFINED_TRANSFORMATION($,$,#17472,#17542);
#495=ITEM_DEFINED_TRANSFORMATION($,$,#17522,#17543);
#496=ITEM_DEFINED_TRANSFORMATION($,$,#17545,#17673);
#497=ITEM_DEFINED_TRANSFORMATION($,$,#17565,#17674);
#498=ITEM_DEFINED_TRANSFORMATION($,$,#17585,#17675);
#499=ITEM_DEFINED_TRANSFORMATION($,$,#17602,#17676);
#500=ITEM_DEFINED_TRANSFORMATION($,$,#17656,#17677);
#501=ITEM_DEFINED_TRANSFORMATION($,$,#16814,#17704);
#502=ITEM_DEFINED_TRANSFORMATION($,$,#16833,#17705);
#503=ITEM_DEFINED_TRANSFORMATION($,$,#17006,#17706);
#504=ITEM_DEFINED_TRANSFORMATION($,$,#17167,#17707);
#505=ITEM_DEFINED_TRANSFORMATION($,$,#17173,#17708);
#506=ITEM_DEFINED_TRANSFORMATION($,$,#17179,#17709);
#507=ITEM_DEFINED_TRANSFORMATION($,$,#17185,#17710);
#508=ITEM_DEFINED_TRANSFORMATION($,$,#17191,#17711);
#509=ITEM_DEFINED_TRANSFORMATION($,$,#17225,#17712);
#510=ITEM_DEFINED_TRANSFORMATION($,$,#17259,#17713);
#511=ITEM_DEFINED_TRANSFORMATION($,$,#17284,#17714);
#512=ITEM_DEFINED_TRANSFORMATION($,$,#17309,#17715);
#513=ITEM_DEFINED_TRANSFORMATION($,$,#17334,#17716);
#514=ITEM_DEFINED_TRANSFORMATION($,$,#17359,#17717);
#515=ITEM_DEFINED_TRANSFORMATION($,$,#17378,#17718);
#516=ITEM_DEFINED_TRANSFORMATION($,$,#17385,#17719);
#517=ITEM_DEFINED_TRANSFORMATION($,$,#17392,#17720);
#518=ITEM_DEFINED_TRANSFORMATION($,$,#17392,#17721);
#519=ITEM_DEFINED_TRANSFORMATION($,$,#17392,#17722);
#520=ITEM_DEFINED_TRANSFORMATION($,$,#17392,#17723);
#521=ITEM_DEFINED_TRANSFORMATION($,$,#17392,#17724);
#522=ITEM_DEFINED_TRANSFORMATION($,$,#17392,#17725);
#523=ITEM_DEFINED_TRANSFORMATION($,$,#17392,#17726);
#524=ITEM_DEFINED_TRANSFORMATION($,$,#17392,#17727);
#525=ITEM_DEFINED_TRANSFORMATION($,$,#17392,#17728);
#526=ITEM_DEFINED_TRANSFORMATION($,$,#17392,#17729);
#527=ITEM_DEFINED_TRANSFORMATION($,$,#17416,#17730);
#528=ITEM_DEFINED_TRANSFORMATION($,$,#17416,#17731);
#529=ITEM_DEFINED_TRANSFORMATION($,$,#17678,#17732);
#530=ITEM_DEFINED_TRANSFORMATION($,$,#17678,#17733);
#531=ITEM_DEFINED_TRANSFORMATION($,$,#17678,#17734);
#532=ITEM_DEFINED_TRANSFORMATION($,$,#17678,#17735);
#533=ITEM_DEFINED_TRANSFORMATION($,$,#17678,#17736);
#534=ITEM_DEFINED_TRANSFORMATION($,$,#17678,#17737);
#535=ITEM_DEFINED_TRANSFORMATION($,$,#17678,#17738);
#536=ITEM_DEFINED_TRANSFORMATION($,$,#17678,#17739);
#537=ITEM_DEFINED_TRANSFORMATION($,$,#17544,#17740);
#538=ITEM_DEFINED_TRANSFORMATION($,$,#17544,#17741);
#539=ITEM_DEFINED_TRANSFORMATION($,$,#17678,#17742);
#540=ITEM_DEFINED_TRANSFORMATION($,$,#17678,#17743);
#541=ITEM_DEFINED_TRANSFORMATION($,$,#17678,#17744);
#542=ITEM_DEFINED_TRANSFORMATION($,$,#17678,#17745);
#543=ITEM_DEFINED_TRANSFORMATION($,$,#17678,#17746);
#544=ITEM_DEFINED_TRANSFORMATION($,$,#17678,#17747);
#545=ITEM_DEFINED_TRANSFORMATION($,$,#17678,#17748);
#546=ITEM_DEFINED_TRANSFORMATION($,$,#17678,#17749);
#547=ITEM_DEFINED_TRANSFORMATION($,$,#17544,#17750);
#548=ITEM_DEFINED_TRANSFORMATION($,$,#17544,#17751);
#549=ITEM_DEFINED_TRANSFORMATION($,$,#17678,#17752);
#550=ITEM_DEFINED_TRANSFORMATION($,$,#17678,#17753);
#551=ITEM_DEFINED_TRANSFORMATION($,$,#17678,#17754);
#552=ITEM_DEFINED_TRANSFORMATION($,$,#17678,#17755);
#553=ITEM_DEFINED_TRANSFORMATION($,$,#17678,#17756);
#554=ITEM_DEFINED_TRANSFORMATION($,$,#17678,#17757);
#555=ITEM_DEFINED_TRANSFORMATION($,$,#17678,#17758);
#556=ITEM_DEFINED_TRANSFORMATION($,$,#17678,#17759);
#557=ITEM_DEFINED_TRANSFORMATION($,$,#17678,#17760);
#558=ITEM_DEFINED_TRANSFORMATION($,$,#17678,#17761);
#559=ITEM_DEFINED_TRANSFORMATION($,$,#17678,#17762);
#560=ITEM_DEFINED_TRANSFORMATION($,$,#17678,#17763);
#561=ITEM_DEFINED_TRANSFORMATION($,$,#17765,#18234);
#562=ITEM_DEFINED_TRANSFORMATION($,$,#17778,#18235);
#563=ITEM_DEFINED_TRANSFORMATION($,$,#17793,#18236);
#564=ITEM_DEFINED_TRANSFORMATION($,$,#17808,#18237);
#565=ITEM_DEFINED_TRANSFORMATION($,$,#17817,#18238);
#566=ITEM_DEFINED_TRANSFORMATION($,$,#17826,#18239);
#567=ITEM_DEFINED_TRANSFORMATION($,$,#17835,#18240);
#568=ITEM_DEFINED_TRANSFORMATION($,$,#18217,#18241);
#569=ITEM_DEFINED_TRANSFORMATION($,$,#18217,#18242);
#570=ITEM_DEFINED_TRANSFORMATION($,$,#17844,#18243);
#571=ITEM_DEFINED_TRANSFORMATION($,$,#17937,#18244);
#572=ITEM_DEFINED_TRANSFORMATION($,$,#17949,#18429);
#573=ITEM_DEFINED_TRANSFORMATION($,$,#17969,#18430);
#574=ITEM_DEFINED_TRANSFORMATION($,$,#17984,#18431);
#575=ITEM_DEFINED_TRANSFORMATION($,$,#17999,#18432);
#576=ITEM_DEFINED_TRANSFORMATION($,$,#18008,#18433);
#577=ITEM_DEFINED_TRANSFORMATION($,$,#18017,#18434);
#578=ITEM_DEFINED_TRANSFORMATION($,$,#18026,#18435);
#579=ITEM_DEFINED_TRANSFORMATION($,$,#18035,#18436);
#580=ITEM_DEFINED_TRANSFORMATION($,$,#18217,#18437);
#581=ITEM_DEFINED_TRANSFORMATION($,$,#18217,#18438);
#582=ITEM_DEFINED_TRANSFORMATION($,$,#18245,#18439);
#583=ITEM_DEFINED_TRANSFORMATION($,$,#18418,#18440);
#584=ITEM_DEFINED_TRANSFORMATION($,$,#18044,#18441);
#585=ITEM_DEFINED_TRANSFORMATION($,$,#18418,#18442);
#586=ITEM_DEFINED_TRANSFORMATION($,$,#18138,#18443);
#587=ITEM_DEFINED_TRANSFORMATION($,$,#18151,#18444);
#588=ITEM_DEFINED_TRANSFORMATION($,$,#18166,#18445);
#589=ITEM_DEFINED_TRANSFORMATION($,$,#18181,#18446);
#590=ITEM_DEFINED_TRANSFORMATION($,$,#18190,#18447);
#591=ITEM_DEFINED_TRANSFORMATION($,$,#18199,#18448);
#592=ITEM_DEFINED_TRANSFORMATION($,$,#18208,#18449);
#593=ITEM_DEFINED_TRANSFORMATION($,$,#18217,#18450);
#594=ITEM_DEFINED_TRANSFORMATION($,$,#18217,#18451);
#595=ITEM_DEFINED_TRANSFORMATION($,$,#18245,#18452);
#596=ITEM_DEFINED_TRANSFORMATION($,$,#18418,#18453);
#597=ITEM_DEFINED_TRANSFORMATION($,$,#16813,#18454);
#598=ITEM_DEFINED_TRANSFORMATION($,$,#17764,#18455);
#599=ITEM_DEFINED_TRANSFORMATION($,$,#17948,#18456);
#600=ITEM_DEFINED_TRANSFORMATION($,$,#18137,#18457);
#601=(
REPRESENTATION_RELATIONSHIP($,$,#73627,#73626)
REPRESENTATION_RELATIONSHIP_WITH_TRANSFORMATION(#491)
SHAPE_REPRESENTATION_RELATIONSHIP()
);
#602=(
REPRESENTATION_RELATIONSHIP($,$,#73628,#73626)
REPRESENTATION_RELATIONSHIP_WITH_TRANSFORMATION(#492)
SHAPE_REPRESENTATION_RELATIONSHIP()
);
#603=(
REPRESENTATION_RELATIONSHIP($,$,#73629,#73626)
REPRESENTATION_RELATIONSHIP_WITH_TRANSFORMATION(#493)
SHAPE_REPRESENTATION_RELATIONSHIP()
);
#604=(
REPRESENTATION_RELATIONSHIP($,$,#73630,#73626)
REPRESENTATION_RELATIONSHIP_WITH_TRANSFORMATION(#494)
SHAPE_REPRESENTATION_RELATIONSHIP()
);
#605=(
REPRESENTATION_RELATIONSHIP($,$,#73631,#73626)
REPRESENTATION_RELATIONSHIP_WITH_TRANSFORMATION(#495)
SHAPE_REPRESENTATION_RELATIONSHIP()
);
#606=(
REPRESENTATION_RELATIONSHIP($,$,#73633,#73632)
REPRESENTATION_RELATIONSHIP_WITH_TRANSFORMATION(#496)
SHAPE_REPRESENTATION_RELATIONSHIP()
);
#607=(
REPRESENTATION_RELATIONSHIP($,$,#73634,#73632)
REPRESENTATION_RELATIONSHIP_WITH_TRANSFORMATION(#497)
SHAPE_REPRESENTATION_RELATIONSHIP()
);
#608=(
REPRESENTATION_RELATIONSHIP($,$,#73635,#73632)
REPRESENTATION_RELATIONSHIP_WITH_TRANSFORMATION(#498)
SHAPE_REPRESENTATION_RELATIONSHIP()
);
#609=(
REPRESENTATION_RELATIONSHIP($,$,#73636,#73632)
REPRESENTATION_RELATIONSHIP_WITH_TRANSFORMATION(#499)
SHAPE_REPRESENTATION_RELATIONSHIP()
);
#610=(
REPRESENTATION_RELATIONSHIP($,$,#73637,#73632)
REPRESENTATION_RELATIONSHIP_WITH_TRANSFORMATION(#500)
SHAPE_REPRESENTATION_RELATIONSHIP()
);
#611=(
REPRESENTATION_RELATIONSHIP($,$,#73609,#73608)
REPRESENTATION_RELATIONSHIP_WITH_TRANSFORMATION(#501)
SHAPE_REPRESENTATION_RELATIONSHIP()
);
#612=(
REPRESENTATION_RELATIONSHIP($,$,#73610,#73608)
REPRESENTATION_RELATIONSHIP_WITH_TRANSFORMATION(#502)
SHAPE_REPRESENTATION_RELATIONSHIP()
);
#613=(
REPRESENTATION_RELATIONSHIP($,$,#73611,#73608)
REPRESENTATION_RELATIONSHIP_WITH_TRANSFORMATION(#503)
SHAPE_REPRESENTATION_RELATIONSHIP()
);
#614=(
REPRESENTATION_RELATIONSHIP($,$,#73612,#73608)
REPRESENTATION_RELATIONSHIP_WITH_TRANSFORMATION(#504)
SHAPE_REPRESENTATION_RELATIONSHIP()
);
#615=(
REPRESENTATION_RELATIONSHIP($,$,#73613,#73608)
REPRESENTATION_RELATIONSHIP_WITH_TRANSFORMATION(#505)
SHAPE_REPRESENTATION_RELATIONSHIP()
);
#616=(
REPRESENTATION_RELATIONSHIP($,$,#73614,#73608)
REPRESENTATION_RELATIONSHIP_WITH_TRANSFORMATION(#506)
SHAPE_REPRESENTATION_RELATIONSHIP()
);
#617=(
REPRESENTATION_RELATIONSHIP($,$,#73615,#73608)
REPRESENTATION_RELATIONSHIP_WITH_TRANSFORMATION(#507)
SHAPE_REPRESENTATION_RELATIONSHIP()
);
#618=(
REPRESENTATION_RELATIONSHIP($,$,#73616,#73608)
REPRESENTATION_RELATIONSHIP_WITH_TRANSFORMATION(#508)
SHAPE_REPRESENTATION_RELATIONSHIP()
);
#619=(
REPRESENTATION_RELATIONSHIP($,$,#73617,#73608)
REPRESENTATION_RELATIONSHIP_WITH_TRANSFORMATION(#509)
SHAPE_REPRESENTATION_RELATIONSHIP()
);
#620=(
REPRESENTATION_RELATIONSHIP($,$,#73618,#73608)
REPRESENTATION_RELATIONSHIP_WITH_TRANSFORMATION(#510)
SHAPE_REPRESENTATION_RELATIONSHIP()
);
#621=(
REPRESENTATION_RELATIONSHIP($,$,#73619,#73608)
REPRESENTATION_RELATIONSHIP_WITH_TRANSFORMATION(#511)
SHAPE_REPRESENTATION_RELATIONSHIP()
);
#622=(
REPRESENTATION_RELATIONSHIP($,$,#73620,#73608)
REPRESENTATION_RELATIONSHIP_WITH_TRANSFORMATION(#512)
SHAPE_REPRESENTATION_RELATIONSHIP()
);
#623=(
REPRESENTATION_RELATIONSHIP($,$,#73621,#73608)
REPRESENTATION_RELATIONSHIP_WITH_TRANSFORMATION(#513)
SHAPE_REPRESENTATION_RELATIONSHIP()
);
#624=(
REPRESENTATION_RELATIONSHIP($,$,#73622,#73608)
REPRESENTATION_RELATIONSHIP_WITH_TRANSFORMATION(#514)
SHAPE_REPRESENTATION_RELATIONSHIP()
);
#625=(
REPRESENTATION_RELATIONSHIP($,$,#73623,#73608)
REPRESENTATION_RELATIONSHIP_WITH_TRANSFORMATION(#515)
SHAPE_REPRESENTATION_RELATIONSHIP()
);
#626=(
REPRESENTATION_RELATIONSHIP($,$,#73624,#73608)
REPRESENTATION_RELATIONSHIP_WITH_TRANSFORMATION(#516)
SHAPE_REPRESENTATION_RELATIONSHIP()
);
#627=(
REPRESENTATION_RELATIONSHIP($,$,#73625,#73608)
REPRESENTATION_RELATIONSHIP_WITH_TRANSFORMATION(#517)
SHAPE_REPRESENTATION_RELATIONSHIP()
);
#628=(
REPRESENTATION_RELATIONSHIP($,$,#73625,#73608)
REPRESENTATION_RELATIONSHIP_WITH_TRANSFORMATION(#518)
SHAPE_REPRESENTATION_RELATIONSHIP()
);
#629=(
REPRESENTATION_RELATIONSHIP($,$,#73625,#73608)
REPRESENTATION_RELATIONSHIP_WITH_TRANSFORMATION(#519)
SHAPE_REPRESENTATION_RELATIONSHIP()
);
#630=(
REPRESENTATION_RELATIONSHIP($,$,#73625,#73608)
REPRESENTATION_RELATIONSHIP_WITH_TRANSFORMATION(#520)
SHAPE_REPRESENTATION_RELATIONSHIP()
);
#631=(
REPRESENTATION_RELATIONSHIP($,$,#73625,#73608)
REPRESENTATION_RELATIONSHIP_WITH_TRANSFORMATION(#521)
SHAPE_REPRESENTATION_RELATIONSHIP()
);
#632=(
REPRESENTATION_RELATIONSHIP($,$,#73625,#73608)
REPRESENTATION_RELATIONSHIP_WITH_TRANSFORMATION(#522)
SHAPE_REPRESENTATION_RELATIONSHIP()
);
#633=(
REPRESENTATION_RELATIONSHIP($,$,#73625,#73608)
REPRESENTATION_RELATIONSHIP_WITH_TRANSFORMATION(#523)
SHAPE_REPRESENTATION_RELATIONSHIP()
);
#634=(
REPRESENTATION_RELATIONSHIP($,$,#73625,#73608)
REPRESENTATION_RELATIONSHIP_WITH_TRANSFORMATION(#524)
SHAPE_REPRESENTATION_RELATIONSHIP()
);
#635=(
REPRESENTATION_RELATIONSHIP($,$,#73625,#73608)
REPRESENTATION_RELATIONSHIP_WITH_TRANSFORMATION(#525)
SHAPE_REPRESENTATION_RELATIONSHIP()
);
#636=(
REPRESENTATION_RELATIONSHIP($,$,#73625,#73608)
REPRESENTATION_RELATIONSHIP_WITH_TRANSFORMATION(#526)
SHAPE_REPRESENTATION_RELATIONSHIP()
);
#637=(
REPRESENTATION_RELATIONSHIP($,$,#73626,#73608)
REPRESENTATION_RELATIONSHIP_WITH_TRANSFORMATION(#527)
SHAPE_REPRESENTATION_RELATIONSHIP()
);
#638=(
REPRESENTATION_RELATIONSHIP($,$,#73626,#73608)
REPRESENTATION_RELATIONSHIP_WITH_TRANSFORMATION(#528)
SHAPE_REPRESENTATION_RELATIONSHIP()
);
#639=(
REPRESENTATION_RELATIONSHIP($,$,#73638,#73608)
REPRESENTATION_RELATIONSHIP_WITH_TRANSFORMATION(#529)
SHAPE_REPRESENTATION_RELATIONSHIP()
);
#640=(
REPRESENTATION_RELATIONSHIP($,$,#73638,#73608)
REPRESENTATION_RELATIONSHIP_WITH_TRANSFORMATION(#530)
SHAPE_REPRESENTATION_RELATIONSHIP()
);
#641=(
REPRESENTATION_RELATIONSHIP($,$,#73638,#73608)
REPRESENTATION_RELATIONSHIP_WITH_TRANSFORMATION(#531)
SHAPE_REPRESENTATION_RELATIONSHIP()
);
#642=(
REPRESENTATION_RELATIONSHIP($,$,#73638,#73608)
REPRESENTATION_RELATIONSHIP_WITH_TRANSFORMATION(#532)
SHAPE_REPRESENTATION_RELATIONSHIP()
);
#643=(
REPRESENTATION_RELATIONSHIP($,$,#73638,#73608)
REPRESENTATION_RELATIONSHIP_WITH_TRANSFORMATION(#533)
SHAPE_REPRESENTATION_RELATIONSHIP()
);
#644=(
REPRESENTATION_RELATIONSHIP($,$,#73638,#73608)
REPRESENTATION_RELATIONSHIP_WITH_TRANSFORMATION(#534)
SHAPE_REPRESENTATION_RELATIONSHIP()
);
#645=(
REPRESENTATION_RELATIONSHIP($,$,#73638,#73608)
REPRESENTATION_RELATIONSHIP_WITH_TRANSFORMATION(#535)
SHAPE_REPRESENTATION_RELATIONSHIP()
);
#646=(
REPRESENTATION_RELATIONSHIP($,$,#73638,#73608)
REPRESENTATION_RELATIONSHIP_WITH_TRANSFORMATION(#536)
SHAPE_REPRESENTATION_RELATIONSHIP()
);
#647=(
REPRESENTATION_RELATIONSHIP($,$,#73632,#73608)
REPRESENTATION_RELATIONSHIP_WITH_TRANSFORMATION(#537)
SHAPE_REPRESENTATION_RELATIONSHIP()
);
#648=(
REPRESENTATION_RELATIONSHIP($,$,#73632,#73608)
REPRESENTATION_RELATIONSHIP_WITH_TRANSFORMATION(#538)
SHAPE_REPRESENTATION_RELATIONSHIP()
);
#649=(
REPRESENTATION_RELATIONSHIP($,$,#73638,#73608)
REPRESENTATION_RELATIONSHIP_WITH_TRANSFORMATION(#539)
SHAPE_REPRESENTATION_RELATIONSHIP()
);
#650=(
REPRESENTATION_RELATIONSHIP($,$,#73638,#73608)
REPRESENTATION_RELATIONSHIP_WITH_TRANSFORMATION(#540)
SHAPE_REPRESENTATION_RELATIONSHIP()
);
#651=(
REPRESENTATION_RELATIONSHIP($,$,#73638,#73608)
REPRESENTATION_RELATIONSHIP_WITH_TRANSFORMATION(#541)
SHAPE_REPRESENTATION_RELATIONSHIP()
);
#652=(
REPRESENTATION_RELATIONSHIP($,$,#73638,#73608)
REPRESENTATION_RELATIONSHIP_WITH_TRANSFORMATION(#542)
SHAPE_REPRESENTATION_RELATIONSHIP()
);
#653=(
REPRESENTATION_RELATIONSHIP($,$,#73638,#73608)
REPRESENTATION_RELATIONSHIP_WITH_TRANSFORMATION(#543)
SHAPE_REPRESENTATION_RELATIONSHIP()
);
#654=(
REPRESENTATION_RELATIONSHIP($,$,#73638,#73608)
REPRESENTATION_RELATIONSHIP_WITH_TRANSFORMATION(#544)
SHAPE_REPRESENTATION_RELATIONSHIP()
);
#655=(
REPRESENTATION_RELATIONSHIP($,$,#73638,#73608)
REPRESENTATION_RELATIONSHIP_WITH_TRANSFORMATION(#545)
SHAPE_REPRESENTATION_RELATIONSHIP()
);
#656=(
REPRESENTATION_RELATIONSHIP($,$,#73638,#73608)
REPRESENTATION_RELATIONSHIP_WITH_TRANSFORMATION(#546)
SHAPE_REPRESENTATION_RELATIONSHIP()
);
#657=(
REPRESENTATION_RELATIONSHIP($,$,#73632,#73608)
REPRESENTATION_RELATIONSHIP_WITH_TRANSFORMATION(#547)
SHAPE_REPRESENTATION_RELATIONSHIP()
);
#658=(
REPRESENTATION_RELATIONSHIP($,$,#73632,#73608)
REPRESENTATION_RELATIONSHIP_WITH_TRANSFORMATION(#548)
SHAPE_REPRESENTATION_RELATIONSHIP()
);
#659=(
REPRESENTATION_RELATIONSHIP($,$,#73638,#73608)
REPRESENTATION_RELATIONSHIP_WITH_TRANSFORMATION(#549)
SHAPE_REPRESENTATION_RELATIONSHIP()
);
#660=(
REPRESENTATION_RELATIONSHIP($,$,#73638,#73608)
REPRESENTATION_RELATIONSHIP_WITH_TRANSFORMATION(#550)
SHAPE_REPRESENTATION_RELATIONSHIP()
);
#661=(
REPRESENTATION_RELATIONSHIP($,$,#73638,#73608)
REPRESENTATION_RELATIONSHIP_WITH_TRANSFORMATION(#551)
SHAPE_REPRESENTATION_RELATIONSHIP()
);
#662=(
REPRESENTATION_RELATIONSHIP($,$,#73638,#73608)
REPRESENTATION_RELATIONSHIP_WITH_TRANSFORMATION(#552)
SHAPE_REPRESENTATION_RELATIONSHIP()
);
#663=(
REPRESENTATION_RELATIONSHIP($,$,#73638,#73608)
REPRESENTATION_RELATIONSHIP_WITH_TRANSFORMATION(#553)
SHAPE_REPRESENTATION_RELATIONSHIP()
);
#664=(
REPRESENTATION_RELATIONSHIP($,$,#73638,#73608)
REPRESENTATION_RELATIONSHIP_WITH_TRANSFORMATION(#554)
SHAPE_REPRESENTATION_RELATIONSHIP()
);
#665=(
REPRESENTATION_RELATIONSHIP($,$,#73638,#73608)
REPRESENTATION_RELATIONSHIP_WITH_TRANSFORMATION(#555)
SHAPE_REPRESENTATION_RELATIONSHIP()
);
#666=(
REPRESENTATION_RELATIONSHIP($,$,#73638,#73608)
REPRESENTATION_RELATIONSHIP_WITH_TRANSFORMATION(#556)
SHAPE_REPRESENTATION_RELATIONSHIP()
);
#667=(
REPRESENTATION_RELATIONSHIP($,$,#73638,#73608)
REPRESENTATION_RELATIONSHIP_WITH_TRANSFORMATION(#557)
SHAPE_REPRESENTATION_RELATIONSHIP()
);
#668=(
REPRESENTATION_RELATIONSHIP($,$,#73638,#73608)
REPRESENTATION_RELATIONSHIP_WITH_TRANSFORMATION(#558)
SHAPE_REPRESENTATION_RELATIONSHIP()
);
#669=(
REPRESENTATION_RELATIONSHIP($,$,#73638,#73608)
REPRESENTATION_RELATIONSHIP_WITH_TRANSFORMATION(#559)
SHAPE_REPRESENTATION_RELATIONSHIP()
);
#670=(
REPRESENTATION_RELATIONSHIP($,$,#73638,#73608)
REPRESENTATION_RELATIONSHIP_WITH_TRANSFORMATION(#560)
SHAPE_REPRESENTATION_RELATIONSHIP()
);
#671=(
REPRESENTATION_RELATIONSHIP($,$,#73640,#73639)
REPRESENTATION_RELATIONSHIP_WITH_TRANSFORMATION(#561)
SHAPE_REPRESENTATION_RELATIONSHIP()
);
#672=(
REPRESENTATION_RELATIONSHIP($,$,#73641,#73639)
REPRESENTATION_RELATIONSHIP_WITH_TRANSFORMATION(#562)
SHAPE_REPRESENTATION_RELATIONSHIP()
);
#673=(
REPRESENTATION_RELATIONSHIP($,$,#73642,#73639)
REPRESENTATION_RELATIONSHIP_WITH_TRANSFORMATION(#563)
SHAPE_REPRESENTATION_RELATIONSHIP()
);
#674=(
REPRESENTATION_RELATIONSHIP($,$,#73643,#73639)
REPRESENTATION_RELATIONSHIP_WITH_TRANSFORMATION(#564)
SHAPE_REPRESENTATION_RELATIONSHIP()
);
#675=(
REPRESENTATION_RELATIONSHIP($,$,#73644,#73639)
REPRESENTATION_RELATIONSHIP_WITH_TRANSFORMATION(#565)
SHAPE_REPRESENTATION_RELATIONSHIP()
);
#676=(
REPRESENTATION_RELATIONSHIP($,$,#73645,#73639)
REPRESENTATION_RELATIONSHIP_WITH_TRANSFORMATION(#566)
SHAPE_REPRESENTATION_RELATIONSHIP()
);
#677=(
REPRESENTATION_RELATIONSHIP($,$,#73646,#73639)
REPRESENTATION_RELATIONSHIP_WITH_TRANSFORMATION(#567)
SHAPE_REPRESENTATION_RELATIONSHIP()
);
#678=(
REPRESENTATION_RELATIONSHIP($,$,#73667,#73639)
REPRESENTATION_RELATIONSHIP_WITH_TRANSFORMATION(#568)
SHAPE_REPRESENTATION_RELATIONSHIP()
);
#679=(
REPRESENTATION_RELATIONSHIP($,$,#73667,#73639)
REPRESENTATION_RELATIONSHIP_WITH_TRANSFORMATION(#569)
SHAPE_REPRESENTATION_RELATIONSHIP()
);
#680=(
REPRESENTATION_RELATIONSHIP($,$,#73647,#73639)
REPRESENTATION_RELATIONSHIP_WITH_TRANSFORMATION(#570)
SHAPE_REPRESENTATION_RELATIONSHIP()
);
#681=(
REPRESENTATION_RELATIONSHIP($,$,#73648,#73639)
REPRESENTATION_RELATIONSHIP_WITH_TRANSFORMATION(#571)
SHAPE_REPRESENTATION_RELATIONSHIP()
);
#682=(
REPRESENTATION_RELATIONSHIP($,$,#73650,#73649)
REPRESENTATION_RELATIONSHIP_WITH_TRANSFORMATION(#572)
SHAPE_REPRESENTATION_RELATIONSHIP()
);
#683=(
REPRESENTATION_RELATIONSHIP($,$,#73651,#73649)
REPRESENTATION_RELATIONSHIP_WITH_TRANSFORMATION(#573)
SHAPE_REPRESENTATION_RELATIONSHIP()
);
#684=(
REPRESENTATION_RELATIONSHIP($,$,#73652,#73649)
REPRESENTATION_RELATIONSHIP_WITH_TRANSFORMATION(#574)
SHAPE_REPRESENTATION_RELATIONSHIP()
);
#685=(
REPRESENTATION_RELATIONSHIP($,$,#73653,#73649)
REPRESENTATION_RELATIONSHIP_WITH_TRANSFORMATION(#575)
SHAPE_REPRESENTATION_RELATIONSHIP()
);
#686=(
REPRESENTATION_RELATIONSHIP($,$,#73654,#73649)
REPRESENTATION_RELATIONSHIP_WITH_TRANSFORMATION(#576)
SHAPE_REPRESENTATION_RELATIONSHIP()
);
#687=(
REPRESENTATION_RELATIONSHIP($,$,#73655,#73649)
REPRESENTATION_RELATIONSHIP_WITH_TRANSFORMATION(#577)
SHAPE_REPRESENTATION_RELATIONSHIP()
);
#688=(
REPRESENTATION_RELATIONSHIP($,$,#73656,#73649)
REPRESENTATION_RELATIONSHIP_WITH_TRANSFORMATION(#578)
SHAPE_REPRESENTATION_RELATIONSHIP()
);
#689=(
REPRESENTATION_RELATIONSHIP($,$,#73657,#73649)
REPRESENTATION_RELATIONSHIP_WITH_TRANSFORMATION(#579)
SHAPE_REPRESENTATION_RELATIONSHIP()
);
#690=(
REPRESENTATION_RELATIONSHIP($,$,#73667,#73649)
REPRESENTATION_RELATIONSHIP_WITH_TRANSFORMATION(#580)
SHAPE_REPRESENTATION_RELATIONSHIP()
);
#691=(
REPRESENTATION_RELATIONSHIP($,$,#73667,#73649)
REPRESENTATION_RELATIONSHIP_WITH_TRANSFORMATION(#581)
SHAPE_REPRESENTATION_RELATIONSHIP()
);
#692=(
REPRESENTATION_RELATIONSHIP($,$,#73668,#73649)
REPRESENTATION_RELATIONSHIP_WITH_TRANSFORMATION(#582)
SHAPE_REPRESENTATION_RELATIONSHIP()
);
#693=(
REPRESENTATION_RELATIONSHIP($,$,#73669,#73649)
REPRESENTATION_RELATIONSHIP_WITH_TRANSFORMATION(#583)
SHAPE_REPRESENTATION_RELATIONSHIP()
);
#694=(
REPRESENTATION_RELATIONSHIP($,$,#73658,#73649)
REPRESENTATION_RELATIONSHIP_WITH_TRANSFORMATION(#584)
SHAPE_REPRESENTATION_RELATIONSHIP()
);
#695=(
REPRESENTATION_RELATIONSHIP($,$,#73669,#73649)
REPRESENTATION_RELATIONSHIP_WITH_TRANSFORMATION(#585)
SHAPE_REPRESENTATION_RELATIONSHIP()
);
#696=(
REPRESENTATION_RELATIONSHIP($,$,#73660,#73659)
REPRESENTATION_RELATIONSHIP_WITH_TRANSFORMATION(#586)
SHAPE_REPRESENTATION_RELATIONSHIP()
);
#697=(
REPRESENTATION_RELATIONSHIP($,$,#73661,#73659)
REPRESENTATION_RELATIONSHIP_WITH_TRANSFORMATION(#587)
SHAPE_REPRESENTATION_RELATIONSHIP()
);
#698=(
REPRESENTATION_RELATIONSHIP($,$,#73662,#73659)
REPRESENTATION_RELATIONSHIP_WITH_TRANSFORMATION(#588)
SHAPE_REPRESENTATION_RELATIONSHIP()
);
#699=(
REPRESENTATION_RELATIONSHIP($,$,#73663,#73659)
REPRESENTATION_RELATIONSHIP_WITH_TRANSFORMATION(#589)
SHAPE_REPRESENTATION_RELATIONSHIP()
);
#700=(
REPRESENTATION_RELATIONSHIP($,$,#73664,#73659)
REPRESENTATION_RELATIONSHIP_WITH_TRANSFORMATION(#590)
SHAPE_REPRESENTATION_RELATIONSHIP()
);
#701=(
REPRESENTATION_RELATIONSHIP($,$,#73665,#73659)
REPRESENTATION_RELATIONSHIP_WITH_TRANSFORMATION(#591)
SHAPE_REPRESENTATION_RELATIONSHIP()
);
#702=(
REPRESENTATION_RELATIONSHIP($,$,#73666,#73659)
REPRESENTATION_RELATIONSHIP_WITH_TRANSFORMATION(#592)
SHAPE_REPRESENTATION_RELATIONSHIP()
);
#703=(
REPRESENTATION_RELATIONSHIP($,$,#73667,#73659)
REPRESENTATION_RELATIONSHIP_WITH_TRANSFORMATION(#593)
SHAPE_REPRESENTATION_RELATIONSHIP()
);
#704=(
REPRESENTATION_RELATIONSHIP($,$,#73667,#73659)
REPRESENTATION_RELATIONSHIP_WITH_TRANSFORMATION(#594)
SHAPE_REPRESENTATION_RELATIONSHIP()
);
#705=(
REPRESENTATION_RELATIONSHIP($,$,#73668,#73659)
REPRESENTATION_RELATIONSHIP_WITH_TRANSFORMATION(#595)
SHAPE_REPRESENTATION_RELATIONSHIP()
);
#706=(
REPRESENTATION_RELATIONSHIP($,$,#73669,#73659)
REPRESENTATION_RELATIONSHIP_WITH_TRANSFORMATION(#596)
SHAPE_REPRESENTATION_RELATIONSHIP()
);
#707=(
REPRESENTATION_RELATIONSHIP($,$,#73608,#73607)
REPRESENTATION_RELATIONSHIP_WITH_TRANSFORMATION(#597)
SHAPE_REPRESENTATION_RELATIONSHIP()
);
#708=(
REPRESENTATION_RELATIONSHIP($,$,#73639,#73607)
REPRESENTATION_RELATIONSHIP_WITH_TRANSFORMATION(#598)
SHAPE_REPRESENTATION_RELATIONSHIP()
);
#709=(
REPRESENTATION_RELATIONSHIP($,$,#73649,#73607)
REPRESENTATION_RELATIONSHIP_WITH_TRANSFORMATION(#599)
SHAPE_REPRESENTATION_RELATIONSHIP()
);
#710=(
REPRESENTATION_RELATIONSHIP($,$,#73659,#73607)
REPRESENTATION_RELATIONSHIP_WITH_TRANSFORMATION(#600)
SHAPE_REPRESENTATION_RELATIONSHIP()
);
#711=CONTEXT_DEPENDENT_SHAPE_REPRESENTATION(#601,#73459);
#712=CONTEXT_DEPENDENT_SHAPE_REPRESENTATION(#602,#73460);
#713=CONTEXT_DEPENDENT_SHAPE_REPRESENTATION(#603,#73461);
#714=CONTEXT_DEPENDENT_SHAPE_REPRESENTATION(#604,#73462);
#715=CONTEXT_DEPENDENT_SHAPE_REPRESENTATION(#605,#73463);
#716=CONTEXT_DEPENDENT_SHAPE_REPRESENTATION(#606,#73470);
#717=CONTEXT_DEPENDENT_SHAPE_REPRESENTATION(#607,#73471);
#718=CONTEXT_DEPENDENT_SHAPE_REPRESENTATION(#608,#73472);
#719=CONTEXT_DEPENDENT_SHAPE_REPRESENTATION(#609,#73473);
#720=CONTEXT_DEPENDENT_SHAPE_REPRESENTATION(#610,#73474);
#721=CONTEXT_DEPENDENT_SHAPE_REPRESENTATION(#611,#73476);
#722=CONTEXT_DEPENDENT_SHAPE_REPRESENTATION(#612,#73477);
#723=CONTEXT_DEPENDENT_SHAPE_REPRESENTATION(#613,#73478);
#724=CONTEXT_DEPENDENT_SHAPE_REPRESENTATION(#614,#73479);
#725=CONTEXT_DEPENDENT_SHAPE_REPRESENTATION(#615,#73480);
#726=CONTEXT_DEPENDENT_SHAPE_REPRESENTATION(#616,#73481);
#727=CONTEXT_DEPENDENT_SHAPE_REPRESENTATION(#617,#73482);
#728=CONTEXT_DEPENDENT_SHAPE_REPRESENTATION(#618,#73483);
#729=CONTEXT_DEPENDENT_SHAPE_REPRESENTATION(#619,#73484);
#730=CONTEXT_DEPENDENT_SHAPE_REPRESENTATION(#620,#73485);
#731=CONTEXT_DEPENDENT_SHAPE_REPRESENTATION(#621,#73486);
#732=CONTEXT_DEPENDENT_SHAPE_REPRESENTATION(#622,#73487);
#733=CONTEXT_DEPENDENT_SHAPE_REPRESENTATION(#623,#73488);
#734=CONTEXT_DEPENDENT_SHAPE_REPRESENTATION(#624,#73489);
#735=CONTEXT_DEPENDENT_SHAPE_REPRESENTATION(#625,#73490);
#736=CONTEXT_DEPENDENT_SHAPE_REPRESENTATION(#626,#73491);
#737=CONTEXT_DEPENDENT_SHAPE_REPRESENTATION(#627,#73492);
#738=CONTEXT_DEPENDENT_SHAPE_REPRESENTATION(#628,#73493);
#739=CONTEXT_DEPENDENT_SHAPE_REPRESENTATION(#629,#73494);
#740=CONTEXT_DEPENDENT_SHAPE_REPRESENTATION(#630,#73495);
#741=CONTEXT_DEPENDENT_SHAPE_REPRESENTATION(#631,#73496);
#742=CONTEXT_DEPENDENT_SHAPE_REPRESENTATION(#632,#73497);
#743=CONTEXT_DEPENDENT_SHAPE_REPRESENTATION(#633,#73498);
#744=CONTEXT_DEPENDENT_SHAPE_REPRESENTATION(#634,#73499);
#745=CONTEXT_DEPENDENT_SHAPE_REPRESENTATION(#635,#73500);
#746=CONTEXT_DEPENDENT_SHAPE_REPRESENTATION(#636,#73501);
#747=CONTEXT_DEPENDENT_SHAPE_REPRESENTATION(#637,#73502);
#748=CONTEXT_DEPENDENT_SHAPE_REPRESENTATION(#638,#73503);
#749=CONTEXT_DEPENDENT_SHAPE_REPRESENTATION(#639,#73504);
#750=CONTEXT_DEPENDENT_SHAPE_REPRESENTATION(#640,#73505);
#751=CONTEXT_DEPENDENT_SHAPE_REPRESENTATION(#641,#73506);
#752=CONTEXT_DEPENDENT_SHAPE_REPRESENTATION(#642,#73507);
#753=CONTEXT_DEPENDENT_SHAPE_REPRESENTATION(#643,#73508);
#754=CONTEXT_DEPENDENT_SHAPE_REPRESENTATION(#644,#73509);
#755=CONTEXT_DEPENDENT_SHAPE_REPRESENTATION(#645,#73510);
#756=CONTEXT_DEPENDENT_SHAPE_REPRESENTATION(#646,#73511);
#757=CONTEXT_DEPENDENT_SHAPE_REPRESENTATION(#647,#73512);
#758=CONTEXT_DEPENDENT_SHAPE_REPRESENTATION(#648,#73513);
#759=CONTEXT_DEPENDENT_SHAPE_REPRESENTATION(#649,#73514);
#760=CONTEXT_DEPENDENT_SHAPE_REPRESENTATION(#650,#73515);
#761=CONTEXT_DEPENDENT_SHAPE_REPRESENTATION(#651,#73516);
#762=CONTEXT_DEPENDENT_SHAPE_REPRESENTATION(#652,#73517);
#763=CONTEXT_DEPENDENT_SHAPE_REPRESENTATION(#653,#73518);
#764=CONTEXT_DEPENDENT_SHAPE_REPRESENTATION(#654,#73519);
#765=CONTEXT_DEPENDENT_SHAPE_REPRESENTATION(#655,#73520);
#766=CONTEXT_DEPENDENT_SHAPE_REPRESENTATION(#656,#73521);
#767=CONTEXT_DEPENDENT_SHAPE_REPRESENTATION(#657,#73522);
#768=CONTEXT_DEPENDENT_SHAPE_REPRESENTATION(#658,#73523);
#769=CONTEXT_DEPENDENT_SHAPE_REPRESENTATION(#659,#73524);
#770=CONTEXT_DEPENDENT_SHAPE_REPRESENTATION(#660,#73525);
#771=CONTEXT_DEPENDENT_SHAPE_REPRESENTATION(#661,#73526);
#772=CONTEXT_DEPENDENT_SHAPE_REPRESENTATION(#662,#73527);
#773=CONTEXT_DEPENDENT_SHAPE_REPRESENTATION(#663,#73528);
#774=CONTEXT_DEPENDENT_SHAPE_REPRESENTATION(#664,#73529);
#775=CONTEXT_DEPENDENT_SHAPE_REPRESENTATION(#665,#73530);
#776=CONTEXT_DEPENDENT_SHAPE_REPRESENTATION(#666,#73531);
#777=CONTEXT_DEPENDENT_SHAPE_REPRESENTATION(#667,#73532);
#778=CONTEXT_DEPENDENT_SHAPE_REPRESENTATION(#668,#73533);
#779=CONTEXT_DEPENDENT_SHAPE_REPRESENTATION(#669,#73534);
#780=CONTEXT_DEPENDENT_SHAPE_REPRESENTATION(#670,#73535);
#781=CONTEXT_DEPENDENT_SHAPE_REPRESENTATION(#671,#73565);
#782=CONTEXT_DEPENDENT_SHAPE_REPRESENTATION(#672,#73566);
#783=CONTEXT_DEPENDENT_SHAPE_REPRESENTATION(#673,#73567);
#784=CONTEXT_DEPENDENT_SHAPE_REPRESENTATION(#674,#73568);
#785=CONTEXT_DEPENDENT_SHAPE_REPRESENTATION(#675,#73569);
#786=CONTEXT_DEPENDENT_SHAPE_REPRESENTATION(#676,#73570);
#787=CONTEXT_DEPENDENT_SHAPE_REPRESENTATION(#677,#73571);
#788=CONTEXT_DEPENDENT_SHAPE_REPRESENTATION(#678,#73572);
#789=CONTEXT_DEPENDENT_SHAPE_REPRESENTATION(#679,#73573);
#790=CONTEXT_DEPENDENT_SHAPE_REPRESENTATION(#680,#73574);
#791=CONTEXT_DEPENDENT_SHAPE_REPRESENTATION(#681,#73575);
#792=CONTEXT_DEPENDENT_SHAPE_REPRESENTATION(#682,#73578);
#793=CONTEXT_DEPENDENT_SHAPE_REPRESENTATION(#683,#73579);
#794=CONTEXT_DEPENDENT_SHAPE_REPRESENTATION(#684,#73580);
#795=CONTEXT_DEPENDENT_SHAPE_REPRESENTATION(#685,#73581);
#796=CONTEXT_DEPENDENT_SHAPE_REPRESENTATION(#686,#73582);
#797=CONTEXT_DEPENDENT_SHAPE_REPRESENTATION(#687,#73583);
#798=CONTEXT_DEPENDENT_SHAPE_REPRESENTATION(#688,#73584);
#799=CONTEXT_DEPENDENT_SHAPE_REPRESENTATION(#689,#73585);
#800=CONTEXT_DEPENDENT_SHAPE_REPRESENTATION(#690,#73586);
#801=CONTEXT_DEPENDENT_SHAPE_REPRESENTATION(#691,#73587);
#802=CONTEXT_DEPENDENT_SHAPE_REPRESENTATION(#692,#73588);
#803=CONTEXT_DEPENDENT_SHAPE_REPRESENTATION(#693,#73589);
#804=CONTEXT_DEPENDENT_SHAPE_REPRESENTATION(#694,#73590);
#805=CONTEXT_DEPENDENT_SHAPE_REPRESENTATION(#695,#73591);
#806=CONTEXT_DEPENDENT_SHAPE_REPRESENTATION(#696,#73592);
#807=CONTEXT_DEPENDENT_SHAPE_REPRESENTATION(#697,#73593);
#808=CONTEXT_DEPENDENT_SHAPE_REPRESENTATION(#698,#73594);
#809=CONTEXT_DEPENDENT_SHAPE_REPRESENTATION(#699,#73595);
#810=CONTEXT_DEPENDENT_SHAPE_REPRESENTATION(#700,#73596);
#811=CONTEXT_DEPENDENT_SHAPE_REPRESENTATION(#701,#73597);
#812=CONTEXT_DEPENDENT_SHAPE_REPRESENTATION(#702,#73598);
#813=CONTEXT_DEPENDENT_SHAPE_REPRESENTATION(#703,#73599);
#814=CONTEXT_DEPENDENT_SHAPE_REPRESENTATION(#704,#73600);
#815=CONTEXT_DEPENDENT_SHAPE_REPRESENTATION(#705,#73601);
#816=CONTEXT_DEPENDENT_SHAPE_REPRESENTATION(#706,#73602);
#817=CONTEXT_DEPENDENT_SHAPE_REPRESENTATION(#707,#73603);
#818=CONTEXT_DEPENDENT_SHAPE_REPRESENTATION(#708,#73604);
#819=CONTEXT_DEPENDENT_SHAPE_REPRESENTATION(#709,#73605);
#820=CONTEXT_DEPENDENT_SHAPE_REPRESENTATION(#710,#73606);
#821=NEXT_ASSEMBLY_USAGE_OCCURRENCE('Inner ring:1','Inner ring:1',
'Inner ring:1',#73690,#73691,'Inner ring:1');
#822=NEXT_ASSEMBLY_USAGE_OCCURRENCE('Outer ring:1','Outer ring:1',
'Outer ring:1',#73690,#73692,'Outer ring:1');
#823=NEXT_ASSEMBLY_USAGE_OCCURRENCE('Balls:1','Balls:1','Balls:1',#73690,
#73693,'Balls:1');
#824=NEXT_ASSEMBLY_USAGE_OCCURRENCE('Cage:1','Cage:1','Cage:1',#73690,#73694,
'Cage:1');
#825=NEXT_ASSEMBLY_USAGE_OCCURRENCE('Seals 2RS:1','Seals 2RS:1',
'Seals 2RS:1',#73690,#73695,'Seals 2RS:1');
#826=NEXT_ASSEMBLY_USAGE_OCCURRENCE('Inner ring (1):1',
'Inner ring (1):1','Inner ring (1):1',#73696,#73697,'Inner ring (1):1');
#827=NEXT_ASSEMBLY_USAGE_OCCURRENCE('Outer ring (1):1',
'Outer ring (1):1','Outer ring (1):1',#73696,#73698,'Outer ring (1):1');
#828=NEXT_ASSEMBLY_USAGE_OCCURRENCE('Balls (1):1','Balls (1):1',
'Balls (1):1',#73696,#73699,'Balls (1):1');
#829=NEXT_ASSEMBLY_USAGE_OCCURRENCE('Cage (1):1','Cage (1):1',
'Cage (1):1',#73696,#73700,'Cage (1):1');
#830=NEXT_ASSEMBLY_USAGE_OCCURRENCE('Seals 2RS (1):1','Seals 2RS (1):1',
'Seals 2RS (1):1',#73696,#73701,'Seals 2RS (1):1');
#831=NEXT_ASSEMBLY_USAGE_OCCURRENCE('Base:1','Base:1','Base:1',#73672,#73673,
'Base:1');
#832=NEXT_ASSEMBLY_USAGE_OCCURRENCE('Lower housing:1','Lower housing:1',
'Lower housing:1',#73672,#73674,'Lower housing:1');
#833=NEXT_ASSEMBLY_USAGE_OCCURRENCE('Upper housing:1','Upper housing:1',
'Upper housing:1',#73672,#73675,'Upper housing:1');
#834=NEXT_ASSEMBLY_USAGE_OCCURRENCE('Split dowel:1','Split dowel:1',
'Split dowel:1',#73672,#73676,'Split dowel:1');
#835=NEXT_ASSEMBLY_USAGE_OCCURRENCE('Split dowel (1):1',
'Split dowel (1):1','Split dowel (1):1',#73672,#73677,
'Split dowel (1):1');
#836=NEXT_ASSEMBLY_USAGE_OCCURRENCE('Split dowel (2):1',
'Split dowel (2):1','Split dowel (2):1',#73672,#73678,
'Split dowel (2):1');
#837=NEXT_ASSEMBLY_USAGE_OCCURRENCE('Split dowel (3):1',
'Split dowel (3):1','Split dowel (3):1',#73672,#73679,
'Split dowel (3):1');
#838=NEXT_ASSEMBLY_USAGE_OCCURRENCE('mm end cap:1','mm end cap:1',
'mm end cap:1',#73672,#73680,'mm end cap:1');
#839=NEXT_ASSEMBLY_USAGE_OCCURRENCE('mm end cap (1):1',
'mm end cap (1):1','mm end cap (1):1',#73672,#73681,'mm end cap (1):1');
#840=NEXT_ASSEMBLY_USAGE_OCCURRENCE('mm end cap (2):1',
'mm end cap (2):1','mm end cap (2):1',#73672,#73682,'mm end cap (2):1');
#841=NEXT_ASSEMBLY_USAGE_OCCURRENCE('mm end cap (3):1',
'mm end cap (3):1','mm end cap (3):1',#73672,#73683,'mm end cap (3):1');
#842=NEXT_ASSEMBLY_USAGE_OCCURRENCE('mm end cap (4):1',
'mm end cap (4):1','mm end cap (4):1',#73672,#73684,'mm end cap (4):1');
#843=NEXT_ASSEMBLY_USAGE_OCCURRENCE('mm end cap (5):1',
'mm end cap (5):1','mm end cap (5):1',#73672,#73685,'mm end cap (5):1');
#844=NEXT_ASSEMBLY_USAGE_OCCURRENCE('Inspection cover:1',
'Inspection cover:1','Inspection cover:1',#73672,#73686,
'Inspection cover:1');
#845=NEXT_ASSEMBLY_USAGE_OCCURRENCE('Foot strip:1','Foot strip:1',
'Foot strip:1',#73672,#73687,'Foot strip:1');
#846=NEXT_ASSEMBLY_USAGE_OCCURRENCE('Foot strip (1):1',
'Foot strip (1):1','Foot strip (1):1',#73672,#73688,'Foot strip (1):1');
#847=NEXT_ASSEMBLY_USAGE_OCCURRENCE('M6x18 mounting screw:2',
'M6x18 mounting screw:2','M6x18 mounting screw:2',#73672,#73689,
'M6x18 mounting screw:2');
#848=NEXT_ASSEMBLY_USAGE_OCCURRENCE('M6x18 mounting screw:3',
'M6x18 mounting screw:3','M6x18 mounting screw:3',#73672,#73689,
'M6x18 mounting screw:3');
#849=NEXT_ASSEMBLY_USAGE_OCCURRENCE('M6x18 mounting screw:4',
'M6x18 mounting screw:4','M6x18 mounting screw:4',#73672,#73689,
'M6x18 mounting screw:4');
#850=NEXT_ASSEMBLY_USAGE_OCCURRENCE('M6x18 mounting screw:5',
'M6x18 mounting screw:5','M6x18 mounting screw:5',#73672,#73689,
'M6x18 mounting screw:5');
#851=NEXT_ASSEMBLY_USAGE_OCCURRENCE('M6x18 mounting screw:6',
'M6x18 mounting screw:6','M6x18 mounting screw:6',#73672,#73689,
'M6x18 mounting screw:6');
#852=NEXT_ASSEMBLY_USAGE_OCCURRENCE('M6x18 mounting screw:7',
'M6x18 mounting screw:7','M6x18 mounting screw:7',#73672,#73689,
'M6x18 mounting screw:7');
#853=NEXT_ASSEMBLY_USAGE_OCCURRENCE('M6x18 mounting screw:8',
'M6x18 mounting screw:8','M6x18 mounting screw:8',#73672,#73689,
'M6x18 mounting screw:8');
#854=NEXT_ASSEMBLY_USAGE_OCCURRENCE('M6x18 mounting screw:9',
'M6x18 mounting screw:9','M6x18 mounting screw:9',#73672,#73689,
'M6x18 mounting screw:9');
#855=NEXT_ASSEMBLY_USAGE_OCCURRENCE('M6x18 mounting screw:10',
'M6x18 mounting screw:10','M6x18 mounting screw:10',#73672,#73689,
'M6x18 mounting screw:10');
#856=NEXT_ASSEMBLY_USAGE_OCCURRENCE('M6x18 mounting screw:11',
'M6x18 mounting screw:11','M6x18 mounting screw:11',#73672,#73689,
'M6x18 mounting screw:11');
#857=NEXT_ASSEMBLY_USAGE_OCCURRENCE(
'Sealed Ball Bearing - 12 x 32 x 10 mm:2',
'Sealed Ball Bearing - 12 x 32 x 10 mm:2',
'Sealed Ball Bearing - 12 x 32 x 10 mm:2',#73672,#73690,
'Sealed Ball Bearing - 12 x 32 x 10 mm:2');
#858=NEXT_ASSEMBLY_USAGE_OCCURRENCE(
'Sealed Ball Bearing - 12 x 32 x 10 mm:3',
'Sealed Ball Bearing - 12 x 32 x 10 mm:3',
'Sealed Ball Bearing - 12 x 32 x 10 mm:3',#73672,#73690,
'Sealed Ball Bearing - 12 x 32 x 10 mm:3');
#859=NEXT_ASSEMBLY_USAGE_OCCURRENCE('Cap Screw - M4x16:2',
'Cap Screw - M4x16:2','Cap Screw - M4x16:2',#73672,#73702,
'Cap Screw - M4x16:2');
#860=NEXT_ASSEMBLY_USAGE_OCCURRENCE('Cap Screw - M4x16:3',
'Cap Screw - M4x16:3','Cap Screw - M4x16:3',#73672,#73702,
'Cap Screw - M4x16:3');
#861=NEXT_ASSEMBLY_USAGE_OCCURRENCE('Cap Screw - M4x16:4',
'Cap Screw - M4x16:4','Cap Screw - M4x16:4',#73672,#73702,
'Cap Screw - M4x16:4');
#862=NEXT_ASSEMBLY_USAGE_OCCURRENCE('Cap Screw - M4x16:5',
'Cap Screw - M4x16:5','Cap Screw - M4x16:5',#73672,#73702,
'Cap Screw - M4x16:5');
#863=NEXT_ASSEMBLY_USAGE_OCCURRENCE('Cap Screw - M4x16:6',
'Cap Screw - M4x16:6','Cap Screw - M4x16:6',#73672,#73702,
'Cap Screw - M4x16:6');
#864=NEXT_ASSEMBLY_USAGE_OCCURRENCE('Cap Screw - M4x16:7',
'Cap Screw - M4x16:7','Cap Screw - M4x16:7',#73672,#73702,
'Cap Screw - M4x16:7');
#865=NEXT_ASSEMBLY_USAGE_OCCURRENCE('Cap Screw - M4x16:8',
'Cap Screw - M4x16:8','Cap Screw - M4x16:8',#73672,#73702,
'Cap Screw - M4x16:8');
#866=NEXT_ASSEMBLY_USAGE_OCCURRENCE('Cap Screw - M4x16:9',
'Cap Screw - M4x16:9','Cap Screw - M4x16:9',#73672,#73702,
'Cap Screw - M4x16:9');
#867=NEXT_ASSEMBLY_USAGE_OCCURRENCE(
'Sealed Ball Bearing - 20 x 47 x 14 mm:2',
'Sealed Ball Bearing - 20 x 47 x 14 mm:2',
'Sealed Ball Bearing - 20 x 47 x 14 mm:2',#73672,#73696,
'Sealed Ball Bearing - 20 x 47 x 14 mm:2');
#868=NEXT_ASSEMBLY_USAGE_OCCURRENCE(
'Sealed Ball Bearing - 20 x 47 x 14 mm:3',
'Sealed Ball Bearing - 20 x 47 x 14 mm:3',
'Sealed Ball Bearing - 20 x 47 x 14 mm:3',#73672,#73696,
'Sealed Ball Bearing - 20 x 47 x 14 mm:3');
#869=NEXT_ASSEMBLY_USAGE_OCCURRENCE('Cap Screw - M4x16:10',
'Cap Screw - M4x16:10','Cap Screw - M4x16:10',#73672,#73702,
'Cap Screw - M4x16:10');
#870=NEXT_ASSEMBLY_USAGE_OCCURRENCE('Cap Screw - M4x16:11',
'Cap Screw - M4x16:11','Cap Screw - M4x16:11',#73672,#73702,
'Cap Screw - M4x16:11');
#871=NEXT_ASSEMBLY_USAGE_OCCURRENCE('Cap Screw - M4x16:12',
'Cap Screw - M4x16:12','Cap Screw - M4x16:12',#73672,#73702,
'Cap Screw - M4x16:12');
#872=NEXT_ASSEMBLY_USAGE_OCCURRENCE('Cap Screw - M4x16:13',
'Cap Screw - M4x16:13','Cap Screw - M4x16:13',#73672,#73702,
'Cap Screw - M4x16:13');
#873=NEXT_ASSEMBLY_USAGE_OCCURRENCE('Cap Screw - M4x16:14',
'Cap Screw - M4x16:14','Cap Screw - M4x16:14',#73672,#73702,
'Cap Screw - M4x16:14');
#874=NEXT_ASSEMBLY_USAGE_OCCURRENCE('Cap Screw - M4x16:15',
'Cap Screw - M4x16:15','Cap Screw - M4x16:15',#73672,#73702,
'Cap Screw - M4x16:15');
#875=NEXT_ASSEMBLY_USAGE_OCCURRENCE('Cap Screw - M4x16:16',
'Cap Screw - M4x16:16','Cap Screw - M4x16:16',#73672,#73702,
'Cap Screw - M4x16:16');
#876=NEXT_ASSEMBLY_USAGE_OCCURRENCE('Cap Screw - M4x16:17',
'Cap Screw - M4x16:17','Cap Screw - M4x16:17',#73672,#73702,
'Cap Screw - M4x16:17');
#877=NEXT_ASSEMBLY_USAGE_OCCURRENCE(
'Sealed Ball Bearing - 20 x 47 x 14 mm:4',
'Sealed Ball Bearing - 20 x 47 x 14 mm:4',
'Sealed Ball Bearing - 20 x 47 x 14 mm:4',#73672,#73696,
'Sealed Ball Bearing - 20 x 47 x 14 mm:4');
#878=NEXT_ASSEMBLY_USAGE_OCCURRENCE(
'Sealed Ball Bearing - 20 x 47 x 14 mm:5',
'Sealed Ball Bearing - 20 x 47 x 14 mm:5',
'Sealed Ball Bearing - 20 x 47 x 14 mm:5',#73672,#73696,
'Sealed Ball Bearing - 20 x 47 x 14 mm:5');
#879=NEXT_ASSEMBLY_USAGE_OCCURRENCE('Cap Screw - M4x16:18',
'Cap Screw - M4x16:18','Cap Screw - M4x16:18',#73672,#73702,
'Cap Screw - M4x16:18');
#880=NEXT_ASSEMBLY_USAGE_OCCURRENCE('Cap Screw - M4x16:19',
'Cap Screw - M4x16:19','Cap Screw - M4x16:19',#73672,#73702,
'Cap Screw - M4x16:19');
#881=NEXT_ASSEMBLY_USAGE_OCCURRENCE('Cap Screw - M4x16:20',
'Cap Screw - M4x16:20','Cap Screw - M4x16:20',#73672,#73702,
'Cap Screw - M4x16:20');
#882=NEXT_ASSEMBLY_USAGE_OCCURRENCE('Cap Screw - M4x16:21',
'Cap Screw - M4x16:21','Cap Screw - M4x16:21',#73672,#73702,
'Cap Screw - M4x16:21');
#883=NEXT_ASSEMBLY_USAGE_OCCURRENCE('Cap Screw - M4x16:22',
'Cap Screw - M4x16:22','Cap Screw - M4x16:22',#73672,#73702,
'Cap Screw - M4x16:22');
#884=NEXT_ASSEMBLY_USAGE_OCCURRENCE('Cap Screw - M4x16:23',
'Cap Screw - M4x16:23','Cap Screw - M4x16:23',#73672,#73702,
'Cap Screw - M4x16:23');
#885=NEXT_ASSEMBLY_USAGE_OCCURRENCE('Cap Screw - M4x16:24',
'Cap Screw - M4x16:24','Cap Screw - M4x16:24',#73672,#73702,
'Cap Screw - M4x16:24');
#886=NEXT_ASSEMBLY_USAGE_OCCURRENCE('Cap Screw - M4x16:25',
'Cap Screw - M4x16:25','Cap Screw - M4x16:25',#73672,#73702,
'Cap Screw - M4x16:25');
#887=NEXT_ASSEMBLY_USAGE_OCCURRENCE('Cap Screw - M4x16:26',
'Cap Screw - M4x16:26','Cap Screw - M4x16:26',#73672,#73702,
'Cap Screw - M4x16:26');
#888=NEXT_ASSEMBLY_USAGE_OCCURRENCE('Cap Screw - M4x16:27',
'Cap Screw - M4x16:27','Cap Screw - M4x16:27',#73672,#73702,
'Cap Screw - M4x16:27');
#889=NEXT_ASSEMBLY_USAGE_OCCURRENCE('Cap Screw - M4x16:28',
'Cap Screw - M4x16:28','Cap Screw - M4x16:28',#73672,#73702,
'Cap Screw - M4x16:28');
#890=NEXT_ASSEMBLY_USAGE_OCCURRENCE('Cap Screw - M4x16:29',
'Cap Screw - M4x16:29','Cap Screw - M4x16:29',#73672,#73702,
'Cap Screw - M4x16:29');
#891=NEXT_ASSEMBLY_USAGE_OCCURRENCE('Shaft 1:1','Shaft 1:1','Shaft 1:1',
#73703,#73704,'Shaft 1:1');
#892=NEXT_ASSEMBLY_USAGE_OCCURRENCE('mm shaft collar:1',
'mm shaft collar:1','mm shaft collar:1',#73703,#73705,
'mm shaft collar:1');
#893=NEXT_ASSEMBLY_USAGE_OCCURRENCE('mm shaft collar (1):1',
'mm shaft collar (1):1','mm shaft collar (1):1',#73703,#73706,
'mm shaft collar (1):1');
#894=NEXT_ASSEMBLY_USAGE_OCCURRENCE('mm outer spacer:1',
'mm outer spacer:1','mm outer spacer:1',#73703,#73707,
'mm outer spacer:1');
#895=NEXT_ASSEMBLY_USAGE_OCCURRENCE('mm outer spacer (1):1',
'mm outer spacer (1):1','mm outer spacer (1):1',#73703,#73708,
'mm outer spacer (1):1');
#896=NEXT_ASSEMBLY_USAGE_OCCURRENCE('Spacer d12 L25:1',
'Spacer d12 L25:1','Spacer d12 L25:1',#73703,#73709,'Spacer d12 L25:1');
#897=NEXT_ASSEMBLY_USAGE_OCCURRENCE('Spacer d12 L53:1',
'Spacer d12 L53:1','Spacer d12 L53:1',#73703,#73710,'Spacer d12 L53:1');
#898=NEXT_ASSEMBLY_USAGE_OCCURRENCE('Socket Set Screw - M5x8:2',
'Socket Set Screw - M5x8:2','Socket Set Screw - M5x8:2',#73703,#73731,
'Socket Set Screw - M5x8:2');
#899=NEXT_ASSEMBLY_USAGE_OCCURRENCE('Socket Set Screw - M5x8:3',
'Socket Set Screw - M5x8:3','Socket Set Screw - M5x8:3',#73703,#73731,
'Socket Set Screw - M5x8:3');
#900=NEXT_ASSEMBLY_USAGE_OCCURRENCE(
'Spur Gear - Module 2, 20 Teeth, 12 mm Bore:2',
'Spur Gear - Module 2, 20 Teeth, 12 mm Bore:2',
'Spur Gear - Module 2, 20 Teeth, 12 mm Bore:2',#73703,#73711,
'Spur Gear - Module 2, 20 Teeth, 12 mm Bore:2');
#901=NEXT_ASSEMBLY_USAGE_OCCURRENCE('Key 4x4x14:2','Key 4x4x14:2',
'Key 4x4x14:2',#73703,#73712,'Key 4x4x14:2');
#902=NEXT_ASSEMBLY_USAGE_OCCURRENCE('Shaft 2:1','Shaft 2:1','Shaft 2:1',
#73713,#73714,'Shaft 2:1');
#903=NEXT_ASSEMBLY_USAGE_OCCURRENCE('mm shaft collar (2):1',
'mm shaft collar (2):1','mm shaft collar (2):1',#73713,#73715,
'mm shaft collar (2):1');
#904=NEXT_ASSEMBLY_USAGE_OCCURRENCE('mm shaft collar (3):1',
'mm shaft collar (3):1','mm shaft collar (3):1',#73713,#73716,
'mm shaft collar (3):1');
#905=NEXT_ASSEMBLY_USAGE_OCCURRENCE('mm outer spacer (2):1',
'mm outer spacer (2):1','mm outer spacer (2):1',#73713,#73717,
'mm outer spacer (2):1');
#906=NEXT_ASSEMBLY_USAGE_OCCURRENCE('mm outer spacer (3):1',
'mm outer spacer (3):1','mm outer spacer (3):1',#73713,#73718,
'mm outer spacer (3):1');
#907=NEXT_ASSEMBLY_USAGE_OCCURRENCE('Spacer d20 L23:1',
'Spacer d20 L23:1','Spacer d20 L23:1',#73713,#73719,'Spacer d20 L23:1');
#908=NEXT_ASSEMBLY_USAGE_OCCURRENCE('Spacer d20 L8:1','Spacer d20 L8:1',
'Spacer d20 L8:1',#73713,#73720,'Spacer d20 L8:1');
#909=NEXT_ASSEMBLY_USAGE_OCCURRENCE('Spacer d20 L11:1',
'Spacer d20 L11:1','Spacer d20 L11:1',#73713,#73721,'Spacer d20 L11:1');
#910=NEXT_ASSEMBLY_USAGE_OCCURRENCE('Socket Set Screw - M5x8:4',
'Socket Set Screw - M5x8:4','Socket Set Screw - M5x8:4',#73713,#73731,
'Socket Set Screw - M5x8:4');
#911=NEXT_ASSEMBLY_USAGE_OCCURRENCE('Socket Set Screw - M5x8:5',
'Socket Set Screw - M5x8:5','Socket Set Screw - M5x8:5',#73713,#73731,
'Socket Set Screw - M5x8:5');
#912=NEXT_ASSEMBLY_USAGE_OCCURRENCE(
'Spur Gear - Module 2, 40 Teeth, 20 mm Bore:2',
'Spur Gear - Module 2, 40 Teeth, 20 mm Bore:2',
'Spur Gear - Module 2, 40 Teeth, 20 mm Bore:2',#73713,#73732,
'Spur Gear - Module 2, 40 Teeth, 20 mm Bore:2');
#913=NEXT_ASSEMBLY_USAGE_OCCURRENCE('Key 6x6x20:2','Key 6x6x20:2',
'Key 6x6x20:2',#73713,#73733,'Key 6x6x20:2');
#914=NEXT_ASSEMBLY_USAGE_OCCURRENCE('Compound pinion m2 z20 b20:2',
'Compound pinion m2 z20 b20:2','Compound pinion m2 z20 b20:2',#73713,#73722,
'Compound pinion m2 z20 b20:2');
#915=NEXT_ASSEMBLY_USAGE_OCCURRENCE('Key 6x6x20:3','Key 6x6x20:3',
'Key 6x6x20:3',#73713,#73733,'Key 6x6x20:3');
#916=NEXT_ASSEMBLY_USAGE_OCCURRENCE('Shaft 3:1','Shaft 3:1','Shaft 3:1',
#73723,#73724,'Shaft 3:1');
#917=NEXT_ASSEMBLY_USAGE_OCCURRENCE('mm shaft collar (4):1',
'mm shaft collar (4):1','mm shaft collar (4):1',#73723,#73725,
'mm shaft collar (4):1');
#918=NEXT_ASSEMBLY_USAGE_OCCURRENCE('mm shaft collar (5):1',
'mm shaft collar (5):1','mm shaft collar (5):1',#73723,#73726,
'mm shaft collar (5):1');
#919=NEXT_ASSEMBLY_USAGE_OCCURRENCE('mm outer spacer (4):1',
'mm outer spacer (4):1','mm outer spacer (4):1',#73723,#73727,
'mm outer spacer (4):1');
#920=NEXT_ASSEMBLY_USAGE_OCCURRENCE('mm outer spacer (5):1',
'mm outer spacer (5):1','mm outer spacer (5):1',#73723,#73728,
'mm outer spacer (5):1');
#921=NEXT_ASSEMBLY_USAGE_OCCURRENCE('Spacer d20 L63:1',
'Spacer d20 L63:1','Spacer d20 L63:1',#73723,#73729,'Spacer d20 L63:1');
#922=NEXT_ASSEMBLY_USAGE_OCCURRENCE('Spacer d20 L11 (1):1',
'Spacer d20 L11 (1):1','Spacer d20 L11 (1):1',#73723,#73730,
'Spacer d20 L11 (1):1');
#923=NEXT_ASSEMBLY_USAGE_OCCURRENCE('Socket Set Screw - M5x8:6',
'Socket Set Screw - M5x8:6','Socket Set Screw - M5x8:6',#73723,#73731,
'Socket Set Screw - M5x8:6');
#924=NEXT_ASSEMBLY_USAGE_OCCURRENCE('Socket Set Screw - M5x8:7',
'Socket Set Screw - M5x8:7','Socket Set Screw - M5x8:7',#73723,#73731,
'Socket Set Screw - M5x8:7');
#925=NEXT_ASSEMBLY_USAGE_OCCURRENCE(
'Spur Gear - Module 2, 40 Teeth, 20 mm Bore:3',
'Spur Gear - Module 2, 40 Teeth, 20 mm Bore:3',
'Spur Gear - Module 2, 40 Teeth, 20 mm Bore:3',#73723,#73732,
'Spur Gear - Module 2, 40 Teeth, 20 mm Bore:3');
#926=NEXT_ASSEMBLY_USAGE_OCCURRENCE('Key 6x6x20:4','Key 6x6x20:4',
'Key 6x6x20:4',#73723,#73733,'Key 6x6x20:4');
#927=NEXT_ASSEMBLY_USAGE_OCCURRENCE('Split housing:1','Split housing:1',
'Split housing:1',#73671,#73672,'Split housing:1');
#928=NEXT_ASSEMBLY_USAGE_OCCURRENCE('Input rotor:1','Input rotor:1',
'Input rotor:1',#73671,#73703,'Input rotor:1');
#929=NEXT_ASSEMBLY_USAGE_OCCURRENCE('Compound rotor:1',
'Compound rotor:1','Compound rotor:1',#73671,#73713,'Compound rotor:1');
#930=NEXT_ASSEMBLY_USAGE_OCCURRENCE('Output rotor:1','Output rotor:1',
'Output rotor:1',#73671,#73723,'Output rotor:1');
#931=B_SPLINE_CURVE_WITH_KNOTS('',3,(#24284,#24285,#24286,#24287,#24288,
#24289,#24290,#24291,#24292,#24293,#24294,#24295,#24296,#24297,#24298,#24299,
#24300,#24301,#24302,#24303,#24304,#24305),.UNSPECIFIED.,.F.,.F.,(4,2,2,
2,2,2,2,2,2,2,4),(0.0591825211272536,0.157966726598481,0.236950089897721,
0.315933453196962,0.391576304923761,0.46721915665056,0.54286200837736,0.618504860104159,
0.697488223403399,0.77647158670264,0.875255792173867),.UNSPECIFIED.);
#932=B_SPLINE_CURVE_WITH_KNOTS('',3,(#24309,#24310,#24311,#24312,#24313,
#24314,#24315,#24316,#24317,#24318,#24319,#24320,#24321,#24322,#24323,#24324,
#24325,#24326,#24327,#24328,#24329,#24330),.UNSPECIFIED.,.F.,.F.,(4,2,2,
2,2,2,2,2,2,2,4),(0.0581119756758434,0.106553146291161,0.213106292582322,
0.30849933801665,0.386091982889075,0.4636846277615,0.541277272633925,0.61886991750635,
0.714262962940678,0.820816109231839,0.869257279847157),.UNSPECIFIED.);
#933=B_SPLINE_CURVE_WITH_KNOTS('',3,(#24336,#24337,#24338,#24339,#24340,
#24341,#24342,#24343,#24344,#24345,#24346,#24347,#24348,#24349,#24350,#24351,
#24352,#24353,#24354,#24355,#24356,#24357),.UNSPECIFIED.,.F.,.F.,(4,2,2,
2,2,2,2,2,2,2,4),(0.0581119756758434,0.106553146291161,0.213106292582322,
0.30849933801665,0.386091982889075,0.4636846277615,0.541277272633925,0.61886991750635,
0.714262962940679,0.820816109231839,0.869257279847157),.UNSPECIFIED.);
#934=B_SPLINE_CURVE_WITH_KNOTS('',3,(#24361,#24362,#24363,#24364,#24365,
#24366,#24367,#24368,#24369,#24370,#24371,#24372,#24373,#24374,#24375,#24376,
#24377,#24378,#24379,#24380,#24381,#24382),.UNSPECIFIED.,.F.,.F.,(4,2,2,
2,2,2,2,2,2,2,4),(0.0581119756758433,0.106553146291161,0.213106292582322,
0.308499338016649,0.386091982889075,0.4636846277615,0.541277272633925,0.61886991750635,
0.714262962940678,0.820816109231839,0.869257279847157),.UNSPECIFIED.);
#935=B_SPLINE_CURVE_WITH_KNOTS('',3,(#24391,#24392,#24393,#24394,#24395,
#24396,#24397,#24398,#24399,#24400,#24401,#24402,#24403,#24404,#24405,#24406,
#24407,#24408,#24409,#24410,#24411,#24412),.UNSPECIFIED.,.F.,.F.,(4,2,2,
2,2,2,2,2,2,2,4),(0.0581119756758433,0.106553146291161,0.213106292582322,
0.30849933801665,0.386091982889075,0.4636846277615,0.541277272633925,0.61886991750635,
0.714262962940678,0.820816109231839,0.869257279847157),.UNSPECIFIED.);
#936=B_SPLINE_CURVE_WITH_KNOTS('',3,(#24416,#24417,#24418,#24419,#24420,
#24421,#24422,#24423,#24424,#24425,#24426,#24427,#24428,#24429,#24430,#24431,
#24432,#24433,#24434,#24435,#24436,#24437),.UNSPECIFIED.,.F.,.F.,(4,2,2,
2,2,2,2,2,2,2,4),(0.0581119756758434,0.106553146291161,0.213106292582322,
0.30849933801665,0.386091982889075,0.4636846277615,0.541277272633925,0.61886991750635,
0.714262962940678,0.820816109231839,0.869257279847157),.UNSPECIFIED.);
#937=B_SPLINE_CURVE_WITH_KNOTS('',3,(#24441,#24442,#24443,#24444,#24445,
#24446,#24447,#24448,#24449,#24450,#24451,#24452,#24453,#24454,#24455,#24456,
#24457,#24458,#24459,#24460,#24461,#24462),.UNSPECIFIED.,.F.,.F.,(4,2,2,
2,2,2,2,2,2,2,4),(0.0581119756758434,0.106553146291161,0.213106292582322,
0.30849933801665,0.386091982889075,0.4636846277615,0.541277272633925,0.61886991750635,
0.714262962940678,0.820816109231839,0.869257279847157),.UNSPECIFIED.);
#938=B_SPLINE_CURVE_WITH_KNOTS('',3,(#24466,#24467,#24468,#24469,#24470,
#24471,#24472,#24473,#24474,#24475,#24476,#24477,#24478,#24479,#24480,#24481,
#24482,#24483,#24484,#24485,#24486,#24487),.UNSPECIFIED.,.F.,.F.,(4,2,2,
2,2,2,2,2,2,2,4),(0.0581119756758433,0.106553146291161,0.213106292582322,
0.30849933801665,0.386091982889075,0.4636846277615,0.541277272633925,0.61886991750635,
0.714262962940678,0.820816109231839,0.869257279847157),.UNSPECIFIED.);
#939=B_SPLINE_CURVE_WITH_KNOTS('',3,(#24495,#24496,#24497,#24498,#24499,
#24500,#24501,#24502,#24503,#24504,#24505,#24506,#24507,#24508,#24509,#24510,
#24511,#24512,#24513,#24514,#24515,#24516),.UNSPECIFIED.,.F.,.F.,(4,2,2,
2,2,2,2,2,2,2,4),(0.0591825211272536,0.157966726598481,0.236950089897721,
0.315933453196962,0.391576304923761,0.467219156650561,0.54286200837736,
0.618504860104159,0.697488223403399,0.77647158670264,0.875255792173867),
 .UNSPECIFIED.);
#940=B_SPLINE_CURVE_WITH_KNOTS('',3,(#24524,#24525,#24526,#24527,#24528,
#24529,#24530,#24531,#24532,#24533,#24534,#24535,#24536,#24537,#24538,#24539,
#24540,#24541,#24542,#24543,#24544,#24545),.UNSPECIFIED.,.F.,.F.,(4,2,2,
2,2,2,2,2,2,2,4),(0.0591825211272536,0.157966726598481,0.236950089897722,
0.315933453196962,0.391576304923761,0.467219156650561,0.54286200837736,
0.618504860104159,0.697488223403399,0.77647158670264,0.875255792173867),
 .UNSPECIFIED.);
#941=B_SPLINE_CURVE_WITH_KNOTS('',3,(#24555,#24556,#24557,#24558,#24559,
#24560,#24561,#24562,#24563,#24564,#24565,#24566,#24567,#24568,#24569,#24570,
#24571,#24572,#24573,#24574,#24575,#24576),.UNSPECIFIED.,.F.,.F.,(4,2,2,
2,2,2,2,2,2,2,4),(0.0591825211272536,0.157966726598481,0.236950089897721,
0.315933453196962,0.391576304923761,0.46721915665056,0.54286200837736,0.618504860104159,
0.697488223403399,0.77647158670264,0.875255792173867),.UNSPECIFIED.);
#942=B_SPLINE_CURVE_WITH_KNOTS('',3,(#24584,#24585,#24586,#24587,#24588,
#24589,#24590,#24591,#24592,#24593,#24594,#24595,#24596,#24597,#24598,#24599,
#24600,#24601,#24602,#24603,#24604,#24605),.UNSPECIFIED.,.F.,.F.,(4,2,2,
2,2,2,2,2,2,2,4),(0.0591825211272536,0.157966726598481,0.236950089897721,
0.315933453196962,0.391576304923761,0.46721915665056,0.542862008377359,
0.618504860104159,0.697488223403399,0.776471586702639,0.875255792173867),
 .UNSPECIFIED.);
#943=B_SPLINE_CURVE_WITH_KNOTS('',3,(#24613,#24614,#24615,#24616,#24617,
#24618,#24619,#24620,#24621,#24622,#24623,#24624,#24625,#24626,#24627,#24628,
#24629,#24630,#24631,#24632,#24633,#24634),.UNSPECIFIED.,.F.,.F.,(4,2,2,
2,2,2,2,2,2,2,4),(0.0591825211272536,0.157966726598481,0.236950089897721,
0.315933453196962,0.391576304923761,0.46721915665056,0.54286200837736,0.618504860104159,
0.697488223403399,0.77647158670264,0.875255792173867),.UNSPECIFIED.);
#944=B_SPLINE_CURVE_WITH_KNOTS('',3,(#24643,#24644,#24645,#24646,#24647,
#24648,#24649,#24650,#24651,#24652,#24653,#24654,#24655,#24656,#24657,#24658,
#24659,#24660,#24661,#24662,#24663,#24664),.UNSPECIFIED.,.F.,.F.,(4,2,2,
2,2,2,2,2,2,2,4),(0.0591825211272536,0.157966726598481,0.236950089897721,
0.315933453196962,0.391576304923761,0.46721915665056,0.542862008377359,
0.618504860104159,0.697488223403399,0.776471586702639,0.875255792173867),
 .UNSPECIFIED.);
#945=B_SPLINE_CURVE_WITH_KNOTS('',3,(#24814,#24815,#24816,#24817,#24818,
#24819,#24820,#24821,#24822,#24823,#24824,#24825,#24826,#24827,#24828,#24829,
#24830,#24831,#24832,#24833,#24834,#24835),.UNSPECIFIED.,.F.,.F.,(4,2,2,
2,2,2,2,2,2,2,4),(0.0789094028588958,0.210573405340968,0.315860108011452,
0.421146810681936,0.522142632548711,0.623138454415485,0.72413427628226,
0.825130098149035,0.930416800819519,1.03570350349,1.16736750597208),
 .UNSPECIFIED.);
#946=B_SPLINE_CURVE_WITH_KNOTS('',3,(#24839,#24840,#24841,#24842,#24843,
#24844,#24845,#24846,#24847,#24848,#24849,#24850,#24851,#24852,#24853,#24854,
#24855,#24856,#24857,#24858,#24859,#24860),.UNSPECIFIED.,.F.,.F.,(4,2,2,
2,2,2,2,2,2,2,4),(0.0774793363974613,0.142088896491891,0.284177792983782,
0.411119756996526,0.514392970548519,0.617666184100513,0.720939397652506,
0.8242126112045,0.951154575217244,1.09324347170913,1.15785303180356),
 .UNSPECIFIED.);
#947=B_SPLINE_CURVE_WITH_KNOTS('',3,(#24866,#24867,#24868,#24869,#24870,
#24871,#24872,#24873,#24874,#24875,#24876,#24877,#24878,#24879,#24880,#24881,
#24882,#24883,#24884,#24885,#24886,#24887),.UNSPECIFIED.,.F.,.F.,(4,2,2,
2,2,2,2,2,2,2,4),(0.0774793363974613,0.142088896491891,0.284177792983782,
0.411119756996525,0.514392970548519,0.617666184100513,0.720939397652506,
0.8242126112045,0.951154575217243,1.09324347170913,1.15785303180356),
 .UNSPECIFIED.);
#948=B_SPLINE_CURVE_WITH_KNOTS('',3,(#24891,#24892,#24893,#24894,#24895,
#24896,#24897,#24898,#24899,#24900,#24901,#24902,#24903,#24904,#24905,#24906,
#24907,#24908,#24909,#24910,#24911,#24912),.UNSPECIFIED.,.F.,.F.,(4,2,2,
2,2,2,2,2,2,2,4),(0.0774793363974614,0.142088896491891,0.284177792983781,
0.411119756996525,0.514392970548519,0.617666184100512,0.720939397652506,
0.824212611204499,0.951154575217243,1.09324347170913,1.15785303180356),
 .UNSPECIFIED.);
#949=B_SPLINE_CURVE_WITH_KNOTS('',3,(#24916,#24917,#24918,#24919,#24920,
#24921,#24922,#24923,#24924,#24925,#24926,#24927),.UNSPECIFIED.,.F.,.F.,
(4,2,2,2,2,4),(0.0774793363974613,0.142088896491891,0.284177792983781,0.411119756996525,
0.514392970548519,0.617666184100512),.UNSPECIFIED.);
#950=B_SPLINE_CURVE_WITH_KNOTS('',3,(#24932,#24933,#24934,#24935,#24936,
#24937,#24938,#24939,#24940,#24941,#24942,#24943),.UNSPECIFIED.,.F.,.F.,
(4,2,2,2,2,4),(0.617666184100512,0.720939397652506,0.824212611204499,0.951154575217243,
1.09324347170913,1.15785303180356),.UNSPECIFIED.);
#951=B_SPLINE_CURVE_WITH_KNOTS('',3,(#24947,#24948,#24949,#24950,#24951,
#24952,#24953,#24954,#24955,#24956,#24957,#24958,#24959,#24960,#24961,#24962,
#24963,#24964,#24965,#24966,#24967,#24968),.UNSPECIFIED.,.F.,.F.,(4,2,2,
2,2,2,2,2,2,2,4),(0.0774793363974613,0.142088896491891,0.284177792983782,
0.411119756996526,0.514392970548519,0.617666184100513,0.720939397652507,
0.8242126112045,0.951154575217245,1.09324347170914,1.15785303180356),
 .UNSPECIFIED.);
#952=B_SPLINE_CURVE_WITH_KNOTS('',3,(#24972,#24973,#24974,#24975,#24976,
#24977,#24978,#24979,#24980,#24981,#24982,#24983,#24984,#24985,#24986,#24987,
#24988,#24989,#24990,#24991,#24992,#24993),.UNSPECIFIED.,.F.,.F.,(4,2,2,
2,2,2,2,2,2,2,4),(0.0774793363974613,0.142088896491891,0.284177792983782,
0.411119756996526,0.514392970548519,0.617666184100513,0.720939397652506,
0.824212611204499,0.951154575217243,1.09324347170913,1.15785303180356),
 .UNSPECIFIED.);
#953=B_SPLINE_CURVE_WITH_KNOTS('',3,(#24997,#24998,#24999,#25000,#25001,
#25002,#25003,#25004,#25005,#25006,#25007,#25008,#25009,#25010,#25011,#25012,
#25013,#25014,#25015,#25016,#25017,#25018),.UNSPECIFIED.,.F.,.F.,(4,2,2,
2,2,2,2,2,2,2,4),(0.0774793363974613,0.142088896491891,0.284177792983782,
0.411119756996526,0.514392970548519,0.617666184100513,0.720939397652506,
0.8242126112045,0.951154575217244,1.09324347170913,1.15785303180356),
 .UNSPECIFIED.);
#954=B_SPLINE_CURVE_WITH_KNOTS('',3,(#25022,#25023,#25024,#25025,#25026,
#25027,#25028,#25029,#25030,#25031,#25032,#25033,#25034,#25035,#25036,#25037,
#25038,#25039,#25040,#25041,#25042,#25043),.UNSPECIFIED.,.F.,.F.,(4,2,2,
2,2,2,2,2,2,2,4),(0.0774793363974613,0.142088896491891,0.284177792983782,
0.411119756996526,0.514392970548519,0.617666184100513,0.720939397652506,
0.8242126112045,0.951154575217243,1.09324347170913,1.15785303180356),
 .UNSPECIFIED.);
#955=B_SPLINE_CURVE_WITH_KNOTS('',3,(#25051,#25052,#25053,#25054,#25055,
#25056,#25057,#25058,#25059,#25060,#25061,#25062,#25063,#25064,#25065,#25066,
#25067,#25068,#25069,#25070,#25071,#25072),.UNSPECIFIED.,.F.,.F.,(4,2,2,
2,2,2,2,2,2,2,4),(0.0789094028588958,0.210573405340968,0.315860108011452,
0.421146810681936,0.522142632548711,0.623138454415485,0.72413427628226,
0.825130098149035,0.930416800819519,1.03570350349,1.16736750597208),
 .UNSPECIFIED.);
#956=B_SPLINE_CURVE_WITH_KNOTS('',3,(#25080,#25081,#25082,#25083,#25084,
#25085,#25086,#25087,#25088,#25089,#25090,#25091,#25092,#25093,#25094,#25095,
#25096,#25097,#25098,#25099,#25100,#25101),.UNSPECIFIED.,.F.,.F.,(4,2,2,
2,2,2,2,2,2,2,4),(0.0789094028588958,0.210573405340969,0.315860108011453,
0.421146810681937,0.522142632548712,0.623138454415486,0.724134276282261,
0.825130098149035,0.930416800819519,1.03570350349,1.16736750597208),
 .UNSPECIFIED.);
#957=B_SPLINE_CURVE_WITH_KNOTS('',3,(#25110,#25111,#25112,#25113,#25114,
#25115,#25116,#25117,#25118,#25119,#25120,#25121),.UNSPECIFIED.,.F.,.F.,
(4,2,2,2,2,4),(0.0789094028588958,0.210573405340968,0.315860108011452,0.421146810681937,
0.522142632548711,0.623138454415486),.UNSPECIFIED.);
#958=B_SPLINE_CURVE_WITH_KNOTS('',3,(#25123,#25124,#25125,#25126,#25127,
#25128,#25129,#25130,#25131,#25132,#25133,#25134),.UNSPECIFIED.,.F.,.F.,
(4,2,2,2,2,4),(0.623138454415486,0.72413427628226,0.825130098149035,0.930416800819519,
1.03570350349,1.16736750597208),.UNSPECIFIED.);
#959=B_SPLINE_CURVE_WITH_KNOTS('',3,(#25141,#25142,#25143,#25144,#25145,
#25146,#25147,#25148,#25149,#25150,#25151,#25152,#25153,#25154,#25155,#25156,
#25157,#25158,#25159,#25160,#25161,#25162),.UNSPECIFIED.,.F.,.F.,(4,2,2,
2,2,2,2,2,2,2,4),(0.0789094028588958,0.210573405340968,0.315860108011452,
0.421146810681936,0.522142632548711,0.623138454415486,0.72413427628226,
0.825130098149035,0.930416800819519,1.03570350349,1.16736750597208),
 .UNSPECIFIED.);
#960=B_SPLINE_CURVE_WITH_KNOTS('',3,(#25170,#25171,#25172,#25173,#25174,
#25175,#25176,#25177,#25178,#25179,#25180,#25181,#25182,#25183,#25184,#25185,
#25186,#25187,#25188,#25189,#25190,#25191),.UNSPECIFIED.,.F.,.F.,(4,2,2,
2,2,2,2,2,2,2,4),(0.0789094028588957,0.210573405340968,0.315860108011452,
0.421146810681936,0.522142632548711,0.623138454415485,0.72413427628226,
0.825130098149035,0.930416800819519,1.03570350349,1.16736750597207),
 .UNSPECIFIED.);
#961=B_SPLINE_CURVE_WITH_KNOTS('',3,(#25199,#25200,#25201,#25202,#25203,
#25204,#25205,#25206,#25207,#25208,#25209,#25210,#25211,#25212,#25213,#25214,
#25215,#25216,#25217,#25218,#25219,#25220),.UNSPECIFIED.,.F.,.F.,(4,2,2,
2,2,2,2,2,2,2,4),(0.0789094028588958,0.210573405340968,0.315860108011452,
0.421146810681936,0.522142632548711,0.623138454415486,0.72413427628226,
0.825130098149035,0.930416800819519,1.03570350349,1.16736750597208),
 .UNSPECIFIED.);
#962=B_SPLINE_CURVE_WITH_KNOTS('',3,(#25229,#25230,#25231,#25232,#25233,
#25234,#25235,#25236,#25237,#25238,#25239,#25240,#25241,#25242,#25243,#25244,
#25245,#25246,#25247,#25248,#25249,#25250),.UNSPECIFIED.,.F.,.F.,(4,2,2,
2,2,2,2,2,2,2,4),(0.0789094028588958,0.210573405340968,0.315860108011452,
0.421146810681936,0.522142632548711,0.623138454415485,0.72413427628226,
0.825130098149035,0.930416800819519,1.03570350349,1.16736750597208),
 .UNSPECIFIED.);
#963=B_SPLINE_CURVE_WITH_KNOTS('',3,(#25465,#25466,#25467,#25468,#25469,
#25470,#25471,#25472,#25473,#25474),.UNSPECIFIED.,.F.,.F.,(4,2,2,2,4),(0.818088904349178,
0.878131747417165,0.957937926194036,1.03774410497091,1.09778694803889),
 .UNSPECIFIED.);
#964=B_SPLINE_CURVE_WITH_KNOTS('',3,(#25480,#25481,#25482,#25483,#25484,
#25485,#25486,#25487,#25488,#25489,#25490,#25491,#25492,#25493,#25494,#25495,
#25496,#25497),.UNSPECIFIED.,.F.,.F.,(4,2,2,2,2,2,2,2,4),(0.,0.0793616477694788,
0.158723295538958,0.238079516586307,0.317435737633657,0.396791958681006,
0.476148179728356,0.555509827497835,0.634871475267313),.UNSPECIFIED.);
#965=B_SPLINE_CURVE_WITH_KNOTS('',3,(#25498,#25499,#25500,#25501,#25502,
#25503,#25504,#25505,#25506,#25507,#25508,#25509,#25510,#25511,#25512,#25513,
#25514,#25515),.UNSPECIFIED.,.F.,.F.,(4,2,2,2,2,2,2,2,4),(0.634871475267313,
0.714233123036792,0.793594770806271,0.87295099185362,0.95230721290097,1.03166343394832,
1.11101965499567,1.19038130276515,1.26974295053463),.UNSPECIFIED.);
#966=B_SPLINE_CURVE_WITH_KNOTS('',3,(#25518,#25519,#25520,#25521,#25522,
#25523,#25524,#25525,#25526,#25527),.UNSPECIFIED.,.F.,.F.,(4,2,2,2,4),(0.17946362021982,
0.239506463287808,0.319312642064679,0.39911882084155,0.459161663909537),
 .UNSPECIFIED.);
#967=B_SPLINE_CURVE_WITH_KNOTS('',3,(#25552,#25553,#25554,#25555,#25556,
#25557,#25558,#25559,#25560,#25561),.UNSPECIFIED.,.F.,.F.,(4,2,2,2,4),(0.818088904349178,
0.878131747417166,0.957937926194037,1.03774410497091,1.0977869480389),
 .UNSPECIFIED.);
#968=B_SPLINE_CURVE_WITH_KNOTS('',3,(#25567,#25568,#25569,#25570,#25571,
#25572,#25573,#25574,#25575,#25576,#25577,#25578,#25579,#25580,#25581,#25582,
#25583,#25584),.UNSPECIFIED.,.F.,.F.,(4,2,2,2,2,2,2,2,4),(0.,0.0793616477694788,
0.158723295538958,0.238079516586307,0.317435737633657,0.396791958681006,
0.476148179728355,0.555509827497834,0.634871475267313),.UNSPECIFIED.);
#969=B_SPLINE_CURVE_WITH_KNOTS('',3,(#25585,#25586,#25587,#25588,#25589,
#25590,#25591,#25592,#25593,#25594,#25595,#25596,#25597,#25598,#25599,#25600,
#25601,#25602),.UNSPECIFIED.,.F.,.F.,(4,2,2,2,2,2,2,2,4),(0.634871475267313,
0.714233123036792,0.79359477080627,0.87295099185362,0.95230721290097,1.03166343394832,
1.11101965499567,1.19038130276515,1.26974295053463),.UNSPECIFIED.);
#970=B_SPLINE_CURVE_WITH_KNOTS('',3,(#25605,#25606,#25607,#25608,#25609,
#25610,#25611,#25612,#25613,#25614),.UNSPECIFIED.,.F.,.F.,(4,2,2,2,4),(0.179463620219821,
0.239506463287808,0.319312642064679,0.39911882084155,0.459161663909537),
 .UNSPECIFIED.);
#971=B_SPLINE_CURVE_WITH_KNOTS('',3,(#37404,#37405,#37406,#37407,#37408,
#37409,#37410,#37411,#37412,#37413,#37414,#37415,#37416,#37417),
 .UNSPECIFIED.,.F.,.F.,(4,2,2,2,2,2,4),(0.756005737987032,0.793568827564648,
0.872922520054202,0.952276212543757,1.03162990503331,1.11098359752287,1.14854668710048),
 .UNSPECIFIED.);
#972=B_SPLINE_CURVE_WITH_KNOTS('',3,(#37423,#37424,#37425,#37426,#37427,
#37428,#37429,#37430,#37431,#37432,#37433,#37434,#37435,#37436,#37437,#37438,
#37439,#37440),.UNSPECIFIED.,.F.,.F.,(4,2,2,2,2,2,2,2,4),(0.,0.0792334805614376,
0.158466961122875,0.237699060165218,0.31693115920756,0.396163258249903,
0.475395357292245,0.554628837853683,0.633862318415121),.UNSPECIFIED.);
#973=B_SPLINE_CURVE_WITH_KNOTS('',3,(#37441,#37442,#37443,#37444,#37445,
#37446,#37447,#37448,#37449,#37450,#37451,#37452,#37453,#37454,#37455,#37456,
#37457,#37458),.UNSPECIFIED.,.F.,.F.,(4,2,2,2,2,2,2,2,4),(0.633862318415121,
0.713095798976558,0.792329279537995,0.871561378580338,0.950793477622681,
1.03002557666502,1.10925767570737,1.1884911562688,1.26772463683024),
 .UNSPECIFIED.);
#974=B_SPLINE_CURVE_WITH_KNOTS('',3,(#37461,#37462,#37463,#37464,#37465,
#37466,#37467,#37468,#37469,#37470,#37471,#37472,#37473,#37474),
 .UNSPECIFIED.,.F.,.F.,(4,2,2,2,2,2,4),(0.121154929624526,0.158718019202143,
0.238071711691697,0.317425404181252,0.396779096670807,0.476132789160362,
0.51369587873798),.UNSPECIFIED.);
#975=B_SPLINE_CURVE_WITH_KNOTS('',3,(#37499,#37500,#37501,#37502,#37503,
#37504,#37505,#37506,#37507,#37508,#37509,#37510,#37511,#37512),
 .UNSPECIFIED.,.F.,.F.,(4,2,2,2,2,2,4),(0.75600573798703,0.793568827564647,
0.872922520054202,0.952276212543757,1.03162990503331,1.11098359752287,1.14854668710048),
 .UNSPECIFIED.);
#976=B_SPLINE_CURVE_WITH_KNOTS('',3,(#37518,#37519,#37520,#37521,#37522,
#37523,#37524,#37525,#37526,#37527,#37528,#37529,#37530,#37531,#37532,#37533,
#37534,#37535),.UNSPECIFIED.,.F.,.F.,(4,2,2,2,2,2,2,2,4),(0.,0.0792334805614374,
0.158466961122875,0.237699060165218,0.31693115920756,0.396163258249903,
0.475395357292246,0.554628837853684,0.633862318415121),.UNSPECIFIED.);
#977=B_SPLINE_CURVE_WITH_KNOTS('',3,(#37536,#37537,#37538,#37539,#37540,
#37541,#37542,#37543,#37544,#37545,#37546,#37547,#37548,#37549,#37550,#37551,
#37552,#37553),.UNSPECIFIED.,.F.,.F.,(4,2,2,2,2,2,2,2,4),(0.633862318415121,
0.713095798976559,0.792329279537996,0.871561378580339,0.950793477622681,
1.03002557666502,1.10925767570737,1.1884911562688,1.26772463683024),
 .UNSPECIFIED.);
#978=B_SPLINE_CURVE_WITH_KNOTS('',3,(#37556,#37557,#37558,#37559,#37560,
#37561,#37562,#37563,#37564,#37565,#37566,#37567,#37568,#37569),
 .UNSPECIFIED.,.F.,.F.,(4,2,2,2,2,2,4),(0.121154929624528,0.158718019202143,
0.238071711691698,0.317425404181252,0.396779096670807,0.476132789160361,
0.513695878737976),.UNSPECIFIED.);
#979=B_SPLINE_CURVE_WITH_KNOTS('',3,(#49298,#49299,#49300,#49301,#49302,
#49303,#49304,#49305,#49306,#49307,#49308,#49309,#49310,#49311),
 .UNSPECIFIED.,.F.,.F.,(4,2,2,2,2,2,4),(0.756005737987022,0.79356882756465,
0.872922520054205,0.95227621254376,1.03162990503331,1.11098359752287,1.14854668710049),
 .UNSPECIFIED.);
#980=B_SPLINE_CURVE_WITH_KNOTS('',3,(#49317,#49318,#49319,#49320,#49321,
#49322,#49323,#49324,#49325,#49326,#49327,#49328,#49329,#49330,#49331,#49332,
#49333,#49334),.UNSPECIFIED.,.F.,.F.,(4,2,2,2,2,2,2,2,4),(0.,0.0792334805614376,
0.158466961122875,0.237699060165218,0.316931159207561,0.396163258249904,
0.475395357292247,0.554628837853685,0.633862318415122),.UNSPECIFIED.);
#981=B_SPLINE_CURVE_WITH_KNOTS('',3,(#49335,#49336,#49337,#49338,#49339,
#49340,#49341,#49342,#49343,#49344,#49345,#49346,#49347,#49348,#49349,#49350,
#49351,#49352),.UNSPECIFIED.,.F.,.F.,(4,2,2,2,2,2,2,2,4),(0.633862318415122,
0.71309579897656,0.792329279537998,0.871561378580341,0.950793477622684,
1.03002557666503,1.10925767570737,1.18849115626881,1.26772463683024),
 .UNSPECIFIED.);
#982=B_SPLINE_CURVE_WITH_KNOTS('',3,(#49355,#49356,#49357,#49358,#49359,
#49360,#49361,#49362,#49363,#49364,#49365,#49366,#49367,#49368),
 .UNSPECIFIED.,.F.,.F.,(4,2,2,2,2,2,4),(0.121154929624522,0.158718019202143,
0.238071711691698,0.317425404181253,0.396779096670808,0.476132789160363,
0.513695878737986),.UNSPECIFIED.);
#983=B_SPLINE_CURVE_WITH_KNOTS('',3,(#49393,#49394,#49395,#49396,#49397,
#49398,#49399,#49400,#49401,#49402,#49403,#49404,#49405,#49406),
 .UNSPECIFIED.,.F.,.F.,(4,2,2,2,2,2,4),(0.756005737987027,0.79356882756465,
0.872922520054205,0.95227621254376,1.03162990503331,1.11098359752287,1.14854668710049),
 .UNSPECIFIED.);
#984=B_SPLINE_CURVE_WITH_KNOTS('',3,(#49412,#49413,#49414,#49415,#49416,
#49417,#49418,#49419,#49420,#49421,#49422,#49423,#49424,#49425,#49426,#49427,
#49428,#49429),.UNSPECIFIED.,.F.,.F.,(4,2,2,2,2,2,2,2,4),(0.,0.0792334805614376,
0.158466961122875,0.237699060165218,0.316931159207561,0.396163258249904,
0.475395357292247,0.554628837853685,0.633862318415122),.UNSPECIFIED.);
#985=B_SPLINE_CURVE_WITH_KNOTS('',3,(#49430,#49431,#49432,#49433,#49434,
#49435,#49436,#49437,#49438,#49439,#49440,#49441,#49442,#49443,#49444,#49445,
#49446,#49447),.UNSPECIFIED.,.F.,.F.,(4,2,2,2,2,2,2,2,4),(0.633862318415122,
0.71309579897656,0.792329279537998,0.871561378580341,0.950793477622684,
1.03002557666503,1.10925767570737,1.18849115626881,1.26772463683024),
 .UNSPECIFIED.);
#986=B_SPLINE_CURVE_WITH_KNOTS('',3,(#49450,#49451,#49452,#49453,#49454,
#49455,#49456,#49457,#49458,#49459,#49460,#49461,#49462,#49463),
 .UNSPECIFIED.,.F.,.F.,(4,2,2,2,2,2,4),(0.121154929624521,0.158718019202143,
0.238071711691698,0.317425404181253,0.396779096670808,0.476132789160363,
0.513695878737991),.UNSPECIFIED.);
#987=B_SPLINE_CURVE_WITH_KNOTS('',3,(#55619,#55620,#55621,#55622,#55623,
#55624),.UNSPECIFIED.,.F.,.F.,(4,2,4),(0.,1.,2.),.UNSPECIFIED.);
#988=B_SPLINE_CURVE_WITH_KNOTS('',3,(#55838,#55839,#55840,#55841,#55842,
#55843),.UNSPECIFIED.,.F.,.F.,(4,2,4),(0.,1.,2.),.UNSPECIFIED.);
#989=B_SPLINE_CURVE_WITH_KNOTS('',3,(#55921,#55922,#55923,#55924,#55925,
#55926),.UNSPECIFIED.,.F.,.F.,(4,2,4),(0.,1.,2.),.UNSPECIFIED.);
#990=B_SPLINE_CURVE_WITH_KNOTS('',3,(#56280,#56281,#56282,#56283,#56284,
#56285),.UNSPECIFIED.,.F.,.F.,(4,2,4),(0.,1.,2.),.UNSPECIFIED.);
#991=B_SPLINE_CURVE_WITH_KNOTS('',3,(#56363,#56364,#56365,#56366,#56367,
#56368),.UNSPECIFIED.,.F.,.F.,(4,2,4),(0.,1.,2.),.UNSPECIFIED.);
#992=B_SPLINE_CURVE_WITH_KNOTS('',3,(#56722,#56723,#56724,#56725,#56726,
#56727),.UNSPECIFIED.,.F.,.F.,(4,2,4),(0.,1.,2.),.UNSPECIFIED.);
#993=B_SPLINE_CURVE_WITH_KNOTS('',3,(#56805,#56806,#56807,#56808,#56809,
#56810),.UNSPECIFIED.,.F.,.F.,(4,2,4),(0.,1.,2.),.UNSPECIFIED.);
#994=B_SPLINE_CURVE_WITH_KNOTS('',3,(#57164,#57165,#57166,#57167,#57168,
#57169),.UNSPECIFIED.,.F.,.F.,(4,2,4),(0.,1.,2.),.UNSPECIFIED.);
#995=B_SPLINE_CURVE_WITH_KNOTS('',3,(#57247,#57248,#57249,#57250,#57251,
#57252),.UNSPECIFIED.,.F.,.F.,(4,2,4),(0.,1.,2.),.UNSPECIFIED.);
#996=B_SPLINE_CURVE_WITH_KNOTS('',3,(#57606,#57607,#57608,#57609,#57610,
#57611),.UNSPECIFIED.,.F.,.F.,(4,2,4),(0.,1.,2.),.UNSPECIFIED.);
#997=B_SPLINE_CURVE_WITH_KNOTS('',3,(#57689,#57690,#57691,#57692,#57693,
#57694),.UNSPECIFIED.,.F.,.F.,(4,2,4),(0.,1.,2.),.UNSPECIFIED.);
#998=B_SPLINE_CURVE_WITH_KNOTS('',3,(#58048,#58049,#58050,#58051,#58052,
#58053),.UNSPECIFIED.,.F.,.F.,(4,2,4),(0.,1.,2.),.UNSPECIFIED.);
#999=B_SPLINE_CURVE_WITH_KNOTS('',3,(#58131,#58132,#58133,#58134,#58135,
#58136),.UNSPECIFIED.,.F.,.F.,(4,2,4),(0.,1.,2.),.UNSPECIFIED.);
#1000=B_SPLINE_CURVE_WITH_KNOTS('',3,(#58490,#58491,#58492,#58493,#58494,
#58495),.UNSPECIFIED.,.F.,.F.,(4,2,4),(0.,1.,2.),.UNSPECIFIED.);
#1001=B_SPLINE_CURVE_WITH_KNOTS('',3,(#58573,#58574,#58575,#58576,#58577,
#58578),.UNSPECIFIED.,.F.,.F.,(4,2,4),(0.,1.,2.),.UNSPECIFIED.);
#1002=B_SPLINE_CURVE_WITH_KNOTS('',3,(#58932,#58933,#58934,#58935,#58936,
#58937),.UNSPECIFIED.,.F.,.F.,(4,2,4),(0.,1.,2.),.UNSPECIFIED.);
#1003=B_SPLINE_CURVE_WITH_KNOTS('',3,(#59015,#59016,#59017,#59018,#59019,
#59020),.UNSPECIFIED.,.F.,.F.,(4,2,4),(0.,1.,2.),.UNSPECIFIED.);
#1004=B_SPLINE_CURVE_WITH_KNOTS('',3,(#59374,#59375,#59376,#59377,#59378,
#59379),.UNSPECIFIED.,.F.,.F.,(4,2,4),(0.,1.,2.),.UNSPECIFIED.);
#1005=B_SPLINE_CURVE_WITH_KNOTS('',3,(#59457,#59458,#59459,#59460,#59461,
#59462),.UNSPECIFIED.,.F.,.F.,(4,2,4),(0.,1.,2.),.UNSPECIFIED.);
#1006=B_SPLINE_CURVE_WITH_KNOTS('',3,(#59816,#59817,#59818,#59819,#59820,
#59821),.UNSPECIFIED.,.F.,.F.,(4,2,4),(0.,1.,2.),.UNSPECIFIED.);
#1007=B_SPLINE_CURVE_WITH_KNOTS('',3,(#59899,#59900,#59901,#59902,#59903,
#59904),.UNSPECIFIED.,.F.,.F.,(4,2,4),(0.,1.,2.),.UNSPECIFIED.);
#1008=B_SPLINE_CURVE_WITH_KNOTS('',3,(#60258,#60259,#60260,#60261,#60262,
#60263),.UNSPECIFIED.,.F.,.F.,(4,2,4),(0.,1.,2.),.UNSPECIFIED.);
#1009=B_SPLINE_CURVE_WITH_KNOTS('',3,(#60341,#60342,#60343,#60344,#60345,
#60346),.UNSPECIFIED.,.F.,.F.,(4,2,4),(0.,1.,2.),.UNSPECIFIED.);
#1010=B_SPLINE_CURVE_WITH_KNOTS('',3,(#60700,#60701,#60702,#60703,#60704,
#60705),.UNSPECIFIED.,.F.,.F.,(4,2,4),(0.,1.,2.),.UNSPECIFIED.);
#1011=B_SPLINE_CURVE_WITH_KNOTS('',3,(#60783,#60784,#60785,#60786,#60787,
#60788),.UNSPECIFIED.,.F.,.F.,(4,2,4),(0.,1.,2.),.UNSPECIFIED.);
#1012=B_SPLINE_CURVE_WITH_KNOTS('',3,(#61142,#61143,#61144,#61145,#61146,
#61147),.UNSPECIFIED.,.F.,.F.,(4,2,4),(0.,1.,2.),.UNSPECIFIED.);
#1013=B_SPLINE_CURVE_WITH_KNOTS('',3,(#61225,#61226,#61227,#61228,#61229,
#61230),.UNSPECIFIED.,.F.,.F.,(4,2,4),(0.,1.,2.),.UNSPECIFIED.);
#1014=B_SPLINE_CURVE_WITH_KNOTS('',3,(#61584,#61585,#61586,#61587,#61588,
#61589),.UNSPECIFIED.,.F.,.F.,(4,2,4),(0.,1.,2.),.UNSPECIFIED.);
#1015=B_SPLINE_CURVE_WITH_KNOTS('',3,(#61667,#61668,#61669,#61670,#61671,
#61672),.UNSPECIFIED.,.F.,.F.,(4,2,4),(0.,1.,2.),.UNSPECIFIED.);
#1016=B_SPLINE_CURVE_WITH_KNOTS('',3,(#62026,#62027,#62028,#62029,#62030,
#62031),.UNSPECIFIED.,.F.,.F.,(4,2,4),(0.,1.,2.),.UNSPECIFIED.);
#1017=B_SPLINE_CURVE_WITH_KNOTS('',3,(#62109,#62110,#62111,#62112,#62113,
#62114),.UNSPECIFIED.,.F.,.F.,(4,2,4),(0.,1.,2.),.UNSPECIFIED.);
#1018=B_SPLINE_CURVE_WITH_KNOTS('',3,(#62468,#62469,#62470,#62471,#62472,
#62473),.UNSPECIFIED.,.F.,.F.,(4,2,4),(0.,1.,2.),.UNSPECIFIED.);
#1019=B_SPLINE_CURVE_WITH_KNOTS('',3,(#62551,#62552,#62553,#62554,#62555,
#62556),.UNSPECIFIED.,.F.,.F.,(4,2,4),(0.,1.,2.),.UNSPECIFIED.);
#1020=B_SPLINE_CURVE_WITH_KNOTS('',3,(#62910,#62911,#62912,#62913,#62914,
#62915),.UNSPECIFIED.,.F.,.F.,(4,2,4),(0.,1.,2.),.UNSPECIFIED.);
#1021=B_SPLINE_CURVE_WITH_KNOTS('',3,(#62993,#62994,#62995,#62996,#62997,
#62998),.UNSPECIFIED.,.F.,.F.,(4,2,4),(0.,1.,2.),.UNSPECIFIED.);
#1022=B_SPLINE_CURVE_WITH_KNOTS('',3,(#63352,#63353,#63354,#63355,#63356,
#63357),.UNSPECIFIED.,.F.,.F.,(4,2,4),(0.,1.,2.),.UNSPECIFIED.);
#1023=B_SPLINE_CURVE_WITH_KNOTS('',3,(#63435,#63436,#63437,#63438,#63439,
#63440),.UNSPECIFIED.,.F.,.F.,(4,2,4),(0.,1.,2.),.UNSPECIFIED.);
#1024=B_SPLINE_CURVE_WITH_KNOTS('',3,(#63794,#63795,#63796,#63797,#63798,
#63799),.UNSPECIFIED.,.F.,.F.,(4,2,4),(0.,1.,2.),.UNSPECIFIED.);
#1025=B_SPLINE_CURVE_WITH_KNOTS('',3,(#63877,#63878,#63879,#63880,#63881,
#63882),.UNSPECIFIED.,.F.,.F.,(4,2,4),(0.,1.,2.),.UNSPECIFIED.);
#1026=B_SPLINE_CURVE_WITH_KNOTS('',3,(#64236,#64237,#64238,#64239,#64240,
#64241),.UNSPECIFIED.,.F.,.F.,(4,2,4),(0.,1.,2.),.UNSPECIFIED.);
#1027=B_SPLINE_CURVE_WITH_KNOTS('',3,(#64319,#64320,#64321,#64322,#64323,
#64324),.UNSPECIFIED.,.F.,.F.,(4,2,4),(0.,1.,2.),.UNSPECIFIED.);
#1028=B_SPLINE_CURVE_WITH_KNOTS('',3,(#64678,#64679,#64680,#64681,#64682,
#64683),.UNSPECIFIED.,.F.,.F.,(4,2,4),(0.,1.,2.),.UNSPECIFIED.);
#1029=B_SPLINE_CURVE_WITH_KNOTS('',3,(#64761,#64762,#64763,#64764,#64765,
#64766),.UNSPECIFIED.,.F.,.F.,(4,2,4),(0.,1.,2.),.UNSPECIFIED.);
#1030=B_SPLINE_CURVE_WITH_KNOTS('',3,(#65120,#65121,#65122,#65123,#65124,
#65125),.UNSPECIFIED.,.F.,.F.,(4,2,4),(0.,1.,2.),.UNSPECIFIED.);
#1031=B_SPLINE_CURVE_WITH_KNOTS('',3,(#65203,#65204,#65205,#65206,#65207,
#65208),.UNSPECIFIED.,.F.,.F.,(4,2,4),(0.,1.,2.),.UNSPECIFIED.);
#1032=B_SPLINE_CURVE_WITH_KNOTS('',3,(#65562,#65563,#65564,#65565,#65566,
#65567),.UNSPECIFIED.,.F.,.F.,(4,2,4),(0.,1.,2.),.UNSPECIFIED.);
#1033=B_SPLINE_CURVE_WITH_KNOTS('',3,(#65645,#65646,#65647,#65648,#65649,
#65650),.UNSPECIFIED.,.F.,.F.,(4,2,4),(0.,1.,2.),.UNSPECIFIED.);
#1034=B_SPLINE_CURVE_WITH_KNOTS('',3,(#66004,#66005,#66006,#66007,#66008,
#66009),.UNSPECIFIED.,.F.,.F.,(4,2,4),(0.,1.,2.),.UNSPECIFIED.);
#1035=B_SPLINE_CURVE_WITH_KNOTS('',3,(#66087,#66088,#66089,#66090,#66091,
#66092),.UNSPECIFIED.,.F.,.F.,(4,2,4),(0.,1.,2.),.UNSPECIFIED.);
#1036=B_SPLINE_CURVE_WITH_KNOTS('',3,(#66446,#66447,#66448,#66449,#66450,
#66451),.UNSPECIFIED.,.F.,.F.,(4,2,4),(0.,1.,2.),.UNSPECIFIED.);
#1037=B_SPLINE_CURVE_WITH_KNOTS('',3,(#66529,#66530,#66531,#66532,#66533,
#66534),.UNSPECIFIED.,.F.,.F.,(4,2,4),(0.,1.,2.),.UNSPECIFIED.);
#1038=B_SPLINE_CURVE_WITH_KNOTS('',3,(#66888,#66889,#66890,#66891,#66892,
#66893),.UNSPECIFIED.,.F.,.F.,(4,2,4),(0.,1.,2.),.UNSPECIFIED.);
#1039=B_SPLINE_CURVE_WITH_KNOTS('',3,(#66971,#66972,#66973,#66974,#66975,
#66976),.UNSPECIFIED.,.F.,.F.,(4,2,4),(0.,1.,2.),.UNSPECIFIED.);
#1040=B_SPLINE_CURVE_WITH_KNOTS('',3,(#67330,#67331,#67332,#67333,#67334,
#67335),.UNSPECIFIED.,.F.,.F.,(4,2,4),(0.,1.,2.),.UNSPECIFIED.);
#1041=B_SPLINE_CURVE_WITH_KNOTS('',3,(#67413,#67414,#67415,#67416,#67417,
#67418),.UNSPECIFIED.,.F.,.F.,(4,2,4),(0.,1.,2.),.UNSPECIFIED.);
#1042=B_SPLINE_CURVE_WITH_KNOTS('',3,(#67772,#67773,#67774,#67775,#67776,
#67777),.UNSPECIFIED.,.F.,.F.,(4,2,4),(0.,1.,2.),.UNSPECIFIED.);
#1043=B_SPLINE_CURVE_WITH_KNOTS('',3,(#67855,#67856,#67857,#67858,#67859,
#67860),.UNSPECIFIED.,.F.,.F.,(4,2,4),(0.,1.,2.),.UNSPECIFIED.);
#1044=B_SPLINE_CURVE_WITH_KNOTS('',3,(#68214,#68215,#68216,#68217,#68218,
#68219),.UNSPECIFIED.,.F.,.F.,(4,2,4),(0.,1.,2.),.UNSPECIFIED.);
#1045=B_SPLINE_CURVE_WITH_KNOTS('',3,(#68297,#68298,#68299,#68300,#68301,
#68302),.UNSPECIFIED.,.F.,.F.,(4,2,4),(0.,1.,2.),.UNSPECIFIED.);
#1046=B_SPLINE_CURVE_WITH_KNOTS('',3,(#68656,#68657,#68658,#68659,#68660,
#68661),.UNSPECIFIED.,.F.,.F.,(4,2,4),(0.,1.,2.),.UNSPECIFIED.);
#1047=B_SPLINE_CURVE_WITH_KNOTS('',3,(#68739,#68740,#68741,#68742,#68743,
#68744),.UNSPECIFIED.,.F.,.F.,(4,2,4),(0.,1.,2.),.UNSPECIFIED.);
#1048=B_SPLINE_CURVE_WITH_KNOTS('',3,(#69098,#69099,#69100,#69101,#69102,
#69103),.UNSPECIFIED.,.F.,.F.,(4,2,4),(0.,1.,2.),.UNSPECIFIED.);
#1049=B_SPLINE_CURVE_WITH_KNOTS('',3,(#69181,#69182,#69183,#69184,#69185,
#69186),.UNSPECIFIED.,.F.,.F.,(4,2,4),(0.,1.,2.),.UNSPECIFIED.);
#1050=B_SPLINE_CURVE_WITH_KNOTS('',3,(#69540,#69541,#69542,#69543,#69544,
#69545),.UNSPECIFIED.,.F.,.F.,(4,2,4),(0.,1.,2.),.UNSPECIFIED.);
#1051=B_SPLINE_CURVE_WITH_KNOTS('',3,(#69623,#69624,#69625,#69626,#69627,
#69628),.UNSPECIFIED.,.F.,.F.,(4,2,4),(0.,1.,2.),.UNSPECIFIED.);
#1052=B_SPLINE_CURVE_WITH_KNOTS('',3,(#69982,#69983,#69984,#69985,#69986,
#69987),.UNSPECIFIED.,.F.,.F.,(4,2,4),(0.,1.,2.),.UNSPECIFIED.);
#1053=B_SPLINE_CURVE_WITH_KNOTS('',3,(#70065,#70066,#70067,#70068,#70069,
#70070),.UNSPECIFIED.,.F.,.F.,(4,2,4),(0.,1.,2.),.UNSPECIFIED.);
#1054=B_SPLINE_CURVE_WITH_KNOTS('',3,(#70424,#70425,#70426,#70427,#70428,
#70429),.UNSPECIFIED.,.F.,.F.,(4,2,4),(0.,1.,2.),.UNSPECIFIED.);
#1055=B_SPLINE_CURVE_WITH_KNOTS('',3,(#70507,#70508,#70509,#70510,#70511,
#70512),.UNSPECIFIED.,.F.,.F.,(4,2,4),(0.,1.,2.),.UNSPECIFIED.);
#1056=B_SPLINE_CURVE_WITH_KNOTS('',3,(#70866,#70867,#70868,#70869,#70870,
#70871),.UNSPECIFIED.,.F.,.F.,(4,2,4),(0.,1.,2.),.UNSPECIFIED.);
#1057=B_SPLINE_CURVE_WITH_KNOTS('',3,(#70949,#70950,#70951,#70952,#70953,
#70954),.UNSPECIFIED.,.F.,.F.,(4,2,4),(0.,1.,2.),.UNSPECIFIED.);
#1058=B_SPLINE_CURVE_WITH_KNOTS('',3,(#71308,#71309,#71310,#71311,#71312,
#71313),.UNSPECIFIED.,.F.,.F.,(4,2,4),(0.,1.,2.),.UNSPECIFIED.);
#1059=B_SPLINE_CURVE_WITH_KNOTS('',3,(#71391,#71392,#71393,#71394,#71395,
#71396),.UNSPECIFIED.,.F.,.F.,(4,2,4),(0.,1.,2.),.UNSPECIFIED.);
#1060=B_SPLINE_CURVE_WITH_KNOTS('',3,(#71750,#71751,#71752,#71753,#71754,
#71755),.UNSPECIFIED.,.F.,.F.,(4,2,4),(0.,1.,2.),.UNSPECIFIED.);
#1061=B_SPLINE_CURVE_WITH_KNOTS('',3,(#71833,#71834,#71835,#71836,#71837,
#71838),.UNSPECIFIED.,.F.,.F.,(4,2,4),(0.,1.,2.),.UNSPECIFIED.);
#1062=B_SPLINE_CURVE_WITH_KNOTS('',3,(#72192,#72193,#72194,#72195,#72196,
#72197),.UNSPECIFIED.,.F.,.F.,(4,2,4),(0.,1.,2.),.UNSPECIFIED.);
#1063=B_SPLINE_CURVE_WITH_KNOTS('',3,(#72275,#72276,#72277,#72278,#72279,
#72280),.UNSPECIFIED.,.F.,.F.,(4,2,4),(0.,1.,2.),.UNSPECIFIED.);
#1064=B_SPLINE_CURVE_WITH_KNOTS('',3,(#72638,#72639,#72640,#72641,#72642,
#72643),.UNSPECIFIED.,.F.,.F.,(4,2,4),(0.,1.,2.),.UNSPECIFIED.);
#1065=B_SPLINE_CURVE_WITH_KNOTS('',3,(#72717,#72718,#72719,#72720,#72721,
#72722),.UNSPECIFIED.,.F.,.F.,(4,2,4),(0.,1.,2.),.UNSPECIFIED.);
#1066=B_SPLINE_CURVE_WITH_KNOTS('',3,(#72864,#72865,#72866,#72867,#72868,
#72869),.UNSPECIFIED.,.F.,.F.,(4,2,4),(0.,1.,2.),.UNSPECIFIED.);
#1067=SPHERICAL_SURFACE('',#17458,0.29765);
#1068=SPHERICAL_SURFACE('',#17460,0.29765);
#1069=SPHERICAL_SURFACE('',#17462,0.29765);
#1070=SPHERICAL_SURFACE('',#17464,0.29765);
#1071=SPHERICAL_SURFACE('',#17466,0.29765);
#1072=SPHERICAL_SURFACE('',#17468,0.29765);
#1073=SPHERICAL_SURFACE('',#17470,0.29765);
#1074=SPHERICAL_SURFACE('',#17473,0.309556);
#1075=SPHERICAL_SURFACE('',#17489,0.309556);
#1076=SPHERICAL_SURFACE('',#17494,0.309556);
#1077=SPHERICAL_SURFACE('',#17500,0.309556);
#1078=SPHERICAL_SURFACE('',#17505,0.309556);
#1079=SPHERICAL_SURFACE('',#17510,0.309556);
#1080=SPHERICAL_SURFACE('',#17518,0.309556);
#1081=SPHERICAL_SURFACE('',#17586,0.3969);
#1082=SPHERICAL_SURFACE('',#17588,0.3969);
#1083=SPHERICAL_SURFACE('',#17590,0.3969);
#1084=SPHERICAL_SURFACE('',#17592,0.3969);
#1085=SPHERICAL_SURFACE('',#17594,0.3969);
#1086=SPHERICAL_SURFACE('',#17596,0.3969);
#1087=SPHERICAL_SURFACE('',#17598,0.3969);
#1088=SPHERICAL_SURFACE('',#17600,0.3969);
#1089=SPHERICAL_SURFACE('',#17603,0.412776);
#1090=SPHERICAL_SURFACE('',#17619,0.412776);
#1091=SPHERICAL_SURFACE('',#17624,0.412776);
#1092=SPHERICAL_SURFACE('',#17629,0.412776);
#1093=SPHERICAL_SURFACE('',#17634,0.412776);
#1094=SPHERICAL_SURFACE('',#17639,0.412776);
#1095=SPHERICAL_SURFACE('',#17644,0.412776);
#1096=SPHERICAL_SURFACE('',#17652,0.412776);
#1097=TOROIDAL_SURFACE('',#17418,1.1,0.309556);
#1098=TOROIDAL_SURFACE('',#17438,1.1,0.309556);
#1099=TOROIDAL_SURFACE('',#17546,1.675,0.412776);
#1100=TOROIDAL_SURFACE('',#17566,1.675,0.412776);
#1101=CONICAL_SURFACE('',#17405,0.475,0.785398163397449);
#1102=CONICAL_SURFACE('',#17409,0.485,0.785398163397448);
#1103=CONICAL_SURFACE('',#17413,0.31,0.463647609000806);
#1104=CONICAL_SURFACE('',#17429,0.63,0.785398163397448);
#1105=CONICAL_SURFACE('',#17436,0.63,0.785398163397448);
#1106=CONICAL_SURFACE('',#17449,1.57,0.785398163397449);
#1107=CONICAL_SURFACE('',#17453,1.57,0.785398163397449);
#1108=CONICAL_SURFACE('',#17557,1.05,0.785398163397449);
#1109=CONICAL_SURFACE('',#17564,1.05,0.785398163397449);
#1110=CONICAL_SURFACE('',#17577,2.3,0.785398163397449);
#1111=CONICAL_SURFACE('',#17581,2.3,0.785398163397449);
#1112=CONICAL_SURFACE('',#17681,0.325,0.785398163397448);
#1113=CONICAL_SURFACE('',#17685,0.335,0.785398163397448);
#1114=CONICAL_SURFACE('',#17689,0.21,0.463647609000806);
#1115=CONICAL_SURFACE('',#17693,0.18,0.785398163397448);
#1116=CONICAL_SURFACE('',#18227,0.235,0.785398163397448);
#1117=CONICAL_SURFACE('',#18231,0.2125,0.785398163397448);
#1118=ORIENTED_CLOSED_SHELL('',*,#16138,.F.);
#1119=ORIENTED_CLOSED_SHELL('',*,#16166,.F.);
#1120=BREP_WITH_VOIDS('Body1',#16139,(#1118));
#1121=BREP_WITH_VOIDS('Body1',#16165,(#1119));
#1122=SHAPE_REPRESENTATION_RELATIONSHIP('SRR','None',#73609,#1178);
#1123=SHAPE_REPRESENTATION_RELATIONSHIP('SRR','None',#73610,#1179);
#1124=SHAPE_REPRESENTATION_RELATIONSHIP('SRR','None',#73611,#1180);
#1125=SHAPE_REPRESENTATION_RELATIONSHIP('SRR','None',#73612,#1181);
#1126=SHAPE_REPRESENTATION_RELATIONSHIP('SRR','None',#73613,#1182);
#1127=SHAPE_REPRESENTATION_RELATIONSHIP('SRR','None',#73614,#1183);
#1128=SHAPE_REPRESENTATION_RELATIONSHIP('SRR','None',#73615,#1184);
#1129=SHAPE_REPRESENTATION_RELATIONSHIP('SRR','None',#73616,#1185);
#1130=SHAPE_REPRESENTATION_RELATIONSHIP('SRR','None',#73617,#1186);
#1131=SHAPE_REPRESENTATION_RELATIONSHIP('SRR','None',#73618,#1187);
#1132=SHAPE_REPRESENTATION_RELATIONSHIP('SRR','None',#73619,#1188);
#1133=SHAPE_REPRESENTATION_RELATIONSHIP('SRR','None',#73620,#1189);
#1134=SHAPE_REPRESENTATION_RELATIONSHIP('SRR','None',#73621,#1190);
#1135=SHAPE_REPRESENTATION_RELATIONSHIP('SRR','None',#73622,#1191);
#1136=SHAPE_REPRESENTATION_RELATIONSHIP('SRR','None',#73623,#1192);
#1137=SHAPE_REPRESENTATION_RELATIONSHIP('SRR','None',#73624,#1193);
#1138=SHAPE_REPRESENTATION_RELATIONSHIP('SRR','None',#73625,#1194);
#1139=SHAPE_REPRESENTATION_RELATIONSHIP('SRR','None',#73627,#1195);
#1140=SHAPE_REPRESENTATION_RELATIONSHIP('SRR','None',#73628,#1196);
#1141=SHAPE_REPRESENTATION_RELATIONSHIP('SRR','None',#73629,#1197);
#1142=SHAPE_REPRESENTATION_RELATIONSHIP('SRR','None',#73630,#1198);
#1143=SHAPE_REPRESENTATION_RELATIONSHIP('SRR','None',#73631,#1199);
#1144=SHAPE_REPRESENTATION_RELATIONSHIP('SRR','None',#73633,#1200);
#1145=SHAPE_REPRESENTATION_RELATIONSHIP('SRR','None',#73634,#1201);
#1146=SHAPE_REPRESENTATION_RELATIONSHIP('SRR','None',#73635,#1202);
#1147=SHAPE_REPRESENTATION_RELATIONSHIP('SRR','None',#73636,#1203);
#1148=SHAPE_REPRESENTATION_RELATIONSHIP('SRR','None',#73637,#1204);
#1149=SHAPE_REPRESENTATION_RELATIONSHIP('SRR','None',#73638,#1205);
#1150=SHAPE_REPRESENTATION_RELATIONSHIP('SRR','None',#73640,#1206);
#1151=SHAPE_REPRESENTATION_RELATIONSHIP('SRR','None',#73641,#1207);
#1152=SHAPE_REPRESENTATION_RELATIONSHIP('SRR','None',#73642,#1208);
#1153=SHAPE_REPRESENTATION_RELATIONSHIP('SRR','None',#73643,#1209);
#1154=SHAPE_REPRESENTATION_RELATIONSHIP('SRR','None',#73644,#1210);
#1155=SHAPE_REPRESENTATION_RELATIONSHIP('SRR','None',#73645,#1211);
#1156=SHAPE_REPRESENTATION_RELATIONSHIP('SRR','None',#73646,#1212);
#1157=SHAPE_REPRESENTATION_RELATIONSHIP('SRR','None',#73647,#1213);
#1158=SHAPE_REPRESENTATION_RELATIONSHIP('SRR','None',#73648,#1214);
#1159=SHAPE_REPRESENTATION_RELATIONSHIP('SRR','None',#73650,#1215);
#1160=SHAPE_REPRESENTATION_RELATIONSHIP('SRR','None',#73651,#1216);
#1161=SHAPE_REPRESENTATION_RELATIONSHIP('SRR','None',#73652,#1217);
#1162=SHAPE_REPRESENTATION_RELATIONSHIP('SRR','None',#73653,#1218);
#1163=SHAPE_REPRESENTATION_RELATIONSHIP('SRR','None',#73654,#1219);
#1164=SHAPE_REPRESENTATION_RELATIONSHIP('SRR','None',#73655,#1220);
#1165=SHAPE_REPRESENTATION_RELATIONSHIP('SRR','None',#73656,#1221);
#1166=SHAPE_REPRESENTATION_RELATIONSHIP('SRR','None',#73657,#1222);
#1167=SHAPE_REPRESENTATION_RELATIONSHIP('SRR','None',#73658,#1223);
#1168=SHAPE_REPRESENTATION_RELATIONSHIP('SRR','None',#73660,#1224);
#1169=SHAPE_REPRESENTATION_RELATIONSHIP('SRR','None',#73661,#1225);
#1170=SHAPE_REPRESENTATION_RELATIONSHIP('SRR','None',#73662,#1226);
#1171=SHAPE_REPRESENTATION_RELATIONSHIP('SRR','None',#73663,#1227);
#1172=SHAPE_REPRESENTATION_RELATIONSHIP('SRR','None',#73664,#1228);
#1173=SHAPE_REPRESENTATION_RELATIONSHIP('SRR','None',#73665,#1229);
#1174=SHAPE_REPRESENTATION_RELATIONSHIP('SRR','None',#73666,#1230);
#1175=SHAPE_REPRESENTATION_RELATIONSHIP('SRR','None',#73667,#1231);
#1176=SHAPE_REPRESENTATION_RELATIONSHIP('SRR','None',#73668,#1232);
#1177=SHAPE_REPRESENTATION_RELATIONSHIP('SRR','None',#73669,#1233);
#1178=ADVANCED_BREP_SHAPE_REPRESENTATION('',(#1305),#73305);
#1179=ADVANCED_BREP_SHAPE_REPRESENTATION('',(#1306),#73306);
#1180=ADVANCED_BREP_SHAPE_REPRESENTATION('',(#1307),#73307);
#1181=ADVANCED_BREP_SHAPE_REPRESENTATION('',(#1308),#73308);
#1182=ADVANCED_BREP_SHAPE_REPRESENTATION('',(#1309),#73309);
#1183=ADVANCED_BREP_SHAPE_REPRESENTATION('',(#1310),#73310);
#1184=ADVANCED_BREP_SHAPE_REPRESENTATION('',(#1311),#73311);
#1185=ADVANCED_BREP_SHAPE_REPRESENTATION('',(#1312),#73312);
#1186=ADVANCED_BREP_SHAPE_REPRESENTATION('',(#1313),#73313);
#1187=ADVANCED_BREP_SHAPE_REPRESENTATION('',(#1314),#73314);
#1188=ADVANCED_BREP_SHAPE_REPRESENTATION('',(#1315),#73315);
#1189=ADVANCED_BREP_SHAPE_REPRESENTATION('',(#1316),#73316);
#1190=ADVANCED_BREP_SHAPE_REPRESENTATION('',(#1317),#73317);
#1191=ADVANCED_BREP_SHAPE_REPRESENTATION('',(#1318),#73318);
#1192=ADVANCED_BREP_SHAPE_REPRESENTATION('',(#1319),#73319);
#1193=ADVANCED_BREP_SHAPE_REPRESENTATION('',(#1320),#73320);
#1194=ADVANCED_BREP_SHAPE_REPRESENTATION('',(#1120),#73321);
#1195=ADVANCED_BREP_SHAPE_REPRESENTATION('',(#1321),#73323);
#1196=ADVANCED_BREP_SHAPE_REPRESENTATION('',(#1322),#73324);
#1197=ADVANCED_BREP_SHAPE_REPRESENTATION('',(#1323,#1324,#1325,#1326,#1327,
#1328,#1329),#73325);
#1198=ADVANCED_BREP_SHAPE_REPRESENTATION('',(#1330),#73326);
#1199=ADVANCED_BREP_SHAPE_REPRESENTATION('',(#1331,#1332),#73327);
#1200=ADVANCED_BREP_SHAPE_REPRESENTATION('',(#1333),#73329);
#1201=ADVANCED_BREP_SHAPE_REPRESENTATION('',(#1334),#73330);
#1202=ADVANCED_BREP_SHAPE_REPRESENTATION('',(#1335,#1336,#1337,#1338,#1339,
#1340,#1341,#1342),#73331);
#1203=ADVANCED_BREP_SHAPE_REPRESENTATION('',(#1343),#73332);
#1204=ADVANCED_BREP_SHAPE_REPRESENTATION('',(#1344,#1345),#73333);
#1205=ADVANCED_BREP_SHAPE_REPRESENTATION('',(#1121),#73334);
#1206=ADVANCED_BREP_SHAPE_REPRESENTATION('',(#1346),#73336);
#1207=ADVANCED_BREP_SHAPE_REPRESENTATION('',(#1347),#73337);
#1208=ADVANCED_BREP_SHAPE_REPRESENTATION('',(#1348),#73338);
#1209=ADVANCED_BREP_SHAPE_REPRESENTATION('',(#1349),#73339);
#1210=ADVANCED_BREP_SHAPE_REPRESENTATION('',(#1350),#73340);
#1211=ADVANCED_BREP_SHAPE_REPRESENTATION('',(#1351),#73341);
#1212=ADVANCED_BREP_SHAPE_REPRESENTATION('',(#1352),#73342);
#1213=ADVANCED_BREP_SHAPE_REPRESENTATION('',(#1353),#73343);
#1214=ADVANCED_BREP_SHAPE_REPRESENTATION('',(#1354),#73344);
#1215=ADVANCED_BREP_SHAPE_REPRESENTATION('',(#1355),#73346);
#1216=ADVANCED_BREP_SHAPE_REPRESENTATION('',(#1356),#73347);
#1217=ADVANCED_BREP_SHAPE_REPRESENTATION('',(#1357),#73348);
#1218=ADVANCED_BREP_SHAPE_REPRESENTATION('',(#1358),#73349);
#1219=ADVANCED_BREP_SHAPE_REPRESENTATION('',(#1359),#73350);
#1220=ADVANCED_BREP_SHAPE_REPRESENTATION('',(#1360),#73351);
#1221=ADVANCED_BREP_SHAPE_REPRESENTATION('',(#1361),#73352);
#1222=ADVANCED_BREP_SHAPE_REPRESENTATION('',(#1362),#73353);
#1223=ADVANCED_BREP_SHAPE_REPRESENTATION('',(#1363),#73354);
#1224=ADVANCED_BREP_SHAPE_REPRESENTATION('',(#1364),#73356);
#1225=ADVANCED_BREP_SHAPE_REPRESENTATION('',(#1365),#73357);
#1226=ADVANCED_BREP_SHAPE_REPRESENTATION('',(#1366),#73358);
#1227=ADVANCED_BREP_SHAPE_REPRESENTATION('',(#1367),#73359);
#1228=ADVANCED_BREP_SHAPE_REPRESENTATION('',(#1368),#73360);
#1229=ADVANCED_BREP_SHAPE_REPRESENTATION('',(#1369),#73361);
#1230=ADVANCED_BREP_SHAPE_REPRESENTATION('',(#1370),#73362);
#1231=ADVANCED_BREP_SHAPE_REPRESENTATION('',(#1371),#73363);
#1232=ADVANCED_BREP_SHAPE_REPRESENTATION('',(#1372),#73364);
#1233=ADVANCED_BREP_SHAPE_REPRESENTATION('',(#1373),#73365);
#1234=STYLED_ITEM('',(#73967),#1305);
#1235=STYLED_ITEM('',(#73967),#1306);
#1236=STYLED_ITEM('',(#73967),#1307);
#1237=STYLED_ITEM('',(#73974),#1308);
#1238=STYLED_ITEM('',(#73974),#1309);
#1239=STYLED_ITEM('',(#73974),#1310);
#1240=STYLED_ITEM('',(#73974),#1311);
#1241=STYLED_ITEM('',(#74002),#1312);
#1242=STYLED_ITEM('',(#74002),#1313);
#1243=STYLED_ITEM('',(#74002),#1314);
#1244=STYLED_ITEM('',(#74002),#1315);
#1245=STYLED_ITEM('',(#74002),#1316);
#1246=STYLED_ITEM('',(#74002),#1317);
#1247=STYLED_ITEM('',(#73974),#1318);
#1248=STYLED_ITEM('',(#73974),#1319);
#1249=STYLED_ITEM('',(#73974),#1320);
#1250=STYLED_ITEM('',(#73995),#1120);
#1251=STYLED_ITEM('',(#73988),#1321);
#1252=STYLED_ITEM('',(#73988),#1322);
#1253=STYLED_ITEM('',(#73988),#1323);
#1254=STYLED_ITEM('',(#73988),#1324);
#1255=STYLED_ITEM('',(#73988),#1325);
#1256=STYLED_ITEM('',(#73988),#1326);
#1257=STYLED_ITEM('',(#73988),#1327);
#1258=STYLED_ITEM('',(#73988),#1328);
#1259=STYLED_ITEM('',(#73988),#1329);
#1260=STYLED_ITEM('',(#73988),#1330);
#1261=STYLED_ITEM('',(#73988),#1331);
#1262=STYLED_ITEM('',(#73988),#1332);
#1263=STYLED_ITEM('',(#73988),#1333);
#1264=STYLED_ITEM('',(#73988),#1334);
#1265=STYLED_ITEM('',(#73988),#1335);
#1266=STYLED_ITEM('',(#73988),#1336);
#1267=STYLED_ITEM('',(#73988),#1337);
#1268=STYLED_ITEM('',(#73988),#1338);
#1269=STYLED_ITEM('',(#73988),#1339);
#1270=STYLED_ITEM('',(#73988),#1340);
#1271=STYLED_ITEM('',(#73988),#1341);
#1272=STYLED_ITEM('',(#73988),#1342);
#1273=STYLED_ITEM('',(#73988),#1343);
#1274=STYLED_ITEM('',(#73988),#1344);
#1275=STYLED_ITEM('',(#73988),#1345);
#1276=STYLED_ITEM('',(#73995),#1121);
#1277=STYLED_ITEM('',(#73988),#1346);
#1278=STYLED_ITEM('',(#73988),#1347);
#1279=STYLED_ITEM('',(#73988),#1348);
#1280=STYLED_ITEM('',(#73974),#1349);
#1281=STYLED_ITEM('',(#73974),#1350);
#1282=STYLED_ITEM('',(#74002),#1351);
#1283=STYLED_ITEM('',(#73981),#1352);
#1284=STYLED_ITEM('',(#74002),#1353);
#1285=STYLED_ITEM('',(#73988),#1354);
#1286=STYLED_ITEM('',(#73988),#1355);
#1287=STYLED_ITEM('',(#73988),#1356);
#1288=STYLED_ITEM('',(#73988),#1357);
#1289=STYLED_ITEM('',(#73974),#1358);
#1290=STYLED_ITEM('',(#73974),#1359);
#1291=STYLED_ITEM('',(#74002),#1360);
#1292=STYLED_ITEM('',(#73981),#1361);
#1293=STYLED_ITEM('',(#73974),#1362);
#1294=STYLED_ITEM('',(#73974),#1363);
#1295=STYLED_ITEM('',(#73988),#1364);
#1296=STYLED_ITEM('',(#73988),#1365);
#1297=STYLED_ITEM('',(#73988),#1366);
#1298=STYLED_ITEM('',(#73974),#1367);
#1299=STYLED_ITEM('',(#73974),#1368);
#1300=STYLED_ITEM('',(#73981),#1369);
#1301=STYLED_ITEM('',(#73974),#1370);
#1302=STYLED_ITEM('',(#73995),#1371);
#1303=STYLED_ITEM('',(#73981),#1372);
#1304=STYLED_ITEM('',(#73988),#1373);
#1305=MANIFOLD_SOLID_BREP('Body1',#16122);
#1306=MANIFOLD_SOLID_BREP('Body1',#16123);
#1307=MANIFOLD_SOLID_BREP('Body1',#16124);
#1308=MANIFOLD_SOLID_BREP('Body1',#16125);
#1309=MANIFOLD_SOLID_BREP('Body1',#16126);
#1310=MANIFOLD_SOLID_BREP('Body1',#16127);
#1311=MANIFOLD_SOLID_BREP('Body1',#16128);
#1312=MANIFOLD_SOLID_BREP('Body1',#16129);
#1313=MANIFOLD_SOLID_BREP('Body1',#16130);
#1314=MANIFOLD_SOLID_BREP('Body1',#16131);
#1315=MANIFOLD_SOLID_BREP('Body1',#16132);
#1316=MANIFOLD_SOLID_BREP('Body1',#16133);
#1317=MANIFOLD_SOLID_BREP('Body1',#16134);
#1318=MANIFOLD_SOLID_BREP('Body1',#16135);
#1319=MANIFOLD_SOLID_BREP('Body1',#16136);
#1320=MANIFOLD_SOLID_BREP('Body1',#16137);
#1321=MANIFOLD_SOLID_BREP('Body1',#16140);
#1322=MANIFOLD_SOLID_BREP('Body1',#16141);
#1323=MANIFOLD_SOLID_BREP('Body1',#16142);
#1324=MANIFOLD_SOLID_BREP('Body2',#16143);
#1325=MANIFOLD_SOLID_BREP('Body3',#16144);
#1326=MANIFOLD_SOLID_BREP('Body4',#16145);
#1327=MANIFOLD_SOLID_BREP('Body5',#16146);
#1328=MANIFOLD_SOLID_BREP('Body6',#16147);
#1329=MANIFOLD_SOLID_BREP('Body7',#16148);
#1330=MANIFOLD_SOLID_BREP('Continuous crown cage',#16149);
#1331=MANIFOLD_SOLID_BREP('Body1',#16150);
#1332=MANIFOLD_SOLID_BREP('Body2',#16151);
#1333=MANIFOLD_SOLID_BREP('Body1',#16152);
#1334=MANIFOLD_SOLID_BREP('Body1',#16153);
#1335=MANIFOLD_SOLID_BREP('Body1',#16154);
#1336=MANIFOLD_SOLID_BREP('Body2',#16155);
#1337=MANIFOLD_SOLID_BREP('Body3',#16156);
#1338=MANIFOLD_SOLID_BREP('Body4',#16157);
#1339=MANIFOLD_SOLID_BREP('Body5',#16158);
#1340=MANIFOLD_SOLID_BREP('Body6',#16159);
#1341=MANIFOLD_SOLID_BREP('Body7',#16160);
#1342=MANIFOLD_SOLID_BREP('Body8',#16161);
#1343=MANIFOLD_SOLID_BREP('Continuous crown cage',#16162);
#1344=MANIFOLD_SOLID_BREP('Body1',#16163);
#1345=MANIFOLD_SOLID_BREP('Body2',#16164);
#1346=MANIFOLD_SOLID_BREP('Body1',#16167);
#1347=MANIFOLD_SOLID_BREP('Body1',#16168);
#1348=MANIFOLD_SOLID_BREP('Body1',#16169);
#1349=MANIFOLD_SOLID_BREP('Body1',#16170);
#1350=MANIFOLD_SOLID_BREP('Body1',#16171);
#1351=MANIFOLD_SOLID_BREP('Body1',#16172);
#1352=MANIFOLD_SOLID_BREP('Body1',#16173);
#1353=MANIFOLD_SOLID_BREP('Body1',#16174);
#1354=MANIFOLD_SOLID_BREP('Body1',#16175);
#1355=MANIFOLD_SOLID_BREP('Body1',#16176);
#1356=MANIFOLD_SOLID_BREP('Body1',#16177);
#1357=MANIFOLD_SOLID_BREP('Body1',#16178);
#1358=MANIFOLD_SOLID_BREP('Body1',#16179);
#1359=MANIFOLD_SOLID_BREP('Body1',#16180);
#1360=MANIFOLD_SOLID_BREP('Body1',#16181);
#1361=MANIFOLD_SOLID_BREP('Body1',#16182);
#1362=MANIFOLD_SOLID_BREP('Body1',#16183);
#1363=MANIFOLD_SOLID_BREP('Body1',#16184);
#1364=MANIFOLD_SOLID_BREP('Body1',#16185);
#1365=MANIFOLD_SOLID_BREP('Body1',#16186);
#1366=MANIFOLD_SOLID_BREP('Body1',#16187);
#1367=MANIFOLD_SOLID_BREP('Body1',#16188);
#1368=MANIFOLD_SOLID_BREP('Body1',#16189);
#1369=MANIFOLD_SOLID_BREP('Body1',#16190);
#1370=MANIFOLD_SOLID_BREP('Body1',#16191);
#1371=MANIFOLD_SOLID_BREP('Body1',#16192);
#1372=MANIFOLD_SOLID_BREP('Body1',#16193);
#1373=MANIFOLD_SOLID_BREP('Body1',#16194);
#1374=FACE_BOUND('',#2924,.T.);
#1375=FACE_BOUND('',#2925,.T.);
#1376=FACE_BOUND('',#2926,.T.);
#1377=FACE_BOUND('',#2927,.T.);
#1378=FACE_BOUND('',#2929,.T.);
#1379=FACE_BOUND('',#2930,.T.);
#1380=FACE_BOUND('',#2931,.T.);
#1381=FACE_BOUND('',#2932,.T.);
#1382=FACE_BOUND('',#2944,.T.);
#1383=FACE_BOUND('',#2945,.T.);
#1384=FACE_BOUND('',#2946,.T.);
#1385=FACE_BOUND('',#2947,.T.);
#1386=FACE_BOUND('',#2948,.T.);
#1387=FACE_BOUND('',#2949,.T.);
#1388=FACE_BOUND('',#2951,.T.);
#1389=FACE_BOUND('',#2952,.T.);
#1390=FACE_BOUND('',#2953,.T.);
#1391=FACE_BOUND('',#2954,.T.);
#1392=FACE_BOUND('',#2955,.T.);
#1393=FACE_BOUND('',#2959,.T.);
#1394=FACE_BOUND('',#2960,.T.);
#1395=FACE_BOUND('',#2961,.T.);
#1396=FACE_BOUND('',#2962,.T.);
#1397=FACE_BOUND('',#2963,.T.);
#1398=FACE_BOUND('',#2964,.T.);
#1399=FACE_BOUND('',#2998,.T.);
#1400=FACE_BOUND('',#2999,.T.);
#1401=FACE_BOUND('',#3000,.T.);
#1402=FACE_BOUND('',#3001,.T.);
#1403=FACE_BOUND('',#3002,.T.);
#1404=FACE_BOUND('',#3009,.T.);
#1405=FACE_BOUND('',#3012,.T.);
#1406=FACE_BOUND('',#3015,.T.);
#1407=FACE_BOUND('',#3018,.T.);
#1408=FACE_BOUND('',#3039,.T.);
#1409=FACE_BOUND('',#3040,.T.);
#1410=FACE_BOUND('',#3041,.T.);
#1411=FACE_BOUND('',#3045,.T.);
#1412=FACE_BOUND('',#3046,.T.);
#1413=FACE_BOUND('',#3047,.T.);
#1414=FACE_BOUND('',#3051,.T.);
#1415=FACE_BOUND('',#3052,.T.);
#1416=FACE_BOUND('',#3053,.T.);
#1417=FACE_BOUND('',#3054,.T.);
#1418=FACE_BOUND('',#3057,.T.);
#1419=FACE_BOUND('',#3058,.T.);
#1420=FACE_BOUND('',#3059,.T.);
#1421=FACE_BOUND('',#3060,.T.);
#1422=FACE_BOUND('',#3081,.T.);
#1423=FACE_BOUND('',#3082,.T.);
#1424=FACE_BOUND('',#3083,.T.);
#1425=FACE_BOUND('',#3084,.T.);
#1426=FACE_BOUND('',#3085,.T.);
#1427=FACE_BOUND('',#3089,.T.);
#1428=FACE_BOUND('',#3090,.T.);
#1429=FACE_BOUND('',#3091,.T.);
#1430=FACE_BOUND('',#3092,.T.);
#1431=FACE_BOUND('',#3093,.T.);
#1432=FACE_BOUND('',#3094,.T.);
#1433=FACE_BOUND('',#3097,.T.);
#1434=FACE_BOUND('',#3098,.T.);
#1435=FACE_BOUND('',#3099,.T.);
#1436=FACE_BOUND('',#3100,.T.);
#1437=FACE_BOUND('',#3101,.T.);
#1438=FACE_BOUND('',#3102,.T.);
#1439=FACE_BOUND('',#3138,.T.);
#1440=FACE_BOUND('',#3139,.T.);
#1441=FACE_BOUND('',#3140,.T.);
#1442=FACE_BOUND('',#3141,.T.);
#1443=FACE_BOUND('',#3142,.T.);
#1444=FACE_BOUND('',#3159,.T.);
#1445=FACE_BOUND('',#3160,.T.);
#1446=FACE_BOUND('',#3161,.T.);
#1447=FACE_BOUND('',#3164,.T.);
#1448=FACE_BOUND('',#3165,.T.);
#1449=FACE_BOUND('',#3166,.T.);
#1450=FACE_BOUND('',#3171,.T.);
#1451=FACE_BOUND('',#3172,.T.);
#1452=FACE_BOUND('',#3173,.T.);
#1453=FACE_BOUND('',#3174,.T.);
#1454=FACE_BOUND('',#3175,.T.);
#1455=FACE_BOUND('',#3178,.T.);
#1456=FACE_BOUND('',#3179,.T.);
#1457=FACE_BOUND('',#3180,.T.);
#1458=FACE_BOUND('',#3181,.T.);
#1459=FACE_BOUND('',#3182,.T.);
#1460=FACE_BOUND('',#3200,.T.);
#1461=FACE_BOUND('',#3207,.T.);
#1462=FACE_BOUND('',#3210,.T.);
#1463=FACE_BOUND('',#3216,.T.);
#1464=FACE_BOUND('',#3223,.T.);
#1465=FACE_BOUND('',#3226,.T.);
#1466=FACE_BOUND('',#3233,.T.);
#1467=FACE_BOUND('',#3237,.T.);
#1468=FACE_BOUND('',#3238,.T.);
#1469=FACE_BOUND('',#3239,.T.);
#1470=FACE_BOUND('',#3240,.T.);
#1471=FACE_BOUND('',#3241,.T.);
#1472=FACE_BOUND('',#3243,.T.);
#1473=FACE_BOUND('',#3244,.T.);
#1474=FACE_BOUND('',#3245,.T.);
#1475=FACE_BOUND('',#3246,.T.);
#1476=FACE_BOUND('',#3247,.T.);
#1477=FACE_BOUND('',#3254,.T.);
#1478=FACE_BOUND('',#3258,.T.);
#1479=FACE_BOUND('',#3259,.T.);
#1480=FACE_BOUND('',#3260,.T.);
#1481=FACE_BOUND('',#3261,.T.);
#1482=FACE_BOUND('',#3262,.T.);
#1483=FACE_BOUND('',#3264,.T.);
#1484=FACE_BOUND('',#3265,.T.);
#1485=FACE_BOUND('',#3266,.T.);
#1486=FACE_BOUND('',#3267,.T.);
#1487=FACE_BOUND('',#3268,.T.);
#1488=FACE_BOUND('',#3275,.T.);
#1489=FACE_BOUND('',#3279,.T.);
#1490=FACE_BOUND('',#3280,.T.);
#1491=FACE_BOUND('',#3281,.T.);
#1492=FACE_BOUND('',#3282,.T.);
#1493=FACE_BOUND('',#3283,.T.);
#1494=FACE_BOUND('',#3285,.T.);
#1495=FACE_BOUND('',#3286,.T.);
#1496=FACE_BOUND('',#3287,.T.);
#1497=FACE_BOUND('',#3288,.T.);
#1498=FACE_BOUND('',#3289,.T.);
#1499=FACE_BOUND('',#3296,.T.);
#1500=FACE_BOUND('',#3300,.T.);
#1501=FACE_BOUND('',#3301,.T.);
#1502=FACE_BOUND('',#3302,.T.);
#1503=FACE_BOUND('',#3303,.T.);
#1504=FACE_BOUND('',#3304,.T.);
#1505=FACE_BOUND('',#3306,.T.);
#1506=FACE_BOUND('',#3307,.T.);
#1507=FACE_BOUND('',#3308,.T.);
#1508=FACE_BOUND('',#3309,.T.);
#1509=FACE_BOUND('',#3310,.T.);
#1510=FACE_BOUND('',#3320,.T.);
#1511=FACE_BOUND('',#3321,.T.);
#1512=FACE_BOUND('',#3322,.T.);
#1513=FACE_BOUND('',#3323,.T.);
#1514=FACE_BOUND('',#3325,.T.);
#1515=FACE_BOUND('',#3326,.T.);
#1516=FACE_BOUND('',#3327,.T.);
#1517=FACE_BOUND('',#3328,.T.);
#1518=FACE_BOUND('',#3355,.T.);
#1519=FACE_BOUND('',#3363,.T.);
#1520=FACE_BOUND('',#3366,.T.);
#1521=FACE_BOUND('',#3371,.T.);
#1522=FACE_BOUND('',#3376,.T.);
#1523=FACE_BOUND('',#3401,.T.);
#1524=FACE_BOUND('',#3404,.T.);
#1525=FACE_BOUND('',#3407,.T.);
#1526=FACE_BOUND('',#3410,.T.);
#1527=FACE_BOUND('',#3413,.T.);
#1528=FACE_BOUND('',#3420,.T.);
#1529=FACE_BOUND('',#3423,.T.);
#1530=FACE_BOUND('',#3428,.T.);
#1531=FACE_BOUND('',#3433,.T.);
#1532=FACE_BOUND('',#3461,.T.);
#1533=FACE_BOUND('',#3464,.T.);
#1534=FACE_BOUND('',#3467,.T.);
#1535=FACE_BOUND('',#3470,.T.);
#1536=FACE_BOUND('',#3473,.T.);
#1537=FACE_BOUND('',#3480,.T.);
#1538=FACE_BOUND('',#3499,.T.);
#1539=FACE_BOUND('',#3506,.T.);
#1540=FACE_BOUND('',#3508,.T.);
#1541=FACE_BOUND('',#3510,.T.);
#1542=FACE_BOUND('',#3512,.T.);
#1543=FACE_BOUND('',#3517,.T.);
#1544=FACE_BOUND('',#3519,.T.);
#1545=FACE_BOUND('',#3521,.T.);
#1546=FACE_BOUND('',#3523,.T.);
#1547=FACE_BOUND('',#3527,.T.);
#1548=FACE_BOUND('',#3529,.T.);
#1549=FACE_BOUND('',#3533,.T.);
#1550=FACE_BOUND('',#3535,.T.);
#1551=FACE_BOUND('',#3539,.T.);
#1552=FACE_BOUND('',#3541,.T.);
#1553=FACE_BOUND('',#3545,.T.);
#1554=FACE_BOUND('',#3547,.T.);
#1555=FACE_BOUND('',#3552,.T.);
#1556=FACE_BOUND('',#3556,.T.);
#1557=FACE_BOUND('',#3637,.T.);
#1558=FACE_BOUND('',#3660,.T.);
#1559=FACE_BOUND('',#3661,.T.);
#1560=FACE_BOUND('',#3668,.T.);
#1561=FACE_BOUND('',#3670,.T.);
#1562=FACE_BOUND('',#3672,.T.);
#1563=FACE_BOUND('',#3674,.T.);
#1564=FACE_BOUND('',#3679,.T.);
#1565=FACE_BOUND('',#3681,.T.);
#1566=FACE_BOUND('',#3683,.T.);
#1567=FACE_BOUND('',#3685,.T.);
#1568=FACE_BOUND('',#3689,.T.);
#1569=FACE_BOUND('',#3691,.T.);
#1570=FACE_BOUND('',#3695,.T.);
#1571=FACE_BOUND('',#3697,.T.);
#1572=FACE_BOUND('',#3701,.T.);
#1573=FACE_BOUND('',#3703,.T.);
#1574=FACE_BOUND('',#3707,.T.);
#1575=FACE_BOUND('',#3709,.T.);
#1576=FACE_BOUND('',#3713,.T.);
#1577=FACE_BOUND('',#3715,.T.);
#1578=FACE_BOUND('',#3720,.T.);
#1579=FACE_BOUND('',#3723,.T.);
#1580=FACE_BOUND('',#3805,.T.);
#1581=FACE_BOUND('',#3813,.T.);
#1582=FACE_BOUND('',#3820,.T.);
#1583=FACE_BOUND('',#3822,.T.);
#1584=FACE_BOUND('',#3824,.T.);
#1585=FACE_BOUND('',#3826,.T.);
#1586=FACE_BOUND('',#3831,.T.);
#1587=FACE_BOUND('',#3833,.T.);
#1588=FACE_BOUND('',#3835,.T.);
#1589=FACE_BOUND('',#3837,.T.);
#1590=FACE_BOUND('',#3841,.T.);
#1591=FACE_BOUND('',#3843,.T.);
#1592=FACE_BOUND('',#3847,.T.);
#1593=FACE_BOUND('',#3849,.T.);
#1594=FACE_BOUND('',#3853,.T.);
#1595=FACE_BOUND('',#3855,.T.);
#1596=FACE_BOUND('',#3859,.T.);
#1597=FACE_BOUND('',#3861,.T.);
#1598=FACE_BOUND('',#3870,.T.);
#1599=FACE_BOUND('',#3879,.T.);
#1600=FACE_BOUND('',#3883,.T.);
#1601=FACE_BOUND('',#4044,.T.);
#1602=PLANE('',#16827);
#1603=PLANE('',#16828);
#1604=PLANE('',#16829);
#1605=PLANE('',#16830);
#1606=PLANE('',#16831);
#1607=PLANE('',#16832);
#1608=PLANE('',#16837);
#1609=PLANE('',#16841);
#1610=PLANE('',#16845);
#1611=PLANE('',#16849);
#1612=PLANE('',#16853);
#1613=PLANE('',#16855);
#1614=PLANE('',#16862);
#1615=PLANE('',#16871);
#1616=PLANE('',#16873);
#1617=PLANE('',#16880);
#1618=PLANE('',#16885);
#1619=PLANE('',#16888);
#1620=PLANE('',#16891);
#1621=PLANE('',#16894);
#1622=PLANE('',#16897);
#1623=PLANE('',#16900);
#1624=PLANE('',#16903);
#1625=PLANE('',#16907);
#1626=PLANE('',#16909);
#1627=PLANE('',#16913);
#1628=PLANE('',#16915);
#1629=PLANE('',#16918);
#1630=PLANE('',#16921);
#1631=PLANE('',#16924);
#1632=PLANE('',#16927);
#1633=PLANE('',#16930);
#1634=PLANE('',#16932);
#1635=PLANE('',#16940);
#1636=PLANE('',#16947);
#1637=PLANE('',#16952);
#1638=PLANE('',#16957);
#1639=PLANE('',#16962);
#1640=PLANE('',#16974);
#1641=PLANE('',#16977);
#1642=PLANE('',#16980);
#1643=PLANE('',#16983);
#1644=PLANE('',#16996);
#1645=PLANE('',#16997);
#1646=PLANE('',#16998);
#1647=PLANE('',#16999);
#1648=PLANE('',#17000);
#1649=PLANE('',#17001);
#1650=PLANE('',#17002);
#1651=PLANE('',#17003);
#1652=PLANE('',#17004);
#1653=PLANE('',#17005);
#1654=PLANE('',#17019);
#1655=PLANE('',#17020);
#1656=PLANE('',#17021);
#1657=PLANE('',#17022);
#1658=PLANE('',#17026);
#1659=PLANE('',#17030);
#1660=PLANE('',#17034);
#1661=PLANE('',#17038);
#1662=PLANE('',#17039);
#1663=PLANE('',#17046);
#1664=PLANE('',#17055);
#1665=PLANE('',#17057);
#1666=PLANE('',#17066);
#1667=PLANE('',#17073);
#1668=PLANE('',#17076);
#1669=PLANE('',#17077);
#1670=PLANE('',#17080);
#1671=PLANE('',#17083);
#1672=PLANE('',#17086);
#1673=PLANE('',#17089);
#1674=PLANE('',#17090);
#1675=PLANE('',#17098);
#1676=PLANE('',#17101);
#1677=PLANE('',#17102);
#1678=PLANE('',#17105);
#1679=PLANE('',#17108);
#1680=PLANE('',#17111);
#1681=PLANE('',#17114);
#1682=PLANE('',#17117);
#1683=PLANE('',#17121);
#1684=PLANE('',#17126);
#1685=PLANE('',#17127);
#1686=PLANE('',#17135);
#1687=PLANE('',#17138);
#1688=PLANE('',#17141);
#1689=PLANE('',#17144);
#1690=PLANE('',#17157);
#1691=PLANE('',#17158);
#1692=PLANE('',#17159);
#1693=PLANE('',#17160);
#1694=PLANE('',#17161);
#1695=PLANE('',#17162);
#1696=PLANE('',#17163);
#1697=PLANE('',#17164);
#1698=PLANE('',#17165);
#1699=PLANE('',#17166);
#1700=PLANE('',#17171);
#1701=PLANE('',#17172);
#1702=PLANE('',#17177);
#1703=PLANE('',#17178);
#1704=PLANE('',#17183);
#1705=PLANE('',#17184);
#1706=PLANE('',#17189);
#1707=PLANE('',#17190);
#1708=PLANE('',#17204);
#1709=PLANE('',#17221);
#1710=PLANE('',#17224);
#1711=PLANE('',#17238);
#1712=PLANE('',#17254);
#1713=PLANE('',#17258);
#1714=PLANE('',#17275);
#1715=PLANE('',#17282);
#1716=PLANE('',#17283);
#1717=PLANE('',#17300);
#1718=PLANE('',#17307);
#1719=PLANE('',#17308);
#1720=PLANE('',#17325);
#1721=PLANE('',#17332);
#1722=PLANE('',#17333);
#1723=PLANE('',#17350);
#1724=PLANE('',#17357);
#1725=PLANE('',#17358);
#1726=PLANE('',#17372);
#1727=PLANE('',#17373);
#1728=PLANE('',#17374);
#1729=PLANE('',#17375);
#1730=PLANE('',#17376);
#1731=PLANE('',#17377);
#1732=PLANE('',#17379);
#1733=PLANE('',#17380);
#1734=PLANE('',#17381);
#1735=PLANE('',#17382);
#1736=PLANE('',#17383);
#1737=PLANE('',#17384);
#1738=PLANE('',#17386);
#1739=PLANE('',#17387);
#1740=PLANE('',#17388);
#1741=PLANE('',#17389);
#1742=PLANE('',#17390);
#1743=PLANE('',#17391);
#1744=PLANE('',#17393);
#1745=PLANE('',#17394);
#1746=PLANE('',#17395);
#1747=PLANE('',#17396);
#1748=PLANE('',#17397);
#1749=PLANE('',#17398);
#1750=PLANE('',#17399);
#1751=PLANE('',#17400);
#1752=PLANE('',#17401);
#1753=PLANE('',#17403);
#1754=PLANE('',#17411);
#1755=PLANE('',#17431);
#1756=PLANE('',#17434);
#1757=PLANE('',#17446);
#1758=PLANE('',#17455);
#1759=PLANE('',#17486);
#1760=PLANE('',#17491);
#1761=PLANE('',#17496);
#1762=PLANE('',#17502);
#1763=PLANE('',#17507);
#1764=PLANE('',#17516);
#1765=PLANE('',#17520);
#1766=PLANE('',#17521);
#1767=PLANE('',#17523);
#1768=PLANE('',#17528);
#1769=PLANE('',#17531);
#1770=PLANE('',#17536);
#1771=PLANE('',#17559);
#1772=PLANE('',#17562);
#1773=PLANE('',#17574);
#1774=PLANE('',#17583);
#1775=PLANE('',#17616);
#1776=PLANE('',#17621);
#1777=PLANE('',#17626);
#1778=PLANE('',#17631);
#1779=PLANE('',#17636);
#1780=PLANE('',#17641);
#1781=PLANE('',#17650);
#1782=PLANE('',#17654);
#1783=PLANE('',#17655);
#1784=PLANE('',#17657);
#1785=PLANE('',#17662);
#1786=PLANE('',#17665);
#1787=PLANE('',#17670);
#1788=PLANE('',#17679);
#1789=PLANE('',#17687);
#1790=PLANE('',#17695);
#1791=PLANE('',#17696);
#1792=PLANE('',#17697);
#1793=PLANE('',#17698);
#1794=PLANE('',#17699);
#1795=PLANE('',#17700);
#1796=PLANE('',#17701);
#1797=PLANE('',#17702);
#1798=PLANE('',#17703);
#1799=PLANE('',#17766);
#1800=PLANE('',#17767);
#1801=PLANE('',#17769);
#1802=PLANE('',#17770);
#1803=PLANE('',#17771);
#1804=PLANE('',#17776);
#1805=PLANE('',#17777);
#1806=PLANE('',#17779);
#1807=PLANE('',#17784);
#1808=PLANE('',#17791);
#1809=PLANE('',#17792);
#1810=PLANE('',#17794);
#1811=PLANE('',#17799);
#1812=PLANE('',#17806);
#1813=PLANE('',#17807);
#1814=PLANE('',#17815);
#1815=PLANE('',#17816);
#1816=PLANE('',#17824);
#1817=PLANE('',#17825);
#1818=PLANE('',#17833);
#1819=PLANE('',#17834);
#1820=PLANE('',#17842);
#1821=PLANE('',#17843);
#1822=PLANE('',#17845);
#1823=PLANE('',#17846);
#1824=PLANE('',#17847);
#1825=PLANE('',#17848);
#1826=PLANE('',#17875);
#1827=PLANE('',#17876);
#1828=PLANE('',#17879);
#1829=PLANE('',#17882);
#1830=PLANE('',#17885);
#1831=PLANE('',#17888);
#1832=PLANE('',#17891);
#1833=PLANE('',#17894);
#1834=PLANE('',#17897);
#1835=PLANE('',#17900);
#1836=PLANE('',#17903);
#1837=PLANE('',#17906);
#1838=PLANE('',#17909);
#1839=PLANE('',#17912);
#1840=PLANE('',#17915);
#1841=PLANE('',#17918);
#1842=PLANE('',#17921);
#1843=PLANE('',#17924);
#1844=PLANE('',#17927);
#1845=PLANE('',#17930);
#1846=PLANE('',#17933);
#1847=PLANE('',#17934);
#1848=PLANE('',#17938);
#1849=PLANE('',#17939);
#1850=PLANE('',#17940);
#1851=PLANE('',#17941);
#1852=PLANE('',#17942);
#1853=PLANE('',#17943);
#1854=PLANE('',#17944);
#1855=PLANE('',#17945);
#1856=PLANE('',#17946);
#1857=PLANE('',#17947);
#1858=PLANE('',#17950);
#1859=PLANE('',#17951);
#1860=PLANE('',#17953);
#1861=PLANE('',#17954);
#1862=PLANE('',#17955);
#1863=PLANE('',#17957);
#1864=PLANE('',#17958);
#1865=PLANE('',#17960);
#1866=PLANE('',#17961);
#1867=PLANE('',#17962);
#1868=PLANE('',#17967);
#1869=PLANE('',#17968);
#1870=PLANE('',#17970);
#1871=PLANE('',#17975);
#1872=PLANE('',#17982);
#1873=PLANE('',#17983);
#1874=PLANE('',#17985);
#1875=PLANE('',#17990);
#1876=PLANE('',#17997);
#1877=PLANE('',#17998);
#1878=PLANE('',#18006);
#1879=PLANE('',#18007);
#1880=PLANE('',#18015);
#1881=PLANE('',#18016);
#1882=PLANE('',#18024);
#1883=PLANE('',#18025);
#1884=PLANE('',#18033);
#1885=PLANE('',#18034);
#1886=PLANE('',#18042);
#1887=PLANE('',#18043);
#1888=PLANE('',#18045);
#1889=PLANE('',#18046);
#1890=PLANE('',#18047);
#1891=PLANE('',#18048);
#1892=PLANE('',#18053);
#1893=PLANE('',#18076);
#1894=PLANE('',#18079);
#1895=PLANE('',#18082);
#1896=PLANE('',#18085);
#1897=PLANE('',#18088);
#1898=PLANE('',#18091);
#1899=PLANE('',#18094);
#1900=PLANE('',#18097);
#1901=PLANE('',#18100);
#1902=PLANE('',#18103);
#1903=PLANE('',#18106);
#1904=PLANE('',#18109);
#1905=PLANE('',#18112);
#1906=PLANE('',#18115);
#1907=PLANE('',#18118);
#1908=PLANE('',#18121);
#1909=PLANE('',#18124);
#1910=PLANE('',#18127);
#1911=PLANE('',#18130);
#1912=PLANE('',#18133);
#1913=PLANE('',#18134);
#1914=PLANE('',#18139);
#1915=PLANE('',#18140);
#1916=PLANE('',#18142);
#1917=PLANE('',#18143);
#1918=PLANE('',#18144);
#1919=PLANE('',#18149);
#1920=PLANE('',#18150);
#1921=PLANE('',#18152);
#1922=PLANE('',#18157);
#1923=PLANE('',#18164);
#1924=PLANE('',#18165);
#1925=PLANE('',#18167);
#1926=PLANE('',#18172);
#1927=PLANE('',#18179);
#1928=PLANE('',#18180);
#1929=PLANE('',#18188);
#1930=PLANE('',#18189);
#1931=PLANE('',#18197);
#1932=PLANE('',#18198);
#1933=PLANE('',#18206);
#1934=PLANE('',#18207);
#1935=PLANE('',#18215);
#1936=PLANE('',#18216);
#1937=PLANE('',#18218);
#1938=PLANE('',#18219);
#1939=PLANE('',#18220);
#1940=PLANE('',#18221);
#1941=PLANE('',#18222);
#1942=PLANE('',#18223);
#1943=PLANE('',#18224);
#1944=PLANE('',#18225);
#1945=PLANE('',#18233);
#1946=PLANE('',#18246);
#1947=PLANE('',#18247);
#1948=PLANE('',#18248);
#1949=PLANE('',#18249);
#1950=PLANE('',#18296);
#1951=PLANE('',#18297);
#1952=PLANE('',#18300);
#1953=PLANE('',#18303);
#1954=PLANE('',#18306);
#1955=PLANE('',#18309);
#1956=PLANE('',#18312);
#1957=PLANE('',#18315);
#1958=PLANE('',#18318);
#1959=PLANE('',#18321);
#1960=PLANE('',#18324);
#1961=PLANE('',#18327);
#1962=PLANE('',#18330);
#1963=PLANE('',#18333);
#1964=PLANE('',#18336);
#1965=PLANE('',#18339);
#1966=PLANE('',#18342);
#1967=PLANE('',#18345);
#1968=PLANE('',#18348);
#1969=PLANE('',#18351);
#1970=PLANE('',#18354);
#1971=PLANE('',#18357);
#1972=PLANE('',#18360);
#1973=PLANE('',#18363);
#1974=PLANE('',#18366);
#1975=PLANE('',#18369);
#1976=PLANE('',#18372);
#1977=PLANE('',#18375);
#1978=PLANE('',#18378);
#1979=PLANE('',#18381);
#1980=PLANE('',#18384);
#1981=PLANE('',#18387);
#1982=PLANE('',#18390);
#1983=PLANE('',#18393);
#1984=PLANE('',#18396);
#1985=PLANE('',#18399);
#1986=PLANE('',#18402);
#1987=PLANE('',#18405);
#1988=PLANE('',#18408);
#1989=PLANE('',#18411);
#1990=PLANE('',#18414);
#1991=PLANE('',#18415);
#1992=PLANE('',#18419);
#1993=PLANE('',#18420);
#1994=PLANE('',#18421);
#1995=PLANE('',#18422);
#1996=PLANE('',#18423);
#1997=PLANE('',#18424);
#1998=PLANE('',#18425);
#1999=PLANE('',#18426);
#2000=PLANE('',#18427);
#2001=PLANE('',#18428);
#2002=FACE_OUTER_BOUND('',#2915,.T.);
#2003=FACE_OUTER_BOUND('',#2916,.T.);
#2004=FACE_OUTER_BOUND('',#2917,.T.);
#2005=FACE_OUTER_BOUND('',#2918,.T.);
#2006=FACE_OUTER_BOUND('',#2919,.T.);
#2007=FACE_OUTER_BOUND('',#2920,.T.);
#2008=FACE_OUTER_BOUND('',#2921,.T.);
#2009=FACE_OUTER_BOUND('',#2922,.T.);
#2010=FACE_OUTER_BOUND('',#2923,.T.);
#2011=FACE_OUTER_BOUND('',#2928,.T.);
#2012=FACE_OUTER_BOUND('',#2933,.T.);
#2013=FACE_OUTER_BOUND('',#2934,.T.);
#2014=FACE_OUTER_BOUND('',#2935,.T.);
#2015=FACE_OUTER_BOUND('',#2936,.T.);
#2016=FACE_OUTER_BOUND('',#2937,.T.);
#2017=FACE_OUTER_BOUND('',#2938,.T.);
#2018=FACE_OUTER_BOUND('',#2939,.T.);
#2019=FACE_OUTER_BOUND('',#2940,.T.);
#2020=FACE_OUTER_BOUND('',#2941,.T.);
#2021=FACE_OUTER_BOUND('',#2942,.T.);
#2022=FACE_OUTER_BOUND('',#2943,.T.);
#2023=FACE_OUTER_BOUND('',#2950,.T.);
#2024=FACE_OUTER_BOUND('',#2956,.T.);
#2025=FACE_OUTER_BOUND('',#2957,.T.);
#2026=FACE_OUTER_BOUND('',#2958,.T.);
#2027=FACE_OUTER_BOUND('',#2965,.T.);
#2028=FACE_OUTER_BOUND('',#2966,.T.);
#2029=FACE_OUTER_BOUND('',#2967,.T.);
#2030=FACE_OUTER_BOUND('',#2968,.T.);
#2031=FACE_OUTER_BOUND('',#2969,.T.);
#2032=FACE_OUTER_BOUND('',#2970,.T.);
#2033=FACE_OUTER_BOUND('',#2971,.T.);
#2034=FACE_OUTER_BOUND('',#2972,.T.);
#2035=FACE_OUTER_BOUND('',#2973,.T.);
#2036=FACE_OUTER_BOUND('',#2974,.T.);
#2037=FACE_OUTER_BOUND('',#2975,.T.);
#2038=FACE_OUTER_BOUND('',#2976,.T.);
#2039=FACE_OUTER_BOUND('',#2977,.T.);
#2040=FACE_OUTER_BOUND('',#2978,.T.);
#2041=FACE_OUTER_BOUND('',#2979,.T.);
#2042=FACE_OUTER_BOUND('',#2980,.T.);
#2043=FACE_OUTER_BOUND('',#2981,.T.);
#2044=FACE_OUTER_BOUND('',#2982,.T.);
#2045=FACE_OUTER_BOUND('',#2983,.T.);
#2046=FACE_OUTER_BOUND('',#2984,.T.);
#2047=FACE_OUTER_BOUND('',#2985,.T.);
#2048=FACE_OUTER_BOUND('',#2986,.T.);
#2049=FACE_OUTER_BOUND('',#2987,.T.);
#2050=FACE_OUTER_BOUND('',#2988,.T.);
#2051=FACE_OUTER_BOUND('',#2989,.T.);
#2052=FACE_OUTER_BOUND('',#2990,.T.);
#2053=FACE_OUTER_BOUND('',#2991,.T.);
#2054=FACE_OUTER_BOUND('',#2992,.T.);
#2055=FACE_OUTER_BOUND('',#2993,.T.);
#2056=FACE_OUTER_BOUND('',#2994,.T.);
#2057=FACE_OUTER_BOUND('',#2995,.T.);
#2058=FACE_OUTER_BOUND('',#2996,.T.);
#2059=FACE_OUTER_BOUND('',#2997,.T.);
#2060=FACE_OUTER_BOUND('',#3003,.T.);
#2061=FACE_OUTER_BOUND('',#3004,.T.);
#2062=FACE_OUTER_BOUND('',#3005,.T.);
#2063=FACE_OUTER_BOUND('',#3006,.T.);
#2064=FACE_OUTER_BOUND('',#3007,.T.);
#2065=FACE_OUTER_BOUND('',#3008,.T.);
#2066=FACE_OUTER_BOUND('',#3010,.T.);
#2067=FACE_OUTER_BOUND('',#3011,.T.);
#2068=FACE_OUTER_BOUND('',#3013,.T.);
#2069=FACE_OUTER_BOUND('',#3014,.T.);
#2070=FACE_OUTER_BOUND('',#3016,.T.);
#2071=FACE_OUTER_BOUND('',#3017,.T.);
#2072=FACE_OUTER_BOUND('',#3019,.T.);
#2073=FACE_OUTER_BOUND('',#3020,.T.);
#2074=FACE_OUTER_BOUND('',#3021,.T.);
#2075=FACE_OUTER_BOUND('',#3022,.T.);
#2076=FACE_OUTER_BOUND('',#3023,.T.);
#2077=FACE_OUTER_BOUND('',#3024,.T.);
#2078=FACE_OUTER_BOUND('',#3025,.T.);
#2079=FACE_OUTER_BOUND('',#3026,.T.);
#2080=FACE_OUTER_BOUND('',#3027,.T.);
#2081=FACE_OUTER_BOUND('',#3028,.T.);
#2082=FACE_OUTER_BOUND('',#3029,.T.);
#2083=FACE_OUTER_BOUND('',#3030,.T.);
#2084=FACE_OUTER_BOUND('',#3031,.T.);
#2085=FACE_OUTER_BOUND('',#3032,.T.);
#2086=FACE_OUTER_BOUND('',#3033,.T.);
#2087=FACE_OUTER_BOUND('',#3034,.T.);
#2088=FACE_OUTER_BOUND('',#3035,.T.);
#2089=FACE_OUTER_BOUND('',#3036,.T.);
#2090=FACE_OUTER_BOUND('',#3037,.T.);
#2091=FACE_OUTER_BOUND('',#3038,.T.);
#2092=FACE_OUTER_BOUND('',#3042,.T.);
#2093=FACE_OUTER_BOUND('',#3043,.T.);
#2094=FACE_OUTER_BOUND('',#3044,.T.);
#2095=FACE_OUTER_BOUND('',#3048,.T.);
#2096=FACE_OUTER_BOUND('',#3049,.T.);
#2097=FACE_OUTER_BOUND('',#3050,.T.);
#2098=FACE_OUTER_BOUND('',#3055,.T.);
#2099=FACE_OUTER_BOUND('',#3056,.T.);
#2100=FACE_OUTER_BOUND('',#3061,.T.);
#2101=FACE_OUTER_BOUND('',#3062,.T.);
#2102=FACE_OUTER_BOUND('',#3063,.T.);
#2103=FACE_OUTER_BOUND('',#3064,.T.);
#2104=FACE_OUTER_BOUND('',#3065,.T.);
#2105=FACE_OUTER_BOUND('',#3066,.T.);
#2106=FACE_OUTER_BOUND('',#3067,.T.);
#2107=FACE_OUTER_BOUND('',#3068,.T.);
#2108=FACE_OUTER_BOUND('',#3069,.T.);
#2109=FACE_OUTER_BOUND('',#3070,.T.);
#2110=FACE_OUTER_BOUND('',#3071,.T.);
#2111=FACE_OUTER_BOUND('',#3072,.T.);
#2112=FACE_OUTER_BOUND('',#3073,.T.);
#2113=FACE_OUTER_BOUND('',#3074,.T.);
#2114=FACE_OUTER_BOUND('',#3075,.T.);
#2115=FACE_OUTER_BOUND('',#3076,.T.);
#2116=FACE_OUTER_BOUND('',#3077,.T.);
#2117=FACE_OUTER_BOUND('',#3078,.T.);
#2118=FACE_OUTER_BOUND('',#3079,.T.);
#2119=FACE_OUTER_BOUND('',#3080,.T.);
#2120=FACE_OUTER_BOUND('',#3086,.T.);
#2121=FACE_OUTER_BOUND('',#3087,.T.);
#2122=FACE_OUTER_BOUND('',#3088,.T.);
#2123=FACE_OUTER_BOUND('',#3095,.T.);
#2124=FACE_OUTER_BOUND('',#3096,.T.);
#2125=FACE_OUTER_BOUND('',#3103,.T.);
#2126=FACE_OUTER_BOUND('',#3104,.T.);
#2127=FACE_OUTER_BOUND('',#3105,.T.);
#2128=FACE_OUTER_BOUND('',#3106,.T.);
#2129=FACE_OUTER_BOUND('',#3107,.T.);
#2130=FACE_OUTER_BOUND('',#3108,.T.);
#2131=FACE_OUTER_BOUND('',#3109,.T.);
#2132=FACE_OUTER_BOUND('',#3110,.T.);
#2133=FACE_OUTER_BOUND('',#3111,.T.);
#2134=FACE_OUTER_BOUND('',#3112,.T.);
#2135=FACE_OUTER_BOUND('',#3113,.T.);
#2136=FACE_OUTER_BOUND('',#3114,.T.);
#2137=FACE_OUTER_BOUND('',#3115,.T.);
#2138=FACE_OUTER_BOUND('',#3116,.T.);
#2139=FACE_OUTER_BOUND('',#3117,.T.);
#2140=FACE_OUTER_BOUND('',#3118,.T.);
#2141=FACE_OUTER_BOUND('',#3119,.T.);
#2142=FACE_OUTER_BOUND('',#3120,.T.);
#2143=FACE_OUTER_BOUND('',#3121,.T.);
#2144=FACE_OUTER_BOUND('',#3122,.T.);
#2145=FACE_OUTER_BOUND('',#3123,.T.);
#2146=FACE_OUTER_BOUND('',#3124,.T.);
#2147=FACE_OUTER_BOUND('',#3125,.T.);
#2148=FACE_OUTER_BOUND('',#3126,.T.);
#2149=FACE_OUTER_BOUND('',#3127,.T.);
#2150=FACE_OUTER_BOUND('',#3128,.T.);
#2151=FACE_OUTER_BOUND('',#3129,.T.);
#2152=FACE_OUTER_BOUND('',#3130,.T.);
#2153=FACE_OUTER_BOUND('',#3131,.T.);
#2154=FACE_OUTER_BOUND('',#3132,.T.);
#2155=FACE_OUTER_BOUND('',#3133,.T.);
#2156=FACE_OUTER_BOUND('',#3134,.T.);
#2157=FACE_OUTER_BOUND('',#3135,.T.);
#2158=FACE_OUTER_BOUND('',#3136,.T.);
#2159=FACE_OUTER_BOUND('',#3137,.T.);
#2160=FACE_OUTER_BOUND('',#3143,.T.);
#2161=FACE_OUTER_BOUND('',#3144,.T.);
#2162=FACE_OUTER_BOUND('',#3145,.T.);
#2163=FACE_OUTER_BOUND('',#3146,.T.);
#2164=FACE_OUTER_BOUND('',#3147,.T.);
#2165=FACE_OUTER_BOUND('',#3148,.T.);
#2166=FACE_OUTER_BOUND('',#3149,.T.);
#2167=FACE_OUTER_BOUND('',#3150,.T.);
#2168=FACE_OUTER_BOUND('',#3151,.T.);
#2169=FACE_OUTER_BOUND('',#3152,.T.);
#2170=FACE_OUTER_BOUND('',#3153,.T.);
#2171=FACE_OUTER_BOUND('',#3154,.T.);
#2172=FACE_OUTER_BOUND('',#3155,.T.);
#2173=FACE_OUTER_BOUND('',#3156,.T.);
#2174=FACE_OUTER_BOUND('',#3157,.T.);
#2175=FACE_OUTER_BOUND('',#3158,.T.);
#2176=FACE_OUTER_BOUND('',#3162,.T.);
#2177=FACE_OUTER_BOUND('',#3163,.T.);
#2178=FACE_OUTER_BOUND('',#3167,.T.);
#2179=FACE_OUTER_BOUND('',#3168,.T.);
#2180=FACE_OUTER_BOUND('',#3169,.T.);
#2181=FACE_OUTER_BOUND('',#3170,.T.);
#2182=FACE_OUTER_BOUND('',#3176,.T.);
#2183=FACE_OUTER_BOUND('',#3177,.T.);
#2184=FACE_OUTER_BOUND('',#3183,.T.);
#2185=FACE_OUTER_BOUND('',#3184,.T.);
#2186=FACE_OUTER_BOUND('',#3185,.T.);
#2187=FACE_OUTER_BOUND('',#3186,.T.);
#2188=FACE_OUTER_BOUND('',#3187,.T.);
#2189=FACE_OUTER_BOUND('',#3188,.T.);
#2190=FACE_OUTER_BOUND('',#3189,.T.);
#2191=FACE_OUTER_BOUND('',#3190,.T.);
#2192=FACE_OUTER_BOUND('',#3191,.T.);
#2193=FACE_OUTER_BOUND('',#3192,.T.);
#2194=FACE_OUTER_BOUND('',#3193,.T.);
#2195=FACE_OUTER_BOUND('',#3194,.T.);
#2196=FACE_OUTER_BOUND('',#3195,.T.);
#2197=FACE_OUTER_BOUND('',#3196,.T.);
#2198=FACE_OUTER_BOUND('',#3197,.T.);
#2199=FACE_OUTER_BOUND('',#3198,.T.);
#2200=FACE_OUTER_BOUND('',#3199,.T.);
#2201=FACE_OUTER_BOUND('',#3201,.T.);
#2202=FACE_OUTER_BOUND('',#3202,.T.);
#2203=FACE_OUTER_BOUND('',#3203,.T.);
#2204=FACE_OUTER_BOUND('',#3204,.T.);
#2205=FACE_OUTER_BOUND('',#3205,.T.);
#2206=FACE_OUTER_BOUND('',#3206,.T.);
#2207=FACE_OUTER_BOUND('',#3208,.T.);
#2208=FACE_OUTER_BOUND('',#3209,.T.);
#2209=FACE_OUTER_BOUND('',#3211,.T.);
#2210=FACE_OUTER_BOUND('',#3212,.T.);
#2211=FACE_OUTER_BOUND('',#3213,.T.);
#2212=FACE_OUTER_BOUND('',#3214,.T.);
#2213=FACE_OUTER_BOUND('',#3215,.T.);
#2214=FACE_OUTER_BOUND('',#3217,.T.);
#2215=FACE_OUTER_BOUND('',#3218,.T.);
#2216=FACE_OUTER_BOUND('',#3219,.T.);
#2217=FACE_OUTER_BOUND('',#3220,.T.);
#2218=FACE_OUTER_BOUND('',#3221,.T.);
#2219=FACE_OUTER_BOUND('',#3222,.T.);
#2220=FACE_OUTER_BOUND('',#3224,.T.);
#2221=FACE_OUTER_BOUND('',#3225,.T.);
#2222=FACE_OUTER_BOUND('',#3227,.T.);
#2223=FACE_OUTER_BOUND('',#3228,.T.);
#2224=FACE_OUTER_BOUND('',#3229,.T.);
#2225=FACE_OUTER_BOUND('',#3230,.T.);
#2226=FACE_OUTER_BOUND('',#3231,.T.);
#2227=FACE_OUTER_BOUND('',#3232,.T.);
#2228=FACE_OUTER_BOUND('',#3234,.T.);
#2229=FACE_OUTER_BOUND('',#3235,.T.);
#2230=FACE_OUTER_BOUND('',#3236,.T.);
#2231=FACE_OUTER_BOUND('',#3242,.T.);
#2232=FACE_OUTER_BOUND('',#3248,.T.);
#2233=FACE_OUTER_BOUND('',#3249,.T.);
#2234=FACE_OUTER_BOUND('',#3250,.T.);
#2235=FACE_OUTER_BOUND('',#3251,.T.);
#2236=FACE_OUTER_BOUND('',#3252,.T.);
#2237=FACE_OUTER_BOUND('',#3253,.T.);
#2238=FACE_OUTER_BOUND('',#3255,.T.);
#2239=FACE_OUTER_BOUND('',#3256,.T.);
#2240=FACE_OUTER_BOUND('',#3257,.T.);
#2241=FACE_OUTER_BOUND('',#3263,.T.);
#2242=FACE_OUTER_BOUND('',#3269,.T.);
#2243=FACE_OUTER_BOUND('',#3270,.T.);
#2244=FACE_OUTER_BOUND('',#3271,.T.);
#2245=FACE_OUTER_BOUND('',#3272,.T.);
#2246=FACE_OUTER_BOUND('',#3273,.T.);
#2247=FACE_OUTER_BOUND('',#3274,.T.);
#2248=FACE_OUTER_BOUND('',#3276,.T.);
#2249=FACE_OUTER_BOUND('',#3277,.T.);
#2250=FACE_OUTER_BOUND('',#3278,.T.);
#2251=FACE_OUTER_BOUND('',#3284,.T.);
#2252=FACE_OUTER_BOUND('',#3290,.T.);
#2253=FACE_OUTER_BOUND('',#3291,.T.);
#2254=FACE_OUTER_BOUND('',#3292,.T.);
#2255=FACE_OUTER_BOUND('',#3293,.T.);
#2256=FACE_OUTER_BOUND('',#3294,.T.);
#2257=FACE_OUTER_BOUND('',#3295,.T.);
#2258=FACE_OUTER_BOUND('',#3297,.T.);
#2259=FACE_OUTER_BOUND('',#3298,.T.);
#2260=FACE_OUTER_BOUND('',#3299,.T.);
#2261=FACE_OUTER_BOUND('',#3305,.T.);
#2262=FACE_OUTER_BOUND('',#3311,.T.);
#2263=FACE_OUTER_BOUND('',#3312,.T.);
#2264=FACE_OUTER_BOUND('',#3313,.T.);
#2265=FACE_OUTER_BOUND('',#3314,.T.);
#2266=FACE_OUTER_BOUND('',#3315,.T.);
#2267=FACE_OUTER_BOUND('',#3316,.T.);
#2268=FACE_OUTER_BOUND('',#3317,.T.);
#2269=FACE_OUTER_BOUND('',#3318,.T.);
#2270=FACE_OUTER_BOUND('',#3319,.T.);
#2271=FACE_OUTER_BOUND('',#3324,.T.);
#2272=FACE_OUTER_BOUND('',#3329,.T.);
#2273=FACE_OUTER_BOUND('',#3330,.T.);
#2274=FACE_OUTER_BOUND('',#3331,.T.);
#2275=FACE_OUTER_BOUND('',#3332,.T.);
#2276=FACE_OUTER_BOUND('',#3333,.T.);
#2277=FACE_OUTER_BOUND('',#3334,.T.);
#2278=FACE_OUTER_BOUND('',#3335,.T.);
#2279=FACE_OUTER_BOUND('',#3336,.T.);
#2280=FACE_OUTER_BOUND('',#3337,.T.);
#2281=FACE_OUTER_BOUND('',#3338,.T.);
#2282=FACE_OUTER_BOUND('',#3339,.T.);
#2283=FACE_OUTER_BOUND('',#3340,.T.);
#2284=FACE_OUTER_BOUND('',#3341,.T.);
#2285=FACE_OUTER_BOUND('',#3342,.T.);
#2286=FACE_OUTER_BOUND('',#3343,.T.);
#2287=FACE_OUTER_BOUND('',#3344,.T.);
#2288=FACE_OUTER_BOUND('',#3345,.T.);
#2289=FACE_OUTER_BOUND('',#3346,.T.);
#2290=FACE_OUTER_BOUND('',#3347,.T.);
#2291=FACE_OUTER_BOUND('',#3348,.T.);
#2292=FACE_OUTER_BOUND('',#3349,.T.);
#2293=FACE_OUTER_BOUND('',#3350,.T.);
#2294=FACE_OUTER_BOUND('',#3351,.T.);
#2295=FACE_OUTER_BOUND('',#3352,.T.);
#2296=FACE_OUTER_BOUND('',#3353,.T.);
#2297=FACE_OUTER_BOUND('',#3354,.T.);
#2298=FACE_OUTER_BOUND('',#3356,.T.);
#2299=FACE_OUTER_BOUND('',#3357,.T.);
#2300=FACE_OUTER_BOUND('',#3358,.T.);
#2301=FACE_OUTER_BOUND('',#3359,.T.);
#2302=FACE_OUTER_BOUND('',#3360,.T.);
#2303=FACE_OUTER_BOUND('',#3361,.T.);
#2304=FACE_OUTER_BOUND('',#3362,.T.);
#2305=FACE_OUTER_BOUND('',#3364,.T.);
#2306=FACE_OUTER_BOUND('',#3365,.T.);
#2307=FACE_OUTER_BOUND('',#3367,.T.);
#2308=FACE_OUTER_BOUND('',#3368,.T.);
#2309=FACE_OUTER_BOUND('',#3369,.T.);
#2310=FACE_OUTER_BOUND('',#3370,.T.);
#2311=FACE_OUTER_BOUND('',#3372,.T.);
#2312=FACE_OUTER_BOUND('',#3373,.T.);
#2313=FACE_OUTER_BOUND('',#3374,.T.);
#2314=FACE_OUTER_BOUND('',#3375,.T.);
#2315=FACE_OUTER_BOUND('',#3377,.T.);
#2316=FACE_OUTER_BOUND('',#3378,.T.);
#2317=FACE_OUTER_BOUND('',#3379,.T.);
#2318=FACE_OUTER_BOUND('',#3380,.T.);
#2319=FACE_OUTER_BOUND('',#3381,.T.);
#2320=FACE_OUTER_BOUND('',#3382,.T.);
#2321=FACE_OUTER_BOUND('',#3383,.T.);
#2322=FACE_OUTER_BOUND('',#3384,.T.);
#2323=FACE_OUTER_BOUND('',#3385,.T.);
#2324=FACE_OUTER_BOUND('',#3386,.T.);
#2325=FACE_OUTER_BOUND('',#3387,.T.);
#2326=FACE_OUTER_BOUND('',#3388,.T.);
#2327=FACE_OUTER_BOUND('',#3389,.T.);
#2328=FACE_OUTER_BOUND('',#3390,.T.);
#2329=FACE_OUTER_BOUND('',#3391,.T.);
#2330=FACE_OUTER_BOUND('',#3392,.T.);
#2331=FACE_OUTER_BOUND('',#3393,.T.);
#2332=FACE_OUTER_BOUND('',#3394,.T.);
#2333=FACE_OUTER_BOUND('',#3395,.T.);
#2334=FACE_OUTER_BOUND('',#3396,.T.);
#2335=FACE_OUTER_BOUND('',#3397,.T.);
#2336=FACE_OUTER_BOUND('',#3398,.T.);
#2337=FACE_OUTER_BOUND('',#3399,.T.);
#2338=FACE_OUTER_BOUND('',#3400,.T.);
#2339=FACE_OUTER_BOUND('',#3402,.T.);
#2340=FACE_OUTER_BOUND('',#3403,.T.);
#2341=FACE_OUTER_BOUND('',#3405,.T.);
#2342=FACE_OUTER_BOUND('',#3406,.T.);
#2343=FACE_OUTER_BOUND('',#3408,.T.);
#2344=FACE_OUTER_BOUND('',#3409,.T.);
#2345=FACE_OUTER_BOUND('',#3411,.T.);
#2346=FACE_OUTER_BOUND('',#3412,.T.);
#2347=FACE_OUTER_BOUND('',#3414,.T.);
#2348=FACE_OUTER_BOUND('',#3415,.T.);
#2349=FACE_OUTER_BOUND('',#3416,.T.);
#2350=FACE_OUTER_BOUND('',#3417,.T.);
#2351=FACE_OUTER_BOUND('',#3418,.T.);
#2352=FACE_OUTER_BOUND('',#3419,.T.);
#2353=FACE_OUTER_BOUND('',#3421,.T.);
#2354=FACE_OUTER_BOUND('',#3422,.T.);
#2355=FACE_OUTER_BOUND('',#3424,.T.);
#2356=FACE_OUTER_BOUND('',#3425,.T.);
#2357=FACE_OUTER_BOUND('',#3426,.T.);
#2358=FACE_OUTER_BOUND('',#3427,.T.);
#2359=FACE_OUTER_BOUND('',#3429,.T.);
#2360=FACE_OUTER_BOUND('',#3430,.T.);
#2361=FACE_OUTER_BOUND('',#3431,.T.);
#2362=FACE_OUTER_BOUND('',#3432,.T.);
#2363=FACE_OUTER_BOUND('',#3434,.T.);
#2364=FACE_OUTER_BOUND('',#3435,.T.);
#2365=FACE_OUTER_BOUND('',#3436,.T.);
#2366=FACE_OUTER_BOUND('',#3437,.T.);
#2367=FACE_OUTER_BOUND('',#3438,.T.);
#2368=FACE_OUTER_BOUND('',#3439,.T.);
#2369=FACE_OUTER_BOUND('',#3440,.T.);
#2370=FACE_OUTER_BOUND('',#3441,.T.);
#2371=FACE_OUTER_BOUND('',#3442,.T.);
#2372=FACE_OUTER_BOUND('',#3443,.T.);
#2373=FACE_OUTER_BOUND('',#3444,.T.);
#2374=FACE_OUTER_BOUND('',#3445,.T.);
#2375=FACE_OUTER_BOUND('',#3446,.T.);
#2376=FACE_OUTER_BOUND('',#3447,.T.);
#2377=FACE_OUTER_BOUND('',#3448,.T.);
#2378=FACE_OUTER_BOUND('',#3449,.T.);
#2379=FACE_OUTER_BOUND('',#3450,.T.);
#2380=FACE_OUTER_BOUND('',#3451,.T.);
#2381=FACE_OUTER_BOUND('',#3452,.T.);
#2382=FACE_OUTER_BOUND('',#3453,.T.);
#2383=FACE_OUTER_BOUND('',#3454,.T.);
#2384=FACE_OUTER_BOUND('',#3455,.T.);
#2385=FACE_OUTER_BOUND('',#3456,.T.);
#2386=FACE_OUTER_BOUND('',#3457,.T.);
#2387=FACE_OUTER_BOUND('',#3458,.T.);
#2388=FACE_OUTER_BOUND('',#3459,.T.);
#2389=FACE_OUTER_BOUND('',#3460,.T.);
#2390=FACE_OUTER_BOUND('',#3462,.T.);
#2391=FACE_OUTER_BOUND('',#3463,.T.);
#2392=FACE_OUTER_BOUND('',#3465,.T.);
#2393=FACE_OUTER_BOUND('',#3466,.T.);
#2394=FACE_OUTER_BOUND('',#3468,.T.);
#2395=FACE_OUTER_BOUND('',#3469,.T.);
#2396=FACE_OUTER_BOUND('',#3471,.T.);
#2397=FACE_OUTER_BOUND('',#3472,.T.);
#2398=FACE_OUTER_BOUND('',#3474,.T.);
#2399=FACE_OUTER_BOUND('',#3475,.T.);
#2400=FACE_OUTER_BOUND('',#3476,.T.);
#2401=FACE_OUTER_BOUND('',#3477,.T.);
#2402=FACE_OUTER_BOUND('',#3478,.T.);
#2403=FACE_OUTER_BOUND('',#3479,.T.);
#2404=FACE_OUTER_BOUND('',#3481,.T.);
#2405=FACE_OUTER_BOUND('',#3482,.T.);
#2406=FACE_OUTER_BOUND('',#3483,.T.);
#2407=FACE_OUTER_BOUND('',#3484,.T.);
#2408=FACE_OUTER_BOUND('',#3485,.T.);
#2409=FACE_OUTER_BOUND('',#3486,.T.);
#2410=FACE_OUTER_BOUND('',#3487,.T.);
#2411=FACE_OUTER_BOUND('',#3488,.T.);
#2412=FACE_OUTER_BOUND('',#3489,.T.);
#2413=FACE_OUTER_BOUND('',#3490,.T.);
#2414=FACE_OUTER_BOUND('',#3491,.T.);
#2415=FACE_OUTER_BOUND('',#3492,.T.);
#2416=FACE_OUTER_BOUND('',#3493,.T.);
#2417=FACE_OUTER_BOUND('',#3494,.T.);
#2418=FACE_OUTER_BOUND('',#3495,.T.);
#2419=FACE_OUTER_BOUND('',#3496,.T.);
#2420=FACE_OUTER_BOUND('',#3497,.T.);
#2421=FACE_OUTER_BOUND('',#3498,.T.);
#2422=FACE_OUTER_BOUND('',#3500,.T.);
#2423=FACE_OUTER_BOUND('',#3501,.T.);
#2424=FACE_OUTER_BOUND('',#3502,.T.);
#2425=FACE_OUTER_BOUND('',#3503,.T.);
#2426=FACE_OUTER_BOUND('',#3504,.T.);
#2427=FACE_OUTER_BOUND('',#3505,.T.);
#2428=FACE_OUTER_BOUND('',#3507,.T.);
#2429=FACE_OUTER_BOUND('',#3509,.T.);
#2430=FACE_OUTER_BOUND('',#3511,.T.);
#2431=FACE_OUTER_BOUND('',#3513,.T.);
#2432=FACE_OUTER_BOUND('',#3514,.T.);
#2433=FACE_OUTER_BOUND('',#3515,.T.);
#2434=FACE_OUTER_BOUND('',#3516,.T.);
#2435=FACE_OUTER_BOUND('',#3518,.T.);
#2436=FACE_OUTER_BOUND('',#3520,.T.);
#2437=FACE_OUTER_BOUND('',#3522,.T.);
#2438=FACE_OUTER_BOUND('',#3524,.T.);
#2439=FACE_OUTER_BOUND('',#3525,.T.);
#2440=FACE_OUTER_BOUND('',#3526,.T.);
#2441=FACE_OUTER_BOUND('',#3528,.T.);
#2442=FACE_OUTER_BOUND('',#3530,.T.);
#2443=FACE_OUTER_BOUND('',#3531,.T.);
#2444=FACE_OUTER_BOUND('',#3532,.T.);
#2445=FACE_OUTER_BOUND('',#3534,.T.);
#2446=FACE_OUTER_BOUND('',#3536,.T.);
#2447=FACE_OUTER_BOUND('',#3537,.T.);
#2448=FACE_OUTER_BOUND('',#3538,.T.);
#2449=FACE_OUTER_BOUND('',#3540,.T.);
#2450=FACE_OUTER_BOUND('',#3542,.T.);
#2451=FACE_OUTER_BOUND('',#3543,.T.);
#2452=FACE_OUTER_BOUND('',#3544,.T.);
#2453=FACE_OUTER_BOUND('',#3546,.T.);
#2454=FACE_OUTER_BOUND('',#3548,.T.);
#2455=FACE_OUTER_BOUND('',#3549,.T.);
#2456=FACE_OUTER_BOUND('',#3550,.T.);
#2457=FACE_OUTER_BOUND('',#3551,.T.);
#2458=FACE_OUTER_BOUND('',#3553,.T.);
#2459=FACE_OUTER_BOUND('',#3554,.T.);
#2460=FACE_OUTER_BOUND('',#3555,.T.);
#2461=FACE_OUTER_BOUND('',#3557,.T.);
#2462=FACE_OUTER_BOUND('',#3558,.T.);
#2463=FACE_OUTER_BOUND('',#3559,.T.);
#2464=FACE_OUTER_BOUND('',#3560,.T.);
#2465=FACE_OUTER_BOUND('',#3561,.T.);
#2466=FACE_OUTER_BOUND('',#3562,.T.);
#2467=FACE_OUTER_BOUND('',#3563,.T.);
#2468=FACE_OUTER_BOUND('',#3564,.T.);
#2469=FACE_OUTER_BOUND('',#3565,.T.);
#2470=FACE_OUTER_BOUND('',#3566,.T.);
#2471=FACE_OUTER_BOUND('',#3567,.T.);
#2472=FACE_OUTER_BOUND('',#3568,.T.);
#2473=FACE_OUTER_BOUND('',#3569,.T.);
#2474=FACE_OUTER_BOUND('',#3570,.T.);
#2475=FACE_OUTER_BOUND('',#3571,.T.);
#2476=FACE_OUTER_BOUND('',#3572,.T.);
#2477=FACE_OUTER_BOUND('',#3573,.T.);
#2478=FACE_OUTER_BOUND('',#3574,.T.);
#2479=FACE_OUTER_BOUND('',#3575,.T.);
#2480=FACE_OUTER_BOUND('',#3576,.T.);
#2481=FACE_OUTER_BOUND('',#3577,.T.);
#2482=FACE_OUTER_BOUND('',#3578,.T.);
#2483=FACE_OUTER_BOUND('',#3579,.T.);
#2484=FACE_OUTER_BOUND('',#3580,.T.);
#2485=FACE_OUTER_BOUND('',#3581,.T.);
#2486=FACE_OUTER_BOUND('',#3582,.T.);
#2487=FACE_OUTER_BOUND('',#3583,.T.);
#2488=FACE_OUTER_BOUND('',#3584,.T.);
#2489=FACE_OUTER_BOUND('',#3585,.T.);
#2490=FACE_OUTER_BOUND('',#3586,.T.);
#2491=FACE_OUTER_BOUND('',#3587,.T.);
#2492=FACE_OUTER_BOUND('',#3588,.T.);
#2493=FACE_OUTER_BOUND('',#3589,.T.);
#2494=FACE_OUTER_BOUND('',#3590,.T.);
#2495=FACE_OUTER_BOUND('',#3591,.T.);
#2496=FACE_OUTER_BOUND('',#3592,.T.);
#2497=FACE_OUTER_BOUND('',#3593,.T.);
#2498=FACE_OUTER_BOUND('',#3594,.T.);
#2499=FACE_OUTER_BOUND('',#3595,.T.);
#2500=FACE_OUTER_BOUND('',#3596,.T.);
#2501=FACE_OUTER_BOUND('',#3597,.T.);
#2502=FACE_OUTER_BOUND('',#3598,.T.);
#2503=FACE_OUTER_BOUND('',#3599,.T.);
#2504=FACE_OUTER_BOUND('',#3600,.T.);
#2505=FACE_OUTER_BOUND('',#3601,.T.);
#2506=FACE_OUTER_BOUND('',#3602,.T.);
#2507=FACE_OUTER_BOUND('',#3603,.T.);
#2508=FACE_OUTER_BOUND('',#3604,.T.);
#2509=FACE_OUTER_BOUND('',#3605,.T.);
#2510=FACE_OUTER_BOUND('',#3606,.T.);
#2511=FACE_OUTER_BOUND('',#3607,.T.);
#2512=FACE_OUTER_BOUND('',#3608,.T.);
#2513=FACE_OUTER_BOUND('',#3609,.T.);
#2514=FACE_OUTER_BOUND('',#3610,.T.);
#2515=FACE_OUTER_BOUND('',#3611,.T.);
#2516=FACE_OUTER_BOUND('',#3612,.T.);
#2517=FACE_OUTER_BOUND('',#3613,.T.);
#2518=FACE_OUTER_BOUND('',#3614,.T.);
#2519=FACE_OUTER_BOUND('',#3615,.T.);
#2520=FACE_OUTER_BOUND('',#3616,.T.);
#2521=FACE_OUTER_BOUND('',#3617,.T.);
#2522=FACE_OUTER_BOUND('',#3618,.T.);
#2523=FACE_OUTER_BOUND('',#3619,.T.);
#2524=FACE_OUTER_BOUND('',#3620,.T.);
#2525=FACE_OUTER_BOUND('',#3621,.T.);
#2526=FACE_OUTER_BOUND('',#3622,.T.);
#2527=FACE_OUTER_BOUND('',#3623,.T.);
#2528=FACE_OUTER_BOUND('',#3624,.T.);
#2529=FACE_OUTER_BOUND('',#3625,.T.);
#2530=FACE_OUTER_BOUND('',#3626,.T.);
#2531=FACE_OUTER_BOUND('',#3627,.T.);
#2532=FACE_OUTER_BOUND('',#3628,.T.);
#2533=FACE_OUTER_BOUND('',#3629,.T.);
#2534=FACE_OUTER_BOUND('',#3630,.T.);
#2535=FACE_OUTER_BOUND('',#3631,.T.);
#2536=FACE_OUTER_BOUND('',#3632,.T.);
#2537=FACE_OUTER_BOUND('',#3633,.T.);
#2538=FACE_OUTER_BOUND('',#3634,.T.);
#2539=FACE_OUTER_BOUND('',#3635,.T.);
#2540=FACE_OUTER_BOUND('',#3636,.T.);
#2541=FACE_OUTER_BOUND('',#3638,.T.);
#2542=FACE_OUTER_BOUND('',#3639,.T.);
#2543=FACE_OUTER_BOUND('',#3640,.T.);
#2544=FACE_OUTER_BOUND('',#3641,.T.);
#2545=FACE_OUTER_BOUND('',#3642,.T.);
#2546=FACE_OUTER_BOUND('',#3643,.T.);
#2547=FACE_OUTER_BOUND('',#3644,.T.);
#2548=FACE_OUTER_BOUND('',#3645,.T.);
#2549=FACE_OUTER_BOUND('',#3646,.T.);
#2550=FACE_OUTER_BOUND('',#3647,.T.);
#2551=FACE_OUTER_BOUND('',#3648,.T.);
#2552=FACE_OUTER_BOUND('',#3649,.T.);
#2553=FACE_OUTER_BOUND('',#3650,.T.);
#2554=FACE_OUTER_BOUND('',#3651,.T.);
#2555=FACE_OUTER_BOUND('',#3652,.T.);
#2556=FACE_OUTER_BOUND('',#3653,.T.);
#2557=FACE_OUTER_BOUND('',#3654,.T.);
#2558=FACE_OUTER_BOUND('',#3655,.T.);
#2559=FACE_OUTER_BOUND('',#3656,.T.);
#2560=FACE_OUTER_BOUND('',#3657,.T.);
#2561=FACE_OUTER_BOUND('',#3658,.T.);
#2562=FACE_OUTER_BOUND('',#3659,.T.);
#2563=FACE_OUTER_BOUND('',#3662,.T.);
#2564=FACE_OUTER_BOUND('',#3663,.T.);
#2565=FACE_OUTER_BOUND('',#3664,.T.);
#2566=FACE_OUTER_BOUND('',#3665,.T.);
#2567=FACE_OUTER_BOUND('',#3666,.T.);
#2568=FACE_OUTER_BOUND('',#3667,.T.);
#2569=FACE_OUTER_BOUND('',#3669,.T.);
#2570=FACE_OUTER_BOUND('',#3671,.T.);
#2571=FACE_OUTER_BOUND('',#3673,.T.);
#2572=FACE_OUTER_BOUND('',#3675,.T.);
#2573=FACE_OUTER_BOUND('',#3676,.T.);
#2574=FACE_OUTER_BOUND('',#3677,.T.);
#2575=FACE_OUTER_BOUND('',#3678,.T.);
#2576=FACE_OUTER_BOUND('',#3680,.T.);
#2577=FACE_OUTER_BOUND('',#3682,.T.);
#2578=FACE_OUTER_BOUND('',#3684,.T.);
#2579=FACE_OUTER_BOUND('',#3686,.T.);
#2580=FACE_OUTER_BOUND('',#3687,.T.);
#2581=FACE_OUTER_BOUND('',#3688,.T.);
#2582=FACE_OUTER_BOUND('',#3690,.T.);
#2583=FACE_OUTER_BOUND('',#3692,.T.);
#2584=FACE_OUTER_BOUND('',#3693,.T.);
#2585=FACE_OUTER_BOUND('',#3694,.T.);
#2586=FACE_OUTER_BOUND('',#3696,.T.);
#2587=FACE_OUTER_BOUND('',#3698,.T.);
#2588=FACE_OUTER_BOUND('',#3699,.T.);
#2589=FACE_OUTER_BOUND('',#3700,.T.);
#2590=FACE_OUTER_BOUND('',#3702,.T.);
#2591=FACE_OUTER_BOUND('',#3704,.T.);
#2592=FACE_OUTER_BOUND('',#3705,.T.);
#2593=FACE_OUTER_BOUND('',#3706,.T.);
#2594=FACE_OUTER_BOUND('',#3708,.T.);
#2595=FACE_OUTER_BOUND('',#3710,.T.);
#2596=FACE_OUTER_BOUND('',#3711,.T.);
#2597=FACE_OUTER_BOUND('',#3712,.T.);
#2598=FACE_OUTER_BOUND('',#3714,.T.);
#2599=FACE_OUTER_BOUND('',#3716,.T.);
#2600=FACE_OUTER_BOUND('',#3717,.T.);
#2601=FACE_OUTER_BOUND('',#3718,.T.);
#2602=FACE_OUTER_BOUND('',#3719,.T.);
#2603=FACE_OUTER_BOUND('',#3721,.T.);
#2604=FACE_OUTER_BOUND('',#3722,.T.);
#2605=FACE_OUTER_BOUND('',#3724,.T.);
#2606=FACE_OUTER_BOUND('',#3725,.T.);
#2607=FACE_OUTER_BOUND('',#3726,.T.);
#2608=FACE_OUTER_BOUND('',#3727,.T.);
#2609=FACE_OUTER_BOUND('',#3728,.T.);
#2610=FACE_OUTER_BOUND('',#3729,.T.);
#2611=FACE_OUTER_BOUND('',#3730,.T.);
#2612=FACE_OUTER_BOUND('',#3731,.T.);
#2613=FACE_OUTER_BOUND('',#3732,.T.);
#2614=FACE_OUTER_BOUND('',#3733,.T.);
#2615=FACE_OUTER_BOUND('',#3734,.T.);
#2616=FACE_OUTER_BOUND('',#3735,.T.);
#2617=FACE_OUTER_BOUND('',#3736,.T.);
#2618=FACE_OUTER_BOUND('',#3737,.T.);
#2619=FACE_OUTER_BOUND('',#3738,.T.);
#2620=FACE_OUTER_BOUND('',#3739,.T.);
#2621=FACE_OUTER_BOUND('',#3740,.T.);
#2622=FACE_OUTER_BOUND('',#3741,.T.);
#2623=FACE_OUTER_BOUND('',#3742,.T.);
#2624=FACE_OUTER_BOUND('',#3743,.T.);
#2625=FACE_OUTER_BOUND('',#3744,.T.);
#2626=FACE_OUTER_BOUND('',#3745,.T.);
#2627=FACE_OUTER_BOUND('',#3746,.T.);
#2628=FACE_OUTER_BOUND('',#3747,.T.);
#2629=FACE_OUTER_BOUND('',#3748,.T.);
#2630=FACE_OUTER_BOUND('',#3749,.T.);
#2631=FACE_OUTER_BOUND('',#3750,.T.);
#2632=FACE_OUTER_BOUND('',#3751,.T.);
#2633=FACE_OUTER_BOUND('',#3752,.T.);
#2634=FACE_OUTER_BOUND('',#3753,.T.);
#2635=FACE_OUTER_BOUND('',#3754,.T.);
#2636=FACE_OUTER_BOUND('',#3755,.T.);
#2637=FACE_OUTER_BOUND('',#3756,.T.);
#2638=FACE_OUTER_BOUND('',#3757,.T.);
#2639=FACE_OUTER_BOUND('',#3758,.T.);
#2640=FACE_OUTER_BOUND('',#3759,.T.);
#2641=FACE_OUTER_BOUND('',#3760,.T.);
#2642=FACE_OUTER_BOUND('',#3761,.T.);
#2643=FACE_OUTER_BOUND('',#3762,.T.);
#2644=FACE_OUTER_BOUND('',#3763,.T.);
#2645=FACE_OUTER_BOUND('',#3764,.T.);
#2646=FACE_OUTER_BOUND('',#3765,.T.);
#2647=FACE_OUTER_BOUND('',#3766,.T.);
#2648=FACE_OUTER_BOUND('',#3767,.T.);
#2649=FACE_OUTER_BOUND('',#3768,.T.);
#2650=FACE_OUTER_BOUND('',#3769,.T.);
#2651=FACE_OUTER_BOUND('',#3770,.T.);
#2652=FACE_OUTER_BOUND('',#3771,.T.);
#2653=FACE_OUTER_BOUND('',#3772,.T.);
#2654=FACE_OUTER_BOUND('',#3773,.T.);
#2655=FACE_OUTER_BOUND('',#3774,.T.);
#2656=FACE_OUTER_BOUND('',#3775,.T.);
#2657=FACE_OUTER_BOUND('',#3776,.T.);
#2658=FACE_OUTER_BOUND('',#3777,.T.);
#2659=FACE_OUTER_BOUND('',#3778,.T.);
#2660=FACE_OUTER_BOUND('',#3779,.T.);
#2661=FACE_OUTER_BOUND('',#3780,.T.);
#2662=FACE_OUTER_BOUND('',#3781,.T.);
#2663=FACE_OUTER_BOUND('',#3782,.T.);
#2664=FACE_OUTER_BOUND('',#3783,.T.);
#2665=FACE_OUTER_BOUND('',#3784,.T.);
#2666=FACE_OUTER_BOUND('',#3785,.T.);
#2667=FACE_OUTER_BOUND('',#3786,.T.);
#2668=FACE_OUTER_BOUND('',#3787,.T.);
#2669=FACE_OUTER_BOUND('',#3788,.T.);
#2670=FACE_OUTER_BOUND('',#3789,.T.);
#2671=FACE_OUTER_BOUND('',#3790,.T.);
#2672=FACE_OUTER_BOUND('',#3791,.T.);
#2673=FACE_OUTER_BOUND('',#3792,.T.);
#2674=FACE_OUTER_BOUND('',#3793,.T.);
#2675=FACE_OUTER_BOUND('',#3794,.T.);
#2676=FACE_OUTER_BOUND('',#3795,.T.);
#2677=FACE_OUTER_BOUND('',#3796,.T.);
#2678=FACE_OUTER_BOUND('',#3797,.T.);
#2679=FACE_OUTER_BOUND('',#3798,.T.);
#2680=FACE_OUTER_BOUND('',#3799,.T.);
#2681=FACE_OUTER_BOUND('',#3800,.T.);
#2682=FACE_OUTER_BOUND('',#3801,.T.);
#2683=FACE_OUTER_BOUND('',#3802,.T.);
#2684=FACE_OUTER_BOUND('',#3803,.T.);
#2685=FACE_OUTER_BOUND('',#3804,.T.);
#2686=FACE_OUTER_BOUND('',#3806,.T.);
#2687=FACE_OUTER_BOUND('',#3807,.T.);
#2688=FACE_OUTER_BOUND('',#3808,.T.);
#2689=FACE_OUTER_BOUND('',#3809,.T.);
#2690=FACE_OUTER_BOUND('',#3810,.T.);
#2691=FACE_OUTER_BOUND('',#3811,.T.);
#2692=FACE_OUTER_BOUND('',#3812,.T.);
#2693=FACE_OUTER_BOUND('',#3814,.T.);
#2694=FACE_OUTER_BOUND('',#3815,.T.);
#2695=FACE_OUTER_BOUND('',#3816,.T.);
#2696=FACE_OUTER_BOUND('',#3817,.T.);
#2697=FACE_OUTER_BOUND('',#3818,.T.);
#2698=FACE_OUTER_BOUND('',#3819,.T.);
#2699=FACE_OUTER_BOUND('',#3821,.T.);
#2700=FACE_OUTER_BOUND('',#3823,.T.);
#2701=FACE_OUTER_BOUND('',#3825,.T.);
#2702=FACE_OUTER_BOUND('',#3827,.T.);
#2703=FACE_OUTER_BOUND('',#3828,.T.);
#2704=FACE_OUTER_BOUND('',#3829,.T.);
#2705=FACE_OUTER_BOUND('',#3830,.T.);
#2706=FACE_OUTER_BOUND('',#3832,.T.);
#2707=FACE_OUTER_BOUND('',#3834,.T.);
#2708=FACE_OUTER_BOUND('',#3836,.T.);
#2709=FACE_OUTER_BOUND('',#3838,.T.);
#2710=FACE_OUTER_BOUND('',#3839,.T.);
#2711=FACE_OUTER_BOUND('',#3840,.T.);
#2712=FACE_OUTER_BOUND('',#3842,.T.);
#2713=FACE_OUTER_BOUND('',#3844,.T.);
#2714=FACE_OUTER_BOUND('',#3845,.T.);
#2715=FACE_OUTER_BOUND('',#3846,.T.);
#2716=FACE_OUTER_BOUND('',#3848,.T.);
#2717=FACE_OUTER_BOUND('',#3850,.T.);
#2718=FACE_OUTER_BOUND('',#3851,.T.);
#2719=FACE_OUTER_BOUND('',#3852,.T.);
#2720=FACE_OUTER_BOUND('',#3854,.T.);
#2721=FACE_OUTER_BOUND('',#3856,.T.);
#2722=FACE_OUTER_BOUND('',#3857,.T.);
#2723=FACE_OUTER_BOUND('',#3858,.T.);
#2724=FACE_OUTER_BOUND('',#3860,.T.);
#2725=FACE_OUTER_BOUND('',#3862,.T.);
#2726=FACE_OUTER_BOUND('',#3863,.T.);
#2727=FACE_OUTER_BOUND('',#3864,.T.);
#2728=FACE_OUTER_BOUND('',#3865,.T.);
#2729=FACE_OUTER_BOUND('',#3866,.T.);
#2730=FACE_OUTER_BOUND('',#3867,.T.);
#2731=FACE_OUTER_BOUND('',#3868,.T.);
#2732=FACE_OUTER_BOUND('',#3869,.T.);
#2733=FACE_OUTER_BOUND('',#3871,.T.);
#2734=FACE_OUTER_BOUND('',#3872,.T.);
#2735=FACE_OUTER_BOUND('',#3873,.T.);
#2736=FACE_OUTER_BOUND('',#3874,.T.);
#2737=FACE_OUTER_BOUND('',#3875,.T.);
#2738=FACE_OUTER_BOUND('',#3876,.T.);
#2739=FACE_OUTER_BOUND('',#3877,.T.);
#2740=FACE_OUTER_BOUND('',#3878,.T.);
#2741=FACE_OUTER_BOUND('',#3880,.T.);
#2742=FACE_OUTER_BOUND('',#3881,.T.);
#2743=FACE_OUTER_BOUND('',#3882,.T.);
#2744=FACE_OUTER_BOUND('',#3884,.T.);
#2745=FACE_OUTER_BOUND('',#3885,.T.);
#2746=FACE_OUTER_BOUND('',#3886,.T.);
#2747=FACE_OUTER_BOUND('',#3887,.T.);
#2748=FACE_OUTER_BOUND('',#3888,.T.);
#2749=FACE_OUTER_BOUND('',#3889,.T.);
#2750=FACE_OUTER_BOUND('',#3890,.T.);
#2751=FACE_OUTER_BOUND('',#3891,.T.);
#2752=FACE_OUTER_BOUND('',#3892,.T.);
#2753=FACE_OUTER_BOUND('',#3893,.T.);
#2754=FACE_OUTER_BOUND('',#3894,.T.);
#2755=FACE_OUTER_BOUND('',#3895,.T.);
#2756=FACE_OUTER_BOUND('',#3896,.T.);
#2757=FACE_OUTER_BOUND('',#3897,.T.);
#2758=FACE_OUTER_BOUND('',#3898,.T.);
#2759=FACE_OUTER_BOUND('',#3899,.T.);
#2760=FACE_OUTER_BOUND('',#3900,.T.);
#2761=FACE_OUTER_BOUND('',#3901,.T.);
#2762=FACE_OUTER_BOUND('',#3902,.T.);
#2763=FACE_OUTER_BOUND('',#3903,.T.);
#2764=FACE_OUTER_BOUND('',#3904,.T.);
#2765=FACE_OUTER_BOUND('',#3905,.T.);
#2766=FACE_OUTER_BOUND('',#3906,.T.);
#2767=FACE_OUTER_BOUND('',#3907,.T.);
#2768=FACE_OUTER_BOUND('',#3908,.T.);
#2769=FACE_OUTER_BOUND('',#3909,.T.);
#2770=FACE_OUTER_BOUND('',#3910,.T.);
#2771=FACE_OUTER_BOUND('',#3911,.T.);
#2772=FACE_OUTER_BOUND('',#3912,.T.);
#2773=FACE_OUTER_BOUND('',#3913,.T.);
#2774=FACE_OUTER_BOUND('',#3914,.T.);
#2775=FACE_OUTER_BOUND('',#3915,.T.);
#2776=FACE_OUTER_BOUND('',#3916,.T.);
#2777=FACE_OUTER_BOUND('',#3917,.T.);
#2778=FACE_OUTER_BOUND('',#3918,.T.);
#2779=FACE_OUTER_BOUND('',#3919,.T.);
#2780=FACE_OUTER_BOUND('',#3920,.T.);
#2781=FACE_OUTER_BOUND('',#3921,.T.);
#2782=FACE_OUTER_BOUND('',#3922,.T.);
#2783=FACE_OUTER_BOUND('',#3923,.T.);
#2784=FACE_OUTER_BOUND('',#3924,.T.);
#2785=FACE_OUTER_BOUND('',#3925,.T.);
#2786=FACE_OUTER_BOUND('',#3926,.T.);
#2787=FACE_OUTER_BOUND('',#3927,.T.);
#2788=FACE_OUTER_BOUND('',#3928,.T.);
#2789=FACE_OUTER_BOUND('',#3929,.T.);
#2790=FACE_OUTER_BOUND('',#3930,.T.);
#2791=FACE_OUTER_BOUND('',#3931,.T.);
#2792=FACE_OUTER_BOUND('',#3932,.T.);
#2793=FACE_OUTER_BOUND('',#3933,.T.);
#2794=FACE_OUTER_BOUND('',#3934,.T.);
#2795=FACE_OUTER_BOUND('',#3935,.T.);
#2796=FACE_OUTER_BOUND('',#3936,.T.);
#2797=FACE_OUTER_BOUND('',#3937,.T.);
#2798=FACE_OUTER_BOUND('',#3938,.T.);
#2799=FACE_OUTER_BOUND('',#3939,.T.);
#2800=FACE_OUTER_BOUND('',#3940,.T.);
#2801=FACE_OUTER_BOUND('',#3941,.T.);
#2802=FACE_OUTER_BOUND('',#3942,.T.);
#2803=FACE_OUTER_BOUND('',#3943,.T.);
#2804=FACE_OUTER_BOUND('',#3944,.T.);
#2805=FACE_OUTER_BOUND('',#3945,.T.);
#2806=FACE_OUTER_BOUND('',#3946,.T.);
#2807=FACE_OUTER_BOUND('',#3947,.T.);
#2808=FACE_OUTER_BOUND('',#3948,.T.);
#2809=FACE_OUTER_BOUND('',#3949,.T.);
#2810=FACE_OUTER_BOUND('',#3950,.T.);
#2811=FACE_OUTER_BOUND('',#3951,.T.);
#2812=FACE_OUTER_BOUND('',#3952,.T.);
#2813=FACE_OUTER_BOUND('',#3953,.T.);
#2814=FACE_OUTER_BOUND('',#3954,.T.);
#2815=FACE_OUTER_BOUND('',#3955,.T.);
#2816=FACE_OUTER_BOUND('',#3956,.T.);
#2817=FACE_OUTER_BOUND('',#3957,.T.);
#2818=FACE_OUTER_BOUND('',#3958,.T.);
#2819=FACE_OUTER_BOUND('',#3959,.T.);
#2820=FACE_OUTER_BOUND('',#3960,.T.);
#2821=FACE_OUTER_BOUND('',#3961,.T.);
#2822=FACE_OUTER_BOUND('',#3962,.T.);
#2823=FACE_OUTER_BOUND('',#3963,.T.);
#2824=FACE_OUTER_BOUND('',#3964,.T.);
#2825=FACE_OUTER_BOUND('',#3965,.T.);
#2826=FACE_OUTER_BOUND('',#3966,.T.);
#2827=FACE_OUTER_BOUND('',#3967,.T.);
#2828=FACE_OUTER_BOUND('',#3968,.T.);
#2829=FACE_OUTER_BOUND('',#3969,.T.);
#2830=FACE_OUTER_BOUND('',#3970,.T.);
#2831=FACE_OUTER_BOUND('',#3971,.T.);
#2832=FACE_OUTER_BOUND('',#3972,.T.);
#2833=FACE_OUTER_BOUND('',#3973,.T.);
#2834=FACE_OUTER_BOUND('',#3974,.T.);
#2835=FACE_OUTER_BOUND('',#3975,.T.);
#2836=FACE_OUTER_BOUND('',#3976,.T.);
#2837=FACE_OUTER_BOUND('',#3977,.T.);
#2838=FACE_OUTER_BOUND('',#3978,.T.);
#2839=FACE_OUTER_BOUND('',#3979,.T.);
#2840=FACE_OUTER_BOUND('',#3980,.T.);
#2841=FACE_OUTER_BOUND('',#3981,.T.);
#2842=FACE_OUTER_BOUND('',#3982,.T.);
#2843=FACE_OUTER_BOUND('',#3983,.T.);
#2844=FACE_OUTER_BOUND('',#3984,.T.);
#2845=FACE_OUTER_BOUND('',#3985,.T.);
#2846=FACE_OUTER_BOUND('',#3986,.T.);
#2847=FACE_OUTER_BOUND('',#3987,.T.);
#2848=FACE_OUTER_BOUND('',#3988,.T.);
#2849=FACE_OUTER_BOUND('',#3989,.T.);
#2850=FACE_OUTER_BOUND('',#3990,.T.);
#2851=FACE_OUTER_BOUND('',#3991,.T.);
#2852=FACE_OUTER_BOUND('',#3992,.T.);
#2853=FACE_OUTER_BOUND('',#3993,.T.);
#2854=FACE_OUTER_BOUND('',#3994,.T.);
#2855=FACE_OUTER_BOUND('',#3995,.T.);
#2856=FACE_OUTER_BOUND('',#3996,.T.);
#2857=FACE_OUTER_BOUND('',#3997,.T.);
#2858=FACE_OUTER_BOUND('',#3998,.T.);
#2859=FACE_OUTER_BOUND('',#3999,.T.);
#2860=FACE_OUTER_BOUND('',#4000,.T.);
#2861=FACE_OUTER_BOUND('',#4001,.T.);
#2862=FACE_OUTER_BOUND('',#4002,.T.);
#2863=FACE_OUTER_BOUND('',#4003,.T.);
#2864=FACE_OUTER_BOUND('',#4004,.T.);
#2865=FACE_OUTER_BOUND('',#4005,.T.);
#2866=FACE_OUTER_BOUND('',#4006,.T.);
#2867=FACE_OUTER_BOUND('',#4007,.T.);
#2868=FACE_OUTER_BOUND('',#4008,.T.);
#2869=FACE_OUTER_BOUND('',#4009,.T.);
#2870=FACE_OUTER_BOUND('',#4010,.T.);
#2871=FACE_OUTER_BOUND('',#4011,.T.);
#2872=FACE_OUTER_BOUND('',#4012,.T.);
#2873=FACE_OUTER_BOUND('',#4013,.T.);
#2874=FACE_OUTER_BOUND('',#4014,.T.);
#2875=FACE_OUTER_BOUND('',#4015,.T.);
#2876=FACE_OUTER_BOUND('',#4016,.T.);
#2877=FACE_OUTER_BOUND('',#4017,.T.);
#2878=FACE_OUTER_BOUND('',#4018,.T.);
#2879=FACE_OUTER_BOUND('',#4019,.T.);
#2880=FACE_OUTER_BOUND('',#4020,.T.);
#2881=FACE_OUTER_BOUND('',#4021,.T.);
#2882=FACE_OUTER_BOUND('',#4022,.T.);
#2883=FACE_OUTER_BOUND('',#4023,.T.);
#2884=FACE_OUTER_BOUND('',#4024,.T.);
#2885=FACE_OUTER_BOUND('',#4025,.T.);
#2886=FACE_OUTER_BOUND('',#4026,.T.);
#2887=FACE_OUTER_BOUND('',#4027,.T.);
#2888=FACE_OUTER_BOUND('',#4028,.T.);
#2889=FACE_OUTER_BOUND('',#4029,.T.);
#2890=FACE_OUTER_BOUND('',#4030,.T.);
#2891=FACE_OUTER_BOUND('',#4031,.T.);
#2892=FACE_OUTER_BOUND('',#4032,.T.);
#2893=FACE_OUTER_BOUND('',#4033,.T.);
#2894=FACE_OUTER_BOUND('',#4034,.T.);
#2895=FACE_OUTER_BOUND('',#4035,.T.);
#2896=FACE_OUTER_BOUND('',#4036,.T.);
#2897=FACE_OUTER_BOUND('',#4037,.T.);
#2898=FACE_OUTER_BOUND('',#4038,.T.);
#2899=FACE_OUTER_BOUND('',#4039,.T.);
#2900=FACE_OUTER_BOUND('',#4040,.T.);
#2901=FACE_OUTER_BOUND('',#4041,.T.);
#2902=FACE_OUTER_BOUND('',#4042,.T.);
#2903=FACE_OUTER_BOUND('',#4043,.T.);
#2904=FACE_OUTER_BOUND('',#4045,.T.);
#2905=FACE_OUTER_BOUND('',#4046,.T.);
#2906=FACE_OUTER_BOUND('',#4047,.T.);
#2907=FACE_OUTER_BOUND('',#4048,.T.);
#2908=FACE_OUTER_BOUND('',#4049,.T.);
#2909=FACE_OUTER_BOUND('',#4050,.T.);
#2910=FACE_OUTER_BOUND('',#4051,.T.);
#2911=FACE_OUTER_BOUND('',#4052,.T.);
#2912=FACE_OUTER_BOUND('',#4053,.T.);
#2913=FACE_OUTER_BOUND('',#4054,.T.);
#2914=FACE_OUTER_BOUND('',#4055,.T.);
#2915=EDGE_LOOP('',(#10507,#10508,#10509,#10510));
#2916=EDGE_LOOP('',(#10511,#10512,#10513,#10514));
#2917=EDGE_LOOP('',(#10515,#10516,#10517,#10518));
#2918=EDGE_LOOP('',(#10519,#10520,#10521,#10522));
#2919=EDGE_LOOP('',(#10523,#10524,#10525,#10526));
#2920=EDGE_LOOP('',(#10527,#10528,#10529,#10530));
#2921=EDGE_LOOP('',(#10531,#10532,#10533,#10534));
#2922=EDGE_LOOP('',(#10535,#10536,#10537,#10538));
#2923=EDGE_LOOP('',(#10539,#10540,#10541,#10542));
#2924=EDGE_LOOP('',(#10543));
#2925=EDGE_LOOP('',(#10544));
#2926=EDGE_LOOP('',(#10545));
#2927=EDGE_LOOP('',(#10546));
#2928=EDGE_LOOP('',(#10547,#10548,#10549,#10550));
#2929=EDGE_LOOP('',(#10551));
#2930=EDGE_LOOP('',(#10552));
#2931=EDGE_LOOP('',(#10553));
#2932=EDGE_LOOP('',(#10554));
#2933=EDGE_LOOP('',(#10555,#10556,#10557,#10558));
#2934=EDGE_LOOP('',(#10559));
#2935=EDGE_LOOP('',(#10560,#10561,#10562,#10563));
#2936=EDGE_LOOP('',(#10564));
#2937=EDGE_LOOP('',(#10565,#10566,#10567,#10568));
#2938=EDGE_LOOP('',(#10569));
#2939=EDGE_LOOP('',(#10570,#10571,#10572,#10573));
#2940=EDGE_LOOP('',(#10574));
#2941=EDGE_LOOP('',(#10575,#10576,#10577,#10578));
#2942=EDGE_LOOP('',(#10579,#10580,#10581,#10582));
#2943=EDGE_LOOP('',(#10583,#10584,#10585,#10586,#10587,#10588,#10589,#10590,
#10591,#10592,#10593,#10594,#10595,#10596));
#2944=EDGE_LOOP('',(#10597));
#2945=EDGE_LOOP('',(#10598));
#2946=EDGE_LOOP('',(#10599));
#2947=EDGE_LOOP('',(#10600));
#2948=EDGE_LOOP('',(#10601));
#2949=EDGE_LOOP('',(#10602));
#2950=EDGE_LOOP('',(#10603,#10604,#10605,#10606,#10607,#10608,#10609,#10610,
#10611,#10612,#10613,#10614));
#2951=EDGE_LOOP('',(#10615));
#2952=EDGE_LOOP('',(#10616));
#2953=EDGE_LOOP('',(#10617));
#2954=EDGE_LOOP('',(#10618));
#2955=EDGE_LOOP('',(#10619));
#2956=EDGE_LOOP('',(#10620,#10621,#10622,#10623));
#2957=EDGE_LOOP('',(#10624,#10625,#10626,#10627));
#2958=EDGE_LOOP('',(#10628,#10629,#10630,#10631,#10632,#10633,#10634,#10635,
#10636,#10637,#10638,#10639,#10640,#10641));
#2959=EDGE_LOOP('',(#10642));
#2960=EDGE_LOOP('',(#10643));
#2961=EDGE_LOOP('',(#10644));
#2962=EDGE_LOOP('',(#10645));
#2963=EDGE_LOOP('',(#10646));
#2964=EDGE_LOOP('',(#10647));
#2965=EDGE_LOOP('',(#10648,#10649,#10650,#10651,#10652,#10653,#10654,#10655));
#2966=EDGE_LOOP('',(#10656,#10657,#10658,#10659));
#2967=EDGE_LOOP('',(#10660,#10661,#10662,#10663));
#2968=EDGE_LOOP('',(#10664,#10665,#10666,#10667,#10668,#10669,#10670,#10671,
#10672,#10673));
#2969=EDGE_LOOP('',(#10674,#10675,#10676,#10677,#10678,#10679,#10680,#10681));
#2970=EDGE_LOOP('',(#10682,#10683,#10684,#10685));
#2971=EDGE_LOOP('',(#10686));
#2972=EDGE_LOOP('',(#10687,#10688,#10689,#10690));
#2973=EDGE_LOOP('',(#10691));
#2974=EDGE_LOOP('',(#10692,#10693,#10694,#10695));
#2975=EDGE_LOOP('',(#10696));
#2976=EDGE_LOOP('',(#10697,#10698,#10699,#10700));
#2977=EDGE_LOOP('',(#10701));
#2978=EDGE_LOOP('',(#10702,#10703,#10704,#10705));
#2979=EDGE_LOOP('',(#10706,#10707,#10708,#10709));
#2980=EDGE_LOOP('',(#10710,#10711,#10712,#10713));
#2981=EDGE_LOOP('',(#10714,#10715,#10716,#10717));
#2982=EDGE_LOOP('',(#10718,#10719,#10720,#10721,#10722,#10723,#10724,#10725));
#2983=EDGE_LOOP('',(#10726,#10727,#10728,#10729));
#2984=EDGE_LOOP('',(#10730,#10731,#10732,#10733));
#2985=EDGE_LOOP('',(#10734,#10735,#10736,#10737,#10738,#10739,#10740,#10741,
#10742,#10743));
#2986=EDGE_LOOP('',(#10744,#10745,#10746,#10747,#10748,#10749,#10750,#10751));
#2987=EDGE_LOOP('',(#10752,#10753,#10754,#10755));
#2988=EDGE_LOOP('',(#10756));
#2989=EDGE_LOOP('',(#10757,#10758,#10759,#10760));
#2990=EDGE_LOOP('',(#10761));
#2991=EDGE_LOOP('',(#10762,#10763,#10764,#10765));
#2992=EDGE_LOOP('',(#10766));
#2993=EDGE_LOOP('',(#10767,#10768,#10769,#10770));
#2994=EDGE_LOOP('',(#10771));
#2995=EDGE_LOOP('',(#10772,#10773,#10774,#10775));
#2996=EDGE_LOOP('',(#10776,#10777,#10778,#10779));
#2997=EDGE_LOOP('',(#10780,#10781,#10782,#10783,#10784,#10785,#10786,#10787,
#10788,#10789,#10790,#10791));
#2998=EDGE_LOOP('',(#10792));
#2999=EDGE_LOOP('',(#10793));
#3000=EDGE_LOOP('',(#10794));
#3001=EDGE_LOOP('',(#10795));
#3002=EDGE_LOOP('',(#10796));
#3003=EDGE_LOOP('',(#10797,#10798,#10799,#10800));
#3004=EDGE_LOOP('',(#10801,#10802,#10803,#10804));
#3005=EDGE_LOOP('',(#10805,#10806,#10807,#10808));
#3006=EDGE_LOOP('',(#10809,#10810,#10811,#10812));
#3007=EDGE_LOOP('',(#10813,#10814,#10815,#10816));
#3008=EDGE_LOOP('',(#10817));
#3009=EDGE_LOOP('',(#10818));
#3010=EDGE_LOOP('',(#10819,#10820,#10821,#10822));
#3011=EDGE_LOOP('',(#10823));
#3012=EDGE_LOOP('',(#10824));
#3013=EDGE_LOOP('',(#10825,#10826,#10827,#10828));
#3014=EDGE_LOOP('',(#10829));
#3015=EDGE_LOOP('',(#10830));
#3016=EDGE_LOOP('',(#10831,#10832,#10833,#10834));
#3017=EDGE_LOOP('',(#10835));
#3018=EDGE_LOOP('',(#10836));
#3019=EDGE_LOOP('',(#10837,#10838,#10839,#10840));
#3020=EDGE_LOOP('',(#10841,#10842,#10843,#10844));
#3021=EDGE_LOOP('',(#10845,#10846,#10847,#10848));
#3022=EDGE_LOOP('',(#10849,#10850,#10851,#10852));
#3023=EDGE_LOOP('',(#10853,#10854,#10855,#10856));
#3024=EDGE_LOOP('',(#10857));
#3025=EDGE_LOOP('',(#10858,#10859,#10860,#10861));
#3026=EDGE_LOOP('',(#10862));
#3027=EDGE_LOOP('',(#10863,#10864,#10865,#10866));
#3028=EDGE_LOOP('',(#10867));
#3029=EDGE_LOOP('',(#10868,#10869,#10870,#10871));
#3030=EDGE_LOOP('',(#10872));
#3031=EDGE_LOOP('',(#10873,#10874,#10875,#10876));
#3032=EDGE_LOOP('',(#10877,#10878,#10879,#10880));
#3033=EDGE_LOOP('',(#10881,#10882,#10883,#10884));
#3034=EDGE_LOOP('',(#10885,#10886,#10887,#10888));
#3035=EDGE_LOOP('',(#10889,#10890,#10891,#10892));
#3036=EDGE_LOOP('',(#10893,#10894,#10895,#10896));
#3037=EDGE_LOOP('',(#10897,#10898,#10899,#10900));
#3038=EDGE_LOOP('',(#10901,#10902,#10903,#10904));
#3039=EDGE_LOOP('',(#10905));
#3040=EDGE_LOOP('',(#10906));
#3041=EDGE_LOOP('',(#10907));
#3042=EDGE_LOOP('',(#10908,#10909,#10910,#10911));
#3043=EDGE_LOOP('',(#10912,#10913,#10914,#10915));
#3044=EDGE_LOOP('',(#10916,#10917,#10918,#10919));
#3045=EDGE_LOOP('',(#10920));
#3046=EDGE_LOOP('',(#10921));
#3047=EDGE_LOOP('',(#10922));
#3048=EDGE_LOOP('',(#10923,#10924,#10925,#10926));
#3049=EDGE_LOOP('',(#10927,#10928,#10929,#10930));
#3050=EDGE_LOOP('',(#10931,#10932,#10933,#10934));
#3051=EDGE_LOOP('',(#10935));
#3052=EDGE_LOOP('',(#10936));
#3053=EDGE_LOOP('',(#10937));
#3054=EDGE_LOOP('',(#10938));
#3055=EDGE_LOOP('',(#10939,#10940,#10941,#10942));
#3056=EDGE_LOOP('',(#10943,#10944,#10945,#10946));
#3057=EDGE_LOOP('',(#10947));
#3058=EDGE_LOOP('',(#10948));
#3059=EDGE_LOOP('',(#10949));
#3060=EDGE_LOOP('',(#10950));
#3061=EDGE_LOOP('',(#10951,#10952,#10953,#10954));
#3062=EDGE_LOOP('',(#10955,#10956,#10957,#10958));
#3063=EDGE_LOOP('',(#10959,#10960,#10961,#10962));
#3064=EDGE_LOOP('',(#10963,#10964,#10965,#10966));
#3065=EDGE_LOOP('',(#10967,#10968,#10969,#10970));
#3066=EDGE_LOOP('',(#10971,#10972,#10973,#10974));
#3067=EDGE_LOOP('',(#10975,#10976,#10977,#10978));
#3068=EDGE_LOOP('',(#10979,#10980,#10981,#10982));
#3069=EDGE_LOOP('',(#10983,#10984,#10985,#10986));
#3070=EDGE_LOOP('',(#10987));
#3071=EDGE_LOOP('',(#10988,#10989,#10990,#10991));
#3072=EDGE_LOOP('',(#10992));
#3073=EDGE_LOOP('',(#10993,#10994,#10995,#10996));
#3074=EDGE_LOOP('',(#10997));
#3075=EDGE_LOOP('',(#10998,#10999,#11000,#11001));
#3076=EDGE_LOOP('',(#11002));
#3077=EDGE_LOOP('',(#11003,#11004,#11005,#11006));
#3078=EDGE_LOOP('',(#11007,#11008,#11009,#11010));
#3079=EDGE_LOOP('',(#11011,#11012,#11013,#11014));
#3080=EDGE_LOOP('',(#11015,#11016,#11017,#11018,#11019,#11020,#11021,#11022,
#11023,#11024,#11025,#11026));
#3081=EDGE_LOOP('',(#11027));
#3082=EDGE_LOOP('',(#11028));
#3083=EDGE_LOOP('',(#11029));
#3084=EDGE_LOOP('',(#11030));
#3085=EDGE_LOOP('',(#11031));
#3086=EDGE_LOOP('',(#11032,#11033,#11034,#11035));
#3087=EDGE_LOOP('',(#11036,#11037,#11038,#11039));
#3088=EDGE_LOOP('',(#11040,#11041,#11042,#11043,#11044,#11045,#11046,#11047,
#11048,#11049,#11050,#11051,#11052,#11053));
#3089=EDGE_LOOP('',(#11054));
#3090=EDGE_LOOP('',(#11055));
#3091=EDGE_LOOP('',(#11056));
#3092=EDGE_LOOP('',(#11057));
#3093=EDGE_LOOP('',(#11058));
#3094=EDGE_LOOP('',(#11059));
#3095=EDGE_LOOP('',(#11060,#11061,#11062,#11063));
#3096=EDGE_LOOP('',(#11064,#11065,#11066,#11067,#11068,#11069,#11070,#11071,
#11072,#11073,#11074,#11075,#11076,#11077));
#3097=EDGE_LOOP('',(#11078));
#3098=EDGE_LOOP('',(#11079));
#3099=EDGE_LOOP('',(#11080));
#3100=EDGE_LOOP('',(#11081));
#3101=EDGE_LOOP('',(#11082));
#3102=EDGE_LOOP('',(#11083));
#3103=EDGE_LOOP('',(#11084,#11085,#11086,#11087,#11088,#11089,#11090,#11091,
#11092,#11093));
#3104=EDGE_LOOP('',(#11094,#11095,#11096,#11097,#11098,#11099,#11100,#11101));
#3105=EDGE_LOOP('',(#11102,#11103,#11104,#11105,#11106,#11107,#11108,#11109));
#3106=EDGE_LOOP('',(#11110,#11111,#11112,#11113));
#3107=EDGE_LOOP('',(#11114));
#3108=EDGE_LOOP('',(#11115,#11116,#11117,#11118));
#3109=EDGE_LOOP('',(#11119));
#3110=EDGE_LOOP('',(#11120,#11121,#11122,#11123));
#3111=EDGE_LOOP('',(#11124));
#3112=EDGE_LOOP('',(#11125,#11126,#11127,#11128));
#3113=EDGE_LOOP('',(#11129));
#3114=EDGE_LOOP('',(#11130,#11131,#11132,#11133));
#3115=EDGE_LOOP('',(#11134,#11135,#11136,#11137));
#3116=EDGE_LOOP('',(#11138,#11139,#11140,#11141));
#3117=EDGE_LOOP('',(#11142,#11143,#11144,#11145));
#3118=EDGE_LOOP('',(#11146,#11147,#11148,#11149));
#3119=EDGE_LOOP('',(#11150,#11151,#11152,#11153));
#3120=EDGE_LOOP('',(#11154,#11155,#11156,#11157,#11158,#11159,#11160,#11161));
#3121=EDGE_LOOP('',(#11162,#11163,#11164,#11165,#11166,#11167,#11168,#11169));
#3122=EDGE_LOOP('',(#11170,#11171,#11172,#11173));
#3123=EDGE_LOOP('',(#11174));
#3124=EDGE_LOOP('',(#11175,#11176,#11177,#11178));
#3125=EDGE_LOOP('',(#11179));
#3126=EDGE_LOOP('',(#11180,#11181,#11182,#11183));
#3127=EDGE_LOOP('',(#11184));
#3128=EDGE_LOOP('',(#11185,#11186,#11187,#11188));
#3129=EDGE_LOOP('',(#11189));
#3130=EDGE_LOOP('',(#11190,#11191,#11192,#11193));
#3131=EDGE_LOOP('',(#11194,#11195,#11196,#11197));
#3132=EDGE_LOOP('',(#11198,#11199,#11200,#11201));
#3133=EDGE_LOOP('',(#11202,#11203,#11204,#11205));
#3134=EDGE_LOOP('',(#11206,#11207,#11208,#11209));
#3135=EDGE_LOOP('',(#11210,#11211,#11212,#11213));
#3136=EDGE_LOOP('',(#11214,#11215,#11216,#11217,#11218,#11219,#11220,#11221,
#11222,#11223));
#3137=EDGE_LOOP('',(#11224,#11225,#11226,#11227,#11228,#11229,#11230,#11231,
#11232,#11233,#11234,#11235));
#3138=EDGE_LOOP('',(#11236));
#3139=EDGE_LOOP('',(#11237));
#3140=EDGE_LOOP('',(#11238));
#3141=EDGE_LOOP('',(#11239));
#3142=EDGE_LOOP('',(#11240));
#3143=EDGE_LOOP('',(#11241,#11242,#11243,#11244));
#3144=EDGE_LOOP('',(#11245));
#3145=EDGE_LOOP('',(#11246,#11247,#11248,#11249));
#3146=EDGE_LOOP('',(#11250));
#3147=EDGE_LOOP('',(#11251,#11252,#11253,#11254));
#3148=EDGE_LOOP('',(#11255));
#3149=EDGE_LOOP('',(#11256,#11257,#11258,#11259));
#3150=EDGE_LOOP('',(#11260));
#3151=EDGE_LOOP('',(#11261,#11262,#11263,#11264));
#3152=EDGE_LOOP('',(#11265,#11266,#11267,#11268));
#3153=EDGE_LOOP('',(#11269,#11270,#11271,#11272));
#3154=EDGE_LOOP('',(#11273,#11274,#11275,#11276));
#3155=EDGE_LOOP('',(#11277,#11278,#11279,#11280));
#3156=EDGE_LOOP('',(#11281,#11282,#11283,#11284));
#3157=EDGE_LOOP('',(#11285,#11286,#11287,#11288));
#3158=EDGE_LOOP('',(#11289,#11290,#11291,#11292));
#3159=EDGE_LOOP('',(#11293));
#3160=EDGE_LOOP('',(#11294));
#3161=EDGE_LOOP('',(#11295));
#3162=EDGE_LOOP('',(#11296,#11297,#11298,#11299));
#3163=EDGE_LOOP('',(#11300,#11301,#11302,#11303));
#3164=EDGE_LOOP('',(#11304));
#3165=EDGE_LOOP('',(#11305));
#3166=EDGE_LOOP('',(#11306));
#3167=EDGE_LOOP('',(#11307,#11308,#11309,#11310));
#3168=EDGE_LOOP('',(#11311,#11312,#11313,#11314));
#3169=EDGE_LOOP('',(#11315,#11316,#11317,#11318));
#3170=EDGE_LOOP('',(#11319,#11320,#11321,#11322));
#3171=EDGE_LOOP('',(#11323,#11324,#11325,#11326));
#3172=EDGE_LOOP('',(#11327));
#3173=EDGE_LOOP('',(#11328));
#3174=EDGE_LOOP('',(#11329));
#3175=EDGE_LOOP('',(#11330));
#3176=EDGE_LOOP('',(#11331,#11332,#11333,#11334));
#3177=EDGE_LOOP('',(#11335,#11336,#11337,#11338));
#3178=EDGE_LOOP('',(#11339,#11340,#11341,#11342));
#3179=EDGE_LOOP('',(#11343));
#3180=EDGE_LOOP('',(#11344));
#3181=EDGE_LOOP('',(#11345));
#3182=EDGE_LOOP('',(#11346));
#3183=EDGE_LOOP('',(#11347,#11348,#11349,#11350));
#3184=EDGE_LOOP('',(#11351));
#3185=EDGE_LOOP('',(#11352));
#3186=EDGE_LOOP('',(#11353,#11354,#11355,#11356));
#3187=EDGE_LOOP('',(#11357));
#3188=EDGE_LOOP('',(#11358));
#3189=EDGE_LOOP('',(#11359,#11360,#11361,#11362));
#3190=EDGE_LOOP('',(#11363));
#3191=EDGE_LOOP('',(#11364));
#3192=EDGE_LOOP('',(#11365,#11366,#11367,#11368));
#3193=EDGE_LOOP('',(#11369));
#3194=EDGE_LOOP('',(#11370));
#3195=EDGE_LOOP('',(#11371,#11372,#11373,#11374));
#3196=EDGE_LOOP('',(#11375,#11376,#11377,#11378));
#3197=EDGE_LOOP('',(#11379,#11380,#11381,#11382));
#3198=EDGE_LOOP('',(#11383,#11384,#11385,#11386));
#3199=EDGE_LOOP('',(#11387,#11388,#11389,#11390,#11391,#11392,#11393,#11394));
#3200=EDGE_LOOP('',(#11395));
#3201=EDGE_LOOP('',(#11396,#11397,#11398,#11399));
#3202=EDGE_LOOP('',(#11400,#11401,#11402,#11403));
#3203=EDGE_LOOP('',(#11404,#11405,#11406,#11407));
#3204=EDGE_LOOP('',(#11408,#11409,#11410,#11411));
#3205=EDGE_LOOP('',(#11412,#11413,#11414,#11415));
#3206=EDGE_LOOP('',(#11416));
#3207=EDGE_LOOP('',(#11417));
#3208=EDGE_LOOP('',(#11418,#11419,#11420,#11421));
#3209=EDGE_LOOP('',(#11422,#11423,#11424,#11425,#11426,#11427,#11428,#11429));
#3210=EDGE_LOOP('',(#11430));
#3211=EDGE_LOOP('',(#11431,#11432,#11433,#11434));
#3212=EDGE_LOOP('',(#11435,#11436,#11437,#11438));
#3213=EDGE_LOOP('',(#11439,#11440,#11441,#11442));
#3214=EDGE_LOOP('',(#11443,#11444,#11445,#11446));
#3215=EDGE_LOOP('',(#11447,#11448,#11449,#11450,#11451,#11452,#11453,#11454));
#3216=EDGE_LOOP('',(#11455));
#3217=EDGE_LOOP('',(#11456,#11457,#11458,#11459));
#3218=EDGE_LOOP('',(#11460,#11461,#11462,#11463));
#3219=EDGE_LOOP('',(#11464,#11465,#11466,#11467));
#3220=EDGE_LOOP('',(#11468,#11469,#11470,#11471));
#3221=EDGE_LOOP('',(#11472,#11473,#11474,#11475));
#3222=EDGE_LOOP('',(#11476));
#3223=EDGE_LOOP('',(#11477));
#3224=EDGE_LOOP('',(#11478,#11479,#11480,#11481));
#3225=EDGE_LOOP('',(#11482,#11483,#11484,#11485,#11486,#11487,#11488,#11489));
#3226=EDGE_LOOP('',(#11490));
#3227=EDGE_LOOP('',(#11491,#11492,#11493,#11494));
#3228=EDGE_LOOP('',(#11495,#11496,#11497,#11498));
#3229=EDGE_LOOP('',(#11499,#11500,#11501,#11502));
#3230=EDGE_LOOP('',(#11503,#11504,#11505,#11506));
#3231=EDGE_LOOP('',(#11507,#11508,#11509,#11510));
#3232=EDGE_LOOP('',(#11511));
#3233=EDGE_LOOP('',(#11512));
#3234=EDGE_LOOP('',(#11513,#11514,#11515,#11516));
#3235=EDGE_LOOP('',(#11517,#11518,#11519,#11520));
#3236=EDGE_LOOP('',(#11521));
#3237=EDGE_LOOP('',(#11522));
#3238=EDGE_LOOP('',(#11523));
#3239=EDGE_LOOP('',(#11524));
#3240=EDGE_LOOP('',(#11525));
#3241=EDGE_LOOP('',(#11526));
#3242=EDGE_LOOP('',(#11527));
#3243=EDGE_LOOP('',(#11528));
#3244=EDGE_LOOP('',(#11529));
#3245=EDGE_LOOP('',(#11530));
#3246=EDGE_LOOP('',(#11531));
#3247=EDGE_LOOP('',(#11532));
#3248=EDGE_LOOP('',(#11533,#11534,#11535,#11536));
#3249=EDGE_LOOP('',(#11537,#11538,#11539,#11540));
#3250=EDGE_LOOP('',(#11541,#11542,#11543,#11544));
#3251=EDGE_LOOP('',(#11545,#11546,#11547,#11548));
#3252=EDGE_LOOP('',(#11549,#11550,#11551,#11552));
#3253=EDGE_LOOP('',(#11553));
#3254=EDGE_LOOP('',(#11554));
#3255=EDGE_LOOP('',(#11555,#11556,#11557,#11558));
#3256=EDGE_LOOP('',(#11559,#11560,#11561,#11562));
#3257=EDGE_LOOP('',(#11563));
#3258=EDGE_LOOP('',(#11564));
#3259=EDGE_LOOP('',(#11565));
#3260=EDGE_LOOP('',(#11566));
#3261=EDGE_LOOP('',(#11567));
#3262=EDGE_LOOP('',(#11568));
#3263=EDGE_LOOP('',(#11569));
#3264=EDGE_LOOP('',(#11570));
#3265=EDGE_LOOP('',(#11571));
#3266=EDGE_LOOP('',(#11572));
#3267=EDGE_LOOP('',(#11573));
#3268=EDGE_LOOP('',(#11574));
#3269=EDGE_LOOP('',(#11575,#11576,#11577,#11578));
#3270=EDGE_LOOP('',(#11579,#11580,#11581,#11582));
#3271=EDGE_LOOP('',(#11583,#11584,#11585,#11586));
#3272=EDGE_LOOP('',(#11587,#11588,#11589,#11590));
#3273=EDGE_LOOP('',(#11591,#11592,#11593,#11594));
#3274=EDGE_LOOP('',(#11595));
#3275=EDGE_LOOP('',(#11596));
#3276=EDGE_LOOP('',(#11597,#11598,#11599,#11600));
#3277=EDGE_LOOP('',(#11601,#11602,#11603,#11604));
#3278=EDGE_LOOP('',(#11605));
#3279=EDGE_LOOP('',(#11606));
#3280=EDGE_LOOP('',(#11607));
#3281=EDGE_LOOP('',(#11608));
#3282=EDGE_LOOP('',(#11609));
#3283=EDGE_LOOP('',(#11610));
#3284=EDGE_LOOP('',(#11611));
#3285=EDGE_LOOP('',(#11612));
#3286=EDGE_LOOP('',(#11613));
#3287=EDGE_LOOP('',(#11614));
#3288=EDGE_LOOP('',(#11615));
#3289=EDGE_LOOP('',(#11616));
#3290=EDGE_LOOP('',(#11617,#11618,#11619,#11620));
#3291=EDGE_LOOP('',(#11621,#11622,#11623,#11624));
#3292=EDGE_LOOP('',(#11625,#11626,#11627,#11628));
#3293=EDGE_LOOP('',(#11629,#11630,#11631,#11632));
#3294=EDGE_LOOP('',(#11633,#11634,#11635,#11636));
#3295=EDGE_LOOP('',(#11637));
#3296=EDGE_LOOP('',(#11638));
#3297=EDGE_LOOP('',(#11639,#11640,#11641,#11642));
#3298=EDGE_LOOP('',(#11643,#11644,#11645,#11646));
#3299=EDGE_LOOP('',(#11647));
#3300=EDGE_LOOP('',(#11648));
#3301=EDGE_LOOP('',(#11649));
#3302=EDGE_LOOP('',(#11650));
#3303=EDGE_LOOP('',(#11651));
#3304=EDGE_LOOP('',(#11652));
#3305=EDGE_LOOP('',(#11653));
#3306=EDGE_LOOP('',(#11654));
#3307=EDGE_LOOP('',(#11655));
#3308=EDGE_LOOP('',(#11656));
#3309=EDGE_LOOP('',(#11657));
#3310=EDGE_LOOP('',(#11658));
#3311=EDGE_LOOP('',(#11659,#11660,#11661,#11662));
#3312=EDGE_LOOP('',(#11663,#11664,#11665,#11666));
#3313=EDGE_LOOP('',(#11667,#11668,#11669,#11670));
#3314=EDGE_LOOP('',(#11671,#11672,#11673,#11674));
#3315=EDGE_LOOP('',(#11675,#11676,#11677,#11678));
#3316=EDGE_LOOP('',(#11679,#11680,#11681,#11682));
#3317=EDGE_LOOP('',(#11683,#11684,#11685,#11686));
#3318=EDGE_LOOP('',(#11687,#11688,#11689,#11690));
#3319=EDGE_LOOP('',(#11691,#11692,#11693,#11694));
#3320=EDGE_LOOP('',(#11695));
#3321=EDGE_LOOP('',(#11696));
#3322=EDGE_LOOP('',(#11697));
#3323=EDGE_LOOP('',(#11698));
#3324=EDGE_LOOP('',(#11699,#11700,#11701,#11702));
#3325=EDGE_LOOP('',(#11703));
#3326=EDGE_LOOP('',(#11704));
#3327=EDGE_LOOP('',(#11705));
#3328=EDGE_LOOP('',(#11706));
#3329=EDGE_LOOP('',(#11707,#11708,#11709,#11710));
#3330=EDGE_LOOP('',(#11711,#11712,#11713,#11714));
#3331=EDGE_LOOP('',(#11715,#11716,#11717,#11718));
#3332=EDGE_LOOP('',(#11719,#11720,#11721,#11722));
#3333=EDGE_LOOP('',(#11723,#11724,#11725,#11726));
#3334=EDGE_LOOP('',(#11727,#11728,#11729,#11730));
#3335=EDGE_LOOP('',(#11731,#11732,#11733,#11734));
#3336=EDGE_LOOP('',(#11735,#11736,#11737,#11738));
#3337=EDGE_LOOP('',(#11739,#11740,#11741,#11742));
#3338=EDGE_LOOP('',(#11743,#11744,#11745,#11746));
#3339=EDGE_LOOP('',(#11747,#11748,#11749,#11750));
#3340=EDGE_LOOP('',(#11751,#11752,#11753,#11754));
#3341=EDGE_LOOP('',(#11755,#11756,#11757,#11758));
#3342=EDGE_LOOP('',(#11759,#11760,#11761,#11762));
#3343=EDGE_LOOP('',(#11763,#11764,#11765,#11766));
#3344=EDGE_LOOP('',(#11767,#11768,#11769,#11770));
#3345=EDGE_LOOP('',(#11771,#11772,#11773,#11774));
#3346=EDGE_LOOP('',(#11775,#11776,#11777,#11778));
#3347=EDGE_LOOP('',(#11779,#11780,#11781,#11782,#11783,#11784));
#3348=EDGE_LOOP('',(#11785,#11786,#11787,#11788,#11789,#11790));
#3349=EDGE_LOOP('',(#11791));
#3350=EDGE_LOOP('',(#11792));
#3351=EDGE_LOOP('',(#11793,#11794,#11795,#11796));
#3352=EDGE_LOOP('',(#11797,#11798,#11799,#11800));
#3353=EDGE_LOOP('',(#11801,#11802,#11803,#11804));
#3354=EDGE_LOOP('',(#11805));
#3355=EDGE_LOOP('',(#11806));
#3356=EDGE_LOOP('',(#11807,#11808,#11809,#11810));
#3357=EDGE_LOOP('',(#11811,#11812,#11813,#11814));
#3358=EDGE_LOOP('',(#11815,#11816,#11817,#11818,#11819,#11820));
#3359=EDGE_LOOP('',(#11821,#11822,#11823,#11824,#11825));
#3360=EDGE_LOOP('',(#11826,#11827,#11828,#11829));
#3361=EDGE_LOOP('',(#11830,#11831,#11832,#11833));
#3362=EDGE_LOOP('',(#11834));
#3363=EDGE_LOOP('',(#11835));
#3364=EDGE_LOOP('',(#11836,#11837,#11838,#11839,#11840));
#3365=EDGE_LOOP('',(#11841));
#3366=EDGE_LOOP('',(#11842));
#3367=EDGE_LOOP('',(#11843,#11844,#11845,#11846));
#3368=EDGE_LOOP('',(#11847,#11848,#11849,#11850,#11851,#11852));
#3369=EDGE_LOOP('',(#11853,#11854,#11855,#11856,#11857));
#3370=EDGE_LOOP('',(#11858));
#3371=EDGE_LOOP('',(#11859));
#3372=EDGE_LOOP('',(#11860,#11861,#11862,#11863));
#3373=EDGE_LOOP('',(#11864,#11865,#11866,#11867));
#3374=EDGE_LOOP('',(#11868,#11869,#11870,#11871));
#3375=EDGE_LOOP('',(#11872));
#3376=EDGE_LOOP('',(#11873));
#3377=EDGE_LOOP('',(#11874,#11875,#11876,#11877,#11878));
#3378=EDGE_LOOP('',(#11879,#11880));
#3379=EDGE_LOOP('',(#11881,#11882));
#3380=EDGE_LOOP('',(#11883,#11884));
#3381=EDGE_LOOP('',(#11885,#11886));
#3382=EDGE_LOOP('',(#11887,#11888));
#3383=EDGE_LOOP('',(#11889,#11890));
#3384=EDGE_LOOP('',(#11891,#11892));
#3385=EDGE_LOOP('',(#11893,#11894,#11895,#11896));
#3386=EDGE_LOOP('',(#11897,#11898,#11899,#11900,#11901,#11902,#11903,#11904,
#11905,#11906,#11907,#11908,#11909,#11910,#11911,#11912,#11913,#11914));
#3387=EDGE_LOOP('',(#11915,#11916,#11917,#11918));
#3388=EDGE_LOOP('',(#11919,#11920,#11921,#11922));
#3389=EDGE_LOOP('',(#11923,#11924,#11925,#11926));
#3390=EDGE_LOOP('',(#11927,#11928,#11929,#11930));
#3391=EDGE_LOOP('',(#11931,#11932,#11933,#11934,#11935,#11936));
#3392=EDGE_LOOP('',(#11937,#11938,#11939,#11940));
#3393=EDGE_LOOP('',(#11941,#11942,#11943,#11944));
#3394=EDGE_LOOP('',(#11945,#11946,#11947,#11948));
#3395=EDGE_LOOP('',(#11949,#11950,#11951,#11952));
#3396=EDGE_LOOP('',(#11953,#11954,#11955,#11956));
#3397=EDGE_LOOP('',(#11957,#11958,#11959,#11960,#11961,#11962,#11963,#11964,
#11965,#11966,#11967,#11968,#11969,#11970,#11971,#11972,#11973,#11974));
#3398=EDGE_LOOP('',(#11975,#11976,#11977,#11978));
#3399=EDGE_LOOP('',(#11979,#11980,#11981,#11982));
#3400=EDGE_LOOP('',(#11983));
#3401=EDGE_LOOP('',(#11984));
#3402=EDGE_LOOP('',(#11985,#11986,#11987,#11988));
#3403=EDGE_LOOP('',(#11989));
#3404=EDGE_LOOP('',(#11990));
#3405=EDGE_LOOP('',(#11991,#11992,#11993,#11994));
#3406=EDGE_LOOP('',(#11995));
#3407=EDGE_LOOP('',(#11996));
#3408=EDGE_LOOP('',(#11997,#11998,#11999,#12000));
#3409=EDGE_LOOP('',(#12001));
#3410=EDGE_LOOP('',(#12002));
#3411=EDGE_LOOP('',(#12003,#12004,#12005,#12006));
#3412=EDGE_LOOP('',(#12007));
#3413=EDGE_LOOP('',(#12008));
#3414=EDGE_LOOP('',(#12009,#12010,#12011,#12012));
#3415=EDGE_LOOP('',(#12013,#12014,#12015,#12016,#12017,#12018));
#3416=EDGE_LOOP('',(#12019,#12020,#12021,#12022,#12023));
#3417=EDGE_LOOP('',(#12024,#12025,#12026,#12027));
#3418=EDGE_LOOP('',(#12028,#12029,#12030,#12031));
#3419=EDGE_LOOP('',(#12032));
#3420=EDGE_LOOP('',(#12033));
#3421=EDGE_LOOP('',(#12034,#12035,#12036,#12037,#12038));
#3422=EDGE_LOOP('',(#12039));
#3423=EDGE_LOOP('',(#12040));
#3424=EDGE_LOOP('',(#12041,#12042,#12043,#12044));
#3425=EDGE_LOOP('',(#12045,#12046,#12047,#12048,#12049,#12050));
#3426=EDGE_LOOP('',(#12051,#12052,#12053,#12054,#12055));
#3427=EDGE_LOOP('',(#12056));
#3428=EDGE_LOOP('',(#12057));
#3429=EDGE_LOOP('',(#12058,#12059,#12060,#12061));
#3430=EDGE_LOOP('',(#12062,#12063,#12064,#12065));
#3431=EDGE_LOOP('',(#12066,#12067,#12068,#12069));
#3432=EDGE_LOOP('',(#12070));
#3433=EDGE_LOOP('',(#12071));
#3434=EDGE_LOOP('',(#12072,#12073,#12074,#12075,#12076));
#3435=EDGE_LOOP('',(#12077,#12078));
#3436=EDGE_LOOP('',(#12079,#12080));
#3437=EDGE_LOOP('',(#12081,#12082));
#3438=EDGE_LOOP('',(#12083,#12084));
#3439=EDGE_LOOP('',(#12085,#12086));
#3440=EDGE_LOOP('',(#12087,#12088));
#3441=EDGE_LOOP('',(#12089,#12090));
#3442=EDGE_LOOP('',(#12091,#12092));
#3443=EDGE_LOOP('',(#12093,#12094,#12095,#12096));
#3444=EDGE_LOOP('',(#12097,#12098,#12099,#12100,#12101,#12102,#12103,#12104,
#12105,#12106,#12107,#12108,#12109,#12110,#12111,#12112,#12113,#12114,#12115,
#12116));
#3445=EDGE_LOOP('',(#12117,#12118,#12119,#12120));
#3446=EDGE_LOOP('',(#12121,#12122,#12123,#12124));
#3447=EDGE_LOOP('',(#12125,#12126,#12127,#12128));
#3448=EDGE_LOOP('',(#12129,#12130,#12131,#12132));
#3449=EDGE_LOOP('',(#12133,#12134,#12135,#12136));
#3450=EDGE_LOOP('',(#12137,#12138,#12139,#12140,#12141,#12142));
#3451=EDGE_LOOP('',(#12143,#12144,#12145,#12146));
#3452=EDGE_LOOP('',(#12147,#12148,#12149,#12150));
#3453=EDGE_LOOP('',(#12151,#12152,#12153,#12154));
#3454=EDGE_LOOP('',(#12155,#12156,#12157,#12158));
#3455=EDGE_LOOP('',(#12159,#12160,#12161,#12162));
#3456=EDGE_LOOP('',(#12163,#12164,#12165,#12166));
#3457=EDGE_LOOP('',(#12167,#12168,#12169,#12170,#12171,#12172,#12173,#12174,
#12175,#12176,#12177,#12178,#12179,#12180,#12181,#12182,#12183,#12184,#12185,
#12186));
#3458=EDGE_LOOP('',(#12187,#12188,#12189,#12190));
#3459=EDGE_LOOP('',(#12191,#12192,#12193,#12194));
#3460=EDGE_LOOP('',(#12195));
#3461=EDGE_LOOP('',(#12196));
#3462=EDGE_LOOP('',(#12197,#12198,#12199,#12200));
#3463=EDGE_LOOP('',(#12201));
#3464=EDGE_LOOP('',(#12202));
#3465=EDGE_LOOP('',(#12203,#12204,#12205,#12206));
#3466=EDGE_LOOP('',(#12207));
#3467=EDGE_LOOP('',(#12208));
#3468=EDGE_LOOP('',(#12209,#12210,#12211,#12212));
#3469=EDGE_LOOP('',(#12213));
#3470=EDGE_LOOP('',(#12214));
#3471=EDGE_LOOP('',(#12215,#12216,#12217,#12218));
#3472=EDGE_LOOP('',(#12219));
#3473=EDGE_LOOP('',(#12220));
#3474=EDGE_LOOP('',(#12221,#12222,#12223,#12224));
#3475=EDGE_LOOP('',(#12225));
#3476=EDGE_LOOP('',(#12226,#12227,#12228,#12229));
#3477=EDGE_LOOP('',(#12230,#12231,#12232,#12233));
#3478=EDGE_LOOP('',(#12234,#12235,#12236,#12237));
#3479=EDGE_LOOP('',(#12238));
#3480=EDGE_LOOP('',(#12239));
#3481=EDGE_LOOP('',(#12240,#12241,#12242,#12243));
#3482=EDGE_LOOP('',(#12244,#12245,#12246,#12247));
#3483=EDGE_LOOP('',(#12248,#12249,#12250,#12251));
#3484=EDGE_LOOP('',(#12252));
#3485=EDGE_LOOP('',(#12253,#12254,#12255,#12256));
#3486=EDGE_LOOP('',(#12257,#12258,#12259,#12260));
#3487=EDGE_LOOP('',(#12261,#12262,#12263,#12264));
#3488=EDGE_LOOP('',(#12265,#12266,#12267,#12268));
#3489=EDGE_LOOP('',(#12269,#12270,#12271,#12272));
#3490=EDGE_LOOP('',(#12273,#12274,#12275,#12276));
#3491=EDGE_LOOP('',(#12277,#12278,#12279,#12280,#12281,#12282));
#3492=EDGE_LOOP('',(#12283,#12284,#12285,#12286,#12287,#12288));
#3493=EDGE_LOOP('',(#12289,#12290,#12291,#12292));
#3494=EDGE_LOOP('',(#12293,#12294,#12295,#12296));
#3495=EDGE_LOOP('',(#12297,#12298,#12299,#12300));
#3496=EDGE_LOOP('',(#12301,#12302,#12303,#12304));
#3497=EDGE_LOOP('',(#12305,#12306,#12307,#12308));
#3498=EDGE_LOOP('',(#12309,#12310,#12311,#12312));
#3499=EDGE_LOOP('',(#12313,#12314,#12315,#12316));
#3500=EDGE_LOOP('',(#12317));
#3501=EDGE_LOOP('',(#12318));
#3502=EDGE_LOOP('',(#12319,#12320));
#3503=EDGE_LOOP('',(#12321,#12322,#12323,#12324,#12325,#12326,#12327,#12328,
#12329));
#3504=EDGE_LOOP('',(#12330,#12331,#12332));
#3505=EDGE_LOOP('',(#12333,#12334,#12335,#12336));
#3506=EDGE_LOOP('',(#12337,#12338,#12339,#12340));
#3507=EDGE_LOOP('',(#12341,#12342,#12343,#12344));
#3508=EDGE_LOOP('',(#12345,#12346));
#3509=EDGE_LOOP('',(#12347));
#3510=EDGE_LOOP('',(#12348));
#3511=EDGE_LOOP('',(#12349));
#3512=EDGE_LOOP('',(#12350));
#3513=EDGE_LOOP('',(#12351,#12352));
#3514=EDGE_LOOP('',(#12353,#12354,#12355,#12356,#12357,#12358,#12359,#12360,
#12361));
#3515=EDGE_LOOP('',(#12362,#12363,#12364));
#3516=EDGE_LOOP('',(#12365,#12366,#12367,#12368));
#3517=EDGE_LOOP('',(#12369,#12370,#12371,#12372));
#3518=EDGE_LOOP('',(#12373,#12374,#12375,#12376));
#3519=EDGE_LOOP('',(#12377,#12378));
#3520=EDGE_LOOP('',(#12379));
#3521=EDGE_LOOP('',(#12380));
#3522=EDGE_LOOP('',(#12381));
#3523=EDGE_LOOP('',(#12382));
#3524=EDGE_LOOP('',(#12383,#12384,#12385,#12386));
#3525=EDGE_LOOP('',(#12387,#12388,#12389,#12390));
#3526=EDGE_LOOP('',(#12391));
#3527=EDGE_LOOP('',(#12392));
#3528=EDGE_LOOP('',(#12393));
#3529=EDGE_LOOP('',(#12394));
#3530=EDGE_LOOP('',(#12395,#12396,#12397,#12398));
#3531=EDGE_LOOP('',(#12399,#12400,#12401,#12402));
#3532=EDGE_LOOP('',(#12403));
#3533=EDGE_LOOP('',(#12404));
#3534=EDGE_LOOP('',(#12405));
#3535=EDGE_LOOP('',(#12406));
#3536=EDGE_LOOP('',(#12407,#12408,#12409,#12410));
#3537=EDGE_LOOP('',(#12411,#12412,#12413,#12414));
#3538=EDGE_LOOP('',(#12415));
#3539=EDGE_LOOP('',(#12416));
#3540=EDGE_LOOP('',(#12417));
#3541=EDGE_LOOP('',(#12418));
#3542=EDGE_LOOP('',(#12419,#12420,#12421,#12422));
#3543=EDGE_LOOP('',(#12423,#12424,#12425,#12426));
#3544=EDGE_LOOP('',(#12427));
#3545=EDGE_LOOP('',(#12428));
#3546=EDGE_LOOP('',(#12429));
#3547=EDGE_LOOP('',(#12430));
#3548=EDGE_LOOP('',(#12431,#12432,#12433,#12434));
#3549=EDGE_LOOP('',(#12435,#12436,#12437,#12438));
#3550=EDGE_LOOP('',(#12439,#12440,#12441,#12442));
#3551=EDGE_LOOP('',(#12443,#12444,#12445,#12446,#12447,#12448,#12449,#12450,
#12451,#12452,#12453,#12454,#12455,#12456,#12457,#12458,#12459,#12460,#12461,
#12462,#12463,#12464,#12465,#12466,#12467,#12468,#12469,#12470,#12471,#12472,
#12473,#12474,#12475,#12476,#12477,#12478,#12479,#12480,#12481,#12482,#12483,
#12484,#12485,#12486,#12487,#12488,#12489,#12490,#12491,#12492,#12493,#12494,
#12495,#12496,#12497,#12498,#12499,#12500,#12501,#12502,#12503,#12504,#12505,
#12506,#12507,#12508,#12509,#12510,#12511,#12512,#12513,#12514,#12515,#12516,
#12517,#12518,#12519,#12520,#12521,#12522));
#3552=EDGE_LOOP('',(#12523,#12524,#12525,#12526));
#3553=EDGE_LOOP('',(#12527,#12528,#12529,#12530));
#3554=EDGE_LOOP('',(#12531,#12532,#12533,#12534));
#3555=EDGE_LOOP('',(#12535));
#3556=EDGE_LOOP('',(#12536,#12537,#12538,#12539));
#3557=EDGE_LOOP('',(#12540,#12541,#12542,#12543));
#3558=EDGE_LOOP('',(#12544,#12545,#12546,#12547));
#3559=EDGE_LOOP('',(#12548,#12549,#12550,#12551));
#3560=EDGE_LOOP('',(#12552,#12553,#12554,#12555));
#3561=EDGE_LOOP('',(#12556,#12557,#12558,#12559));
#3562=EDGE_LOOP('',(#12560,#12561,#12562,#12563));
#3563=EDGE_LOOP('',(#12564,#12565,#12566,#12567));
#3564=EDGE_LOOP('',(#12568,#12569,#12570,#12571));
#3565=EDGE_LOOP('',(#12572,#12573,#12574,#12575));
#3566=EDGE_LOOP('',(#12576,#12577,#12578,#12579));
#3567=EDGE_LOOP('',(#12580,#12581,#12582,#12583));
#3568=EDGE_LOOP('',(#12584,#12585,#12586,#12587));
#3569=EDGE_LOOP('',(#12588,#12589,#12590,#12591));
#3570=EDGE_LOOP('',(#12592,#12593,#12594,#12595));
#3571=EDGE_LOOP('',(#12596,#12597,#12598,#12599));
#3572=EDGE_LOOP('',(#12600,#12601,#12602,#12603));
#3573=EDGE_LOOP('',(#12604,#12605,#12606,#12607));
#3574=EDGE_LOOP('',(#12608,#12609,#12610,#12611));
#3575=EDGE_LOOP('',(#12612,#12613,#12614,#12615));
#3576=EDGE_LOOP('',(#12616,#12617,#12618,#12619));
#3577=EDGE_LOOP('',(#12620,#12621,#12622,#12623));
#3578=EDGE_LOOP('',(#12624,#12625,#12626,#12627));
#3579=EDGE_LOOP('',(#12628,#12629,#12630,#12631));
#3580=EDGE_LOOP('',(#12632,#12633,#12634,#12635));
#3581=EDGE_LOOP('',(#12636,#12637,#12638,#12639));
#3582=EDGE_LOOP('',(#12640,#12641,#12642,#12643));
#3583=EDGE_LOOP('',(#12644,#12645,#12646,#12647));
#3584=EDGE_LOOP('',(#12648,#12649,#12650,#12651));
#3585=EDGE_LOOP('',(#12652,#12653,#12654,#12655));
#3586=EDGE_LOOP('',(#12656,#12657,#12658,#12659));
#3587=EDGE_LOOP('',(#12660,#12661,#12662,#12663));
#3588=EDGE_LOOP('',(#12664,#12665,#12666,#12667));
#3589=EDGE_LOOP('',(#12668,#12669,#12670,#12671));
#3590=EDGE_LOOP('',(#12672,#12673,#12674,#12675));
#3591=EDGE_LOOP('',(#12676,#12677,#12678,#12679));
#3592=EDGE_LOOP('',(#12680,#12681,#12682,#12683));
#3593=EDGE_LOOP('',(#12684,#12685,#12686,#12687));
#3594=EDGE_LOOP('',(#12688,#12689,#12690,#12691));
#3595=EDGE_LOOP('',(#12692,#12693,#12694,#12695));
#3596=EDGE_LOOP('',(#12696,#12697,#12698,#12699));
#3597=EDGE_LOOP('',(#12700,#12701,#12702,#12703));
#3598=EDGE_LOOP('',(#12704,#12705,#12706,#12707));
#3599=EDGE_LOOP('',(#12708,#12709,#12710,#12711));
#3600=EDGE_LOOP('',(#12712,#12713,#12714,#12715));
#3601=EDGE_LOOP('',(#12716,#12717,#12718,#12719));
#3602=EDGE_LOOP('',(#12720,#12721,#12722,#12723));
#3603=EDGE_LOOP('',(#12724,#12725,#12726,#12727));
#3604=EDGE_LOOP('',(#12728,#12729,#12730,#12731));
#3605=EDGE_LOOP('',(#12732,#12733,#12734,#12735));
#3606=EDGE_LOOP('',(#12736,#12737,#12738,#12739));
#3607=EDGE_LOOP('',(#12740,#12741,#12742,#12743));
#3608=EDGE_LOOP('',(#12744,#12745,#12746,#12747));
#3609=EDGE_LOOP('',(#12748,#12749,#12750,#12751));
#3610=EDGE_LOOP('',(#12752,#12753,#12754,#12755));
#3611=EDGE_LOOP('',(#12756,#12757,#12758,#12759));
#3612=EDGE_LOOP('',(#12760,#12761,#12762,#12763));
#3613=EDGE_LOOP('',(#12764,#12765,#12766,#12767));
#3614=EDGE_LOOP('',(#12768,#12769,#12770,#12771));
#3615=EDGE_LOOP('',(#12772,#12773,#12774,#12775));
#3616=EDGE_LOOP('',(#12776,#12777,#12778,#12779));
#3617=EDGE_LOOP('',(#12780,#12781,#12782,#12783));
#3618=EDGE_LOOP('',(#12784,#12785,#12786,#12787));
#3619=EDGE_LOOP('',(#12788,#12789,#12790,#12791));
#3620=EDGE_LOOP('',(#12792,#12793,#12794,#12795));
#3621=EDGE_LOOP('',(#12796,#12797,#12798,#12799));
#3622=EDGE_LOOP('',(#12800,#12801,#12802,#12803));
#3623=EDGE_LOOP('',(#12804,#12805,#12806,#12807));
#3624=EDGE_LOOP('',(#12808,#12809,#12810,#12811));
#3625=EDGE_LOOP('',(#12812,#12813,#12814,#12815));
#3626=EDGE_LOOP('',(#12816,#12817,#12818,#12819));
#3627=EDGE_LOOP('',(#12820,#12821,#12822,#12823));
#3628=EDGE_LOOP('',(#12824,#12825,#12826,#12827));
#3629=EDGE_LOOP('',(#12828,#12829,#12830,#12831));
#3630=EDGE_LOOP('',(#12832,#12833,#12834,#12835));
#3631=EDGE_LOOP('',(#12836,#12837,#12838,#12839));
#3632=EDGE_LOOP('',(#12840,#12841,#12842,#12843));
#3633=EDGE_LOOP('',(#12844,#12845,#12846,#12847));
#3634=EDGE_LOOP('',(#12848,#12849,#12850,#12851));
#3635=EDGE_LOOP('',(#12852,#12853,#12854,#12855));
#3636=EDGE_LOOP('',(#12856,#12857,#12858,#12859,#12860,#12861,#12862,#12863,
#12864,#12865,#12866,#12867,#12868,#12869,#12870,#12871,#12872,#12873,#12874,
#12875,#12876,#12877,#12878,#12879,#12880,#12881,#12882,#12883,#12884,#12885,
#12886,#12887,#12888,#12889,#12890,#12891,#12892,#12893,#12894,#12895,#12896,
#12897,#12898,#12899,#12900,#12901,#12902,#12903,#12904,#12905,#12906,#12907,
#12908,#12909,#12910,#12911,#12912,#12913,#12914,#12915,#12916,#12917,#12918,
#12919,#12920,#12921,#12922,#12923,#12924,#12925,#12926,#12927,#12928,#12929,
#12930,#12931,#12932,#12933,#12934,#12935));
#3637=EDGE_LOOP('',(#12936));
#3638=EDGE_LOOP('',(#12937,#12938,#12939,#12940));
#3639=EDGE_LOOP('',(#12941,#12942,#12943,#12944,#12945,#12946,#12947,#12948));
#3640=EDGE_LOOP('',(#12949,#12950,#12951,#12952));
#3641=EDGE_LOOP('',(#12953,#12954,#12955,#12956));
#3642=EDGE_LOOP('',(#12957,#12958,#12959,#12960));
#3643=EDGE_LOOP('',(#12961,#12962,#12963,#12964));
#3644=EDGE_LOOP('',(#12965,#12966,#12967,#12968,#12969,#12970,#12971,#12972));
#3645=EDGE_LOOP('',(#12973,#12974,#12975,#12976));
#3646=EDGE_LOOP('',(#12977,#12978,#12979,#12980));
#3647=EDGE_LOOP('',(#12981,#12982,#12983,#12984));
#3648=EDGE_LOOP('',(#12985,#12986,#12987,#12988));
#3649=EDGE_LOOP('',(#12989,#12990,#12991,#12992));
#3650=EDGE_LOOP('',(#12993,#12994,#12995,#12996));
#3651=EDGE_LOOP('',(#12997,#12998,#12999,#13000));
#3652=EDGE_LOOP('',(#13001,#13002,#13003,#13004));
#3653=EDGE_LOOP('',(#13005,#13006,#13007,#13008));
#3654=EDGE_LOOP('',(#13009,#13010,#13011,#13012));
#3655=EDGE_LOOP('',(#13013,#13014,#13015,#13016));
#3656=EDGE_LOOP('',(#13017,#13018,#13019,#13020));
#3657=EDGE_LOOP('',(#13021,#13022,#13023,#13024));
#3658=EDGE_LOOP('',(#13025,#13026,#13027,#13028));
#3659=EDGE_LOOP('',(#13029,#13030,#13031,#13032));
#3660=EDGE_LOOP('',(#13033,#13034,#13035,#13036));
#3661=EDGE_LOOP('',(#13037,#13038,#13039,#13040));
#3662=EDGE_LOOP('',(#13041));
#3663=EDGE_LOOP('',(#13042));
#3664=EDGE_LOOP('',(#13043,#13044));
#3665=EDGE_LOOP('',(#13045,#13046,#13047,#13048,#13049,#13050,#13051,#13052,
#13053));
#3666=EDGE_LOOP('',(#13054,#13055,#13056));
#3667=EDGE_LOOP('',(#13057,#13058,#13059,#13060));
#3668=EDGE_LOOP('',(#13061,#13062,#13063,#13064));
#3669=EDGE_LOOP('',(#13065,#13066,#13067,#13068));
#3670=EDGE_LOOP('',(#13069,#13070));
#3671=EDGE_LOOP('',(#13071));
#3672=EDGE_LOOP('',(#13072));
#3673=EDGE_LOOP('',(#13073));
#3674=EDGE_LOOP('',(#13074));
#3675=EDGE_LOOP('',(#13075,#13076));
#3676=EDGE_LOOP('',(#13077,#13078,#13079,#13080,#13081,#13082,#13083,#13084,
#13085));
#3677=EDGE_LOOP('',(#13086,#13087,#13088));
#3678=EDGE_LOOP('',(#13089,#13090,#13091,#13092));
#3679=EDGE_LOOP('',(#13093,#13094,#13095,#13096));
#3680=EDGE_LOOP('',(#13097,#13098,#13099,#13100));
#3681=EDGE_LOOP('',(#13101,#13102));
#3682=EDGE_LOOP('',(#13103));
#3683=EDGE_LOOP('',(#13104));
#3684=EDGE_LOOP('',(#13105));
#3685=EDGE_LOOP('',(#13106));
#3686=EDGE_LOOP('',(#13107,#13108,#13109,#13110));
#3687=EDGE_LOOP('',(#13111,#13112,#13113,#13114));
#3688=EDGE_LOOP('',(#13115));
#3689=EDGE_LOOP('',(#13116));
#3690=EDGE_LOOP('',(#13117));
#3691=EDGE_LOOP('',(#13118));
#3692=EDGE_LOOP('',(#13119,#13120,#13121,#13122));
#3693=EDGE_LOOP('',(#13123,#13124,#13125,#13126));
#3694=EDGE_LOOP('',(#13127));
#3695=EDGE_LOOP('',(#13128));
#3696=EDGE_LOOP('',(#13129));
#3697=EDGE_LOOP('',(#13130));
#3698=EDGE_LOOP('',(#13131,#13132,#13133,#13134));
#3699=EDGE_LOOP('',(#13135,#13136,#13137,#13138));
#3700=EDGE_LOOP('',(#13139));
#3701=EDGE_LOOP('',(#13140));
#3702=EDGE_LOOP('',(#13141));
#3703=EDGE_LOOP('',(#13142));
#3704=EDGE_LOOP('',(#13143,#13144,#13145,#13146));
#3705=EDGE_LOOP('',(#13147,#13148,#13149,#13150));
#3706=EDGE_LOOP('',(#13151));
#3707=EDGE_LOOP('',(#13152));
#3708=EDGE_LOOP('',(#13153));
#3709=EDGE_LOOP('',(#13154));
#3710=EDGE_LOOP('',(#13155,#13156,#13157,#13158));
#3711=EDGE_LOOP('',(#13159,#13160,#13161,#13162));
#3712=EDGE_LOOP('',(#13163));
#3713=EDGE_LOOP('',(#13164));
#3714=EDGE_LOOP('',(#13165));
#3715=EDGE_LOOP('',(#13166));
#3716=EDGE_LOOP('',(#13167,#13168,#13169,#13170));
#3717=EDGE_LOOP('',(#13171,#13172,#13173,#13174));
#3718=EDGE_LOOP('',(#13175,#13176,#13177,#13178));
#3719=EDGE_LOOP('',(#13179));
#3720=EDGE_LOOP('',(#13180,#13181,#13182,#13183));
#3721=EDGE_LOOP('',(#13184,#13185,#13186,#13187));
#3722=EDGE_LOOP('',(#13188,#13189,#13190,#13191,#13192,#13193,#13194,#13195,
#13196,#13197,#13198,#13199,#13200,#13201,#13202,#13203,#13204,#13205,#13206,
#13207,#13208,#13209,#13210,#13211,#13212,#13213,#13214,#13215,#13216,#13217,
#13218,#13219,#13220,#13221,#13222,#13223,#13224,#13225,#13226,#13227,#13228,
#13229,#13230,#13231,#13232,#13233,#13234,#13235,#13236,#13237,#13238,#13239,
#13240,#13241,#13242,#13243,#13244,#13245,#13246,#13247,#13248,#13249,#13250,
#13251,#13252,#13253,#13254,#13255,#13256,#13257,#13258,#13259,#13260,#13261,
#13262,#13263,#13264,#13265,#13266,#13267));
#3723=EDGE_LOOP('',(#13268,#13269,#13270,#13271));
#3724=EDGE_LOOP('',(#13272,#13273,#13274,#13275));
#3725=EDGE_LOOP('',(#13276,#13277,#13278,#13279));
#3726=EDGE_LOOP('',(#13280,#13281,#13282,#13283));
#3727=EDGE_LOOP('',(#13284,#13285,#13286,#13287));
#3728=EDGE_LOOP('',(#13288,#13289,#13290,#13291));
#3729=EDGE_LOOP('',(#13292,#13293,#13294,#13295));
#3730=EDGE_LOOP('',(#13296,#13297,#13298,#13299));
#3731=EDGE_LOOP('',(#13300,#13301,#13302,#13303));
#3732=EDGE_LOOP('',(#13304,#13305,#13306,#13307));
#3733=EDGE_LOOP('',(#13308,#13309,#13310,#13311));
#3734=EDGE_LOOP('',(#13312,#13313,#13314,#13315));
#3735=EDGE_LOOP('',(#13316,#13317,#13318,#13319));
#3736=EDGE_LOOP('',(#13320,#13321,#13322,#13323));
#3737=EDGE_LOOP('',(#13324,#13325,#13326,#13327));
#3738=EDGE_LOOP('',(#13328,#13329,#13330,#13331));
#3739=EDGE_LOOP('',(#13332,#13333,#13334,#13335));
#3740=EDGE_LOOP('',(#13336,#13337,#13338,#13339));
#3741=EDGE_LOOP('',(#13340,#13341,#13342,#13343));
#3742=EDGE_LOOP('',(#13344,#13345,#13346,#13347));
#3743=EDGE_LOOP('',(#13348,#13349,#13350,#13351));
#3744=EDGE_LOOP('',(#13352,#13353,#13354,#13355));
#3745=EDGE_LOOP('',(#13356,#13357,#13358,#13359));
#3746=EDGE_LOOP('',(#13360,#13361,#13362,#13363));
#3747=EDGE_LOOP('',(#13364,#13365,#13366,#13367));
#3748=EDGE_LOOP('',(#13368,#13369,#13370,#13371));
#3749=EDGE_LOOP('',(#13372,#13373,#13374,#13375));
#3750=EDGE_LOOP('',(#13376,#13377,#13378,#13379));
#3751=EDGE_LOOP('',(#13380,#13381,#13382,#13383));
#3752=EDGE_LOOP('',(#13384,#13385,#13386,#13387));
#3753=EDGE_LOOP('',(#13388,#13389,#13390,#13391));
#3754=EDGE_LOOP('',(#13392,#13393,#13394,#13395));
#3755=EDGE_LOOP('',(#13396,#13397,#13398,#13399));
#3756=EDGE_LOOP('',(#13400,#13401,#13402,#13403));
#3757=EDGE_LOOP('',(#13404,#13405,#13406,#13407));
#3758=EDGE_LOOP('',(#13408,#13409,#13410,#13411));
#3759=EDGE_LOOP('',(#13412,#13413,#13414,#13415));
#3760=EDGE_LOOP('',(#13416,#13417,#13418,#13419));
#3761=EDGE_LOOP('',(#13420,#13421,#13422,#13423));
#3762=EDGE_LOOP('',(#13424,#13425,#13426,#13427));
#3763=EDGE_LOOP('',(#13428,#13429,#13430,#13431));
#3764=EDGE_LOOP('',(#13432,#13433,#13434,#13435));
#3765=EDGE_LOOP('',(#13436,#13437,#13438,#13439));
#3766=EDGE_LOOP('',(#13440,#13441,#13442,#13443));
#3767=EDGE_LOOP('',(#13444,#13445,#13446,#13447));
#3768=EDGE_LOOP('',(#13448,#13449,#13450,#13451));
#3769=EDGE_LOOP('',(#13452,#13453,#13454,#13455));
#3770=EDGE_LOOP('',(#13456,#13457,#13458,#13459));
#3771=EDGE_LOOP('',(#13460,#13461,#13462,#13463));
#3772=EDGE_LOOP('',(#13464,#13465,#13466,#13467));
#3773=EDGE_LOOP('',(#13468,#13469,#13470,#13471));
#3774=EDGE_LOOP('',(#13472,#13473,#13474,#13475));
#3775=EDGE_LOOP('',(#13476,#13477,#13478,#13479));
#3776=EDGE_LOOP('',(#13480,#13481,#13482,#13483));
#3777=EDGE_LOOP('',(#13484,#13485,#13486,#13487));
#3778=EDGE_LOOP('',(#13488,#13489,#13490,#13491));
#3779=EDGE_LOOP('',(#13492,#13493,#13494,#13495));
#3780=EDGE_LOOP('',(#13496,#13497,#13498,#13499));
#3781=EDGE_LOOP('',(#13500,#13501,#13502,#13503));
#3782=EDGE_LOOP('',(#13504,#13505,#13506,#13507));
#3783=EDGE_LOOP('',(#13508,#13509,#13510,#13511));
#3784=EDGE_LOOP('',(#13512,#13513,#13514,#13515));
#3785=EDGE_LOOP('',(#13516,#13517,#13518,#13519));
#3786=EDGE_LOOP('',(#13520,#13521,#13522,#13523));
#3787=EDGE_LOOP('',(#13524,#13525,#13526,#13527));
#3788=EDGE_LOOP('',(#13528,#13529,#13530,#13531));
#3789=EDGE_LOOP('',(#13532,#13533,#13534,#13535));
#3790=EDGE_LOOP('',(#13536,#13537,#13538,#13539));
#3791=EDGE_LOOP('',(#13540,#13541,#13542,#13543));
#3792=EDGE_LOOP('',(#13544,#13545,#13546,#13547));
#3793=EDGE_LOOP('',(#13548,#13549,#13550,#13551));
#3794=EDGE_LOOP('',(#13552,#13553,#13554,#13555));
#3795=EDGE_LOOP('',(#13556,#13557,#13558,#13559));
#3796=EDGE_LOOP('',(#13560,#13561,#13562,#13563));
#3797=EDGE_LOOP('',(#13564,#13565,#13566,#13567));
#3798=EDGE_LOOP('',(#13568,#13569,#13570,#13571));
#3799=EDGE_LOOP('',(#13572,#13573,#13574,#13575));
#3800=EDGE_LOOP('',(#13576,#13577,#13578,#13579));
#3801=EDGE_LOOP('',(#13580,#13581,#13582,#13583));
#3802=EDGE_LOOP('',(#13584,#13585,#13586,#13587));
#3803=EDGE_LOOP('',(#13588,#13589,#13590,#13591));
#3804=EDGE_LOOP('',(#13592,#13593,#13594,#13595,#13596,#13597,#13598,#13599,
#13600,#13601,#13602,#13603,#13604,#13605,#13606,#13607,#13608,#13609,#13610,
#13611,#13612,#13613,#13614,#13615,#13616,#13617,#13618,#13619,#13620,#13621,
#13622,#13623,#13624,#13625,#13626,#13627,#13628,#13629,#13630,#13631,#13632,
#13633,#13634,#13635,#13636,#13637,#13638,#13639,#13640,#13641,#13642,#13643,
#13644,#13645,#13646,#13647,#13648,#13649,#13650,#13651,#13652,#13653,#13654,
#13655,#13656,#13657,#13658,#13659,#13660,#13661,#13662,#13663,#13664,#13665,
#13666,#13667,#13668,#13669,#13670,#13671));
#3805=EDGE_LOOP('',(#13672));
#3806=EDGE_LOOP('',(#13673,#13674,#13675,#13676));
#3807=EDGE_LOOP('',(#13677,#13678,#13679,#13680));
#3808=EDGE_LOOP('',(#13681,#13682,#13683,#13684));
#3809=EDGE_LOOP('',(#13685,#13686,#13687,#13688));
#3810=EDGE_LOOP('',(#13689,#13690,#13691,#13692));
#3811=EDGE_LOOP('',(#13693,#13694,#13695,#13696));
#3812=EDGE_LOOP('',(#13697,#13698,#13699,#13700));
#3813=EDGE_LOOP('',(#13701,#13702,#13703,#13704));
#3814=EDGE_LOOP('',(#13705));
#3815=EDGE_LOOP('',(#13706));
#3816=EDGE_LOOP('',(#13707,#13708));
#3817=EDGE_LOOP('',(#13709,#13710,#13711,#13712,#13713,#13714,#13715,#13716,
#13717));
#3818=EDGE_LOOP('',(#13718,#13719,#13720));
#3819=EDGE_LOOP('',(#13721,#13722,#13723,#13724));
#3820=EDGE_LOOP('',(#13725,#13726,#13727,#13728));
#3821=EDGE_LOOP('',(#13729,#13730,#13731,#13732));
#3822=EDGE_LOOP('',(#13733,#13734));
#3823=EDGE_LOOP('',(#13735));
#3824=EDGE_LOOP('',(#13736));
#3825=EDGE_LOOP('',(#13737));
#3826=EDGE_LOOP('',(#13738));
#3827=EDGE_LOOP('',(#13739,#13740));
#3828=EDGE_LOOP('',(#13741,#13742,#13743,#13744,#13745,#13746,#13747,#13748,
#13749));
#3829=EDGE_LOOP('',(#13750,#13751,#13752));
#3830=EDGE_LOOP('',(#13753,#13754,#13755,#13756));
#3831=EDGE_LOOP('',(#13757,#13758,#13759,#13760));
#3832=EDGE_LOOP('',(#13761,#13762,#13763,#13764));
#3833=EDGE_LOOP('',(#13765,#13766));
#3834=EDGE_LOOP('',(#13767));
#3835=EDGE_LOOP('',(#13768));
#3836=EDGE_LOOP('',(#13769));
#3837=EDGE_LOOP('',(#13770));
#3838=EDGE_LOOP('',(#13771,#13772,#13773,#13774));
#3839=EDGE_LOOP('',(#13775,#13776,#13777,#13778));
#3840=EDGE_LOOP('',(#13779));
#3841=EDGE_LOOP('',(#13780));
#3842=EDGE_LOOP('',(#13781));
#3843=EDGE_LOOP('',(#13782));
#3844=EDGE_LOOP('',(#13783,#13784,#13785,#13786));
#3845=EDGE_LOOP('',(#13787,#13788,#13789,#13790));
#3846=EDGE_LOOP('',(#13791));
#3847=EDGE_LOOP('',(#13792));
#3848=EDGE_LOOP('',(#13793));
#3849=EDGE_LOOP('',(#13794));
#3850=EDGE_LOOP('',(#13795,#13796,#13797,#13798));
#3851=EDGE_LOOP('',(#13799,#13800,#13801,#13802));
#3852=EDGE_LOOP('',(#13803));
#3853=EDGE_LOOP('',(#13804));
#3854=EDGE_LOOP('',(#13805));
#3855=EDGE_LOOP('',(#13806));
#3856=EDGE_LOOP('',(#13807,#13808,#13809,#13810));
#3857=EDGE_LOOP('',(#13811,#13812,#13813,#13814));
#3858=EDGE_LOOP('',(#13815));
#3859=EDGE_LOOP('',(#13816));
#3860=EDGE_LOOP('',(#13817));
#3861=EDGE_LOOP('',(#13818));
#3862=EDGE_LOOP('',(#13819,#13820,#13821,#13822));
#3863=EDGE_LOOP('',(#13823,#13824,#13825,#13826));
#3864=EDGE_LOOP('',(#13827,#13828,#13829,#13830));
#3865=EDGE_LOOP('',(#13831,#13832,#13833,#13834));
#3866=EDGE_LOOP('',(#13835,#13836,#13837,#13838));
#3867=EDGE_LOOP('',(#13839,#13840,#13841,#13842));
#3868=EDGE_LOOP('',(#13843,#13844,#13845,#13846,#13847,#13848));
#3869=EDGE_LOOP('',(#13849));
#3870=EDGE_LOOP('',(#13850,#13851,#13852,#13853,#13854,#13855));
#3871=EDGE_LOOP('',(#13856,#13857,#13858,#13859));
#3872=EDGE_LOOP('',(#13860,#13861,#13862,#13863));
#3873=EDGE_LOOP('',(#13864,#13865,#13866,#13867));
#3874=EDGE_LOOP('',(#13868));
#3875=EDGE_LOOP('',(#13869,#13870,#13871,#13872));
#3876=EDGE_LOOP('',(#13873,#13874,#13875,#13876));
#3877=EDGE_LOOP('',(#13877,#13878,#13879,#13880));
#3878=EDGE_LOOP('',(#13881,#13882,#13883,#13884,#13885,#13886,#13887,#13888,
#13889,#13890,#13891,#13892,#13893,#13894,#13895,#13896,#13897,#13898,#13899,
#13900,#13901,#13902,#13903,#13904,#13905,#13906,#13907,#13908,#13909,#13910,
#13911,#13912,#13913,#13914,#13915,#13916,#13917,#13918,#13919,#13920,#13921,
#13922,#13923,#13924,#13925,#13926,#13927,#13928,#13929,#13930,#13931,#13932,
#13933,#13934,#13935,#13936,#13937,#13938,#13939,#13940,#13941,#13942,#13943,
#13944,#13945,#13946,#13947,#13948,#13949,#13950,#13951,#13952,#13953,#13954,
#13955,#13956,#13957,#13958,#13959,#13960,#13961,#13962,#13963,#13964,#13965,
#13966,#13967,#13968,#13969,#13970,#13971,#13972,#13973,#13974,#13975,#13976,
#13977,#13978,#13979,#13980,#13981,#13982,#13983,#13984,#13985,#13986,#13987,
#13988,#13989,#13990,#13991,#13992,#13993,#13994,#13995,#13996,#13997,#13998,
#13999,#14000,#14001,#14002,#14003,#14004,#14005,#14006,#14007,#14008,#14009,
#14010,#14011,#14012,#14013,#14014,#14015,#14016,#14017,#14018,#14019,#14020,
#14021,#14022,#14023,#14024,#14025,#14026,#14027,#14028,#14029,#14030,#14031,
#14032,#14033,#14034,#14035,#14036,#14037,#14038,#14039,#14040));
#3879=EDGE_LOOP('',(#14041,#14042,#14043,#14044));
#3880=EDGE_LOOP('',(#14045,#14046,#14047,#14048));
#3881=EDGE_LOOP('',(#14049,#14050,#14051,#14052));
#3882=EDGE_LOOP('',(#14053));
#3883=EDGE_LOOP('',(#14054,#14055,#14056,#14057));
#3884=EDGE_LOOP('',(#14058,#14059,#14060,#14061));
#3885=EDGE_LOOP('',(#14062,#14063,#14064,#14065));
#3886=EDGE_LOOP('',(#14066,#14067,#14068,#14069));
#3887=EDGE_LOOP('',(#14070,#14071,#14072,#14073));
#3888=EDGE_LOOP('',(#14074,#14075,#14076,#14077));
#3889=EDGE_LOOP('',(#14078,#14079,#14080,#14081));
#3890=EDGE_LOOP('',(#14082,#14083,#14084,#14085));
#3891=EDGE_LOOP('',(#14086,#14087,#14088,#14089));
#3892=EDGE_LOOP('',(#14090,#14091,#14092,#14093));
#3893=EDGE_LOOP('',(#14094,#14095,#14096,#14097));
#3894=EDGE_LOOP('',(#14098,#14099,#14100,#14101));
#3895=EDGE_LOOP('',(#14102,#14103,#14104,#14105));
#3896=EDGE_LOOP('',(#14106,#14107,#14108,#14109));
#3897=EDGE_LOOP('',(#14110,#14111,#14112,#14113));
#3898=EDGE_LOOP('',(#14114,#14115,#14116,#14117));
#3899=EDGE_LOOP('',(#14118,#14119,#14120,#14121));
#3900=EDGE_LOOP('',(#14122,#14123,#14124,#14125));
#3901=EDGE_LOOP('',(#14126,#14127,#14128,#14129));
#3902=EDGE_LOOP('',(#14130,#14131,#14132,#14133));
#3903=EDGE_LOOP('',(#14134,#14135,#14136,#14137));
#3904=EDGE_LOOP('',(#14138,#14139,#14140,#14141));
#3905=EDGE_LOOP('',(#14142,#14143,#14144,#14145));
#3906=EDGE_LOOP('',(#14146,#14147,#14148,#14149));
#3907=EDGE_LOOP('',(#14150,#14151,#14152,#14153));
#3908=EDGE_LOOP('',(#14154,#14155,#14156,#14157));
#3909=EDGE_LOOP('',(#14158,#14159,#14160,#14161));
#3910=EDGE_LOOP('',(#14162,#14163,#14164,#14165));
#3911=EDGE_LOOP('',(#14166,#14167,#14168,#14169));
#3912=EDGE_LOOP('',(#14170,#14171,#14172,#14173));
#3913=EDGE_LOOP('',(#14174,#14175,#14176,#14177));
#3914=EDGE_LOOP('',(#14178,#14179,#14180,#14181));
#3915=EDGE_LOOP('',(#14182,#14183,#14184,#14185));
#3916=EDGE_LOOP('',(#14186,#14187,#14188,#14189));
#3917=EDGE_LOOP('',(#14190,#14191,#14192,#14193));
#3918=EDGE_LOOP('',(#14194,#14195,#14196,#14197));
#3919=EDGE_LOOP('',(#14198,#14199,#14200,#14201));
#3920=EDGE_LOOP('',(#14202,#14203,#14204,#14205));
#3921=EDGE_LOOP('',(#14206,#14207,#14208,#14209));
#3922=EDGE_LOOP('',(#14210,#14211,#14212,#14213));
#3923=EDGE_LOOP('',(#14214,#14215,#14216,#14217));
#3924=EDGE_LOOP('',(#14218,#14219,#14220,#14221));
#3925=EDGE_LOOP('',(#14222,#14223,#14224,#14225));
#3926=EDGE_LOOP('',(#14226,#14227,#14228,#14229));
#3927=EDGE_LOOP('',(#14230,#14231,#14232,#14233));
#3928=EDGE_LOOP('',(#14234,#14235,#14236,#14237));
#3929=EDGE_LOOP('',(#14238,#14239,#14240,#14241));
#3930=EDGE_LOOP('',(#14242,#14243,#14244,#14245));
#3931=EDGE_LOOP('',(#14246,#14247,#14248,#14249));
#3932=EDGE_LOOP('',(#14250,#14251,#14252,#14253));
#3933=EDGE_LOOP('',(#14254,#14255,#14256,#14257));
#3934=EDGE_LOOP('',(#14258,#14259,#14260,#14261));
#3935=EDGE_LOOP('',(#14262,#14263,#14264,#14265));
#3936=EDGE_LOOP('',(#14266,#14267,#14268,#14269));
#3937=EDGE_LOOP('',(#14270,#14271,#14272,#14273));
#3938=EDGE_LOOP('',(#14274,#14275,#14276,#14277));
#3939=EDGE_LOOP('',(#14278,#14279,#14280,#14281));
#3940=EDGE_LOOP('',(#14282,#14283,#14284,#14285));
#3941=EDGE_LOOP('',(#14286,#14287,#14288,#14289));
#3942=EDGE_LOOP('',(#14290,#14291,#14292,#14293));
#3943=EDGE_LOOP('',(#14294,#14295,#14296,#14297));
#3944=EDGE_LOOP('',(#14298,#14299,#14300,#14301));
#3945=EDGE_LOOP('',(#14302,#14303,#14304,#14305));
#3946=EDGE_LOOP('',(#14306,#14307,#14308,#14309));
#3947=EDGE_LOOP('',(#14310,#14311,#14312,#14313));
#3948=EDGE_LOOP('',(#14314,#14315,#14316,#14317));
#3949=EDGE_LOOP('',(#14318,#14319,#14320,#14321));
#3950=EDGE_LOOP('',(#14322,#14323,#14324,#14325));
#3951=EDGE_LOOP('',(#14326,#14327,#14328,#14329));
#3952=EDGE_LOOP('',(#14330,#14331,#14332,#14333));
#3953=EDGE_LOOP('',(#14334,#14335,#14336,#14337));
#3954=EDGE_LOOP('',(#14338,#14339,#14340,#14341));
#3955=EDGE_LOOP('',(#14342,#14343,#14344,#14345));
#3956=EDGE_LOOP('',(#14346,#14347,#14348,#14349));
#3957=EDGE_LOOP('',(#14350,#14351,#14352,#14353));
#3958=EDGE_LOOP('',(#14354,#14355,#14356,#14357));
#3959=EDGE_LOOP('',(#14358,#14359,#14360,#14361));
#3960=EDGE_LOOP('',(#14362,#14363,#14364,#14365));
#3961=EDGE_LOOP('',(#14366,#14367,#14368,#14369));
#3962=EDGE_LOOP('',(#14370,#14371,#14372,#14373));
#3963=EDGE_LOOP('',(#14374,#14375,#14376,#14377));
#3964=EDGE_LOOP('',(#14378,#14379,#14380,#14381));
#3965=EDGE_LOOP('',(#14382,#14383,#14384,#14385));
#3966=EDGE_LOOP('',(#14386,#14387,#14388,#14389));
#3967=EDGE_LOOP('',(#14390,#14391,#14392,#14393));
#3968=EDGE_LOOP('',(#14394,#14395,#14396,#14397));
#3969=EDGE_LOOP('',(#14398,#14399,#14400,#14401));
#3970=EDGE_LOOP('',(#14402,#14403,#14404,#14405));
#3971=EDGE_LOOP('',(#14406,#14407,#14408,#14409));
#3972=EDGE_LOOP('',(#14410,#14411,#14412,#14413));
#3973=EDGE_LOOP('',(#14414,#14415,#14416,#14417));
#3974=EDGE_LOOP('',(#14418,#14419,#14420,#14421));
#3975=EDGE_LOOP('',(#14422,#14423,#14424,#14425));
#3976=EDGE_LOOP('',(#14426,#14427,#14428,#14429));
#3977=EDGE_LOOP('',(#14430,#14431,#14432,#14433));
#3978=EDGE_LOOP('',(#14434,#14435,#14436,#14437));
#3979=EDGE_LOOP('',(#14438,#14439,#14440,#14441));
#3980=EDGE_LOOP('',(#14442,#14443,#14444,#14445));
#3981=EDGE_LOOP('',(#14446,#14447,#14448,#14449));
#3982=EDGE_LOOP('',(#14450,#14451,#14452,#14453));
#3983=EDGE_LOOP('',(#14454,#14455,#14456,#14457));
#3984=EDGE_LOOP('',(#14458,#14459,#14460,#14461));
#3985=EDGE_LOOP('',(#14462,#14463,#14464,#14465));
#3986=EDGE_LOOP('',(#14466,#14467,#14468,#14469));
#3987=EDGE_LOOP('',(#14470,#14471,#14472,#14473));
#3988=EDGE_LOOP('',(#14474,#14475,#14476,#14477));
#3989=EDGE_LOOP('',(#14478,#14479,#14480,#14481));
#3990=EDGE_LOOP('',(#14482,#14483,#14484,#14485));
#3991=EDGE_LOOP('',(#14486,#14487,#14488,#14489));
#3992=EDGE_LOOP('',(#14490,#14491,#14492,#14493));
#3993=EDGE_LOOP('',(#14494,#14495,#14496,#14497));
#3994=EDGE_LOOP('',(#14498,#14499,#14500,#14501));
#3995=EDGE_LOOP('',(#14502,#14503,#14504,#14505));
#3996=EDGE_LOOP('',(#14506,#14507,#14508,#14509));
#3997=EDGE_LOOP('',(#14510,#14511,#14512,#14513));
#3998=EDGE_LOOP('',(#14514,#14515,#14516,#14517));
#3999=EDGE_LOOP('',(#14518,#14519,#14520,#14521));
#4000=EDGE_LOOP('',(#14522,#14523,#14524,#14525));
#4001=EDGE_LOOP('',(#14526,#14527,#14528,#14529));
#4002=EDGE_LOOP('',(#14530,#14531,#14532,#14533));
#4003=EDGE_LOOP('',(#14534,#14535,#14536,#14537));
#4004=EDGE_LOOP('',(#14538,#14539,#14540,#14541));
#4005=EDGE_LOOP('',(#14542,#14543,#14544,#14545));
#4006=EDGE_LOOP('',(#14546,#14547,#14548,#14549));
#4007=EDGE_LOOP('',(#14550,#14551,#14552,#14553));
#4008=EDGE_LOOP('',(#14554,#14555,#14556,#14557));
#4009=EDGE_LOOP('',(#14558,#14559,#14560,#14561));
#4010=EDGE_LOOP('',(#14562,#14563,#14564,#14565));
#4011=EDGE_LOOP('',(#14566,#14567,#14568,#14569));
#4012=EDGE_LOOP('',(#14570,#14571,#14572,#14573));
#4013=EDGE_LOOP('',(#14574,#14575,#14576,#14577));
#4014=EDGE_LOOP('',(#14578,#14579,#14580,#14581));
#4015=EDGE_LOOP('',(#14582,#14583,#14584,#14585));
#4016=EDGE_LOOP('',(#14586,#14587,#14588,#14589));
#4017=EDGE_LOOP('',(#14590,#14591,#14592,#14593));
#4018=EDGE_LOOP('',(#14594,#14595,#14596,#14597));
#4019=EDGE_LOOP('',(#14598,#14599,#14600,#14601));
#4020=EDGE_LOOP('',(#14602,#14603,#14604,#14605));
#4021=EDGE_LOOP('',(#14606,#14607,#14608,#14609));
#4022=EDGE_LOOP('',(#14610,#14611,#14612,#14613));
#4023=EDGE_LOOP('',(#14614,#14615,#14616,#14617));
#4024=EDGE_LOOP('',(#14618,#14619,#14620,#14621));
#4025=EDGE_LOOP('',(#14622,#14623,#14624,#14625));
#4026=EDGE_LOOP('',(#14626,#14627,#14628,#14629));
#4027=EDGE_LOOP('',(#14630,#14631,#14632,#14633));
#4028=EDGE_LOOP('',(#14634,#14635,#14636,#14637));
#4029=EDGE_LOOP('',(#14638,#14639,#14640,#14641));
#4030=EDGE_LOOP('',(#14642,#14643,#14644,#14645));
#4031=EDGE_LOOP('',(#14646,#14647,#14648,#14649));
#4032=EDGE_LOOP('',(#14650,#14651,#14652,#14653));
#4033=EDGE_LOOP('',(#14654,#14655,#14656,#14657));
#4034=EDGE_LOOP('',(#14658,#14659,#14660,#14661));
#4035=EDGE_LOOP('',(#14662,#14663,#14664,#14665));
#4036=EDGE_LOOP('',(#14666,#14667,#14668,#14669));
#4037=EDGE_LOOP('',(#14670,#14671,#14672,#14673));
#4038=EDGE_LOOP('',(#14674,#14675,#14676,#14677));
#4039=EDGE_LOOP('',(#14678,#14679,#14680,#14681));
#4040=EDGE_LOOP('',(#14682,#14683,#14684,#14685));
#4041=EDGE_LOOP('',(#14686,#14687,#14688,#14689));
#4042=EDGE_LOOP('',(#14690,#14691,#14692,#14693));
#4043=EDGE_LOOP('',(#14694,#14695,#14696,#14697,#14698,#14699,#14700,#14701,
#14702,#14703,#14704,#14705,#14706,#14707,#14708,#14709,#14710,#14711,#14712,
#14713,#14714,#14715,#14716,#14717,#14718,#14719,#14720,#14721,#14722,#14723,
#14724,#14725,#14726,#14727,#14728,#14729,#14730,#14731,#14732,#14733,#14734,
#14735,#14736,#14737,#14738,#14739,#14740,#14741,#14742,#14743,#14744,#14745,
#14746,#14747,#14748,#14749,#14750,#14751,#14752,#14753,#14754,#14755,#14756,
#14757,#14758,#14759,#14760,#14761,#14762,#14763,#14764,#14765,#14766,#14767,
#14768,#14769,#14770,#14771,#14772,#14773,#14774,#14775,#14776,#14777,#14778,
#14779,#14780,#14781,#14782,#14783,#14784,#14785,#14786,#14787,#14788,#14789,
#14790,#14791,#14792,#14793,#14794,#14795,#14796,#14797,#14798,#14799,#14800,
#14801,#14802,#14803,#14804,#14805,#14806,#14807,#14808,#14809,#14810,#14811,
#14812,#14813,#14814,#14815,#14816,#14817,#14818,#14819,#14820,#14821,#14822,
#14823,#14824,#14825,#14826,#14827,#14828,#14829,#14830,#14831,#14832,#14833,
#14834,#14835,#14836,#14837,#14838,#14839,#14840,#14841,#14842,#14843,#14844,
#14845,#14846,#14847,#14848,#14849,#14850,#14851,#14852,#14853));
#4044=EDGE_LOOP('',(#14854));
#4045=EDGE_LOOP('',(#14855,#14856,#14857,#14858));
#4046=EDGE_LOOP('',(#14859,#14860,#14861,#14862,#14863,#14864,#14865,#14866));
#4047=EDGE_LOOP('',(#14867,#14868,#14869,#14870));
#4048=EDGE_LOOP('',(#14871,#14872,#14873,#14874));
#4049=EDGE_LOOP('',(#14875,#14876,#14877,#14878));
#4050=EDGE_LOOP('',(#14879,#14880,#14881,#14882));
#4051=EDGE_LOOP('',(#14883,#14884,#14885,#14886,#14887,#14888,#14889,#14890));
#4052=EDGE_LOOP('',(#14891,#14892,#14893,#14894));
#4053=EDGE_LOOP('',(#14895,#14896,#14897,#14898));
#4054=EDGE_LOOP('',(#14899,#14900,#14901,#14902));
#4055=EDGE_LOOP('',(#14903,#14904,#14905,#14906));
#4056=LINE('',#22781,#5080);
#4057=LINE('',#22787,#5081);
#4058=LINE('',#22793,#5082);
#4059=LINE('',#22799,#5083);
#4060=LINE('',#22804,#5084);
#4061=LINE('',#22806,#5085);
#4062=LINE('',#22808,#5086);
#4063=LINE('',#22809,#5087);
#4064=LINE('',#22812,#5088);
#4065=LINE('',#22814,#5089);
#4066=LINE('',#22815,#5090);
#4067=LINE('',#22818,#5091);
#4068=LINE('',#22820,#5092);
#4069=LINE('',#22821,#5093);
#4070=LINE('',#22823,#5094);
#4071=LINE('',#22824,#5095);
#4072=LINE('',#22832,#5096);
#4073=LINE('',#22839,#5097);
#4074=LINE('',#22846,#5098);
#4075=LINE('',#22853,#5099);
#4076=LINE('',#22859,#5100);
#4077=LINE('',#22863,#5101);
#4078=LINE('',#22867,#5102);
#4079=LINE('',#22870,#5103);
#4080=LINE('',#22873,#5104);
#4081=LINE('',#22875,#5105);
#4082=LINE('',#22877,#5106);
#4083=LINE('',#22879,#5107);
#4084=LINE('',#22881,#5108);
#4085=LINE('',#22883,#5109);
#4086=LINE('',#22885,#5110);
#4087=LINE('',#22887,#5111);
#4088=LINE('',#22889,#5112);
#4089=LINE('',#22893,#5113);
#4090=LINE('',#22896,#5114);
#4091=LINE('',#22907,#5115);
#4092=LINE('',#22909,#5116);
#4093=LINE('',#22911,#5117);
#4094=LINE('',#22913,#5118);
#4095=LINE('',#22915,#5119);
#4096=LINE('',#22917,#5120);
#4097=LINE('',#22919,#5121);
#4098=LINE('',#22921,#5122);
#4099=LINE('',#22922,#5123);
#4100=LINE('',#22937,#5124);
#4101=LINE('',#22942,#5125);
#4102=LINE('',#22945,#5126);
#4103=LINE('',#22949,#5127);
#4104=LINE('',#22953,#5128);
#4105=LINE('',#22955,#5129);
#4106=LINE('',#22957,#5130);
#4107=LINE('',#22959,#5131);
#4108=LINE('',#22961,#5132);
#4109=LINE('',#22963,#5133);
#4110=LINE('',#22965,#5134);
#4111=LINE('',#22966,#5135);
#4112=LINE('',#22977,#5136);
#4113=LINE('',#22979,#5137);
#4114=LINE('',#22981,#5138);
#4115=LINE('',#22983,#5139);
#4116=LINE('',#22984,#5140);
#4117=LINE('',#22989,#5141);
#4118=LINE('',#22993,#5142);
#4119=LINE('',#22997,#5143);
#4120=LINE('',#23001,#5144);
#4121=LINE('',#23003,#5145);
#4122=LINE('',#23005,#5146);
#4123=LINE('',#23006,#5147);
#4124=LINE('',#23009,#5148);
#4125=LINE('',#23011,#5149);
#4126=LINE('',#23012,#5150);
#4127=LINE('',#23016,#5151);
#4128=LINE('',#23021,#5152);
#4129=LINE('',#23025,#5153);
#4130=LINE('',#23030,#5154);
#4131=LINE('',#23035,#5155);
#4132=LINE('',#23039,#5156);
#4133=LINE('',#23044,#5157);
#4134=LINE('',#23048,#5158);
#4135=LINE('',#23051,#5159);
#4136=LINE('',#23053,#5160);
#4137=LINE('',#23055,#5161);
#4138=LINE('',#23057,#5162);
#4139=LINE('',#23058,#5163);
#4140=LINE('',#23060,#5164);
#4141=LINE('',#23065,#5165);
#4142=LINE('',#23067,#5166);
#4143=LINE('',#23069,#5167);
#4144=LINE('',#23071,#5168);
#4145=LINE('',#23075,#5169);
#4146=LINE('',#23077,#5170);
#4147=LINE('',#23078,#5171);
#4148=LINE('',#23082,#5172);
#4149=LINE('',#23087,#5173);
#4150=LINE('',#23091,#5174);
#4151=LINE('',#23096,#5175);
#4152=LINE('',#23101,#5176);
#4153=LINE('',#23105,#5177);
#4154=LINE('',#23108,#5178);
#4155=LINE('',#23110,#5179);
#4156=LINE('',#23112,#5180);
#4157=LINE('',#23113,#5181);
#4158=LINE('',#23114,#5182);
#4159=LINE('',#23115,#5183);
#4160=LINE('',#23136,#5184);
#4161=LINE('',#23145,#5185);
#4162=LINE('',#23154,#5186);
#4163=LINE('',#23163,#5187);
#4164=LINE('',#23171,#5188);
#4165=LINE('',#23175,#5189);
#4166=LINE('',#23179,#5190);
#4167=LINE('',#23183,#5191);
#4168=LINE('',#23187,#5192);
#4169=LINE('',#23192,#5193);
#4170=LINE('',#23197,#5194);
#4171=LINE('',#23202,#5195);
#4172=LINE('',#23207,#5196);
#4173=LINE('',#23211,#5197);
#4174=LINE('',#23215,#5198);
#4175=LINE('',#23219,#5199);
#4176=LINE('',#23223,#5200);
#4177=LINE('',#23227,#5201);
#4178=LINE('',#23229,#5202);
#4179=LINE('',#23231,#5203);
#4180=LINE('',#23233,#5204);
#4181=LINE('',#23235,#5205);
#4182=LINE('',#23237,#5206);
#4183=LINE('',#23239,#5207);
#4184=LINE('',#23241,#5208);
#4185=LINE('',#23244,#5209);
#4186=LINE('',#23251,#5210);
#4187=LINE('',#23257,#5211);
#4188=LINE('',#23263,#5212);
#4189=LINE('',#23269,#5213);
#4190=LINE('',#23274,#5214);
#4191=LINE('',#23276,#5215);
#4192=LINE('',#23278,#5216);
#4193=LINE('',#23279,#5217);
#4194=LINE('',#23282,#5218);
#4195=LINE('',#23284,#5219);
#4196=LINE('',#23285,#5220);
#4197=LINE('',#23288,#5221);
#4198=LINE('',#23290,#5222);
#4199=LINE('',#23291,#5223);
#4200=LINE('',#23293,#5224);
#4201=LINE('',#23294,#5225);
#4202=LINE('',#23299,#5226);
#4203=LINE('',#23306,#5227);
#4204=LINE('',#23313,#5228);
#4205=LINE('',#23320,#5229);
#4206=LINE('',#23326,#5230);
#4207=LINE('',#23330,#5231);
#4208=LINE('',#23334,#5232);
#4209=LINE('',#23337,#5233);
#4210=LINE('',#23340,#5234);
#4211=LINE('',#23343,#5235);
#4212=LINE('',#23346,#5236);
#4213=LINE('',#23348,#5237);
#4214=LINE('',#23350,#5238);
#4215=LINE('',#23352,#5239);
#4216=LINE('',#23354,#5240);
#4217=LINE('',#23356,#5241);
#4218=LINE('',#23358,#5242);
#4219=LINE('',#23360,#5243);
#4220=LINE('',#23361,#5244);
#4221=LINE('',#23375,#5245);
#4222=LINE('',#23380,#5246);
#4223=LINE('',#23384,#5247);
#4224=LINE('',#23386,#5248);
#4225=LINE('',#23388,#5249);
#4226=LINE('',#23390,#5250);
#4227=LINE('',#23392,#5251);
#4228=LINE('',#23394,#5252);
#4229=LINE('',#23396,#5253);
#4230=LINE('',#23398,#5254);
#4231=LINE('',#23402,#5255);
#4232=LINE('',#23405,#5256);
#4233=LINE('',#23416,#5257);
#4234=LINE('',#23420,#5258);
#4235=LINE('',#23424,#5259);
#4236=LINE('',#23428,#5260);
#4237=LINE('',#23430,#5261);
#4238=LINE('',#23432,#5262);
#4239=LINE('',#23434,#5263);
#4240=LINE('',#23436,#5264);
#4241=LINE('',#23438,#5265);
#4242=LINE('',#23440,#5266);
#4243=LINE('',#23441,#5267);
#4244=LINE('',#23452,#5268);
#4245=LINE('',#23456,#5269);
#4246=LINE('',#23460,#5270);
#4247=LINE('',#23462,#5271);
#4248=LINE('',#23464,#5272);
#4249=LINE('',#23465,#5273);
#4250=LINE('',#23468,#5274);
#4251=LINE('',#23470,#5275);
#4252=LINE('',#23471,#5276);
#4253=LINE('',#23474,#5277);
#4254=LINE('',#23476,#5278);
#4255=LINE('',#23478,#5279);
#4256=LINE('',#23479,#5280);
#4257=LINE('',#23483,#5281);
#4258=LINE('',#23488,#5282);
#4259=LINE('',#23492,#5283);
#4260=LINE('',#23497,#5284);
#4261=LINE('',#23503,#5285);
#4262=LINE('',#23507,#5286);
#4263=LINE('',#23511,#5287);
#4264=LINE('',#23514,#5288);
#4265=LINE('',#23518,#5289);
#4266=LINE('',#23521,#5290);
#4267=LINE('',#23524,#5291);
#4268=LINE('',#23526,#5292);
#4269=LINE('',#23527,#5293);
#4270=LINE('',#23530,#5294);
#4271=LINE('',#23532,#5295);
#4272=LINE('',#23534,#5296);
#4273=LINE('',#23535,#5297);
#4274=LINE('',#23539,#5298);
#4275=LINE('',#23544,#5299);
#4276=LINE('',#23548,#5300);
#4277=LINE('',#23553,#5301);
#4278=LINE('',#23559,#5302);
#4279=LINE('',#23563,#5303);
#4280=LINE('',#23566,#5304);
#4281=LINE('',#23570,#5305);
#4282=LINE('',#23573,#5306);
#4283=LINE('',#23577,#5307);
#4284=LINE('',#23580,#5308);
#4285=LINE('',#23582,#5309);
#4286=LINE('',#23584,#5310);
#4287=LINE('',#23585,#5311);
#4288=LINE('',#23587,#5312);
#4289=LINE('',#23588,#5313);
#4290=LINE('',#23601,#5314);
#4291=LINE('',#23606,#5315);
#4292=LINE('',#23611,#5316);
#4293=LINE('',#23616,#5317);
#4294=LINE('',#23621,#5318);
#4295=LINE('',#23625,#5319);
#4296=LINE('',#23629,#5320);
#4297=LINE('',#23633,#5321);
#4298=LINE('',#23637,#5322);
#4299=LINE('',#23641,#5323);
#4300=LINE('',#23644,#5324);
#4301=LINE('',#23646,#5325);
#4302=LINE('',#23648,#5326);
#4303=LINE('',#23650,#5327);
#4304=LINE('',#23652,#5328);
#4305=LINE('',#23654,#5329);
#4306=LINE('',#23656,#5330);
#4307=LINE('',#23659,#5331);
#4308=LINE('',#23666,#5332);
#4309=LINE('',#23675,#5333);
#4310=LINE('',#23684,#5334);
#4311=LINE('',#23693,#5335);
#4312=LINE('',#23701,#5336);
#4313=LINE('',#23705,#5337);
#4314=LINE('',#23710,#5338);
#4315=LINE('',#23714,#5339);
#4316=LINE('',#23719,#5340);
#4317=LINE('',#23723,#5341);
#4318=LINE('',#23728,#5342);
#4319=LINE('',#23732,#5343);
#4320=LINE('',#23753,#5344);
#4321=LINE('',#23759,#5345);
#4322=LINE('',#23765,#5346);
#4323=LINE('',#23769,#5347);
#4324=LINE('',#23774,#5348);
#4325=LINE('',#23778,#5349);
#4326=LINE('',#23783,#5350);
#4327=LINE('',#23787,#5351);
#4328=LINE('',#23792,#5352);
#4329=LINE('',#23796,#5353);
#4330=LINE('',#23815,#5354);
#4331=LINE('',#23823,#5355);
#4332=LINE('',#23830,#5356);
#4333=LINE('',#23836,#5357);
#4334=LINE('',#23842,#5358);
#4335=LINE('',#23848,#5359);
#4336=LINE('',#23854,#5360);
#4337=LINE('',#23861,#5361);
#4338=LINE('',#23867,#5362);
#4339=LINE('',#23876,#5363);
#4340=LINE('',#23882,#5364);
#4341=LINE('',#23888,#5365);
#4342=LINE('',#23894,#5366);
#4343=LINE('',#23900,#5367);
#4344=LINE('',#23908,#5368);
#4345=LINE('',#23913,#5369);
#4346=LINE('',#23922,#5370);
#4347=LINE('',#23928,#5371);
#4348=LINE('',#23934,#5372);
#4349=LINE('',#23940,#5373);
#4350=LINE('',#23946,#5374);
#4351=LINE('',#23953,#5375);
#4352=LINE('',#23959,#5376);
#4353=LINE('',#23968,#5377);
#4354=LINE('',#23974,#5378);
#4355=LINE('',#23980,#5379);
#4356=LINE('',#23986,#5380);
#4357=LINE('',#23992,#5381);
#4358=LINE('',#24000,#5382);
#4359=LINE('',#24005,#5383);
#4360=LINE('',#24014,#5384);
#4361=LINE('',#24020,#5385);
#4362=LINE('',#24026,#5386);
#4363=LINE('',#24032,#5387);
#4364=LINE('',#24037,#5388);
#4365=LINE('',#24039,#5389);
#4366=LINE('',#24041,#5390);
#4367=LINE('',#24042,#5391);
#4368=LINE('',#24045,#5392);
#4369=LINE('',#24047,#5393);
#4370=LINE('',#24048,#5394);
#4371=LINE('',#24051,#5395);
#4372=LINE('',#24053,#5396);
#4373=LINE('',#24054,#5397);
#4374=LINE('',#24056,#5398);
#4375=LINE('',#24057,#5399);
#4376=LINE('',#24064,#5400);
#4377=LINE('',#24066,#5401);
#4378=LINE('',#24068,#5402);
#4379=LINE('',#24069,#5403);
#4380=LINE('',#24072,#5404);
#4381=LINE('',#24074,#5405);
#4382=LINE('',#24075,#5406);
#4383=LINE('',#24078,#5407);
#4384=LINE('',#24080,#5408);
#4385=LINE('',#24081,#5409);
#4386=LINE('',#24083,#5410);
#4387=LINE('',#24084,#5411);
#4388=LINE('',#24091,#5412);
#4389=LINE('',#24093,#5413);
#4390=LINE('',#24095,#5414);
#4391=LINE('',#24096,#5415);
#4392=LINE('',#24099,#5416);
#4393=LINE('',#24101,#5417);
#4394=LINE('',#24102,#5418);
#4395=LINE('',#24105,#5419);
#4396=LINE('',#24107,#5420);
#4397=LINE('',#24108,#5421);
#4398=LINE('',#24110,#5422);
#4399=LINE('',#24111,#5423);
#4400=LINE('',#24118,#5424);
#4401=LINE('',#24120,#5425);
#4402=LINE('',#24122,#5426);
#4403=LINE('',#24123,#5427);
#4404=LINE('',#24126,#5428);
#4405=LINE('',#24128,#5429);
#4406=LINE('',#24129,#5430);
#4407=LINE('',#24132,#5431);
#4408=LINE('',#24134,#5432);
#4409=LINE('',#24135,#5433);
#4410=LINE('',#24138,#5434);
#4411=LINE('',#24140,#5435);
#4412=LINE('',#24141,#5436);
#4413=LINE('',#24144,#5437);
#4414=LINE('',#24146,#5438);
#4415=LINE('',#24147,#5439);
#4416=LINE('',#24149,#5440);
#4417=LINE('',#24150,#5441);
#4418=LINE('',#24162,#5442);
#4419=LINE('',#24166,#5443);
#4420=LINE('',#24170,#5444);
#4421=LINE('',#24177,#5445);
#4422=LINE('',#24179,#5446);
#4423=LINE('',#24194,#5447);
#4424=LINE('',#24200,#5448);
#4425=LINE('',#24204,#5449);
#4426=LINE('',#24210,#5450);
#4427=LINE('',#24215,#5451);
#4428=LINE('',#24230,#5452);
#4429=LINE('',#24239,#5453);
#4430=LINE('',#24243,#5454);
#4431=LINE('',#24247,#5455);
#4432=LINE('',#24250,#5456);
#4433=LINE('',#24386,#5457);
#4434=LINE('',#24639,#5458);
#4435=LINE('',#24681,#5459);
#4436=LINE('',#24686,#5460);
#4437=LINE('',#24695,#5461);
#4438=LINE('',#24700,#5462);
#4439=LINE('',#24720,#5463);
#4440=LINE('',#24726,#5464);
#4441=LINE('',#24730,#5465);
#4442=LINE('',#24736,#5466);
#4443=LINE('',#24741,#5467);
#4444=LINE('',#24756,#5468);
#4445=LINE('',#24765,#5469);
#4446=LINE('',#24769,#5470);
#4447=LINE('',#24773,#5471);
#4448=LINE('',#24776,#5472);
#4449=LINE('',#24929,#5473);
#4450=LINE('',#25225,#5474);
#4451=LINE('',#25267,#5475);
#4452=LINE('',#25272,#5476);
#4453=LINE('',#25281,#5477);
#4454=LINE('',#25286,#5478);
#4455=LINE('',#25299,#5479);
#4456=LINE('',#25303,#5480);
#4457=LINE('',#25307,#5481);
#4458=LINE('',#25314,#5482);
#4459=LINE('',#25318,#5483);
#4460=LINE('',#25322,#5484);
#4461=LINE('',#25327,#5485);
#4462=LINE('',#25329,#5486);
#4463=LINE('',#25331,#5487);
#4464=LINE('',#25332,#5488);
#4465=LINE('',#25335,#5489);
#4466=LINE('',#25337,#5490);
#4467=LINE('',#25338,#5491);
#4468=LINE('',#25341,#5492);
#4469=LINE('',#25343,#5493);
#4470=LINE('',#25344,#5494);
#4471=LINE('',#25347,#5495);
#4472=LINE('',#25349,#5496);
#4473=LINE('',#25350,#5497);
#4474=LINE('',#25353,#5498);
#4475=LINE('',#25355,#5499);
#4476=LINE('',#25356,#5500);
#4477=LINE('',#25358,#5501);
#4478=LINE('',#25359,#5502);
#4479=LINE('',#25427,#5503);
#4480=LINE('',#25429,#5504);
#4481=LINE('',#25431,#5505);
#4482=LINE('',#25432,#5506);
#4483=LINE('',#25437,#5507);
#4484=LINE('',#25438,#5508);
#4485=LINE('',#25441,#5509);
#4486=LINE('',#25443,#5510);
#4487=LINE('',#25444,#5511);
#4488=LINE('',#25446,#5512);
#4489=LINE('',#25453,#5513);
#4490=LINE('',#25461,#5514);
#4491=LINE('',#25478,#5515);
#4492=LINE('',#25529,#5516);
#4493=LINE('',#25534,#5517);
#4494=LINE('',#25540,#5518);
#4495=LINE('',#25548,#5519);
#4496=LINE('',#25565,#5520);
#4497=LINE('',#25616,#5521);
#4498=LINE('',#25621,#5522);
#4499=LINE('',#25627,#5523);
#4500=LINE('',#25636,#5524);
#4501=LINE('',#25642,#5525);
#4502=LINE('',#25651,#5526);
#4503=LINE('',#25657,#5527);
#4504=LINE('',#25666,#5528);
#4505=LINE('',#25672,#5529);
#4506=LINE('',#25681,#5530);
#4507=LINE('',#25687,#5531);
#4508=LINE('',#25695,#5532);
#4509=LINE('',#25697,#5533);
#4510=LINE('',#25699,#5534);
#4511=LINE('',#25700,#5535);
#4512=LINE('',#25703,#5536);
#4513=LINE('',#25705,#5537);
#4514=LINE('',#25706,#5538);
#4515=LINE('',#25709,#5539);
#4516=LINE('',#25711,#5540);
#4517=LINE('',#25712,#5541);
#4518=LINE('',#25789,#5542);
#4519=LINE('',#25935,#5543);
#4520=LINE('',#26081,#5544);
#4521=LINE('',#26227,#5545);
#4522=LINE('',#26373,#5546);
#4523=LINE('',#26519,#5547);
#4524=LINE('',#26665,#5548);
#4525=LINE('',#26811,#5549);
#4526=LINE('',#26957,#5550);
#4527=LINE('',#27103,#5551);
#4528=LINE('',#27249,#5552);
#4529=LINE('',#27395,#5553);
#4530=LINE('',#27541,#5554);
#4531=LINE('',#27687,#5555);
#4532=LINE('',#27833,#5556);
#4533=LINE('',#27979,#5557);
#4534=LINE('',#28125,#5558);
#4535=LINE('',#28271,#5559);
#4536=LINE('',#28417,#5560);
#4537=LINE('',#28563,#5561);
#4538=LINE('',#28641,#5562);
#4539=LINE('',#28785,#5563);
#4540=LINE('',#28857,#5564);
#4541=LINE('',#28860,#5565);
#4542=LINE('',#28861,#5566);
#4543=LINE('',#29073,#5567);
#4544=LINE('',#29077,#5568);
#4545=LINE('',#29289,#5569);
#4546=LINE('',#29292,#5570);
#4547=LINE('',#29293,#5571);
#4548=LINE('',#29505,#5572);
#4549=LINE('',#29509,#5573);
#4550=LINE('',#29721,#5574);
#4551=LINE('',#29724,#5575);
#4552=LINE('',#29725,#5576);
#4553=LINE('',#29937,#5577);
#4554=LINE('',#29941,#5578);
#4555=LINE('',#30153,#5579);
#4556=LINE('',#30156,#5580);
#4557=LINE('',#30157,#5581);
#4558=LINE('',#30369,#5582);
#4559=LINE('',#30373,#5583);
#4560=LINE('',#30585,#5584);
#4561=LINE('',#30588,#5585);
#4562=LINE('',#30589,#5586);
#4563=LINE('',#30801,#5587);
#4564=LINE('',#30805,#5588);
#4565=LINE('',#31017,#5589);
#4566=LINE('',#31020,#5590);
#4567=LINE('',#31021,#5591);
#4568=LINE('',#31233,#5592);
#4569=LINE('',#31237,#5593);
#4570=LINE('',#31449,#5594);
#4571=LINE('',#31452,#5595);
#4572=LINE('',#31453,#5596);
#4573=LINE('',#31665,#5597);
#4574=LINE('',#31669,#5598);
#4575=LINE('',#31881,#5599);
#4576=LINE('',#31884,#5600);
#4577=LINE('',#31885,#5601);
#4578=LINE('',#32097,#5602);
#4579=LINE('',#32101,#5603);
#4580=LINE('',#32313,#5604);
#4581=LINE('',#32316,#5605);
#4582=LINE('',#32317,#5606);
#4583=LINE('',#32529,#5607);
#4584=LINE('',#32533,#5608);
#4585=LINE('',#32745,#5609);
#4586=LINE('',#32748,#5610);
#4587=LINE('',#32749,#5611);
#4588=LINE('',#32961,#5612);
#4589=LINE('',#32965,#5613);
#4590=LINE('',#33177,#5614);
#4591=LINE('',#33180,#5615);
#4592=LINE('',#33181,#5616);
#4593=LINE('',#33393,#5617);
#4594=LINE('',#33397,#5618);
#4595=LINE('',#33609,#5619);
#4596=LINE('',#33612,#5620);
#4597=LINE('',#33613,#5621);
#4598=LINE('',#33825,#5622);
#4599=LINE('',#33829,#5623);
#4600=LINE('',#34041,#5624);
#4601=LINE('',#34044,#5625);
#4602=LINE('',#34045,#5626);
#4603=LINE('',#34257,#5627);
#4604=LINE('',#34261,#5628);
#4605=LINE('',#34473,#5629);
#4606=LINE('',#34476,#5630);
#4607=LINE('',#34477,#5631);
#4608=LINE('',#34689,#5632);
#4609=LINE('',#34693,#5633);
#4610=LINE('',#34905,#5634);
#4611=LINE('',#34908,#5635);
#4612=LINE('',#34909,#5636);
#4613=LINE('',#35121,#5637);
#4614=LINE('',#35125,#5638);
#4615=LINE('',#35337,#5639);
#4616=LINE('',#35340,#5640);
#4617=LINE('',#35341,#5641);
#4618=LINE('',#35553,#5642);
#4619=LINE('',#35557,#5643);
#4620=LINE('',#35769,#5644);
#4621=LINE('',#35772,#5645);
#4622=LINE('',#35773,#5646);
#4623=LINE('',#35985,#5647);
#4624=LINE('',#35989,#5648);
#4625=LINE('',#36201,#5649);
#4626=LINE('',#36204,#5650);
#4627=LINE('',#36205,#5651);
#4628=LINE('',#36417,#5652);
#4629=LINE('',#36421,#5653);
#4630=LINE('',#36633,#5654);
#4631=LINE('',#36636,#5655);
#4632=LINE('',#36637,#5656);
#4633=LINE('',#36849,#5657);
#4634=LINE('',#36853,#5658);
#4635=LINE('',#37065,#5659);
#4636=LINE('',#37068,#5660);
#4637=LINE('',#37069,#5661);
#4638=LINE('',#37281,#5662);
#4639=LINE('',#37289,#5663);
#4640=LINE('',#37291,#5664);
#4641=LINE('',#37293,#5665);
#4642=LINE('',#37295,#5666);
#4643=LINE('',#37297,#5667);
#4644=LINE('',#37299,#5668);
#4645=LINE('',#37301,#5669);
#4646=LINE('',#37302,#5670);
#4647=LINE('',#37305,#5671);
#4648=LINE('',#37307,#5672);
#4649=LINE('',#37308,#5673);
#4650=LINE('',#37311,#5674);
#4651=LINE('',#37312,#5675);
#4652=LINE('',#37315,#5676);
#4653=LINE('',#37316,#5677);
#4654=LINE('',#37319,#5678);
#4655=LINE('',#37320,#5679);
#4656=LINE('',#37323,#5680);
#4657=LINE('',#37325,#5681);
#4658=LINE('',#37327,#5682);
#4659=LINE('',#37328,#5683);
#4660=LINE('',#37330,#5684);
#4661=LINE('',#37332,#5685);
#4662=LINE('',#37334,#5686);
#4663=LINE('',#37341,#5687);
#4664=LINE('',#37343,#5688);
#4665=LINE('',#37345,#5689);
#4666=LINE('',#37346,#5690);
#4667=LINE('',#37351,#5691);
#4668=LINE('',#37352,#5692);
#4669=LINE('',#37355,#5693);
#4670=LINE('',#37357,#5694);
#4671=LINE('',#37358,#5695);
#4672=LINE('',#37360,#5696);
#4673=LINE('',#37366,#5697);
#4674=LINE('',#37368,#5698);
#4675=LINE('',#37370,#5699);
#4676=LINE('',#37371,#5700);
#4677=LINE('',#37376,#5701);
#4678=LINE('',#37377,#5702);
#4679=LINE('',#37380,#5703);
#4680=LINE('',#37382,#5704);
#4681=LINE('',#37383,#5705);
#4682=LINE('',#37385,#5706);
#4683=LINE('',#37392,#5707);
#4684=LINE('',#37400,#5708);
#4685=LINE('',#37421,#5709);
#4686=LINE('',#37476,#5710);
#4687=LINE('',#37481,#5711);
#4688=LINE('',#37487,#5712);
#4689=LINE('',#37495,#5713);
#4690=LINE('',#37516,#5714);
#4691=LINE('',#37571,#5715);
#4692=LINE('',#37576,#5716);
#4693=LINE('',#37582,#5717);
#4694=LINE('',#37591,#5718);
#4695=LINE('',#37597,#5719);
#4696=LINE('',#37606,#5720);
#4697=LINE('',#37612,#5721);
#4698=LINE('',#37621,#5722);
#4699=LINE('',#37627,#5723);
#4700=LINE('',#37636,#5724);
#4701=LINE('',#37642,#5725);
#4702=LINE('',#37651,#5726);
#4703=LINE('',#37657,#5727);
#4704=LINE('',#37665,#5728);
#4705=LINE('',#37667,#5729);
#4706=LINE('',#37669,#5730);
#4707=LINE('',#37670,#5731);
#4708=LINE('',#37673,#5732);
#4709=LINE('',#37675,#5733);
#4710=LINE('',#37676,#5734);
#4711=LINE('',#37679,#5735);
#4712=LINE('',#37681,#5736);
#4713=LINE('',#37682,#5737);
#4714=LINE('',#37765,#5738);
#4715=LINE('',#37911,#5739);
#4716=LINE('',#38057,#5740);
#4717=LINE('',#38203,#5741);
#4718=LINE('',#38349,#5742);
#4719=LINE('',#38495,#5743);
#4720=LINE('',#38641,#5744);
#4721=LINE('',#38787,#5745);
#4722=LINE('',#38933,#5746);
#4723=LINE('',#39079,#5747);
#4724=LINE('',#39225,#5748);
#4725=LINE('',#39371,#5749);
#4726=LINE('',#39517,#5750);
#4727=LINE('',#39663,#5751);
#4728=LINE('',#39809,#5752);
#4729=LINE('',#39955,#5753);
#4730=LINE('',#40101,#5754);
#4731=LINE('',#40247,#5755);
#4732=LINE('',#40393,#5756);
#4733=LINE('',#40539,#5757);
#4734=LINE('',#40612,#5758);
#4735=LINE('',#40755,#5759);
#4736=LINE('',#40827,#5760);
#4737=LINE('',#40830,#5761);
#4738=LINE('',#40831,#5762);
#4739=LINE('',#41043,#5763);
#4740=LINE('',#41047,#5764);
#4741=LINE('',#41259,#5765);
#4742=LINE('',#41262,#5766);
#4743=LINE('',#41263,#5767);
#4744=LINE('',#41475,#5768);
#4745=LINE('',#41479,#5769);
#4746=LINE('',#41691,#5770);
#4747=LINE('',#41694,#5771);
#4748=LINE('',#41695,#5772);
#4749=LINE('',#41907,#5773);
#4750=LINE('',#41911,#5774);
#4751=LINE('',#42123,#5775);
#4752=LINE('',#42126,#5776);
#4753=LINE('',#42127,#5777);
#4754=LINE('',#42339,#5778);
#4755=LINE('',#42343,#5779);
#4756=LINE('',#42555,#5780);
#4757=LINE('',#42558,#5781);
#4758=LINE('',#42559,#5782);
#4759=LINE('',#42771,#5783);
#4760=LINE('',#42775,#5784);
#4761=LINE('',#42987,#5785);
#4762=LINE('',#42990,#5786);
#4763=LINE('',#42991,#5787);
#4764=LINE('',#43203,#5788);
#4765=LINE('',#43207,#5789);
#4766=LINE('',#43419,#5790);
#4767=LINE('',#43422,#5791);
#4768=LINE('',#43423,#5792);
#4769=LINE('',#43635,#5793);
#4770=LINE('',#43639,#5794);
#4771=LINE('',#43851,#5795);
#4772=LINE('',#43854,#5796);
#4773=LINE('',#43855,#5797);
#4774=LINE('',#44067,#5798);
#4775=LINE('',#44071,#5799);
#4776=LINE('',#44283,#5800);
#4777=LINE('',#44286,#5801);
#4778=LINE('',#44287,#5802);
#4779=LINE('',#44499,#5803);
#4780=LINE('',#44503,#5804);
#4781=LINE('',#44715,#5805);
#4782=LINE('',#44718,#5806);
#4783=LINE('',#44719,#5807);
#4784=LINE('',#44931,#5808);
#4785=LINE('',#44935,#5809);
#4786=LINE('',#45147,#5810);
#4787=LINE('',#45150,#5811);
#4788=LINE('',#45151,#5812);
#4789=LINE('',#45363,#5813);
#4790=LINE('',#45367,#5814);
#4791=LINE('',#45579,#5815);
#4792=LINE('',#45582,#5816);
#4793=LINE('',#45583,#5817);
#4794=LINE('',#45795,#5818);
#4795=LINE('',#45799,#5819);
#4796=LINE('',#46011,#5820);
#4797=LINE('',#46014,#5821);
#4798=LINE('',#46015,#5822);
#4799=LINE('',#46227,#5823);
#4800=LINE('',#46231,#5824);
#4801=LINE('',#46443,#5825);
#4802=LINE('',#46446,#5826);
#4803=LINE('',#46447,#5827);
#4804=LINE('',#46659,#5828);
#4805=LINE('',#46663,#5829);
#4806=LINE('',#46875,#5830);
#4807=LINE('',#46878,#5831);
#4808=LINE('',#46879,#5832);
#4809=LINE('',#47091,#5833);
#4810=LINE('',#47095,#5834);
#4811=LINE('',#47307,#5835);
#4812=LINE('',#47310,#5836);
#4813=LINE('',#47311,#5837);
#4814=LINE('',#47523,#5838);
#4815=LINE('',#47527,#5839);
#4816=LINE('',#47739,#5840);
#4817=LINE('',#47742,#5841);
#4818=LINE('',#47743,#5842);
#4819=LINE('',#47955,#5843);
#4820=LINE('',#47959,#5844);
#4821=LINE('',#48171,#5845);
#4822=LINE('',#48174,#5846);
#4823=LINE('',#48175,#5847);
#4824=LINE('',#48387,#5848);
#4825=LINE('',#48391,#5849);
#4826=LINE('',#48603,#5850);
#4827=LINE('',#48606,#5851);
#4828=LINE('',#48607,#5852);
#4829=LINE('',#48819,#5853);
#4830=LINE('',#48823,#5854);
#4831=LINE('',#49035,#5855);
#4832=LINE('',#49038,#5856);
#4833=LINE('',#49039,#5857);
#4834=LINE('',#49251,#5858);
#4835=LINE('',#49260,#5859);
#4836=LINE('',#49262,#5860);
#4837=LINE('',#49264,#5861);
#4838=LINE('',#49265,#5862);
#4839=LINE('',#49270,#5863);
#4840=LINE('',#49271,#5864);
#4841=LINE('',#49274,#5865);
#4842=LINE('',#49276,#5866);
#4843=LINE('',#49277,#5867);
#4844=LINE('',#49279,#5868);
#4845=LINE('',#49286,#5869);
#4846=LINE('',#49294,#5870);
#4847=LINE('',#49315,#5871);
#4848=LINE('',#49370,#5872);
#4849=LINE('',#49375,#5873);
#4850=LINE('',#49381,#5874);
#4851=LINE('',#49389,#5875);
#4852=LINE('',#49410,#5876);
#4853=LINE('',#49465,#5877);
#4854=LINE('',#49470,#5878);
#4855=LINE('',#49476,#5879);
#4856=LINE('',#49485,#5880);
#4857=LINE('',#49491,#5881);
#4858=LINE('',#49500,#5882);
#4859=LINE('',#49506,#5883);
#4860=LINE('',#49515,#5884);
#4861=LINE('',#49521,#5885);
#4862=LINE('',#49530,#5886);
#4863=LINE('',#49536,#5887);
#4864=LINE('',#49544,#5888);
#4865=LINE('',#49546,#5889);
#4866=LINE('',#49548,#5890);
#4867=LINE('',#49549,#5891);
#4868=LINE('',#49552,#5892);
#4869=LINE('',#49554,#5893);
#4870=LINE('',#49555,#5894);
#4871=LINE('',#49558,#5895);
#4872=LINE('',#49560,#5896);
#4873=LINE('',#49561,#5897);
#4874=LINE('',#49564,#5898);
#4875=LINE('',#49566,#5899);
#4876=LINE('',#49567,#5900);
#4877=LINE('',#49570,#5901);
#4878=LINE('',#49572,#5902);
#4879=LINE('',#49573,#5903);
#4880=LINE('',#49575,#5904);
#4881=LINE('',#49576,#5905);
#4882=LINE('',#49584,#5906);
#4883=LINE('',#49588,#5907);
#4884=LINE('',#49592,#5908);
#4885=LINE('',#49609,#5909);
#4886=LINE('',#49611,#5910);
#4887=LINE('',#49613,#5911);
#4888=LINE('',#49614,#5912);
#4889=LINE('',#49617,#5913);
#4890=LINE('',#49619,#5914);
#4891=LINE('',#49620,#5915);
#4892=LINE('',#49623,#5916);
#4893=LINE('',#49625,#5917);
#4894=LINE('',#49626,#5918);
#4895=LINE('',#49703,#5919);
#4896=LINE('',#49849,#5920);
#4897=LINE('',#49995,#5921);
#4898=LINE('',#50141,#5922);
#4899=LINE('',#50287,#5923);
#4900=LINE('',#50433,#5924);
#4901=LINE('',#50579,#5925);
#4902=LINE('',#50725,#5926);
#4903=LINE('',#50871,#5927);
#4904=LINE('',#51017,#5928);
#4905=LINE('',#51163,#5929);
#4906=LINE('',#51309,#5930);
#4907=LINE('',#51455,#5931);
#4908=LINE('',#51601,#5932);
#4909=LINE('',#51747,#5933);
#4910=LINE('',#51893,#5934);
#4911=LINE('',#52039,#5935);
#4912=LINE('',#52185,#5936);
#4913=LINE('',#52331,#5937);
#4914=LINE('',#52477,#5938);
#4915=LINE('',#52623,#5939);
#4916=LINE('',#52769,#5940);
#4917=LINE('',#52915,#5941);
#4918=LINE('',#53061,#5942);
#4919=LINE('',#53207,#5943);
#4920=LINE('',#53353,#5944);
#4921=LINE('',#53499,#5945);
#4922=LINE('',#53645,#5946);
#4923=LINE('',#53791,#5947);
#4924=LINE('',#53937,#5948);
#4925=LINE('',#54083,#5949);
#4926=LINE('',#54229,#5950);
#4927=LINE('',#54375,#5951);
#4928=LINE('',#54521,#5952);
#4929=LINE('',#54667,#5953);
#4930=LINE('',#54813,#5954);
#4931=LINE('',#54959,#5955);
#4932=LINE('',#55105,#5956);
#4933=LINE('',#55251,#5957);
#4934=LINE('',#55397,#5958);
#4935=LINE('',#55475,#5959);
#4936=LINE('',#55696,#5960);
#4937=LINE('',#55845,#5961);
#4938=LINE('',#55917,#5962);
#4939=LINE('',#56138,#5963);
#4940=LINE('',#56287,#5964);
#4941=LINE('',#56359,#5965);
#4942=LINE('',#56580,#5966);
#4943=LINE('',#56729,#5967);
#4944=LINE('',#56801,#5968);
#4945=LINE('',#57022,#5969);
#4946=LINE('',#57171,#5970);
#4947=LINE('',#57243,#5971);
#4948=LINE('',#57464,#5972);
#4949=LINE('',#57613,#5973);
#4950=LINE('',#57685,#5974);
#4951=LINE('',#57906,#5975);
#4952=LINE('',#58055,#5976);
#4953=LINE('',#58127,#5977);
#4954=LINE('',#58348,#5978);
#4955=LINE('',#58497,#5979);
#4956=LINE('',#58569,#5980);
#4957=LINE('',#58790,#5981);
#4958=LINE('',#58939,#5982);
#4959=LINE('',#59011,#5983);
#4960=LINE('',#59232,#5984);
#4961=LINE('',#59381,#5985);
#4962=LINE('',#59453,#5986);
#4963=LINE('',#59674,#5987);
#4964=LINE('',#59823,#5988);
#4965=LINE('',#59895,#5989);
#4966=LINE('',#60116,#5990);
#4967=LINE('',#60265,#5991);
#4968=LINE('',#60337,#5992);
#4969=LINE('',#60558,#5993);
#4970=LINE('',#60707,#5994);
#4971=LINE('',#60779,#5995);
#4972=LINE('',#61000,#5996);
#4973=LINE('',#61149,#5997);
#4974=LINE('',#61221,#5998);
#4975=LINE('',#61442,#5999);
#4976=LINE('',#61591,#6000);
#4977=LINE('',#61663,#6001);
#4978=LINE('',#61884,#6002);
#4979=LINE('',#62033,#6003);
#4980=LINE('',#62105,#6004);
#4981=LINE('',#62326,#6005);
#4982=LINE('',#62475,#6006);
#4983=LINE('',#62547,#6007);
#4984=LINE('',#62768,#6008);
#4985=LINE('',#62917,#6009);
#4986=LINE('',#62989,#6010);
#4987=LINE('',#63210,#6011);
#4988=LINE('',#63359,#6012);
#4989=LINE('',#63431,#6013);
#4990=LINE('',#63652,#6014);
#4991=LINE('',#63801,#6015);
#4992=LINE('',#63873,#6016);
#4993=LINE('',#64094,#6017);
#4994=LINE('',#64243,#6018);
#4995=LINE('',#64315,#6019);
#4996=LINE('',#64536,#6020);
#4997=LINE('',#64685,#6021);
#4998=LINE('',#64757,#6022);
#4999=LINE('',#64978,#6023);
#5000=LINE('',#65127,#6024);
#5001=LINE('',#65199,#6025);
#5002=LINE('',#65420,#6026);
#5003=LINE('',#65569,#6027);
#5004=LINE('',#65641,#6028);
#5005=LINE('',#65862,#6029);
#5006=LINE('',#66011,#6030);
#5007=LINE('',#66083,#6031);
#5008=LINE('',#66304,#6032);
#5009=LINE('',#66453,#6033);
#5010=LINE('',#66525,#6034);
#5011=LINE('',#66746,#6035);
#5012=LINE('',#66895,#6036);
#5013=LINE('',#66967,#6037);
#5014=LINE('',#67188,#6038);
#5015=LINE('',#67337,#6039);
#5016=LINE('',#67409,#6040);
#5017=LINE('',#67630,#6041);
#5018=LINE('',#67779,#6042);
#5019=LINE('',#67851,#6043);
#5020=LINE('',#68072,#6044);
#5021=LINE('',#68221,#6045);
#5022=LINE('',#68293,#6046);
#5023=LINE('',#68514,#6047);
#5024=LINE('',#68663,#6048);
#5025=LINE('',#68735,#6049);
#5026=LINE('',#68956,#6050);
#5027=LINE('',#69105,#6051);
#5028=LINE('',#69177,#6052);
#5029=LINE('',#69398,#6053);
#5030=LINE('',#69547,#6054);
#5031=LINE('',#69619,#6055);
#5032=LINE('',#69840,#6056);
#5033=LINE('',#69989,#6057);
#5034=LINE('',#70061,#6058);
#5035=LINE('',#70282,#6059);
#5036=LINE('',#70431,#6060);
#5037=LINE('',#70503,#6061);
#5038=LINE('',#70724,#6062);
#5039=LINE('',#70873,#6063);
#5040=LINE('',#70945,#6064);
#5041=LINE('',#71166,#6065);
#5042=LINE('',#71315,#6066);
#5043=LINE('',#71387,#6067);
#5044=LINE('',#71608,#6068);
#5045=LINE('',#71757,#6069);
#5046=LINE('',#71829,#6070);
#5047=LINE('',#72050,#6071);
#5048=LINE('',#72199,#6072);
#5049=LINE('',#72271,#6073);
#5050=LINE('',#72492,#6074);
#5051=LINE('',#72495,#6075);
#5052=LINE('',#72496,#6076);
#5053=LINE('',#72871,#6077);
#5054=LINE('',#73153,#6078);
#5055=LINE('',#73155,#6079);
#5056=LINE('',#73163,#6080);
#5057=LINE('',#73165,#6081);
#5058=LINE('',#73167,#6082);
#5059=LINE('',#73169,#6083);
#5060=LINE('',#73171,#6084);
#5061=LINE('',#73173,#6085);
#5062=LINE('',#73175,#6086);
#5063=LINE('',#73176,#6087);
#5064=LINE('',#73179,#6088);
#5065=LINE('',#73181,#6089);
#5066=LINE('',#73182,#6090);
#5067=LINE('',#73185,#6091);
#5068=LINE('',#73186,#6092);
#5069=LINE('',#73189,#6093);
#5070=LINE('',#73190,#6094);
#5071=LINE('',#73193,#6095);
#5072=LINE('',#73194,#6096);
#5073=LINE('',#73198,#6097);
#5074=LINE('',#73199,#6098);
#5075=LINE('',#73201,#6099);
#5076=LINE('',#73202,#6100);
#5077=LINE('',#73204,#6101);
#5078=LINE('',#73206,#6102);
#5079=LINE('',#73208,#6103);
#5080=VECTOR('',#18468,0.25);
#5081=VECTOR('',#18475,0.25);
#5082=VECTOR('',#18482,0.25);
#5083=VECTOR('',#18489,0.25);
#5084=VECTOR('',#18494,1.);
#5085=VECTOR('',#18495,1.);
#5086=VECTOR('',#18496,1.);
#5087=VECTOR('',#18497,1.);
#5088=VECTOR('',#18500,1.);
#5089=VECTOR('',#18501,1.);
#5090=VECTOR('',#18502,1.);
#5091=VECTOR('',#18505,1.);
#5092=VECTOR('',#18506,1.);
#5093=VECTOR('',#18507,1.);
#5094=VECTOR('',#18510,1.);
#5095=VECTOR('',#18511,1.);
#5096=VECTOR('',#18522,0.164999999999999);
#5097=VECTOR('',#18531,0.164999999999999);
#5098=VECTOR('',#18540,0.164999999999999);
#5099=VECTOR('',#18549,0.164999999999999);
#5100=VECTOR('',#18556,1.);
#5101=VECTOR('',#18559,1.);
#5102=VECTOR('',#18564,1.);
#5103=VECTOR('',#18567,1.);
#5104=VECTOR('',#18570,1.);
#5105=VECTOR('',#18571,1.);
#5106=VECTOR('',#18572,1.);
#5107=VECTOR('',#18573,1.);
#5108=VECTOR('',#18574,1.);
#5109=VECTOR('',#18575,1.);
#5110=VECTOR('',#18576,1.);
#5111=VECTOR('',#18577,1.);
#5112=VECTOR('',#18578,1.);
#5113=VECTOR('',#18581,1.);
#5114=VECTOR('',#18584,1.);
#5115=VECTOR('',#18595,1.);
#5116=VECTOR('',#18596,1.);
#5117=VECTOR('',#18597,1.);
#5118=VECTOR('',#18598,1.);
#5119=VECTOR('',#18599,1.);
#5120=VECTOR('',#18600,1.);
#5121=VECTOR('',#18601,1.);
#5122=VECTOR('',#18602,1.);
#5123=VECTOR('',#18603,1.);
#5124=VECTOR('',#18618,1.);
#5125=VECTOR('',#18625,1.);
#5126=VECTOR('',#18628,1.);
#5127=VECTOR('',#18631,1.);
#5128=VECTOR('',#18634,1.);
#5129=VECTOR('',#18635,1.);
#5130=VECTOR('',#18636,1.);
#5131=VECTOR('',#18637,1.);
#5132=VECTOR('',#18638,1.);
#5133=VECTOR('',#18639,1.);
#5134=VECTOR('',#18640,1.);
#5135=VECTOR('',#18641,1.);
#5136=VECTOR('',#18652,1.);
#5137=VECTOR('',#18653,1.);
#5138=VECTOR('',#18654,1.);
#5139=VECTOR('',#18655,1.);
#5140=VECTOR('',#18656,1.);
#5141=VECTOR('',#18663,1.);
#5142=VECTOR('',#18668,1.);
#5143=VECTOR('',#18671,1.);
#5144=VECTOR('',#18674,1.);
#5145=VECTOR('',#18675,1.);
#5146=VECTOR('',#18676,1.);
#5147=VECTOR('',#18677,1.);
#5148=VECTOR('',#18680,1.);
#5149=VECTOR('',#18681,1.);
#5150=VECTOR('',#18682,1.);
#5151=VECTOR('',#18687,0.165);
#5152=VECTOR('',#18694,0.165);
#5153=VECTOR('',#18699,0.165);
#5154=VECTOR('',#18706,0.165);
#5155=VECTOR('',#18713,1.);
#5156=VECTOR('',#18718,1.);
#5157=VECTOR('',#18725,1.);
#5158=VECTOR('',#18730,1.);
#5159=VECTOR('',#18733,1.);
#5160=VECTOR('',#18734,1.);
#5161=VECTOR('',#18735,1.);
#5162=VECTOR('',#18736,1.);
#5163=VECTOR('',#18737,1.);
#5164=VECTOR('',#18740,1.);
#5165=VECTOR('',#18747,1.);
#5166=VECTOR('',#18748,1.);
#5167=VECTOR('',#18749,1.);
#5168=VECTOR('',#18750,1.);
#5169=VECTOR('',#18755,1.);
#5170=VECTOR('',#18756,1.);
#5171=VECTOR('',#18757,1.);
#5172=VECTOR('',#18762,0.165);
#5173=VECTOR('',#18769,0.165);
#5174=VECTOR('',#18774,0.165);
#5175=VECTOR('',#18781,0.165);
#5176=VECTOR('',#18788,1.);
#5177=VECTOR('',#18793,1.);
#5178=VECTOR('',#18798,1.);
#5179=VECTOR('',#18799,1.);
#5180=VECTOR('',#18800,1.);
#5181=VECTOR('',#18801,1.);
#5182=VECTOR('',#18802,1.);
#5183=VECTOR('',#18803,1.);
#5184=VECTOR('',#18830,0.6);
#5185=VECTOR('',#18841,0.6);
#5186=VECTOR('',#18852,0.6);
#5187=VECTOR('',#18863,0.6);
#5188=VECTOR('',#18874,0.33);
#5189=VECTOR('',#18879,0.33);
#5190=VECTOR('',#18884,0.33);
#5191=VECTOR('',#18889,0.33);
#5192=VECTOR('',#18894,0.149999999999999);
#5193=VECTOR('',#18901,0.149999999999999);
#5194=VECTOR('',#18908,0.15);
#5195=VECTOR('',#18915,0.15);
#5196=VECTOR('',#18922,0.25);
#5197=VECTOR('',#18927,0.25);
#5198=VECTOR('',#18932,0.25);
#5199=VECTOR('',#18937,0.25);
#5200=VECTOR('',#18942,0.25);
#5201=VECTOR('',#18947,0.25);
#5202=VECTOR('',#18950,1.);
#5203=VECTOR('',#18953,1.);
#5204=VECTOR('',#18956,1.);
#5205=VECTOR('',#18959,1.);
#5206=VECTOR('',#18962,1.);
#5207=VECTOR('',#18965,1.);
#5208=VECTOR('',#18968,1.);
#5209=VECTOR('',#18973,1.);
#5210=VECTOR('',#18982,0.164999999999999);
#5211=VECTOR('',#18989,0.165);
#5212=VECTOR('',#18996,0.165);
#5213=VECTOR('',#19003,0.164999999999999);
#5214=VECTOR('',#19008,1.);
#5215=VECTOR('',#19009,1.);
#5216=VECTOR('',#19010,1.);
#5217=VECTOR('',#19011,1.);
#5218=VECTOR('',#19014,1.);
#5219=VECTOR('',#19015,1.);
#5220=VECTOR('',#19016,1.);
#5221=VECTOR('',#19019,1.);
#5222=VECTOR('',#19020,1.);
#5223=VECTOR('',#19021,1.);
#5224=VECTOR('',#19024,1.);
#5225=VECTOR('',#19025,1.);
#5226=VECTOR('',#19030,0.164999999999999);
#5227=VECTOR('',#19039,0.164999999999999);
#5228=VECTOR('',#19048,0.164999999999999);
#5229=VECTOR('',#19057,0.164999999999999);
#5230=VECTOR('',#19064,1.);
#5231=VECTOR('',#19067,1.);
#5232=VECTOR('',#19072,1.);
#5233=VECTOR('',#19075,1.);
#5234=VECTOR('',#19078,1.);
#5235=VECTOR('',#19081,1.);
#5236=VECTOR('',#19084,1.);
#5237=VECTOR('',#19085,1.);
#5238=VECTOR('',#19086,1.);
#5239=VECTOR('',#19087,1.);
#5240=VECTOR('',#19088,1.);
#5241=VECTOR('',#19089,1.);
#5242=VECTOR('',#19090,1.);
#5243=VECTOR('',#19091,1.);
#5244=VECTOR('',#19092,1.);
#5245=VECTOR('',#19105,1.);
#5246=VECTOR('',#19112,1.);
#5247=VECTOR('',#19117,1.);
#5248=VECTOR('',#19118,1.);
#5249=VECTOR('',#19119,1.);
#5250=VECTOR('',#19120,1.);
#5251=VECTOR('',#19121,1.);
#5252=VECTOR('',#19122,1.);
#5253=VECTOR('',#19123,1.);
#5254=VECTOR('',#19124,1.);
#5255=VECTOR('',#19127,1.);
#5256=VECTOR('',#19130,1.);
#5257=VECTOR('',#19141,1.);
#5258=VECTOR('',#19146,1.);
#5259=VECTOR('',#19149,1.);
#5260=VECTOR('',#19152,1.);
#5261=VECTOR('',#19153,1.);
#5262=VECTOR('',#19154,1.);
#5263=VECTOR('',#19155,1.);
#5264=VECTOR('',#19156,1.);
#5265=VECTOR('',#19157,1.);
#5266=VECTOR('',#19158,1.);
#5267=VECTOR('',#19159,1.);
#5268=VECTOR('',#19170,1.);
#5269=VECTOR('',#19173,1.);
#5270=VECTOR('',#19176,1.);
#5271=VECTOR('',#19177,1.);
#5272=VECTOR('',#19178,1.);
#5273=VECTOR('',#19179,1.);
#5274=VECTOR('',#19182,1.);
#5275=VECTOR('',#19183,1.);
#5276=VECTOR('',#19184,1.);
#5277=VECTOR('',#19187,1.);
#5278=VECTOR('',#19188,1.);
#5279=VECTOR('',#19189,1.);
#5280=VECTOR('',#19190,1.);
#5281=VECTOR('',#19195,0.165);
#5282=VECTOR('',#19202,0.165);
#5283=VECTOR('',#19207,0.165);
#5284=VECTOR('',#19214,0.165);
#5285=VECTOR('',#19221,1.);
#5286=VECTOR('',#19228,1.);
#5287=VECTOR('',#19233,1.);
#5288=VECTOR('',#19236,1.);
#5289=VECTOR('',#19241,1.);
#5290=VECTOR('',#19246,1.);
#5291=VECTOR('',#19249,1.);
#5292=VECTOR('',#19250,1.);
#5293=VECTOR('',#19251,1.);
#5294=VECTOR('',#19254,1.);
#5295=VECTOR('',#19255,1.);
#5296=VECTOR('',#19256,1.);
#5297=VECTOR('',#19257,1.);
#5298=VECTOR('',#19262,0.165);
#5299=VECTOR('',#19269,0.165);
#5300=VECTOR('',#19274,0.165);
#5301=VECTOR('',#19281,0.165);
#5302=VECTOR('',#19290,1.);
#5303=VECTOR('',#19295,1.);
#5304=VECTOR('',#19298,1.);
#5305=VECTOR('',#19303,1.);
#5306=VECTOR('',#19308,1.);
#5307=VECTOR('',#19313,1.);
#5308=VECTOR('',#19316,1.);
#5309=VECTOR('',#19317,1.);
#5310=VECTOR('',#19318,1.);
#5311=VECTOR('',#19319,1.);
#5312=VECTOR('',#19322,1.);
#5313=VECTOR('',#19323,1.);
#5314=VECTOR('',#19336,0.149999999999999);
#5315=VECTOR('',#19343,0.149999999999999);
#5316=VECTOR('',#19350,0.15);
#5317=VECTOR('',#19357,0.15);
#5318=VECTOR('',#19364,0.329999999999998);
#5319=VECTOR('',#19369,0.33);
#5320=VECTOR('',#19374,0.33);
#5321=VECTOR('',#19379,0.33);
#5322=VECTOR('',#19384,0.329999999999998);
#5323=VECTOR('',#19389,0.329999999999998);
#5324=VECTOR('',#19394,1.);
#5325=VECTOR('',#19397,1.);
#5326=VECTOR('',#19400,1.);
#5327=VECTOR('',#19403,1.);
#5328=VECTOR('',#19406,1.);
#5329=VECTOR('',#19409,1.);
#5330=VECTOR('',#19412,1.);
#5331=VECTOR('',#19417,1.);
#5332=VECTOR('',#19426,0.15);
#5333=VECTOR('',#19439,0.15);
#5334=VECTOR('',#19452,0.149999999999999);
#5335=VECTOR('',#19465,0.149999999999999);
#5336=VECTOR('',#19476,1.);
#5337=VECTOR('',#19479,1.);
#5338=VECTOR('',#19484,1.);
#5339=VECTOR('',#19487,1.);
#5340=VECTOR('',#19492,1.);
#5341=VECTOR('',#19495,1.);
#5342=VECTOR('',#19500,1.);
#5343=VECTOR('',#19503,1.);
#5344=VECTOR('',#19538,1.59);
#5345=VECTOR('',#19547,1.2);
#5346=VECTOR('',#19554,1.);
#5347=VECTOR('',#19557,1.);
#5348=VECTOR('',#19562,1.);
#5349=VECTOR('',#19565,1.);
#5350=VECTOR('',#19570,1.);
#5351=VECTOR('',#19573,1.);
#5352=VECTOR('',#19578,1.);
#5353=VECTOR('',#19581,1.);
#5354=VECTOR('',#19614,1.59);
#5355=VECTOR('',#19625,1.2);
#5356=VECTOR('',#19634,0.225);
#5357=VECTOR('',#19641,0.225);
#5358=VECTOR('',#19648,0.225000000000001);
#5359=VECTOR('',#19655,0.225000000000001);
#5360=VECTOR('',#19662,2.34);
#5361=VECTOR('',#19671,1.9);
#5362=VECTOR('',#19678,2.9);
#5363=VECTOR('',#19691,0.225);
#5364=VECTOR('',#19698,0.225);
#5365=VECTOR('',#19705,0.225000000000001);
#5366=VECTOR('',#19712,0.225000000000001);
#5367=VECTOR('',#19719,2.34);
#5368=VECTOR('',#19730,1.9);
#5369=VECTOR('',#19735,2.9);
#5370=VECTOR('',#19748,0.225);
#5371=VECTOR('',#19755,0.225);
#5372=VECTOR('',#19762,0.225);
#5373=VECTOR('',#19769,0.225);
#5374=VECTOR('',#19776,2.34);
#5375=VECTOR('',#19785,1.9);
#5376=VECTOR('',#19792,2.9);
#5377=VECTOR('',#19805,0.225);
#5378=VECTOR('',#19812,0.225);
#5379=VECTOR('',#19819,0.225);
#5380=VECTOR('',#19826,0.225);
#5381=VECTOR('',#19833,2.34);
#5382=VECTOR('',#19844,1.9);
#5383=VECTOR('',#19849,2.9);
#5384=VECTOR('',#19862,0.225);
#5385=VECTOR('',#19869,0.225);
#5386=VECTOR('',#19876,0.225);
#5387=VECTOR('',#19883,0.225);
#5388=VECTOR('',#19888,1.);
#5389=VECTOR('',#19889,1.);
#5390=VECTOR('',#19890,1.);
#5391=VECTOR('',#19891,1.);
#5392=VECTOR('',#19894,1.);
#5393=VECTOR('',#19895,1.);
#5394=VECTOR('',#19896,1.);
#5395=VECTOR('',#19899,1.);
#5396=VECTOR('',#19900,1.);
#5397=VECTOR('',#19901,1.);
#5398=VECTOR('',#19904,1.);
#5399=VECTOR('',#19905,1.);
#5400=VECTOR('',#19914,1.);
#5401=VECTOR('',#19915,1.);
#5402=VECTOR('',#19916,1.);
#5403=VECTOR('',#19917,1.);
#5404=VECTOR('',#19920,1.);
#5405=VECTOR('',#19921,1.);
#5406=VECTOR('',#19922,1.);
#5407=VECTOR('',#19925,1.);
#5408=VECTOR('',#19926,1.);
#5409=VECTOR('',#19927,1.);
#5410=VECTOR('',#19930,1.);
#5411=VECTOR('',#19931,1.);
#5412=VECTOR('',#19940,1.);
#5413=VECTOR('',#19941,1.);
#5414=VECTOR('',#19942,1.);
#5415=VECTOR('',#19943,1.);
#5416=VECTOR('',#19946,1.);
#5417=VECTOR('',#19947,1.);
#5418=VECTOR('',#19948,1.);
#5419=VECTOR('',#19951,1.);
#5420=VECTOR('',#19952,1.);
#5421=VECTOR('',#19953,1.);
#5422=VECTOR('',#19956,1.);
#5423=VECTOR('',#19957,1.);
#5424=VECTOR('',#19966,1.);
#5425=VECTOR('',#19967,1.);
#5426=VECTOR('',#19968,1.);
#5427=VECTOR('',#19969,1.);
#5428=VECTOR('',#19972,1.);
#5429=VECTOR('',#19973,1.);
#5430=VECTOR('',#19974,1.);
#5431=VECTOR('',#19977,1.);
#5432=VECTOR('',#19978,1.);
#5433=VECTOR('',#19979,1.);
#5434=VECTOR('',#19982,1.);
#5435=VECTOR('',#19983,1.);
#5436=VECTOR('',#19984,1.);
#5437=VECTOR('',#19987,1.);
#5438=VECTOR('',#19988,1.);
#5439=VECTOR('',#19989,1.);
#5440=VECTOR('',#19992,1.);
#5441=VECTOR('',#19993,1.);
#5442=VECTOR('',#20010,0.475);
#5443=VECTOR('',#20015,0.5);
#5444=VECTOR('',#20020,0.485);
#5445=VECTOR('',#20029,0.31);
#5446=VECTOR('',#20032,0.3);
#5447=VECTOR('',#20051,1.070235);
#5448=VECTOR('',#20058,0.6);
#5449=VECTOR('',#20063,0.63);
#5450=VECTOR('',#20072,1.070235);
#5451=VECTOR('',#20079,0.63);
#5452=VECTOR('',#20098,1.129765);
#5453=VECTOR('',#20109,1.57);
#5454=VECTOR('',#20114,1.6);
#5455=VECTOR('',#20119,1.57);
#5456=VECTOR('',#20124,1.129765);
#5457=VECTOR('',#20171,1.123812);
#5458=VECTOR('',#20240,1.076188);
#5459=VECTOR('',#20269,1.119765);
#5460=VECTOR('',#20276,1.085235);
#5461=VECTOR('',#20287,1.119765);
#5462=VECTOR('',#20294,1.085235);
#5463=VECTOR('',#20323,1.63531);
#5464=VECTOR('',#20330,1.);
#5465=VECTOR('',#20335,1.05);
#5466=VECTOR('',#20344,1.63531);
#5467=VECTOR('',#20351,1.05);
#5468=VECTOR('',#20370,1.71469);
#5469=VECTOR('',#20381,2.3);
#5470=VECTOR('',#20386,2.35);
#5471=VECTOR('',#20391,2.3);
#5472=VECTOR('',#20396,1.71469);
#5473=VECTOR('',#20447,1.706752);
#5474=VECTOR('',#20524,1.643248);
#5475=VECTOR('',#20553,1.70469);
#5476=VECTOR('',#20560,1.65031);
#5477=VECTOR('',#20571,1.70469);
#5478=VECTOR('',#20578,1.65031);
#5479=VECTOR('',#20599,0.325);
#5480=VECTOR('',#20604,0.35);
#5481=VECTOR('',#20609,0.335);
#5482=VECTOR('',#20618,0.21);
#5483=VECTOR('',#20623,0.2);
#5484=VECTOR('',#20628,0.18);
#5485=VECTOR('',#20633,1.);
#5486=VECTOR('',#20634,1.);
#5487=VECTOR('',#20635,1.);
#5488=VECTOR('',#20636,1.);
#5489=VECTOR('',#20639,1.);
#5490=VECTOR('',#20640,1.);
#5491=VECTOR('',#20641,1.);
#5492=VECTOR('',#20644,1.);
#5493=VECTOR('',#20645,1.);
#5494=VECTOR('',#20646,1.);
#5495=VECTOR('',#20649,1.);
#5496=VECTOR('',#20650,1.);
#5497=VECTOR('',#20651,1.);
#5498=VECTOR('',#20654,1.);
#5499=VECTOR('',#20655,1.);
#5500=VECTOR('',#20656,1.);
#5501=VECTOR('',#20659,1.);
#5502=VECTOR('',#20660,1.);
#5503=VECTOR('',#20791,1.);
#5504=VECTOR('',#20792,1.);
#5505=VECTOR('',#20793,1.);
#5506=VECTOR('',#20794,1.);
#5507=VECTOR('',#20799,1.);
#5508=VECTOR('',#20800,1.);
#5509=VECTOR('',#20803,1.);
#5510=VECTOR('',#20804,1.);
#5511=VECTOR('',#20805,1.);
#5512=VECTOR('',#20808,1.);
#5513=VECTOR('',#20817,0.6);
#5514=VECTOR('',#20828,1.);
#5515=VECTOR('',#20835,0.21);
#5516=VECTOR('',#20840,1.);
#5517=VECTOR('',#20845,0.605);
#5518=VECTOR('',#20852,1.);
#5519=VECTOR('',#20863,1.);
#5520=VECTOR('',#20870,0.21);
#5521=VECTOR('',#20875,1.);
#5522=VECTOR('',#20880,0.605);
#5523=VECTOR('',#20887,1.);
#5524=VECTOR('',#20900,0.605);
#5525=VECTOR('',#20907,0.9);
#5526=VECTOR('',#20920,0.605);
#5527=VECTOR('',#20927,0.9);
#5528=VECTOR('',#20940,0.605);
#5529=VECTOR('',#20947,0.9);
#5530=VECTOR('',#20960,0.605);
#5531=VECTOR('',#20967,0.9);
#5532=VECTOR('',#20978,1.);
#5533=VECTOR('',#20979,1.);
#5534=VECTOR('',#20980,1.);
#5535=VECTOR('',#20981,1.);
#5536=VECTOR('',#20984,1.);
#5537=VECTOR('',#20985,1.);
#5538=VECTOR('',#20986,1.);
#5539=VECTOR('',#20989,1.);
#5540=VECTOR('',#20990,1.);
#5541=VECTOR('',#20991,1.);
#5542=VECTOR('',#20996,1.);
#5543=VECTOR('',#20999,1.);
#5544=VECTOR('',#21002,1.);
#5545=VECTOR('',#21005,1.);
#5546=VECTOR('',#21008,1.);
#5547=VECTOR('',#21011,1.);
#5548=VECTOR('',#21014,1.);
#5549=VECTOR('',#21017,1.);
#5550=VECTOR('',#21020,1.);
#5551=VECTOR('',#21023,1.);
#5552=VECTOR('',#21026,1.);
#5553=VECTOR('',#21029,1.);
#5554=VECTOR('',#21032,1.);
#5555=VECTOR('',#21035,1.);
#5556=VECTOR('',#21038,1.);
#5557=VECTOR('',#21041,1.);
#5558=VECTOR('',#21044,1.);
#5559=VECTOR('',#21047,1.);
#5560=VECTOR('',#21050,1.);
#5561=VECTOR('',#21053,1.);
#5562=VECTOR('',#21064,1.4);
#5563=VECTOR('',#21069,1.);
#5564=VECTOR('',#21070,1.);
#5565=VECTOR('',#21073,1.);
#5566=VECTOR('',#21074,1.);
#5567=VECTOR('',#21075,1.);
#5568=VECTOR('',#21080,1.);
#5569=VECTOR('',#21081,1.);
#5570=VECTOR('',#21084,1.);
#5571=VECTOR('',#21085,1.);
#5572=VECTOR('',#21086,1.);
#5573=VECTOR('',#21091,1.);
#5574=VECTOR('',#21092,1.);
#5575=VECTOR('',#21095,1.);
#5576=VECTOR('',#21096,1.);
#5577=VECTOR('',#21097,1.);
#5578=VECTOR('',#21102,1.);
#5579=VECTOR('',#21103,1.);
#5580=VECTOR('',#21106,1.);
#5581=VECTOR('',#21107,1.);
#5582=VECTOR('',#21108,1.);
#5583=VECTOR('',#21113,1.);
#5584=VECTOR('',#21114,1.);
#5585=VECTOR('',#21117,1.);
#5586=VECTOR('',#21118,1.);
#5587=VECTOR('',#21119,1.);
#5588=VECTOR('',#21124,1.);
#5589=VECTOR('',#21125,1.);
#5590=VECTOR('',#21128,1.);
#5591=VECTOR('',#21129,1.);
#5592=VECTOR('',#21130,1.);
#5593=VECTOR('',#21135,1.);
#5594=VECTOR('',#21136,1.);
#5595=VECTOR('',#21139,1.);
#5596=VECTOR('',#21140,1.);
#5597=VECTOR('',#21141,1.);
#5598=VECTOR('',#21146,1.);
#5599=VECTOR('',#21147,1.);
#5600=VECTOR('',#21150,1.);
#5601=VECTOR('',#21151,1.);
#5602=VECTOR('',#21152,1.);
#5603=VECTOR('',#21157,1.);
#5604=VECTOR('',#21158,1.);
#5605=VECTOR('',#21161,1.);
#5606=VECTOR('',#21162,1.);
#5607=VECTOR('',#21163,1.);
#5608=VECTOR('',#21168,1.);
#5609=VECTOR('',#21169,1.);
#5610=VECTOR('',#21172,1.);
#5611=VECTOR('',#21173,1.);
#5612=VECTOR('',#21174,1.);
#5613=VECTOR('',#21179,1.);
#5614=VECTOR('',#21180,1.);
#5615=VECTOR('',#21183,1.);
#5616=VECTOR('',#21184,1.);
#5617=VECTOR('',#21185,1.);
#5618=VECTOR('',#21190,1.);
#5619=VECTOR('',#21191,1.);
#5620=VECTOR('',#21194,1.);
#5621=VECTOR('',#21195,1.);
#5622=VECTOR('',#21196,1.);
#5623=VECTOR('',#21201,1.);
#5624=VECTOR('',#21202,1.);
#5625=VECTOR('',#21205,1.);
#5626=VECTOR('',#21206,1.);
#5627=VECTOR('',#21207,1.);
#5628=VECTOR('',#21212,1.);
#5629=VECTOR('',#21213,1.);
#5630=VECTOR('',#21216,1.);
#5631=VECTOR('',#21217,1.);
#5632=VECTOR('',#21218,1.);
#5633=VECTOR('',#21223,1.);
#5634=VECTOR('',#21224,1.);
#5635=VECTOR('',#21227,1.);
#5636=VECTOR('',#21228,1.);
#5637=VECTOR('',#21229,1.);
#5638=VECTOR('',#21234,1.);
#5639=VECTOR('',#21235,1.);
#5640=VECTOR('',#21238,1.);
#5641=VECTOR('',#21239,1.);
#5642=VECTOR('',#21240,1.);
#5643=VECTOR('',#21245,1.);
#5644=VECTOR('',#21246,1.);
#5645=VECTOR('',#21249,1.);
#5646=VECTOR('',#21250,1.);
#5647=VECTOR('',#21251,1.);
#5648=VECTOR('',#21256,1.);
#5649=VECTOR('',#21257,1.);
#5650=VECTOR('',#21260,1.);
#5651=VECTOR('',#21261,1.);
#5652=VECTOR('',#21262,1.);
#5653=VECTOR('',#21267,1.);
#5654=VECTOR('',#21268,1.);
#5655=VECTOR('',#21271,1.);
#5656=VECTOR('',#21272,1.);
#5657=VECTOR('',#21273,1.);
#5658=VECTOR('',#21278,1.);
#5659=VECTOR('',#21279,1.);
#5660=VECTOR('',#21282,1.);
#5661=VECTOR('',#21283,1.);
#5662=VECTOR('',#21284,1.);
#5663=VECTOR('',#21295,1.);
#5664=VECTOR('',#21296,1.);
#5665=VECTOR('',#21297,1.);
#5666=VECTOR('',#21298,1.);
#5667=VECTOR('',#21299,1.);
#5668=VECTOR('',#21300,1.);
#5669=VECTOR('',#21301,1.);
#5670=VECTOR('',#21302,1.);
#5671=VECTOR('',#21305,1.);
#5672=VECTOR('',#21306,1.);
#5673=VECTOR('',#21307,1.);
#5674=VECTOR('',#21310,1.);
#5675=VECTOR('',#21311,1.);
#5676=VECTOR('',#21314,1.);
#5677=VECTOR('',#21315,1.);
#5678=VECTOR('',#21318,1.);
#5679=VECTOR('',#21319,1.);
#5680=VECTOR('',#21322,1.);
#5681=VECTOR('',#21323,1.);
#5682=VECTOR('',#21324,1.);
#5683=VECTOR('',#21325,1.);
#5684=VECTOR('',#21328,1.);
#5685=VECTOR('',#21331,1.);
#5686=VECTOR('',#21334,1.);
#5687=VECTOR('',#21343,1.);
#5688=VECTOR('',#21344,1.);
#5689=VECTOR('',#21345,1.);
#5690=VECTOR('',#21346,1.);
#5691=VECTOR('',#21351,1.);
#5692=VECTOR('',#21352,1.);
#5693=VECTOR('',#21355,1.);
#5694=VECTOR('',#21356,1.);
#5695=VECTOR('',#21357,1.);
#5696=VECTOR('',#21360,1.);
#5697=VECTOR('',#21367,1.);
#5698=VECTOR('',#21368,1.);
#5699=VECTOR('',#21369,1.);
#5700=VECTOR('',#21370,1.);
#5701=VECTOR('',#21375,1.);
#5702=VECTOR('',#21376,1.);
#5703=VECTOR('',#21379,1.);
#5704=VECTOR('',#21380,1.);
#5705=VECTOR('',#21381,1.);
#5706=VECTOR('',#21384,1.);
#5707=VECTOR('',#21393,1.);
#5708=VECTOR('',#21404,1.);
#5709=VECTOR('',#21411,0.21);
#5710=VECTOR('',#21416,1.);
#5711=VECTOR('',#21421,1.005);
#5712=VECTOR('',#21428,1.4);
#5713=VECTOR('',#21439,1.);
#5714=VECTOR('',#21446,0.21);
#5715=VECTOR('',#21451,1.);
#5716=VECTOR('',#21456,1.005);
#5717=VECTOR('',#21463,1.4);
#5718=VECTOR('',#21476,1.005);
#5719=VECTOR('',#21483,1.3);
#5720=VECTOR('',#21496,1.005);
#5721=VECTOR('',#21503,1.3);
#5722=VECTOR('',#21516,1.005);
#5723=VECTOR('',#21523,1.3);
#5724=VECTOR('',#21536,1.005);
#5725=VECTOR('',#21543,1.3);
#5726=VECTOR('',#21556,1.005);
#5727=VECTOR('',#21563,1.3);
#5728=VECTOR('',#21574,1.);
#5729=VECTOR('',#21575,1.);
#5730=VECTOR('',#21576,1.);
#5731=VECTOR('',#21577,1.);
#5732=VECTOR('',#21580,1.);
#5733=VECTOR('',#21581,1.);
#5734=VECTOR('',#21582,1.);
#5735=VECTOR('',#21585,1.);
#5736=VECTOR('',#21586,1.);
#5737=VECTOR('',#21587,1.);
#5738=VECTOR('',#21602,1.);
#5739=VECTOR('',#21605,1.);
#5740=VECTOR('',#21608,1.);
#5741=VECTOR('',#21611,1.);
#5742=VECTOR('',#21614,1.);
#5743=VECTOR('',#21617,1.);
#5744=VECTOR('',#21620,1.);
#5745=VECTOR('',#21623,1.);
#5746=VECTOR('',#21626,1.);
#5747=VECTOR('',#21629,1.);
#5748=VECTOR('',#21632,1.);
#5749=VECTOR('',#21635,1.);
#5750=VECTOR('',#21638,1.);
#5751=VECTOR('',#21641,1.);
#5752=VECTOR('',#21644,1.);
#5753=VECTOR('',#21647,1.);
#5754=VECTOR('',#21650,1.);
#5755=VECTOR('',#21653,1.);
#5756=VECTOR('',#21656,1.);
#5757=VECTOR('',#21659,1.);
#5758=VECTOR('',#21662,1.4);
#5759=VECTOR('',#21665,1.);
#5760=VECTOR('',#21666,1.);
#5761=VECTOR('',#21669,1.);
#5762=VECTOR('',#21670,1.);
#5763=VECTOR('',#21671,1.);
#5764=VECTOR('',#21676,1.);
#5765=VECTOR('',#21677,1.);
#5766=VECTOR('',#21680,1.);
#5767=VECTOR('',#21681,1.);
#5768=VECTOR('',#21682,1.);
#5769=VECTOR('',#21687,1.);
#5770=VECTOR('',#21688,1.);
#5771=VECTOR('',#21691,1.);
#5772=VECTOR('',#21692,1.);
#5773=VECTOR('',#21693,1.);
#5774=VECTOR('',#21698,1.);
#5775=VECTOR('',#21699,1.);
#5776=VECTOR('',#21702,1.);
#5777=VECTOR('',#21703,1.);
#5778=VECTOR('',#21704,1.);
#5779=VECTOR('',#21709,1.);
#5780=VECTOR('',#21710,1.);
#5781=VECTOR('',#21713,1.);
#5782=VECTOR('',#21714,1.);
#5783=VECTOR('',#21715,1.);
#5784=VECTOR('',#21720,1.);
#5785=VECTOR('',#21721,1.);
#5786=VECTOR('',#21724,1.);
#5787=VECTOR('',#21725,1.);
#5788=VECTOR('',#21726,1.);
#5789=VECTOR('',#21731,1.);
#5790=VECTOR('',#21732,1.);
#5791=VECTOR('',#21735,1.);
#5792=VECTOR('',#21736,1.);
#5793=VECTOR('',#21737,1.);
#5794=VECTOR('',#21742,1.);
#5795=VECTOR('',#21743,1.);
#5796=VECTOR('',#21746,1.);
#5797=VECTOR('',#21747,1.);
#5798=VECTOR('',#21748,1.);
#5799=VECTOR('',#21753,1.);
#5800=VECTOR('',#21754,1.);
#5801=VECTOR('',#21757,1.);
#5802=VECTOR('',#21758,1.);
#5803=VECTOR('',#21759,1.);
#5804=VECTOR('',#21764,1.);
#5805=VECTOR('',#21765,1.);
#5806=VECTOR('',#21768,1.);
#5807=VECTOR('',#21769,1.);
#5808=VECTOR('',#21770,1.);
#5809=VECTOR('',#21775,1.);
#5810=VECTOR('',#21776,1.);
#5811=VECTOR('',#21779,1.);
#5812=VECTOR('',#21780,1.);
#5813=VECTOR('',#21781,1.);
#5814=VECTOR('',#21786,1.);
#5815=VECTOR('',#21787,1.);
#5816=VECTOR('',#21790,1.);
#5817=VECTOR('',#21791,1.);
#5818=VECTOR('',#21792,1.);
#5819=VECTOR('',#21797,1.);
#5820=VECTOR('',#21798,1.);
#5821=VECTOR('',#21801,1.);
#5822=VECTOR('',#21802,1.);
#5823=VECTOR('',#21803,1.);
#5824=VECTOR('',#21808,1.);
#5825=VECTOR('',#21809,1.);
#5826=VECTOR('',#21812,1.);
#5827=VECTOR('',#21813,1.);
#5828=VECTOR('',#21814,1.);
#5829=VECTOR('',#21819,1.);
#5830=VECTOR('',#21820,1.);
#5831=VECTOR('',#21823,1.);
#5832=VECTOR('',#21824,1.);
#5833=VECTOR('',#21825,1.);
#5834=VECTOR('',#21830,1.);
#5835=VECTOR('',#21831,1.);
#5836=VECTOR('',#21834,1.);
#5837=VECTOR('',#21835,1.);
#5838=VECTOR('',#21836,1.);
#5839=VECTOR('',#21841,1.);
#5840=VECTOR('',#21842,1.);
#5841=VECTOR('',#21845,1.);
#5842=VECTOR('',#21846,1.);
#5843=VECTOR('',#21847,1.);
#5844=VECTOR('',#21852,1.);
#5845=VECTOR('',#21853,1.);
#5846=VECTOR('',#21856,1.);
#5847=VECTOR('',#21857,1.);
#5848=VECTOR('',#21858,1.);
#5849=VECTOR('',#21863,1.);
#5850=VECTOR('',#21864,1.);
#5851=VECTOR('',#21867,1.);
#5852=VECTOR('',#21868,1.);
#5853=VECTOR('',#21869,1.);
#5854=VECTOR('',#21874,1.);
#5855=VECTOR('',#21875,1.);
#5856=VECTOR('',#21878,1.);
#5857=VECTOR('',#21879,1.);
#5858=VECTOR('',#21880,1.);
#5859=VECTOR('',#21893,1.);
#5860=VECTOR('',#21894,1.);
#5861=VECTOR('',#21895,1.);
#5862=VECTOR('',#21896,1.);
#5863=VECTOR('',#21901,1.);
#5864=VECTOR('',#21902,1.);
#5865=VECTOR('',#21905,1.);
#5866=VECTOR('',#21906,1.);
#5867=VECTOR('',#21907,1.);
#5868=VECTOR('',#21910,1.);
#5869=VECTOR('',#21919,1.);
#5870=VECTOR('',#21930,1.);
#5871=VECTOR('',#21937,0.210000000000001);
#5872=VECTOR('',#21942,1.);
#5873=VECTOR('',#21947,1.005);
#5874=VECTOR('',#21954,1.4);
#5875=VECTOR('',#21965,1.);
#5876=VECTOR('',#21972,0.210000000000001);
#5877=VECTOR('',#21977,1.);
#5878=VECTOR('',#21982,1.005);
#5879=VECTOR('',#21989,1.4);
#5880=VECTOR('',#22002,1.005);
#5881=VECTOR('',#22009,1.3);
#5882=VECTOR('',#22022,1.005);
#5883=VECTOR('',#22029,1.3);
#5884=VECTOR('',#22042,1.005);
#5885=VECTOR('',#22049,1.3);
#5886=VECTOR('',#22062,1.005);
#5887=VECTOR('',#22069,1.3);
#5888=VECTOR('',#22080,1.);
#5889=VECTOR('',#22081,1.);
#5890=VECTOR('',#22082,1.);
#5891=VECTOR('',#22083,1.);
#5892=VECTOR('',#22086,1.);
#5893=VECTOR('',#22087,1.);
#5894=VECTOR('',#22088,1.);
#5895=VECTOR('',#22091,1.);
#5896=VECTOR('',#22092,1.);
#5897=VECTOR('',#22093,1.);
#5898=VECTOR('',#22096,1.);
#5899=VECTOR('',#22097,1.);
#5900=VECTOR('',#22098,1.);
#5901=VECTOR('',#22101,1.);
#5902=VECTOR('',#22102,1.);
#5903=VECTOR('',#22103,1.);
#5904=VECTOR('',#22106,1.);
#5905=VECTOR('',#22107,1.);
#5906=VECTOR('',#22118,0.235);
#5907=VECTOR('',#22123,0.25);
#5908=VECTOR('',#22128,0.2125);
#5909=VECTOR('',#22157,1.);
#5910=VECTOR('',#22158,1.);
#5911=VECTOR('',#22159,1.);
#5912=VECTOR('',#22160,1.);
#5913=VECTOR('',#22163,1.);
#5914=VECTOR('',#22164,1.);
#5915=VECTOR('',#22165,1.);
#5916=VECTOR('',#22168,1.);
#5917=VECTOR('',#22169,1.);
#5918=VECTOR('',#22170,1.);
#5919=VECTOR('',#22175,1.);
#5920=VECTOR('',#22178,1.);
#5921=VECTOR('',#22181,1.);
#5922=VECTOR('',#22184,1.);
#5923=VECTOR('',#22187,1.);
#5924=VECTOR('',#22190,1.);
#5925=VECTOR('',#22193,1.);
#5926=VECTOR('',#22196,1.);
#5927=VECTOR('',#22199,1.);
#5928=VECTOR('',#22202,1.);
#5929=VECTOR('',#22205,1.);
#5930=VECTOR('',#22208,1.);
#5931=VECTOR('',#22211,1.);
#5932=VECTOR('',#22214,1.);
#5933=VECTOR('',#22217,1.);
#5934=VECTOR('',#22220,1.);
#5935=VECTOR('',#22223,1.);
#5936=VECTOR('',#22226,1.);
#5937=VECTOR('',#22229,1.);
#5938=VECTOR('',#22232,1.);
#5939=VECTOR('',#22235,1.);
#5940=VECTOR('',#22238,1.);
#5941=VECTOR('',#22241,1.);
#5942=VECTOR('',#22244,1.);
#5943=VECTOR('',#22247,1.);
#5944=VECTOR('',#22250,1.);
#5945=VECTOR('',#22253,1.);
#5946=VECTOR('',#22256,1.);
#5947=VECTOR('',#22259,1.);
#5948=VECTOR('',#22262,1.);
#5949=VECTOR('',#22265,1.);
#5950=VECTOR('',#22268,1.);
#5951=VECTOR('',#22271,1.);
#5952=VECTOR('',#22274,1.);
#5953=VECTOR('',#22277,1.);
#5954=VECTOR('',#22280,1.);
#5955=VECTOR('',#22283,1.);
#5956=VECTOR('',#22286,1.);
#5957=VECTOR('',#22289,1.);
#5958=VECTOR('',#22292,1.);
#5959=VECTOR('',#22303,2.);
#5960=VECTOR('',#22308,1.);
#5961=VECTOR('',#22309,1.);
#5962=VECTOR('',#22312,1.);
#5963=VECTOR('',#22317,1.);
#5964=VECTOR('',#22318,1.);
#5965=VECTOR('',#22321,1.);
#5966=VECTOR('',#22326,1.);
#5967=VECTOR('',#22327,1.);
#5968=VECTOR('',#22330,1.);
#5969=VECTOR('',#22335,1.);
#5970=VECTOR('',#22336,1.);
#5971=VECTOR('',#22339,1.);
#5972=VECTOR('',#22344,1.);
#5973=VECTOR('',#22345,1.);
#5974=VECTOR('',#22348,1.);
#5975=VECTOR('',#22353,1.);
#5976=VECTOR('',#22354,1.);
#5977=VECTOR('',#22357,1.);
#5978=VECTOR('',#22362,1.);
#5979=VECTOR('',#22363,1.);
#5980=VECTOR('',#22366,1.);
#5981=VECTOR('',#22371,1.);
#5982=VECTOR('',#22372,1.);
#5983=VECTOR('',#22375,1.);
#5984=VECTOR('',#22380,1.);
#5985=VECTOR('',#22381,1.);
#5986=VECTOR('',#22384,1.);
#5987=VECTOR('',#22389,1.);
#5988=VECTOR('',#22390,1.);
#5989=VECTOR('',#22393,1.);
#5990=VECTOR('',#22398,1.);
#5991=VECTOR('',#22399,1.);
#5992=VECTOR('',#22402,1.);
#5993=VECTOR('',#22407,1.);
#5994=VECTOR('',#22408,1.);
#5995=VECTOR('',#22411,1.);
#5996=VECTOR('',#22416,1.);
#5997=VECTOR('',#22417,1.);
#5998=VECTOR('',#22420,1.);
#5999=VECTOR('',#22425,1.);
#6000=VECTOR('',#22426,1.);
#6001=VECTOR('',#22429,1.);
#6002=VECTOR('',#22434,1.);
#6003=VECTOR('',#22435,1.);
#6004=VECTOR('',#22438,1.);
#6005=VECTOR('',#22443,1.);
#6006=VECTOR('',#22444,1.);
#6007=VECTOR('',#22447,1.);
#6008=VECTOR('',#22452,1.);
#6009=VECTOR('',#22453,1.);
#6010=VECTOR('',#22456,1.);
#6011=VECTOR('',#22461,1.);
#6012=VECTOR('',#22462,1.);
#6013=VECTOR('',#22465,1.);
#6014=VECTOR('',#22470,1.);
#6015=VECTOR('',#22471,1.);
#6016=VECTOR('',#22474,1.);
#6017=VECTOR('',#22479,1.);
#6018=VECTOR('',#22480,1.);
#6019=VECTOR('',#22483,1.);
#6020=VECTOR('',#22488,1.);
#6021=VECTOR('',#22489,1.);
#6022=VECTOR('',#22492,1.);
#6023=VECTOR('',#22497,1.);
#6024=VECTOR('',#22498,1.);
#6025=VECTOR('',#22501,1.);
#6026=VECTOR('',#22506,1.);
#6027=VECTOR('',#22507,1.);
#6028=VECTOR('',#22510,1.);
#6029=VECTOR('',#22515,1.);
#6030=VECTOR('',#22516,1.);
#6031=VECTOR('',#22519,1.);
#6032=VECTOR('',#22524,1.);
#6033=VECTOR('',#22525,1.);
#6034=VECTOR('',#22528,1.);
#6035=VECTOR('',#22533,1.);
#6036=VECTOR('',#22534,1.);
#6037=VECTOR('',#22537,1.);
#6038=VECTOR('',#22542,1.);
#6039=VECTOR('',#22543,1.);
#6040=VECTOR('',#22546,1.);
#6041=VECTOR('',#22551,1.);
#6042=VECTOR('',#22552,1.);
#6043=VECTOR('',#22555,1.);
#6044=VECTOR('',#22560,1.);
#6045=VECTOR('',#22561,1.);
#6046=VECTOR('',#22564,1.);
#6047=VECTOR('',#22569,1.);
#6048=VECTOR('',#22570,1.);
#6049=VECTOR('',#22573,1.);
#6050=VECTOR('',#22578,1.);
#6051=VECTOR('',#22579,1.);
#6052=VECTOR('',#22582,1.);
#6053=VECTOR('',#22587,1.);
#6054=VECTOR('',#22588,1.);
#6055=VECTOR('',#22591,1.);
#6056=VECTOR('',#22596,1.);
#6057=VECTOR('',#22597,1.);
#6058=VECTOR('',#22600,1.);
#6059=VECTOR('',#22605,1.);
#6060=VECTOR('',#22606,1.);
#6061=VECTOR('',#22609,1.);
#6062=VECTOR('',#22614,1.);
#6063=VECTOR('',#22615,1.);
#6064=VECTOR('',#22618,1.);
#6065=VECTOR('',#22623,1.);
#6066=VECTOR('',#22624,1.);
#6067=VECTOR('',#22627,1.);
#6068=VECTOR('',#22632,1.);
#6069=VECTOR('',#22633,1.);
#6070=VECTOR('',#22636,1.);
#6071=VECTOR('',#22641,1.);
#6072=VECTOR('',#22642,1.);
#6073=VECTOR('',#22645,1.);
#6074=VECTOR('',#22650,1.);
#6075=VECTOR('',#22653,1.);
#6076=VECTOR('',#22654,1.);
#6077=VECTOR('',#22659,1.);
#6078=VECTOR('',#22660,1.);
#6079=VECTOR('',#22663,1.);
#6080=VECTOR('',#22674,1.);
#6081=VECTOR('',#22675,1.);
#6082=VECTOR('',#22676,1.);
#6083=VECTOR('',#22677,1.);
#6084=VECTOR('',#22678,1.);
#6085=VECTOR('',#22679,1.);
#6086=VECTOR('',#22680,1.);
#6087=VECTOR('',#22681,1.);
#6088=VECTOR('',#22684,1.);
#6089=VECTOR('',#22685,1.);
#6090=VECTOR('',#22686,1.);
#6091=VECTOR('',#22689,1.);
#6092=VECTOR('',#22690,1.);
#6093=VECTOR('',#22693,1.);
#6094=VECTOR('',#22694,1.);
#6095=VECTOR('',#22697,1.);
#6096=VECTOR('',#22698,1.);
#6097=VECTOR('',#22701,1.);
#6098=VECTOR('',#22702,1.);
#6099=VECTOR('',#22703,1.);
#6100=VECTOR('',#22704,1.);
#6101=VECTOR('',#22707,1.);
#6102=VECTOR('',#22710,1.);
#6103=VECTOR('',#22713,1.);
#6104=CIRCLE('',#16816,0.25);
#6105=CIRCLE('',#16817,0.25);
#6106=CIRCLE('',#16819,0.25);
#6107=CIRCLE('',#16820,0.25);
#6108=CIRCLE('',#16822,0.25);
#6109=CIRCLE('',#16823,0.25);
#6110=CIRCLE('',#16825,0.25);
#6111=CIRCLE('',#16826,0.25);
#6112=CIRCLE('',#16835,0.164999999999999);
#6113=CIRCLE('',#16836,0.164999999999999);
#6114=CIRCLE('',#16839,0.164999999999999);
#6115=CIRCLE('',#16840,0.164999999999999);
#6116=CIRCLE('',#16843,0.164999999999999);
#6117=CIRCLE('',#16844,0.164999999999999);
#6118=CIRCLE('',#16847,0.164999999999999);
#6119=CIRCLE('',#16848,0.164999999999999);
#6120=CIRCLE('',#16851,2.35);
#6121=CIRCLE('',#16852,2.35);
#6122=CIRCLE('',#16854,1.9);
#6123=CIRCLE('',#16856,1.6);
#6124=CIRCLE('',#16857,2.35);
#6125=CIRCLE('',#16858,0.165);
#6126=CIRCLE('',#16859,0.165);
#6127=CIRCLE('',#16860,0.165);
#6128=CIRCLE('',#16861,0.165);
#6129=CIRCLE('',#16863,0.149999999999999);
#6130=CIRCLE('',#16864,0.25);
#6131=CIRCLE('',#16865,0.25);
#6132=CIRCLE('',#16866,0.25);
#6133=CIRCLE('',#16867,0.149999999999999);
#6134=CIRCLE('',#16869,2.35);
#6135=CIRCLE('',#16870,2.35);
#6136=CIRCLE('',#16872,1.9);
#6137=CIRCLE('',#16874,2.35);
#6138=CIRCLE('',#16875,1.6);
#6139=CIRCLE('',#16876,0.165);
#6140=CIRCLE('',#16877,0.165);
#6141=CIRCLE('',#16878,0.165);
#6142=CIRCLE('',#16879,0.165);
#6143=CIRCLE('',#16882,1.9);
#6144=CIRCLE('',#16884,1.9);
#6145=CIRCLE('',#16886,1.9);
#6146=CIRCLE('',#16887,1.2);
#6147=CIRCLE('',#16890,0.165);
#6148=CIRCLE('',#16893,0.165);
#6149=CIRCLE('',#16896,0.165);
#6150=CIRCLE('',#16899,0.165);
#6151=CIRCLE('',#16902,2.35);
#6152=CIRCLE('',#16904,1.9);
#6153=CIRCLE('',#16906,2.35);
#6154=CIRCLE('',#16908,1.9);
#6155=CIRCLE('',#16912,1.9);
#6156=CIRCLE('',#16914,1.2);
#6157=CIRCLE('',#16917,0.165);
#6158=CIRCLE('',#16920,0.165);
#6159=CIRCLE('',#16923,0.165);
#6160=CIRCLE('',#16926,0.165);
#6161=CIRCLE('',#16929,1.6);
#6162=CIRCLE('',#16931,1.2);
#6163=CIRCLE('',#16933,0.15);
#6164=CIRCLE('',#16934,0.25);
#6165=CIRCLE('',#16935,0.25);
#6166=CIRCLE('',#16936,0.25);
#6167=CIRCLE('',#16937,0.15);
#6168=CIRCLE('',#16939,1.6);
#6169=CIRCLE('',#16941,1.2);
#6170=CIRCLE('',#16945,0.6);
#6171=CIRCLE('',#16946,0.6);
#6172=CIRCLE('',#16948,0.33);
#6173=CIRCLE('',#16950,0.6);
#6174=CIRCLE('',#16951,0.6);
#6175=CIRCLE('',#16953,0.33);
#6176=CIRCLE('',#16955,0.6);
#6177=CIRCLE('',#16956,0.6);
#6178=CIRCLE('',#16958,0.33);
#6179=CIRCLE('',#16960,0.6);
#6180=CIRCLE('',#16961,0.6);
#6181=CIRCLE('',#16963,0.33);
#6182=CIRCLE('',#16965,0.33);
#6183=CIRCLE('',#16967,0.33);
#6184=CIRCLE('',#16969,0.33);
#6185=CIRCLE('',#16971,0.33);
#6186=CIRCLE('',#16973,0.149999999999999);
#6187=CIRCLE('',#16976,0.149999999999999);
#6188=CIRCLE('',#16979,0.15);
#6189=CIRCLE('',#16982,0.15);
#6190=CIRCLE('',#16985,0.25);
#6191=CIRCLE('',#16987,0.25);
#6192=CIRCLE('',#16989,0.25);
#6193=CIRCLE('',#16991,0.25);
#6194=CIRCLE('',#16993,0.25);
#6195=CIRCLE('',#16995,0.25);
#6196=CIRCLE('',#17008,0.164999999999999);
#6197=CIRCLE('',#17009,0.164999999999999);
#6198=CIRCLE('',#17011,0.165);
#6199=CIRCLE('',#17012,0.165);
#6200=CIRCLE('',#17014,0.165);
#6201=CIRCLE('',#17015,0.165);
#6202=CIRCLE('',#17017,0.164999999999999);
#6203=CIRCLE('',#17018,0.164999999999999);
#6204=CIRCLE('',#17024,0.164999999999999);
#6205=CIRCLE('',#17025,0.164999999999999);
#6206=CIRCLE('',#17028,0.164999999999999);
#6207=CIRCLE('',#17029,0.164999999999999);
#6208=CIRCLE('',#17032,0.164999999999999);
#6209=CIRCLE('',#17033,0.164999999999999);
#6210=CIRCLE('',#17036,0.164999999999999);
#6211=CIRCLE('',#17037,0.164999999999999);
#6212=CIRCLE('',#17040,2.35);
#6213=CIRCLE('',#17041,1.9);
#6214=CIRCLE('',#17043,2.35);
#6215=CIRCLE('',#17045,1.9);
#6216=CIRCLE('',#17047,0.149999999999999);
#6217=CIRCLE('',#17048,0.329999999999998);
#6218=CIRCLE('',#17049,0.329999999999998);
#6219=CIRCLE('',#17050,0.329999999999998);
#6220=CIRCLE('',#17051,0.149999999999999);
#6221=CIRCLE('',#17053,2.35);
#6222=CIRCLE('',#17054,2.35);
#6223=CIRCLE('',#17056,1.9);
#6224=CIRCLE('',#17058,1.6);
#6225=CIRCLE('',#17059,2.35);
#6226=CIRCLE('',#17060,0.165);
#6227=CIRCLE('',#17061,0.165);
#6228=CIRCLE('',#17062,0.165);
#6229=CIRCLE('',#17063,0.165);
#6230=CIRCLE('',#17065,1.9);
#6231=CIRCLE('',#17067,2.35);
#6232=CIRCLE('',#17068,1.6);
#6233=CIRCLE('',#17069,0.165);
#6234=CIRCLE('',#17070,0.165);
#6235=CIRCLE('',#17071,0.165);
#6236=CIRCLE('',#17072,0.165);
#6237=CIRCLE('',#17074,1.9);
#6238=CIRCLE('',#17075,1.2);
#6239=CIRCLE('',#17079,0.165);
#6240=CIRCLE('',#17082,0.165);
#6241=CIRCLE('',#17085,0.165);
#6242=CIRCLE('',#17088,0.165);
#6243=CIRCLE('',#17091,2.35);
#6244=CIRCLE('',#17092,1.9);
#6245=CIRCLE('',#17095,1.9);
#6246=CIRCLE('',#17097,2.35);
#6247=CIRCLE('',#17099,1.9);
#6248=CIRCLE('',#17104,0.165);
#6249=CIRCLE('',#17107,0.165);
#6250=CIRCLE('',#17110,0.165);
#6251=CIRCLE('',#17113,0.165);
#6252=CIRCLE('',#17116,1.6);
#6253=CIRCLE('',#17118,1.2);
#6254=CIRCLE('',#17120,1.6);
#6255=CIRCLE('',#17122,1.2);
#6256=CIRCLE('',#17125,1.2);
#6257=CIRCLE('',#17128,0.15);
#6258=CIRCLE('',#17129,0.33);
#6259=CIRCLE('',#17130,0.33);
#6260=CIRCLE('',#17131,0.33);
#6261=CIRCLE('',#17132,0.15);
#6262=CIRCLE('',#17134,0.149999999999999);
#6263=CIRCLE('',#17137,0.149999999999999);
#6264=CIRCLE('',#17140,0.15);
#6265=CIRCLE('',#17143,0.15);
#6266=CIRCLE('',#17146,0.329999999999998);
#6267=CIRCLE('',#17148,0.33);
#6268=CIRCLE('',#17150,0.33);
#6269=CIRCLE('',#17152,0.33);
#6270=CIRCLE('',#17154,0.329999999999998);
#6271=CIRCLE('',#17156,0.329999999999998);
#6272=CIRCLE('',#17169,0.15);
#6273=CIRCLE('',#17170,0.15);
#6274=CIRCLE('',#17175,0.15);
#6275=CIRCLE('',#17176,0.15);
#6276=CIRCLE('',#17181,0.149999999999999);
#6277=CIRCLE('',#17182,0.149999999999999);
#6278=CIRCLE('',#17187,0.149999999999999);
#6279=CIRCLE('',#17188,0.149999999999999);
#6280=CIRCLE('',#17193,0.225);
#6281=CIRCLE('',#17194,0.225);
#6282=CIRCLE('',#17196,0.225);
#6283=CIRCLE('',#17197,0.225);
#6284=CIRCLE('',#17199,0.225);
#6285=CIRCLE('',#17200,0.225);
#6286=CIRCLE('',#17202,0.225);
#6287=CIRCLE('',#17203,0.225);
#6288=CIRCLE('',#17205,2.2);
#6289=CIRCLE('',#17206,2.2);
#6290=CIRCLE('',#17207,2.2);
#6291=CIRCLE('',#17208,2.2);
#6292=CIRCLE('',#17209,1.2);
#6293=CIRCLE('',#17211,2.2);
#6294=CIRCLE('',#17213,2.2);
#6295=CIRCLE('',#17215,2.2);
#6296=CIRCLE('',#17217,2.2);
#6297=CIRCLE('',#17219,1.59);
#6298=CIRCLE('',#17220,1.59);
#6299=CIRCLE('',#17222,1.2);
#6300=CIRCLE('',#17227,0.225);
#6301=CIRCLE('',#17228,0.225);
#6302=CIRCLE('',#17230,0.225);
#6303=CIRCLE('',#17231,0.225);
#6304=CIRCLE('',#17233,0.225);
#6305=CIRCLE('',#17234,0.225);
#6306=CIRCLE('',#17236,0.225);
#6307=CIRCLE('',#17237,0.225);
#6308=CIRCLE('',#17239,2.2);
#6309=CIRCLE('',#17240,2.2);
#6310=CIRCLE('',#17241,2.2);
#6311=CIRCLE('',#17242,2.2);
#6312=CIRCLE('',#17243,1.59);
#6313=CIRCLE('',#17245,2.2);
#6314=CIRCLE('',#17247,2.2);
#6315=CIRCLE('',#17249,2.2);
#6316=CIRCLE('',#17251,2.2);
#6317=CIRCLE('',#17253,1.59);
#6318=CIRCLE('',#17255,1.2);
#6319=CIRCLE('',#17257,1.2);
#6320=CIRCLE('',#17261,0.225);
#6321=CIRCLE('',#17262,0.225);
#6322=CIRCLE('',#17264,0.225);
#6323=CIRCLE('',#17265,0.225);
#6324=CIRCLE('',#17267,0.225000000000001);
#6325=CIRCLE('',#17268,0.225000000000001);
#6326=CIRCLE('',#17270,0.225000000000001);
#6327=CIRCLE('',#17271,0.225000000000001);
#6328=CIRCLE('',#17273,2.34);
#6329=CIRCLE('',#17274,2.34);
#6330=CIRCLE('',#17276,1.9);
#6331=CIRCLE('',#17278,1.9);
#6332=CIRCLE('',#17280,2.9);
#6333=CIRCLE('',#17281,2.9);
#6334=CIRCLE('',#17286,0.225);
#6335=CIRCLE('',#17287,0.225);
#6336=CIRCLE('',#17289,0.225);
#6337=CIRCLE('',#17290,0.225);
#6338=CIRCLE('',#17292,0.225000000000001);
#6339=CIRCLE('',#17293,0.225000000000001);
#6340=CIRCLE('',#17295,0.225000000000001);
#6341=CIRCLE('',#17296,0.225000000000001);
#6342=CIRCLE('',#17298,2.34);
#6343=CIRCLE('',#17299,2.34);
#6344=CIRCLE('',#17301,1.9);
#6345=CIRCLE('',#17303,1.9);
#6346=CIRCLE('',#17305,2.9);
#6347=CIRCLE('',#17306,2.9);
#6348=CIRCLE('',#17311,0.225);
#6349=CIRCLE('',#17312,0.225);
#6350=CIRCLE('',#17314,0.225);
#6351=CIRCLE('',#17315,0.225);
#6352=CIRCLE('',#17317,0.225);
#6353=CIRCLE('',#17318,0.225);
#6354=CIRCLE('',#17320,0.225);
#6355=CIRCLE('',#17321,0.225);
#6356=CIRCLE('',#17323,2.34);
#6357=CIRCLE('',#17324,2.34);
#6358=CIRCLE('',#17326,1.9);
#6359=CIRCLE('',#17328,1.9);
#6360=CIRCLE('',#17330,2.9);
#6361=CIRCLE('',#17331,2.9);
#6362=CIRCLE('',#17336,0.225);
#6363=CIRCLE('',#17337,0.225);
#6364=CIRCLE('',#17339,0.225);
#6365=CIRCLE('',#17340,0.225);
#6366=CIRCLE('',#17342,0.225);
#6367=CIRCLE('',#17343,0.225);
#6368=CIRCLE('',#17345,0.225);
#6369=CIRCLE('',#17346,0.225);
#6370=CIRCLE('',#17348,2.34);
#6371=CIRCLE('',#17349,2.34);
#6372=CIRCLE('',#17351,1.9);
#6373=CIRCLE('',#17353,1.9);
#6374=CIRCLE('',#17355,2.9);
#6375=CIRCLE('',#17356,2.9);
#6376=CIRCLE('',#17361,0.225);
#6377=CIRCLE('',#17362,0.225);
#6378=CIRCLE('',#17364,0.225);
#6379=CIRCLE('',#17365,0.225);
#6380=CIRCLE('',#17367,0.225);
#6381=CIRCLE('',#17368,0.225);
#6382=CIRCLE('',#17370,0.225);
#6383=CIRCLE('',#17371,0.225);
#6384=CIRCLE('',#17402,0.2942);
#6385=CIRCLE('',#17404,0.45);
#6386=CIRCLE('',#17406,0.5);
#6387=CIRCLE('',#17408,0.5);
#6388=CIRCLE('',#17410,0.47);
#6389=CIRCLE('',#17412,0.32);
#6390=CIRCLE('',#17414,0.2942);
#6391=CIRCLE('',#17419,1.070235);
#6392=CIRCLE('',#17420,1.070235);
#6393=CIRCLE('',#17421,0.309556);
#6394=CIRCLE('',#17422,1.070235);
#6395=CIRCLE('',#17423,1.070235);
#6396=CIRCLE('',#17425,1.070235);
#6397=CIRCLE('',#17427,0.6);
#6398=CIRCLE('',#17428,0.6);
#6399=CIRCLE('',#17430,0.66);
#6400=CIRCLE('',#17433,1.070235);
#6401=CIRCLE('',#17435,0.66);
#6402=CIRCLE('',#17439,1.129765);
#6403=CIRCLE('',#17440,1.129765);
#6404=CIRCLE('',#17441,0.309556);
#6405=CIRCLE('',#17442,1.129765);
#6406=CIRCLE('',#17443,1.129765);
#6407=CIRCLE('',#17445,1.129765);
#6408=CIRCLE('',#17447,1.54);
#6409=CIRCLE('',#17448,1.129765);
#6410=CIRCLE('',#17450,1.6);
#6411=CIRCLE('',#17452,1.6);
#6412=CIRCLE('',#17454,1.54);
#6413=CIRCLE('',#17459,0.29765);
#6414=CIRCLE('',#17461,0.29765);
#6415=CIRCLE('',#17463,0.29765);
#6416=CIRCLE('',#17465,0.29765);
#6417=CIRCLE('',#17467,0.29765);
#6418=CIRCLE('',#17469,0.29765);
#6419=CIRCLE('',#17471,0.29765);
#6420=CIRCLE('',#17474,0.303778037777585);
#6421=CIRCLE('',#17475,0.303778037777585);
#6422=CIRCLE('',#17477,1.123812);
#6423=CIRCLE('',#17478,1.123812);
#6424=CIRCLE('',#17479,1.123812);
#6425=CIRCLE('',#17480,1.123812);
#6426=CIRCLE('',#17481,1.123812);
#6427=CIRCLE('',#17482,1.123812);
#6428=CIRCLE('',#17483,1.123812);
#6429=CIRCLE('',#17484,1.123812);
#6430=CIRCLE('',#17485,1.123812);
#6431=CIRCLE('',#17487,1.076188);
#6432=CIRCLE('',#17488,0.303778037777585);
#6433=CIRCLE('',#17490,0.303778037777585);
#6434=CIRCLE('',#17492,1.076188);
#6435=CIRCLE('',#17493,0.303778037777585);
#6436=CIRCLE('',#17495,0.303778037777585);
#6437=CIRCLE('',#17497,1.076188);
#6438=CIRCLE('',#17498,1.076188);
#6439=CIRCLE('',#17499,0.303778037777585);
#6440=CIRCLE('',#17501,0.303778037777585);
#6441=CIRCLE('',#17503,1.076188);
#6442=CIRCLE('',#17504,0.303778037777585);
#6443=CIRCLE('',#17506,0.303778037777585);
#6444=CIRCLE('',#17508,1.076188);
#6445=CIRCLE('',#17509,0.303778037777585);
#6446=CIRCLE('',#17511,0.303778037777585);
#6447=CIRCLE('',#17513,1.076188);
#6448=CIRCLE('',#17514,1.076188);
#6449=CIRCLE('',#17515,1.076188);
#6450=CIRCLE('',#17517,0.303778037777585);
#6451=CIRCLE('',#17519,0.303778037777585);
#6452=CIRCLE('',#17524,1.119765);
#6453=CIRCLE('',#17525,1.085235);
#6454=CIRCLE('',#17527,1.119765);
#6455=CIRCLE('',#17529,1.085235);
#6456=CIRCLE('',#17532,1.119765);
#6457=CIRCLE('',#17533,1.085235);
#6458=CIRCLE('',#17535,1.119765);
#6459=CIRCLE('',#17537,1.085235);
#6460=CIRCLE('',#17547,1.63531);
#6461=CIRCLE('',#17548,1.63531);
#6462=CIRCLE('',#17549,0.412776);
#6463=CIRCLE('',#17550,1.63531);
#6464=CIRCLE('',#17551,1.63531);
#6465=CIRCLE('',#17553,1.63531);
#6466=CIRCLE('',#17555,1.);
#6467=CIRCLE('',#17556,1.);
#6468=CIRCLE('',#17558,1.1);
#6469=CIRCLE('',#17561,1.63531);
#6470=CIRCLE('',#17563,1.1);
#6471=CIRCLE('',#17567,1.71469);
#6472=CIRCLE('',#17568,1.71469);
#6473=CIRCLE('',#17569,0.412776);
#6474=CIRCLE('',#17570,1.71469);
#6475=CIRCLE('',#17571,1.71469);
#6476=CIRCLE('',#17573,1.71469);
#6477=CIRCLE('',#17575,2.25);
#6478=CIRCLE('',#17576,1.71469);
#6479=CIRCLE('',#17578,2.35);
#6480=CIRCLE('',#17580,2.35);
#6481=CIRCLE('',#17582,2.25);
#6482=CIRCLE('',#17587,0.3969);
#6483=CIRCLE('',#17589,0.3969);
#6484=CIRCLE('',#17591,0.3969);
#6485=CIRCLE('',#17593,0.3969);
#6486=CIRCLE('',#17595,0.3969);
#6487=CIRCLE('',#17597,0.3969);
#6488=CIRCLE('',#17599,0.3969);
#6489=CIRCLE('',#17601,0.3969);
#6490=CIRCLE('',#17604,0.405071403305639);
#6491=CIRCLE('',#17605,0.405071403305639);
#6492=CIRCLE('',#17607,1.706752);
#6493=CIRCLE('',#17608,1.706752);
#6494=CIRCLE('',#17609,1.706752);
#6495=CIRCLE('',#17610,1.706752);
#6496=CIRCLE('',#17611,1.706752);
#6497=CIRCLE('',#17612,1.706752);
#6498=CIRCLE('',#17613,1.706752);
#6499=CIRCLE('',#17614,1.706752);
#6500=CIRCLE('',#17615,1.706752);
#6501=CIRCLE('',#17617,1.643248);
#6502=CIRCLE('',#17618,0.405071403305639);
#6503=CIRCLE('',#17620,0.405071403305639);
#6504=CIRCLE('',#17622,1.643248);
#6505=CIRCLE('',#17623,0.405071403305639);
#6506=CIRCLE('',#17625,0.405071403305639);
#6507=CIRCLE('',#17627,1.643248);
#6508=CIRCLE('',#17628,0.405071403305639);
#6509=CIRCLE('',#17630,0.405071403305639);
#6510=CIRCLE('',#17632,1.643248);
#6511=CIRCLE('',#17633,0.405071403305639);
#6512=CIRCLE('',#17635,0.405071403305639);
#6513=CIRCLE('',#17637,1.643248);
#6514=CIRCLE('',#17638,0.405071403305639);
#6515=CIRCLE('',#17640,0.405071403305639);
#6516=CIRCLE('',#17642,1.643248);
#6517=CIRCLE('',#17643,0.405071403305639);
#6518=CIRCLE('',#17645,0.405071403305639);
#6519=CIRCLE('',#17647,1.643248);
#6520=CIRCLE('',#17648,1.643248);
#6521=CIRCLE('',#17649,1.643248);
#6522=CIRCLE('',#17651,0.405071403305639);
#6523=CIRCLE('',#17653,0.405071403305639);
#6524=CIRCLE('',#17658,1.70469);
#6525=CIRCLE('',#17659,1.65031);
#6526=CIRCLE('',#17661,1.70469);
#6527=CIRCLE('',#17663,1.65031);
#6528=CIRCLE('',#17666,1.70469);
#6529=CIRCLE('',#17667,1.65031);
#6530=CIRCLE('',#17669,1.70469);
#6531=CIRCLE('',#17671,1.65031);
#6532=CIRCLE('',#17680,0.3);
#6533=CIRCLE('',#17682,0.35);
#6534=CIRCLE('',#17684,0.35);
#6535=CIRCLE('',#17686,0.32);
#6536=CIRCLE('',#17688,0.22);
#6537=CIRCLE('',#17690,0.1954);
#6538=CIRCLE('',#17692,0.1954);
#6539=CIRCLE('',#17694,0.16);
#6540=CIRCLE('',#17768,0.6);
#6541=CIRCLE('',#17772,0.6);
#6542=CIRCLE('',#17774,0.6);
#6543=CIRCLE('',#17775,0.6);
#6544=CIRCLE('',#17780,0.21);
#6545=CIRCLE('',#17782,0.21);
#6546=CIRCLE('',#17783,0.21);
#6547=CIRCLE('',#17786,0.605);
#6548=CIRCLE('',#17787,0.605);
#6549=CIRCLE('',#17789,1.);
#6550=CIRCLE('',#17790,1.);
#6551=CIRCLE('',#17795,0.21);
#6552=CIRCLE('',#17797,0.21);
#6553=CIRCLE('',#17798,0.21);
#6554=CIRCLE('',#17801,0.605);
#6555=CIRCLE('',#17802,0.605);
#6556=CIRCLE('',#17804,1.);
#6557=CIRCLE('',#17805,1.);
#6558=CIRCLE('',#17810,0.605);
#6559=CIRCLE('',#17811,0.605);
#6560=CIRCLE('',#17813,0.9);
#6561=CIRCLE('',#17814,0.9);
#6562=CIRCLE('',#17819,0.605);
#6563=CIRCLE('',#17820,0.605);
#6564=CIRCLE('',#17822,0.9);
#6565=CIRCLE('',#17823,0.9);
#6566=CIRCLE('',#17828,0.605);
#6567=CIRCLE('',#17829,0.605);
#6568=CIRCLE('',#17831,0.9);
#6569=CIRCLE('',#17832,0.9);
#6570=CIRCLE('',#17837,0.605);
#6571=CIRCLE('',#17838,0.605);
#6572=CIRCLE('',#17840,0.9);
#6573=CIRCLE('',#17841,0.9);
#6574=CIRCLE('',#17849,1.75);
#6575=CIRCLE('',#17850,1.75);
#6576=CIRCLE('',#17851,1.75);
#6577=CIRCLE('',#17852,1.75);
#6578=CIRCLE('',#17853,1.75);
#6579=CIRCLE('',#17854,1.75);
#6580=CIRCLE('',#17855,1.75);
#6581=CIRCLE('',#17856,1.75);
#6582=CIRCLE('',#17857,1.75);
#6583=CIRCLE('',#17858,1.75);
#6584=CIRCLE('',#17859,1.75);
#6585=CIRCLE('',#17860,1.75);
#6586=CIRCLE('',#17861,1.75);
#6587=CIRCLE('',#17862,1.75);
#6588=CIRCLE('',#17863,1.75);
#6589=CIRCLE('',#17864,1.75);
#6590=CIRCLE('',#17865,1.75);
#6591=CIRCLE('',#17866,1.75);
#6592=CIRCLE('',#17867,1.75);
#6593=CIRCLE('',#17868,1.75);
#6594=CIRCLE('',#17869,0.6);
#6595=CIRCLE('',#17871,0.6);
#6596=CIRCLE('',#17873,1.4);
#6597=CIRCLE('',#17874,1.4);
#6598=CIRCLE('',#17878,1.75);
#6599=CIRCLE('',#17881,1.75);
#6600=CIRCLE('',#17884,1.75);
#6601=CIRCLE('',#17887,1.75);
#6602=CIRCLE('',#17890,1.75);
#6603=CIRCLE('',#17893,1.75);
#6604=CIRCLE('',#17896,1.75);
#6605=CIRCLE('',#17899,1.75);
#6606=CIRCLE('',#17902,1.75);
#6607=CIRCLE('',#17905,1.75);
#6608=CIRCLE('',#17908,1.75);
#6609=CIRCLE('',#17911,1.75);
#6610=CIRCLE('',#17914,1.75);
#6611=CIRCLE('',#17917,1.75);
#6612=CIRCLE('',#17920,1.75);
#6613=CIRCLE('',#17923,1.75);
#6614=CIRCLE('',#17926,1.75);
#6615=CIRCLE('',#17929,1.75);
#6616=CIRCLE('',#17932,1.75);
#6617=CIRCLE('',#17935,1.75);
#6618=CIRCLE('',#17952,1.);
#6619=CIRCLE('',#17956,1.);
#6620=CIRCLE('',#17959,1.);
#6621=CIRCLE('',#17963,1.);
#6622=CIRCLE('',#17965,1.);
#6623=CIRCLE('',#17966,1.);
#6624=CIRCLE('',#17971,0.21);
#6625=CIRCLE('',#17973,0.21);
#6626=CIRCLE('',#17974,0.21);
#6627=CIRCLE('',#17977,1.005);
#6628=CIRCLE('',#17978,1.005);
#6629=CIRCLE('',#17980,1.4);
#6630=CIRCLE('',#17981,1.4);
#6631=CIRCLE('',#17986,0.21);
#6632=CIRCLE('',#17988,0.21);
#6633=CIRCLE('',#17989,0.21);
#6634=CIRCLE('',#17992,1.005);
#6635=CIRCLE('',#17993,1.005);
#6636=CIRCLE('',#17995,1.4);
#6637=CIRCLE('',#17996,1.4);
#6638=CIRCLE('',#18001,1.005);
#6639=CIRCLE('',#18002,1.005);
#6640=CIRCLE('',#18004,1.3);
#6641=CIRCLE('',#18005,1.3);
#6642=CIRCLE('',#18010,1.005);
#6643=CIRCLE('',#18011,1.005);
#6644=CIRCLE('',#18013,1.3);
#6645=CIRCLE('',#18014,1.3);
#6646=CIRCLE('',#18019,1.005);
#6647=CIRCLE('',#18020,1.005);
#6648=CIRCLE('',#18022,1.3);
#6649=CIRCLE('',#18023,1.3);
#6650=CIRCLE('',#18028,1.005);
#6651=CIRCLE('',#18029,1.005);
#6652=CIRCLE('',#18031,1.3);
#6653=CIRCLE('',#18032,1.3);
#6654=CIRCLE('',#18037,1.005);
#6655=CIRCLE('',#18038,1.005);
#6656=CIRCLE('',#18040,1.3);
#6657=CIRCLE('',#18041,1.3);
#6658=CIRCLE('',#18049,1.4);
#6659=CIRCLE('',#18050,1.);
#6660=CIRCLE('',#18052,1.);
#6661=CIRCLE('',#18054,1.75);
#6662=CIRCLE('',#18055,1.75);
#6663=CIRCLE('',#18056,1.75);
#6664=CIRCLE('',#18057,1.75);
#6665=CIRCLE('',#18058,1.75);
#6666=CIRCLE('',#18059,1.75);
#6667=CIRCLE('',#18060,1.75);
#6668=CIRCLE('',#18061,1.75);
#6669=CIRCLE('',#18062,1.75);
#6670=CIRCLE('',#18063,1.75);
#6671=CIRCLE('',#18064,1.75);
#6672=CIRCLE('',#18065,1.75);
#6673=CIRCLE('',#18066,1.75);
#6674=CIRCLE('',#18067,1.75);
#6675=CIRCLE('',#18068,1.75);
#6676=CIRCLE('',#18069,1.75);
#6677=CIRCLE('',#18070,1.75);
#6678=CIRCLE('',#18071,1.75);
#6679=CIRCLE('',#18072,1.75);
#6680=CIRCLE('',#18073,1.75);
#6681=CIRCLE('',#18075,1.4);
#6682=CIRCLE('',#18078,1.75);
#6683=CIRCLE('',#18081,1.75);
#6684=CIRCLE('',#18084,1.75);
#6685=CIRCLE('',#18087,1.75);
#6686=CIRCLE('',#18090,1.75);
#6687=CIRCLE('',#18093,1.75);
#6688=CIRCLE('',#18096,1.75);
#6689=CIRCLE('',#18099,1.75);
#6690=CIRCLE('',#18102,1.75);
#6691=CIRCLE('',#18105,1.75);
#6692=CIRCLE('',#18108,1.75);
#6693=CIRCLE('',#18111,1.75);
#6694=CIRCLE('',#18114,1.75);
#6695=CIRCLE('',#18117,1.75);
#6696=CIRCLE('',#18120,1.75);
#6697=CIRCLE('',#18123,1.75);
#6698=CIRCLE('',#18126,1.75);
#6699=CIRCLE('',#18129,1.75);
#6700=CIRCLE('',#18132,1.75);
#6701=CIRCLE('',#18135,1.75);
#6702=CIRCLE('',#18141,1.);
#6703=CIRCLE('',#18145,1.);
#6704=CIRCLE('',#18147,1.);
#6705=CIRCLE('',#18148,1.);
#6706=CIRCLE('',#18153,0.210000000000001);
#6707=CIRCLE('',#18155,0.210000000000001);
#6708=CIRCLE('',#18156,0.210000000000001);
#6709=CIRCLE('',#18159,1.005);
#6710=CIRCLE('',#18160,1.005);
#6711=CIRCLE('',#18162,1.4);
#6712=CIRCLE('',#18163,1.4);
#6713=CIRCLE('',#18168,0.210000000000001);
#6714=CIRCLE('',#18170,0.210000000000001);
#6715=CIRCLE('',#18171,0.210000000000001);
#6716=CIRCLE('',#18174,1.005);
#6717=CIRCLE('',#18175,1.005);
#6718=CIRCLE('',#18177,1.4);
#6719=CIRCLE('',#18178,1.4);
#6720=CIRCLE('',#18183,1.005);
#6721=CIRCLE('',#18184,1.005);
#6722=CIRCLE('',#18186,1.3);
#6723=CIRCLE('',#18187,1.3);
#6724=CIRCLE('',#18192,1.005);
#6725=CIRCLE('',#18193,1.005);
#6726=CIRCLE('',#18195,1.3);
#6727=CIRCLE('',#18196,1.3);
#6728=CIRCLE('',#18201,1.005);
#6729=CIRCLE('',#18202,1.005);
#6730=CIRCLE('',#18204,1.3);
#6731=CIRCLE('',#18205,1.3);
#6732=CIRCLE('',#18210,1.005);
#6733=CIRCLE('',#18211,1.005);
#6734=CIRCLE('',#18213,1.3);
#6735=CIRCLE('',#18214,1.3);
#6736=CIRCLE('',#18226,0.22);
#6737=CIRCLE('',#18228,0.24505);
#6738=CIRCLE('',#18230,0.24505);
#6739=CIRCLE('',#18232,0.175);
#6740=CIRCLE('',#18250,3.75);
#6741=CIRCLE('',#18251,3.75);
#6742=CIRCLE('',#18252,3.75);
#6743=CIRCLE('',#18253,3.75);
#6744=CIRCLE('',#18254,3.75);
#6745=CIRCLE('',#18255,3.75);
#6746=CIRCLE('',#18256,3.75);
#6747=CIRCLE('',#18257,3.75);
#6748=CIRCLE('',#18258,3.75);
#6749=CIRCLE('',#18259,3.75);
#6750=CIRCLE('',#18260,3.75);
#6751=CIRCLE('',#18261,3.75);
#6752=CIRCLE('',#18262,3.75);
#6753=CIRCLE('',#18263,3.75);
#6754=CIRCLE('',#18264,3.75);
#6755=CIRCLE('',#18265,3.75);
#6756=CIRCLE('',#18266,3.75);
#6757=CIRCLE('',#18267,3.75);
#6758=CIRCLE('',#18268,3.75);
#6759=CIRCLE('',#18269,3.75);
#6760=CIRCLE('',#18270,3.75);
#6761=CIRCLE('',#18271,3.75);
#6762=CIRCLE('',#18272,3.75);
#6763=CIRCLE('',#18273,3.75);
#6764=CIRCLE('',#18274,3.75);
#6765=CIRCLE('',#18275,3.75);
#6766=CIRCLE('',#18276,3.75);
#6767=CIRCLE('',#18277,3.75);
#6768=CIRCLE('',#18278,3.75);
#6769=CIRCLE('',#18279,3.75);
#6770=CIRCLE('',#18280,3.75);
#6771=CIRCLE('',#18281,3.75);
#6772=CIRCLE('',#18282,3.75);
#6773=CIRCLE('',#18283,3.75);
#6774=CIRCLE('',#18284,3.75);
#6775=CIRCLE('',#18285,3.75);
#6776=CIRCLE('',#18286,3.75);
#6777=CIRCLE('',#18287,3.75);
#6778=CIRCLE('',#18288,3.75);
#6779=CIRCLE('',#18289,3.75);
#6780=CIRCLE('',#18290,1.);
#6781=CIRCLE('',#18292,1.);
#6782=CIRCLE('',#18294,2.);
#6783=CIRCLE('',#18295,2.);
#6784=CIRCLE('',#18299,3.75);
#6785=CIRCLE('',#18302,3.75);
#6786=CIRCLE('',#18305,3.75);
#6787=CIRCLE('',#18308,3.75);
#6788=CIRCLE('',#18311,3.75);
#6789=CIRCLE('',#18314,3.75);
#6790=CIRCLE('',#18317,3.75);
#6791=CIRCLE('',#18320,3.75);
#6792=CIRCLE('',#18323,3.75);
#6793=CIRCLE('',#18326,3.75);
#6794=CIRCLE('',#18329,3.75);
#6795=CIRCLE('',#18332,3.75);
#6796=CIRCLE('',#18335,3.75);
#6797=CIRCLE('',#18338,3.75);
#6798=CIRCLE('',#18341,3.75);
#6799=CIRCLE('',#18344,3.75);
#6800=CIRCLE('',#18347,3.75);
#6801=CIRCLE('',#18350,3.75);
#6802=CIRCLE('',#18353,3.75);
#6803=CIRCLE('',#18356,3.75);
#6804=CIRCLE('',#18359,3.75);
#6805=CIRCLE('',#18362,3.75);
#6806=CIRCLE('',#18365,3.75);
#6807=CIRCLE('',#18368,3.75);
#6808=CIRCLE('',#18371,3.75);
#6809=CIRCLE('',#18374,3.75);
#6810=CIRCLE('',#18377,3.75);
#6811=CIRCLE('',#18380,3.75);
#6812=CIRCLE('',#18383,3.75);
#6813=CIRCLE('',#18386,3.75);
#6814=CIRCLE('',#18389,3.75);
#6815=CIRCLE('',#18392,3.75);
#6816=CIRCLE('',#18395,3.75);
#6817=CIRCLE('',#18398,3.75);
#6818=CIRCLE('',#18401,3.75);
#6819=CIRCLE('',#18404,3.75);
#6820=CIRCLE('',#18407,3.75);
#6821=CIRCLE('',#18410,3.75);
#6822=CIRCLE('',#18413,3.75);
#6823=CIRCLE('',#18416,3.75);
#6824=VERTEX_POINT('',#22778);
#6825=VERTEX_POINT('',#22780);
#6826=VERTEX_POINT('',#22784);
#6827=VERTEX_POINT('',#22786);
#6828=VERTEX_POINT('',#22790);
#6829=VERTEX_POINT('',#22792);
#6830=VERTEX_POINT('',#22796);
#6831=VERTEX_POINT('',#22798);
#6832=VERTEX_POINT('',#22802);
#6833=VERTEX_POINT('',#22803);
#6834=VERTEX_POINT('',#22805);
#6835=VERTEX_POINT('',#22807);
#6836=VERTEX_POINT('',#22811);
#6837=VERTEX_POINT('',#22813);
#6838=VERTEX_POINT('',#22817);
#6839=VERTEX_POINT('',#22819);
#6840=VERTEX_POINT('',#22829);
#6841=VERTEX_POINT('',#22831);
#6842=VERTEX_POINT('',#22836);
#6843=VERTEX_POINT('',#22838);
#6844=VERTEX_POINT('',#22843);
#6845=VERTEX_POINT('',#22845);
#6846=VERTEX_POINT('',#22850);
#6847=VERTEX_POINT('',#22852);
#6848=VERTEX_POINT('',#22857);
#6849=VERTEX_POINT('',#22858);
#6850=VERTEX_POINT('',#22860);
#6851=VERTEX_POINT('',#22862);
#6852=VERTEX_POINT('',#22866);
#6853=VERTEX_POINT('',#22868);
#6854=VERTEX_POINT('',#22872);
#6855=VERTEX_POINT('',#22874);
#6856=VERTEX_POINT('',#22876);
#6857=VERTEX_POINT('',#22878);
#6858=VERTEX_POINT('',#22880);
#6859=VERTEX_POINT('',#22882);
#6860=VERTEX_POINT('',#22884);
#6861=VERTEX_POINT('',#22886);
#6862=VERTEX_POINT('',#22888);
#6863=VERTEX_POINT('',#22890);
#6864=VERTEX_POINT('',#22892);
#6865=VERTEX_POINT('',#22894);
#6866=VERTEX_POINT('',#22897);
#6867=VERTEX_POINT('',#22899);
#6868=VERTEX_POINT('',#22901);
#6869=VERTEX_POINT('',#22903);
#6870=VERTEX_POINT('',#22906);
#6871=VERTEX_POINT('',#22908);
#6872=VERTEX_POINT('',#22910);
#6873=VERTEX_POINT('',#22912);
#6874=VERTEX_POINT('',#22914);
#6875=VERTEX_POINT('',#22916);
#6876=VERTEX_POINT('',#22918);
#6877=VERTEX_POINT('',#22920);
#6878=VERTEX_POINT('',#22923);
#6879=VERTEX_POINT('',#22925);
#6880=VERTEX_POINT('',#22927);
#6881=VERTEX_POINT('',#22929);
#6882=VERTEX_POINT('',#22931);
#6883=VERTEX_POINT('',#22934);
#6884=VERTEX_POINT('',#22936);
#6885=VERTEX_POINT('',#22940);
#6886=VERTEX_POINT('',#22944);
#6887=VERTEX_POINT('',#22946);
#6888=VERTEX_POINT('',#22948);
#6889=VERTEX_POINT('',#22950);
#6890=VERTEX_POINT('',#22952);
#6891=VERTEX_POINT('',#22954);
#6892=VERTEX_POINT('',#22956);
#6893=VERTEX_POINT('',#22958);
#6894=VERTEX_POINT('',#22960);
#6895=VERTEX_POINT('',#22962);
#6896=VERTEX_POINT('',#22964);
#6897=VERTEX_POINT('',#22967);
#6898=VERTEX_POINT('',#22969);
#6899=VERTEX_POINT('',#22971);
#6900=VERTEX_POINT('',#22973);
#6901=VERTEX_POINT('',#22976);
#6902=VERTEX_POINT('',#22978);
#6903=VERTEX_POINT('',#22980);
#6904=VERTEX_POINT('',#22982);
#6905=VERTEX_POINT('',#22988);
#6906=VERTEX_POINT('',#22992);
#6907=VERTEX_POINT('',#22994);
#6908=VERTEX_POINT('',#22996);
#6909=VERTEX_POINT('',#22998);
#6910=VERTEX_POINT('',#23000);
#6911=VERTEX_POINT('',#23002);
#6912=VERTEX_POINT('',#23004);
#6913=VERTEX_POINT('',#23008);
#6914=VERTEX_POINT('',#23010);
#6915=VERTEX_POINT('',#23014);
#6916=VERTEX_POINT('',#23019);
#6917=VERTEX_POINT('',#23024);
#6918=VERTEX_POINT('',#23029);
#6919=VERTEX_POINT('',#23034);
#6920=VERTEX_POINT('',#23038);
#6921=VERTEX_POINT('',#23042);
#6922=VERTEX_POINT('',#23046);
#6923=VERTEX_POINT('',#23050);
#6924=VERTEX_POINT('',#23052);
#6925=VERTEX_POINT('',#23054);
#6926=VERTEX_POINT('',#23056);
#6927=VERTEX_POINT('',#23064);
#6928=VERTEX_POINT('',#23066);
#6929=VERTEX_POINT('',#23068);
#6930=VERTEX_POINT('',#23070);
#6931=VERTEX_POINT('',#23074);
#6932=VERTEX_POINT('',#23076);
#6933=VERTEX_POINT('',#23080);
#6934=VERTEX_POINT('',#23085);
#6935=VERTEX_POINT('',#23090);
#6936=VERTEX_POINT('',#23095);
#6937=VERTEX_POINT('',#23100);
#6938=VERTEX_POINT('',#23104);
#6939=VERTEX_POINT('',#23109);
#6940=VERTEX_POINT('',#23111);
#6941=VERTEX_POINT('',#23116);
#6942=VERTEX_POINT('',#23118);
#6943=VERTEX_POINT('',#23120);
#6944=VERTEX_POINT('',#23122);
#6945=VERTEX_POINT('',#23124);
#6946=VERTEX_POINT('',#23133);
#6947=VERTEX_POINT('',#23135);
#6948=VERTEX_POINT('',#23139);
#6949=VERTEX_POINT('',#23142);
#6950=VERTEX_POINT('',#23144);
#6951=VERTEX_POINT('',#23148);
#6952=VERTEX_POINT('',#23151);
#6953=VERTEX_POINT('',#23153);
#6954=VERTEX_POINT('',#23157);
#6955=VERTEX_POINT('',#23160);
#6956=VERTEX_POINT('',#23162);
#6957=VERTEX_POINT('',#23166);
#6958=VERTEX_POINT('',#23169);
#6959=VERTEX_POINT('',#23173);
#6960=VERTEX_POINT('',#23177);
#6961=VERTEX_POINT('',#23181);
#6962=VERTEX_POINT('',#23185);
#6963=VERTEX_POINT('',#23190);
#6964=VERTEX_POINT('',#23195);
#6965=VERTEX_POINT('',#23200);
#6966=VERTEX_POINT('',#23205);
#6967=VERTEX_POINT('',#23209);
#6968=VERTEX_POINT('',#23213);
#6969=VERTEX_POINT('',#23217);
#6970=VERTEX_POINT('',#23221);
#6971=VERTEX_POINT('',#23225);
#6972=VERTEX_POINT('',#23248);
#6973=VERTEX_POINT('',#23250);
#6974=VERTEX_POINT('',#23254);
#6975=VERTEX_POINT('',#23256);
#6976=VERTEX_POINT('',#23260);
#6977=VERTEX_POINT('',#23262);
#6978=VERTEX_POINT('',#23266);
#6979=VERTEX_POINT('',#23268);
#6980=VERTEX_POINT('',#23272);
#6981=VERTEX_POINT('',#23273);
#6982=VERTEX_POINT('',#23275);
#6983=VERTEX_POINT('',#23277);
#6984=VERTEX_POINT('',#23281);
#6985=VERTEX_POINT('',#23283);
#6986=VERTEX_POINT('',#23287);
#6987=VERTEX_POINT('',#23289);
#6988=VERTEX_POINT('',#23296);
#6989=VERTEX_POINT('',#23298);
#6990=VERTEX_POINT('',#23303);
#6991=VERTEX_POINT('',#23305);
#6992=VERTEX_POINT('',#23310);
#6993=VERTEX_POINT('',#23312);
#6994=VERTEX_POINT('',#23317);
#6995=VERTEX_POINT('',#23319);
#6996=VERTEX_POINT('',#23324);
#6997=VERTEX_POINT('',#23325);
#6998=VERTEX_POINT('',#23327);
#6999=VERTEX_POINT('',#23329);
#7000=VERTEX_POINT('',#23333);
#7001=VERTEX_POINT('',#23335);
#7002=VERTEX_POINT('',#23339);
#7003=VERTEX_POINT('',#23341);
#7004=VERTEX_POINT('',#23345);
#7005=VERTEX_POINT('',#23347);
#7006=VERTEX_POINT('',#23349);
#7007=VERTEX_POINT('',#23351);
#7008=VERTEX_POINT('',#23353);
#7009=VERTEX_POINT('',#23355);
#7010=VERTEX_POINT('',#23357);
#7011=VERTEX_POINT('',#23359);
#7012=VERTEX_POINT('',#23362);
#7013=VERTEX_POINT('',#23364);
#7014=VERTEX_POINT('',#23366);
#7015=VERTEX_POINT('',#23368);
#7016=VERTEX_POINT('',#23370);
#7017=VERTEX_POINT('',#23373);
#7018=VERTEX_POINT('',#23374);
#7019=VERTEX_POINT('',#23379);
#7020=VERTEX_POINT('',#23383);
#7021=VERTEX_POINT('',#23385);
#7022=VERTEX_POINT('',#23387);
#7023=VERTEX_POINT('',#23389);
#7024=VERTEX_POINT('',#23391);
#7025=VERTEX_POINT('',#23393);
#7026=VERTEX_POINT('',#23395);
#7027=VERTEX_POINT('',#23397);
#7028=VERTEX_POINT('',#23399);
#7029=VERTEX_POINT('',#23401);
#7030=VERTEX_POINT('',#23403);
#7031=VERTEX_POINT('',#23406);
#7032=VERTEX_POINT('',#23408);
#7033=VERTEX_POINT('',#23410);
#7034=VERTEX_POINT('',#23412);
#7035=VERTEX_POINT('',#23415);
#7036=VERTEX_POINT('',#23419);
#7037=VERTEX_POINT('',#23421);
#7038=VERTEX_POINT('',#23423);
#7039=VERTEX_POINT('',#23425);
#7040=VERTEX_POINT('',#23427);
#7041=VERTEX_POINT('',#23429);
#7042=VERTEX_POINT('',#23431);
#7043=VERTEX_POINT('',#23433);
#7044=VERTEX_POINT('',#23435);
#7045=VERTEX_POINT('',#23437);
#7046=VERTEX_POINT('',#23439);
#7047=VERTEX_POINT('',#23442);
#7048=VERTEX_POINT('',#23444);
#7049=VERTEX_POINT('',#23446);
#7050=VERTEX_POINT('',#23448);
#7051=VERTEX_POINT('',#23451);
#7052=VERTEX_POINT('',#23453);
#7053=VERTEX_POINT('',#23455);
#7054=VERTEX_POINT('',#23457);
#7055=VERTEX_POINT('',#23459);
#7056=VERTEX_POINT('',#23461);
#7057=VERTEX_POINT('',#23463);
#7058=VERTEX_POINT('',#23467);
#7059=VERTEX_POINT('',#23469);
#7060=VERTEX_POINT('',#23473);
#7061=VERTEX_POINT('',#23475);
#7062=VERTEX_POINT('',#23477);
#7063=VERTEX_POINT('',#23481);
#7064=VERTEX_POINT('',#23486);
#7065=VERTEX_POINT('',#23491);
#7066=VERTEX_POINT('',#23496);
#7067=VERTEX_POINT('',#23501);
#7068=VERTEX_POINT('',#23502);
#7069=VERTEX_POINT('',#23509);
#7070=VERTEX_POINT('',#23513);
#7071=VERTEX_POINT('',#23517);
#7072=VERTEX_POINT('',#23523);
#7073=VERTEX_POINT('',#23525);
#7074=VERTEX_POINT('',#23529);
#7075=VERTEX_POINT('',#23531);
#7076=VERTEX_POINT('',#23533);
#7077=VERTEX_POINT('',#23537);
#7078=VERTEX_POINT('',#23542);
#7079=VERTEX_POINT('',#23547);
#7080=VERTEX_POINT('',#23552);
#7081=VERTEX_POINT('',#23557);
#7082=VERTEX_POINT('',#23561);
#7083=VERTEX_POINT('',#23565);
#7084=VERTEX_POINT('',#23569);
#7085=VERTEX_POINT('',#23575);
#7086=VERTEX_POINT('',#23579);
#7087=VERTEX_POINT('',#23581);
#7088=VERTEX_POINT('',#23583);
#7089=VERTEX_POINT('',#23589);
#7090=VERTEX_POINT('',#23591);
#7091=VERTEX_POINT('',#23593);
#7092=VERTEX_POINT('',#23595);
#7093=VERTEX_POINT('',#23597);
#7094=VERTEX_POINT('',#23600);
#7095=VERTEX_POINT('',#23605);
#7096=VERTEX_POINT('',#23610);
#7097=VERTEX_POINT('',#23615);
#7098=VERTEX_POINT('',#23620);
#7099=VERTEX_POINT('',#23624);
#7100=VERTEX_POINT('',#23628);
#7101=VERTEX_POINT('',#23632);
#7102=VERTEX_POINT('',#23636);
#7103=VERTEX_POINT('',#23640);
#7104=VERTEX_POINT('',#23663);
#7105=VERTEX_POINT('',#23665);
#7106=VERTEX_POINT('',#23672);
#7107=VERTEX_POINT('',#23674);
#7108=VERTEX_POINT('',#23681);
#7109=VERTEX_POINT('',#23683);
#7110=VERTEX_POINT('',#23690);
#7111=VERTEX_POINT('',#23692);
#7112=VERTEX_POINT('',#23699);
#7113=VERTEX_POINT('',#23700);
#7114=VERTEX_POINT('',#23702);
#7115=VERTEX_POINT('',#23704);
#7116=VERTEX_POINT('',#23708);
#7117=VERTEX_POINT('',#23709);
#7118=VERTEX_POINT('',#23711);
#7119=VERTEX_POINT('',#23713);
#7120=VERTEX_POINT('',#23717);
#7121=VERTEX_POINT('',#23718);
#7122=VERTEX_POINT('',#23720);
#7123=VERTEX_POINT('',#23722);
#7124=VERTEX_POINT('',#23726);
#7125=VERTEX_POINT('',#23727);
#7126=VERTEX_POINT('',#23729);
#7127=VERTEX_POINT('',#23731);
#7128=VERTEX_POINT('',#23739);
#7129=VERTEX_POINT('',#23750);
#7130=VERTEX_POINT('',#23752);
#7131=VERTEX_POINT('',#23756);
#7132=VERTEX_POINT('',#23763);
#7133=VERTEX_POINT('',#23764);
#7134=VERTEX_POINT('',#23766);
#7135=VERTEX_POINT('',#23768);
#7136=VERTEX_POINT('',#23772);
#7137=VERTEX_POINT('',#23773);
#7138=VERTEX_POINT('',#23775);
#7139=VERTEX_POINT('',#23777);
#7140=VERTEX_POINT('',#23781);
#7141=VERTEX_POINT('',#23782);
#7142=VERTEX_POINT('',#23784);
#7143=VERTEX_POINT('',#23786);
#7144=VERTEX_POINT('',#23790);
#7145=VERTEX_POINT('',#23791);
#7146=VERTEX_POINT('',#23793);
#7147=VERTEX_POINT('',#23795);
#7148=VERTEX_POINT('',#23803);
#7149=VERTEX_POINT('',#23814);
#7150=VERTEX_POINT('',#23818);
#7151=VERTEX_POINT('',#23821);
#7152=VERTEX_POINT('',#23827);
#7153=VERTEX_POINT('',#23829);
#7154=VERTEX_POINT('',#23833);
#7155=VERTEX_POINT('',#23835);
#7156=VERTEX_POINT('',#23839);
#7157=VERTEX_POINT('',#23841);
#7158=VERTEX_POINT('',#23845);
#7159=VERTEX_POINT('',#23847);
#7160=VERTEX_POINT('',#23851);
#7161=VERTEX_POINT('',#23853);
#7162=VERTEX_POINT('',#23857);
#7163=VERTEX_POINT('',#23860);
#7164=VERTEX_POINT('',#23864);
#7165=VERTEX_POINT('',#23866);
#7166=VERTEX_POINT('',#23873);
#7167=VERTEX_POINT('',#23875);
#7168=VERTEX_POINT('',#23879);
#7169=VERTEX_POINT('',#23881);
#7170=VERTEX_POINT('',#23885);
#7171=VERTEX_POINT('',#23887);
#7172=VERTEX_POINT('',#23891);
#7173=VERTEX_POINT('',#23893);
#7174=VERTEX_POINT('',#23897);
#7175=VERTEX_POINT('',#23899);
#7176=VERTEX_POINT('',#23903);
#7177=VERTEX_POINT('',#23906);
#7178=VERTEX_POINT('',#23910);
#7179=VERTEX_POINT('',#23912);
#7180=VERTEX_POINT('',#23919);
#7181=VERTEX_POINT('',#23921);
#7182=VERTEX_POINT('',#23925);
#7183=VERTEX_POINT('',#23927);
#7184=VERTEX_POINT('',#23931);
#7185=VERTEX_POINT('',#23933);
#7186=VERTEX_POINT('',#23937);
#7187=VERTEX_POINT('',#23939);
#7188=VERTEX_POINT('',#23943);
#7189=VERTEX_POINT('',#23945);
#7190=VERTEX_POINT('',#23949);
#7191=VERTEX_POINT('',#23952);
#7192=VERTEX_POINT('',#23956);
#7193=VERTEX_POINT('',#23958);
#7194=VERTEX_POINT('',#23965);
#7195=VERTEX_POINT('',#23967);
#7196=VERTEX_POINT('',#23971);
#7197=VERTEX_POINT('',#23973);
#7198=VERTEX_POINT('',#23977);
#7199=VERTEX_POINT('',#23979);
#7200=VERTEX_POINT('',#23983);
#7201=VERTEX_POINT('',#23985);
#7202=VERTEX_POINT('',#23989);
#7203=VERTEX_POINT('',#23991);
#7204=VERTEX_POINT('',#23995);
#7205=VERTEX_POINT('',#23998);
#7206=VERTEX_POINT('',#24002);
#7207=VERTEX_POINT('',#24004);
#7208=VERTEX_POINT('',#24011);
#7209=VERTEX_POINT('',#24013);
#7210=VERTEX_POINT('',#24017);
#7211=VERTEX_POINT('',#24019);
#7212=VERTEX_POINT('',#24023);
#7213=VERTEX_POINT('',#24025);
#7214=VERTEX_POINT('',#24029);
#7215=VERTEX_POINT('',#24031);
#7216=VERTEX_POINT('',#24035);
#7217=VERTEX_POINT('',#24036);
#7218=VERTEX_POINT('',#24038);
#7219=VERTEX_POINT('',#24040);
#7220=VERTEX_POINT('',#24044);
#7221=VERTEX_POINT('',#24046);
#7222=VERTEX_POINT('',#24050);
#7223=VERTEX_POINT('',#24052);
#7224=VERTEX_POINT('',#24062);
#7225=VERTEX_POINT('',#24063);
#7226=VERTEX_POINT('',#24065);
#7227=VERTEX_POINT('',#24067);
#7228=VERTEX_POINT('',#24071);
#7229=VERTEX_POINT('',#24073);
#7230=VERTEX_POINT('',#24077);
#7231=VERTEX_POINT('',#24079);
#7232=VERTEX_POINT('',#24089);
#7233=VERTEX_POINT('',#24090);
#7234=VERTEX_POINT('',#24092);
#7235=VERTEX_POINT('',#24094);
#7236=VERTEX_POINT('',#24098);
#7237=VERTEX_POINT('',#24100);
#7238=VERTEX_POINT('',#24104);
#7239=VERTEX_POINT('',#24106);
#7240=VERTEX_POINT('',#24116);
#7241=VERTEX_POINT('',#24117);
#7242=VERTEX_POINT('',#24119);
#7243=VERTEX_POINT('',#24121);
#7244=VERTEX_POINT('',#24125);
#7245=VERTEX_POINT('',#24127);
#7246=VERTEX_POINT('',#24131);
#7247=VERTEX_POINT('',#24133);
#7248=VERTEX_POINT('',#24137);
#7249=VERTEX_POINT('',#24139);
#7250=VERTEX_POINT('',#24143);
#7251=VERTEX_POINT('',#24145);
#7252=VERTEX_POINT('',#24154);
#7253=VERTEX_POINT('',#24157);
#7254=VERTEX_POINT('',#24160);
#7255=VERTEX_POINT('',#24164);
#7256=VERTEX_POINT('',#24168);
#7257=VERTEX_POINT('',#24172);
#7258=VERTEX_POINT('',#24175);
#7259=VERTEX_POINT('',#24183);
#7260=VERTEX_POINT('',#24184);
#7261=VERTEX_POINT('',#24187);
#7262=VERTEX_POINT('',#24189);
#7263=VERTEX_POINT('',#24193);
#7264=VERTEX_POINT('',#24197);
#7265=VERTEX_POINT('',#24199);
#7266=VERTEX_POINT('',#24203);
#7267=VERTEX_POINT('',#24208);
#7268=VERTEX_POINT('',#24212);
#7269=VERTEX_POINT('',#24218);
#7270=VERTEX_POINT('',#24219);
#7271=VERTEX_POINT('',#24222);
#7272=VERTEX_POINT('',#24224);
#7273=VERTEX_POINT('',#24228);
#7274=VERTEX_POINT('',#24232);
#7275=VERTEX_POINT('',#24234);
#7276=VERTEX_POINT('',#24237);
#7277=VERTEX_POINT('',#24241);
#7278=VERTEX_POINT('',#24245);
#7279=VERTEX_POINT('',#24253);
#7280=VERTEX_POINT('',#24254);
#7281=VERTEX_POINT('',#24257);
#7282=VERTEX_POINT('',#24258);
#7283=VERTEX_POINT('',#24261);
#7284=VERTEX_POINT('',#24262);
#7285=VERTEX_POINT('',#24265);
#7286=VERTEX_POINT('',#24266);
#7287=VERTEX_POINT('',#24269);
#7288=VERTEX_POINT('',#24270);
#7289=VERTEX_POINT('',#24273);
#7290=VERTEX_POINT('',#24274);
#7291=VERTEX_POINT('',#24277);
#7292=VERTEX_POINT('',#24278);
#7293=VERTEX_POINT('',#24282);
#7294=VERTEX_POINT('',#24283);
#7295=VERTEX_POINT('',#24306);
#7296=VERTEX_POINT('',#24308);
#7297=VERTEX_POINT('',#24333);
#7298=VERTEX_POINT('',#24335);
#7299=VERTEX_POINT('',#24358);
#7300=VERTEX_POINT('',#24360);
#7301=VERTEX_POINT('',#24383);
#7302=VERTEX_POINT('',#24385);
#7303=VERTEX_POINT('',#24388);
#7304=VERTEX_POINT('',#24390);
#7305=VERTEX_POINT('',#24413);
#7306=VERTEX_POINT('',#24415);
#7307=VERTEX_POINT('',#24438);
#7308=VERTEX_POINT('',#24440);
#7309=VERTEX_POINT('',#24463);
#7310=VERTEX_POINT('',#24465);
#7311=VERTEX_POINT('',#24490);
#7312=VERTEX_POINT('',#24494);
#7313=VERTEX_POINT('',#24519);
#7314=VERTEX_POINT('',#24523);
#7315=VERTEX_POINT('',#24548);
#7316=VERTEX_POINT('',#24550);
#7317=VERTEX_POINT('',#24554);
#7318=VERTEX_POINT('',#24579);
#7319=VERTEX_POINT('',#24583);
#7320=VERTEX_POINT('',#24608);
#7321=VERTEX_POINT('',#24612);
#7322=VERTEX_POINT('',#24637);
#7323=VERTEX_POINT('',#24640);
#7324=VERTEX_POINT('',#24642);
#7325=VERTEX_POINT('',#24674);
#7326=VERTEX_POINT('',#24676);
#7327=VERTEX_POINT('',#24679);
#7328=VERTEX_POINT('',#24683);
#7329=VERTEX_POINT('',#24688);
#7330=VERTEX_POINT('',#24690);
#7331=VERTEX_POINT('',#24693);
#7332=VERTEX_POINT('',#24697);
#7333=VERTEX_POINT('',#24709);
#7334=VERTEX_POINT('',#24710);
#7335=VERTEX_POINT('',#24713);
#7336=VERTEX_POINT('',#24715);
#7337=VERTEX_POINT('',#24719);
#7338=VERTEX_POINT('',#24723);
#7339=VERTEX_POINT('',#24725);
#7340=VERTEX_POINT('',#24729);
#7341=VERTEX_POINT('',#24734);
#7342=VERTEX_POINT('',#24738);
#7343=VERTEX_POINT('',#24744);
#7344=VERTEX_POINT('',#24745);
#7345=VERTEX_POINT('',#24748);
#7346=VERTEX_POINT('',#24750);
#7347=VERTEX_POINT('',#24754);
#7348=VERTEX_POINT('',#24758);
#7349=VERTEX_POINT('',#24760);
#7350=VERTEX_POINT('',#24763);
#7351=VERTEX_POINT('',#24767);
#7352=VERTEX_POINT('',#24771);
#7353=VERTEX_POINT('',#24779);
#7354=VERTEX_POINT('',#24780);
#7355=VERTEX_POINT('',#24783);
#7356=VERTEX_POINT('',#24784);
#7357=VERTEX_POINT('',#24787);
#7358=VERTEX_POINT('',#24788);
#7359=VERTEX_POINT('',#24791);
#7360=VERTEX_POINT('',#24792);
#7361=VERTEX_POINT('',#24795);
#7362=VERTEX_POINT('',#24796);
#7363=VERTEX_POINT('',#24799);
#7364=VERTEX_POINT('',#24800);
#7365=VERTEX_POINT('',#24803);
#7366=VERTEX_POINT('',#24804);
#7367=VERTEX_POINT('',#24807);
#7368=VERTEX_POINT('',#24808);
#7369=VERTEX_POINT('',#24812);
#7370=VERTEX_POINT('',#24813);
#7371=VERTEX_POINT('',#24836);
#7372=VERTEX_POINT('',#24838);
#7373=VERTEX_POINT('',#24863);
#7374=VERTEX_POINT('',#24865);
#7375=VERTEX_POINT('',#24888);
#7376=VERTEX_POINT('',#24890);
#7377=VERTEX_POINT('',#24913);
#7378=VERTEX_POINT('',#24915);
#7379=VERTEX_POINT('',#24928);
#7380=VERTEX_POINT('',#24931);
#7381=VERTEX_POINT('',#24944);
#7382=VERTEX_POINT('',#24946);
#7383=VERTEX_POINT('',#24969);
#7384=VERTEX_POINT('',#24971);
#7385=VERTEX_POINT('',#24994);
#7386=VERTEX_POINT('',#24996);
#7387=VERTEX_POINT('',#25019);
#7388=VERTEX_POINT('',#25021);
#7389=VERTEX_POINT('',#25046);
#7390=VERTEX_POINT('',#25050);
#7391=VERTEX_POINT('',#25075);
#7392=VERTEX_POINT('',#25079);
#7393=VERTEX_POINT('',#25104);
#7394=VERTEX_POINT('',#25108);
#7395=VERTEX_POINT('',#25109);
#7396=VERTEX_POINT('',#25136);
#7397=VERTEX_POINT('',#25140);
#7398=VERTEX_POINT('',#25165);
#7399=VERTEX_POINT('',#25169);
#7400=VERTEX_POINT('',#25194);
#7401=VERTEX_POINT('',#25198);
#7402=VERTEX_POINT('',#25223);
#7403=VERTEX_POINT('',#25226);
#7404=VERTEX_POINT('',#25228);
#7405=VERTEX_POINT('',#25260);
#7406=VERTEX_POINT('',#25262);
#7407=VERTEX_POINT('',#25265);
#7408=VERTEX_POINT('',#25269);
#7409=VERTEX_POINT('',#25274);
#7410=VERTEX_POINT('',#25276);
#7411=VERTEX_POINT('',#25279);
#7412=VERTEX_POINT('',#25283);
#7413=VERTEX_POINT('',#25294);
#7414=VERTEX_POINT('',#25297);
#7415=VERTEX_POINT('',#25301);
#7416=VERTEX_POINT('',#25305);
#7417=VERTEX_POINT('',#25309);
#7418=VERTEX_POINT('',#25312);
#7419=VERTEX_POINT('',#25316);
#7420=VERTEX_POINT('',#25320);
#7421=VERTEX_POINT('',#25325);
#7422=VERTEX_POINT('',#25326);
#7423=VERTEX_POINT('',#25328);
#7424=VERTEX_POINT('',#25330);
#7425=VERTEX_POINT('',#25334);
#7426=VERTEX_POINT('',#25336);
#7427=VERTEX_POINT('',#25340);
#7428=VERTEX_POINT('',#25342);
#7429=VERTEX_POINT('',#25346);
#7430=VERTEX_POINT('',#25348);
#7431=VERTEX_POINT('',#25352);
#7432=VERTEX_POINT('',#25354);
#7433=VERTEX_POINT('',#25425);
#7434=VERTEX_POINT('',#25426);
#7435=VERTEX_POINT('',#25428);
#7436=VERTEX_POINT('',#25430);
#7437=VERTEX_POINT('',#25434);
#7438=VERTEX_POINT('',#25436);
#7439=VERTEX_POINT('',#25440);
#7440=VERTEX_POINT('',#25442);
#7441=VERTEX_POINT('',#25450);
#7442=VERTEX_POINT('',#25452);
#7443=VERTEX_POINT('',#25459);
#7444=VERTEX_POINT('',#25460);
#7445=VERTEX_POINT('',#25464);
#7446=VERTEX_POINT('',#25475);
#7447=VERTEX_POINT('',#25477);
#7448=VERTEX_POINT('',#25479);
#7449=VERTEX_POINT('',#25516);
#7450=VERTEX_POINT('',#25531);
#7451=VERTEX_POINT('',#25533);
#7452=VERTEX_POINT('',#25537);
#7453=VERTEX_POINT('',#25539);
#7454=VERTEX_POINT('',#25546);
#7455=VERTEX_POINT('',#25547);
#7456=VERTEX_POINT('',#25551);
#7457=VERTEX_POINT('',#25562);
#7458=VERTEX_POINT('',#25564);
#7459=VERTEX_POINT('',#25566);
#7460=VERTEX_POINT('',#25603);
#7461=VERTEX_POINT('',#25618);
#7462=VERTEX_POINT('',#25620);
#7463=VERTEX_POINT('',#25624);
#7464=VERTEX_POINT('',#25626);
#7465=VERTEX_POINT('',#25633);
#7466=VERTEX_POINT('',#25635);
#7467=VERTEX_POINT('',#25639);
#7468=VERTEX_POINT('',#25641);
#7469=VERTEX_POINT('',#25648);
#7470=VERTEX_POINT('',#25650);
#7471=VERTEX_POINT('',#25654);
#7472=VERTEX_POINT('',#25656);
#7473=VERTEX_POINT('',#25663);
#7474=VERTEX_POINT('',#25665);
#7475=VERTEX_POINT('',#25669);
#7476=VERTEX_POINT('',#25671);
#7477=VERTEX_POINT('',#25678);
#7478=VERTEX_POINT('',#25680);
#7479=VERTEX_POINT('',#25684);
#7480=VERTEX_POINT('',#25686);
#7481=VERTEX_POINT('',#25693);
#7482=VERTEX_POINT('',#25694);
#7483=VERTEX_POINT('',#25696);
#7484=VERTEX_POINT('',#25698);
#7485=VERTEX_POINT('',#25702);
#7486=VERTEX_POINT('',#25704);
#7487=VERTEX_POINT('',#25708);
#7488=VERTEX_POINT('',#25710);
#7489=VERTEX_POINT('',#25714);
#7490=VERTEX_POINT('',#25715);
#7491=VERTEX_POINT('',#25717);
#7492=VERTEX_POINT('',#25788);
#7493=VERTEX_POINT('',#25790);
#7494=VERTEX_POINT('',#25861);
#7495=VERTEX_POINT('',#25863);
#7496=VERTEX_POINT('',#25934);
#7497=VERTEX_POINT('',#25936);
#7498=VERTEX_POINT('',#26007);
#7499=VERTEX_POINT('',#26009);
#7500=VERTEX_POINT('',#26080);
#7501=VERTEX_POINT('',#26082);
#7502=VERTEX_POINT('',#26153);
#7503=VERTEX_POINT('',#26155);
#7504=VERTEX_POINT('',#26226);
#7505=VERTEX_POINT('',#26228);
#7506=VERTEX_POINT('',#26299);
#7507=VERTEX_POINT('',#26301);
#7508=VERTEX_POINT('',#26372);
#7509=VERTEX_POINT('',#26374);
#7510=VERTEX_POINT('',#26445);
#7511=VERTEX_POINT('',#26447);
#7512=VERTEX_POINT('',#26518);
#7513=VERTEX_POINT('',#26520);
#7514=VERTEX_POINT('',#26591);
#7515=VERTEX_POINT('',#26593);
#7516=VERTEX_POINT('',#26664);
#7517=VERTEX_POINT('',#26666);
#7518=VERTEX_POINT('',#26737);
#7519=VERTEX_POINT('',#26739);
#7520=VERTEX_POINT('',#26810);
#7521=VERTEX_POINT('',#26812);
#7522=VERTEX_POINT('',#26883);
#7523=VERTEX_POINT('',#26885);
#7524=VERTEX_POINT('',#26956);
#7525=VERTEX_POINT('',#26958);
#7526=VERTEX_POINT('',#27029);
#7527=VERTEX_POINT('',#27031);
#7528=VERTEX_POINT('',#27102);
#7529=VERTEX_POINT('',#27104);
#7530=VERTEX_POINT('',#27175);
#7531=VERTEX_POINT('',#27177);
#7532=VERTEX_POINT('',#27248);
#7533=VERTEX_POINT('',#27250);
#7534=VERTEX_POINT('',#27321);
#7535=VERTEX_POINT('',#27323);
#7536=VERTEX_POINT('',#27394);
#7537=VERTEX_POINT('',#27396);
#7538=VERTEX_POINT('',#27467);
#7539=VERTEX_POINT('',#27469);
#7540=VERTEX_POINT('',#27540);
#7541=VERTEX_POINT('',#27542);
#7542=VERTEX_POINT('',#27613);
#7543=VERTEX_POINT('',#27615);
#7544=VERTEX_POINT('',#27686);
#7545=VERTEX_POINT('',#27688);
#7546=VERTEX_POINT('',#27759);
#7547=VERTEX_POINT('',#27761);
#7548=VERTEX_POINT('',#27832);
#7549=VERTEX_POINT('',#27834);
#7550=VERTEX_POINT('',#27905);
#7551=VERTEX_POINT('',#27907);
#7552=VERTEX_POINT('',#27978);
#7553=VERTEX_POINT('',#27980);
#7554=VERTEX_POINT('',#28051);
#7555=VERTEX_POINT('',#28053);
#7556=VERTEX_POINT('',#28124);
#7557=VERTEX_POINT('',#28126);
#7558=VERTEX_POINT('',#28197);
#7559=VERTEX_POINT('',#28199);
#7560=VERTEX_POINT('',#28270);
#7561=VERTEX_POINT('',#28272);
#7562=VERTEX_POINT('',#28343);
#7563=VERTEX_POINT('',#28345);
#7564=VERTEX_POINT('',#28416);
#7565=VERTEX_POINT('',#28418);
#7566=VERTEX_POINT('',#28489);
#7567=VERTEX_POINT('',#28491);
#7568=VERTEX_POINT('',#28562);
#7569=VERTEX_POINT('',#28638);
#7570=VERTEX_POINT('',#28640);
#7571=VERTEX_POINT('',#28784);
#7572=VERTEX_POINT('',#28786);
#7573=VERTEX_POINT('',#28859);
#7574=VERTEX_POINT('',#29002);
#7575=VERTEX_POINT('',#29075);
#7576=VERTEX_POINT('',#29218);
#7577=VERTEX_POINT('',#29291);
#7578=VERTEX_POINT('',#29434);
#7579=VERTEX_POINT('',#29507);
#7580=VERTEX_POINT('',#29650);
#7581=VERTEX_POINT('',#29723);
#7582=VERTEX_POINT('',#29866);
#7583=VERTEX_POINT('',#29939);
#7584=VERTEX_POINT('',#30082);
#7585=VERTEX_POINT('',#30155);
#7586=VERTEX_POINT('',#30298);
#7587=VERTEX_POINT('',#30371);
#7588=VERTEX_POINT('',#30514);
#7589=VERTEX_POINT('',#30587);
#7590=VERTEX_POINT('',#30730);
#7591=VERTEX_POINT('',#30803);
#7592=VERTEX_POINT('',#30946);
#7593=VERTEX_POINT('',#31019);
#7594=VERTEX_POINT('',#31162);
#7595=VERTEX_POINT('',#31235);
#7596=VERTEX_POINT('',#31378);
#7597=VERTEX_POINT('',#31451);
#7598=VERTEX_POINT('',#31594);
#7599=VERTEX_POINT('',#31667);
#7600=VERTEX_POINT('',#31810);
#7601=VERTEX_POINT('',#31883);
#7602=VERTEX_POINT('',#32026);
#7603=VERTEX_POINT('',#32099);
#7604=VERTEX_POINT('',#32242);
#7605=VERTEX_POINT('',#32315);
#7606=VERTEX_POINT('',#32458);
#7607=VERTEX_POINT('',#32531);
#7608=VERTEX_POINT('',#32674);
#7609=VERTEX_POINT('',#32747);
#7610=VERTEX_POINT('',#32890);
#7611=VERTEX_POINT('',#32963);
#7612=VERTEX_POINT('',#33106);
#7613=VERTEX_POINT('',#33179);
#7614=VERTEX_POINT('',#33322);
#7615=VERTEX_POINT('',#33395);
#7616=VERTEX_POINT('',#33538);
#7617=VERTEX_POINT('',#33611);
#7618=VERTEX_POINT('',#33754);
#7619=VERTEX_POINT('',#33827);
#7620=VERTEX_POINT('',#33970);
#7621=VERTEX_POINT('',#34043);
#7622=VERTEX_POINT('',#34186);
#7623=VERTEX_POINT('',#34259);
#7624=VERTEX_POINT('',#34402);
#7625=VERTEX_POINT('',#34475);
#7626=VERTEX_POINT('',#34618);
#7627=VERTEX_POINT('',#34691);
#7628=VERTEX_POINT('',#34834);
#7629=VERTEX_POINT('',#34907);
#7630=VERTEX_POINT('',#35050);
#7631=VERTEX_POINT('',#35123);
#7632=VERTEX_POINT('',#35266);
#7633=VERTEX_POINT('',#35339);
#7634=VERTEX_POINT('',#35482);
#7635=VERTEX_POINT('',#35555);
#7636=VERTEX_POINT('',#35698);
#7637=VERTEX_POINT('',#35771);
#7638=VERTEX_POINT('',#35914);
#7639=VERTEX_POINT('',#35987);
#7640=VERTEX_POINT('',#36130);
#7641=VERTEX_POINT('',#36203);
#7642=VERTEX_POINT('',#36346);
#7643=VERTEX_POINT('',#36419);
#7644=VERTEX_POINT('',#36562);
#7645=VERTEX_POINT('',#36635);
#7646=VERTEX_POINT('',#36778);
#7647=VERTEX_POINT('',#36851);
#7648=VERTEX_POINT('',#36994);
#7649=VERTEX_POINT('',#37067);
#7650=VERTEX_POINT('',#37210);
#7651=VERTEX_POINT('',#37287);
#7652=VERTEX_POINT('',#37288);
#7653=VERTEX_POINT('',#37290);
#7654=VERTEX_POINT('',#37292);
#7655=VERTEX_POINT('',#37294);
#7656=VERTEX_POINT('',#37296);
#7657=VERTEX_POINT('',#37298);
#7658=VERTEX_POINT('',#37300);
#7659=VERTEX_POINT('',#37304);
#7660=VERTEX_POINT('',#37306);
#7661=VERTEX_POINT('',#37310);
#7662=VERTEX_POINT('',#37314);
#7663=VERTEX_POINT('',#37318);
#7664=VERTEX_POINT('',#37322);
#7665=VERTEX_POINT('',#37324);
#7666=VERTEX_POINT('',#37326);
#7667=VERTEX_POINT('',#37339);
#7668=VERTEX_POINT('',#37340);
#7669=VERTEX_POINT('',#37342);
#7670=VERTEX_POINT('',#37344);
#7671=VERTEX_POINT('',#37348);
#7672=VERTEX_POINT('',#37350);
#7673=VERTEX_POINT('',#37354);
#7674=VERTEX_POINT('',#37356);
#7675=VERTEX_POINT('',#37364);
#7676=VERTEX_POINT('',#37365);
#7677=VERTEX_POINT('',#37367);
#7678=VERTEX_POINT('',#37369);
#7679=VERTEX_POINT('',#37373);
#7680=VERTEX_POINT('',#37375);
#7681=VERTEX_POINT('',#37379);
#7682=VERTEX_POINT('',#37381);
#7683=VERTEX_POINT('',#37389);
#7684=VERTEX_POINT('',#37391);
#7685=VERTEX_POINT('',#37398);
#7686=VERTEX_POINT('',#37399);
#7687=VERTEX_POINT('',#37403);
#7688=VERTEX_POINT('',#37418);
#7689=VERTEX_POINT('',#37420);
#7690=VERTEX_POINT('',#37422);
#7691=VERTEX_POINT('',#37459);
#7692=VERTEX_POINT('',#37478);
#7693=VERTEX_POINT('',#37480);
#7694=VERTEX_POINT('',#37484);
#7695=VERTEX_POINT('',#37486);
#7696=VERTEX_POINT('',#37493);
#7697=VERTEX_POINT('',#37494);
#7698=VERTEX_POINT('',#37498);
#7699=VERTEX_POINT('',#37513);
#7700=VERTEX_POINT('',#37515);
#7701=VERTEX_POINT('',#37517);
#7702=VERTEX_POINT('',#37554);
#7703=VERTEX_POINT('',#37573);
#7704=VERTEX_POINT('',#37575);
#7705=VERTEX_POINT('',#37579);
#7706=VERTEX_POINT('',#37581);
#7707=VERTEX_POINT('',#37588);
#7708=VERTEX_POINT('',#37590);
#7709=VERTEX_POINT('',#37594);
#7710=VERTEX_POINT('',#37596);
#7711=VERTEX_POINT('',#37603);
#7712=VERTEX_POINT('',#37605);
#7713=VERTEX_POINT('',#37609);
#7714=VERTEX_POINT('',#37611);
#7715=VERTEX_POINT('',#37618);
#7716=VERTEX_POINT('',#37620);
#7717=VERTEX_POINT('',#37624);
#7718=VERTEX_POINT('',#37626);
#7719=VERTEX_POINT('',#37633);
#7720=VERTEX_POINT('',#37635);
#7721=VERTEX_POINT('',#37639);
#7722=VERTEX_POINT('',#37641);
#7723=VERTEX_POINT('',#37648);
#7724=VERTEX_POINT('',#37650);
#7725=VERTEX_POINT('',#37654);
#7726=VERTEX_POINT('',#37656);
#7727=VERTEX_POINT('',#37663);
#7728=VERTEX_POINT('',#37664);
#7729=VERTEX_POINT('',#37666);
#7730=VERTEX_POINT('',#37668);
#7731=VERTEX_POINT('',#37672);
#7732=VERTEX_POINT('',#37674);
#7733=VERTEX_POINT('',#37678);
#7734=VERTEX_POINT('',#37680);
#7735=VERTEX_POINT('',#37684);
#7736=VERTEX_POINT('',#37690);
#7737=VERTEX_POINT('',#37691);
#7738=VERTEX_POINT('',#37693);
#7739=VERTEX_POINT('',#37764);
#7740=VERTEX_POINT('',#37766);
#7741=VERTEX_POINT('',#37837);
#7742=VERTEX_POINT('',#37839);
#7743=VERTEX_POINT('',#37910);
#7744=VERTEX_POINT('',#37912);
#7745=VERTEX_POINT('',#37983);
#7746=VERTEX_POINT('',#37985);
#7747=VERTEX_POINT('',#38056);
#7748=VERTEX_POINT('',#38058);
#7749=VERTEX_POINT('',#38129);
#7750=VERTEX_POINT('',#38131);
#7751=VERTEX_POINT('',#38202);
#7752=VERTEX_POINT('',#38204);
#7753=VERTEX_POINT('',#38275);
#7754=VERTEX_POINT('',#38277);
#7755=VERTEX_POINT('',#38348);
#7756=VERTEX_POINT('',#38350);
#7757=VERTEX_POINT('',#38421);
#7758=VERTEX_POINT('',#38423);
#7759=VERTEX_POINT('',#38494);
#7760=VERTEX_POINT('',#38496);
#7761=VERTEX_POINT('',#38567);
#7762=VERTEX_POINT('',#38569);
#7763=VERTEX_POINT('',#38640);
#7764=VERTEX_POINT('',#38642);
#7765=VERTEX_POINT('',#38713);
#7766=VERTEX_POINT('',#38715);
#7767=VERTEX_POINT('',#38786);
#7768=VERTEX_POINT('',#38788);
#7769=VERTEX_POINT('',#38859);
#7770=VERTEX_POINT('',#38861);
#7771=VERTEX_POINT('',#38932);
#7772=VERTEX_POINT('',#38934);
#7773=VERTEX_POINT('',#39005);
#7774=VERTEX_POINT('',#39007);
#7775=VERTEX_POINT('',#39078);
#7776=VERTEX_POINT('',#39080);
#7777=VERTEX_POINT('',#39151);
#7778=VERTEX_POINT('',#39153);
#7779=VERTEX_POINT('',#39224);
#7780=VERTEX_POINT('',#39226);
#7781=VERTEX_POINT('',#39297);
#7782=VERTEX_POINT('',#39299);
#7783=VERTEX_POINT('',#39370);
#7784=VERTEX_POINT('',#39372);
#7785=VERTEX_POINT('',#39443);
#7786=VERTEX_POINT('',#39445);
#7787=VERTEX_POINT('',#39516);
#7788=VERTEX_POINT('',#39518);
#7789=VERTEX_POINT('',#39589);
#7790=VERTEX_POINT('',#39591);
#7791=VERTEX_POINT('',#39662);
#7792=VERTEX_POINT('',#39664);
#7793=VERTEX_POINT('',#39735);
#7794=VERTEX_POINT('',#39737);
#7795=VERTEX_POINT('',#39808);
#7796=VERTEX_POINT('',#39810);
#7797=VERTEX_POINT('',#39881);
#7798=VERTEX_POINT('',#39883);
#7799=VERTEX_POINT('',#39954);
#7800=VERTEX_POINT('',#39956);
#7801=VERTEX_POINT('',#40027);
#7802=VERTEX_POINT('',#40029);
#7803=VERTEX_POINT('',#40100);
#7804=VERTEX_POINT('',#40102);
#7805=VERTEX_POINT('',#40173);
#7806=VERTEX_POINT('',#40175);
#7807=VERTEX_POINT('',#40246);
#7808=VERTEX_POINT('',#40248);
#7809=VERTEX_POINT('',#40319);
#7810=VERTEX_POINT('',#40321);
#7811=VERTEX_POINT('',#40392);
#7812=VERTEX_POINT('',#40394);
#7813=VERTEX_POINT('',#40465);
#7814=VERTEX_POINT('',#40467);
#7815=VERTEX_POINT('',#40538);
#7816=VERTEX_POINT('',#40611);
#7817=VERTEX_POINT('',#40754);
#7818=VERTEX_POINT('',#40756);
#7819=VERTEX_POINT('',#40829);
#7820=VERTEX_POINT('',#40972);
#7821=VERTEX_POINT('',#41045);
#7822=VERTEX_POINT('',#41188);
#7823=VERTEX_POINT('',#41261);
#7824=VERTEX_POINT('',#41404);
#7825=VERTEX_POINT('',#41477);
#7826=VERTEX_POINT('',#41620);
#7827=VERTEX_POINT('',#41693);
#7828=VERTEX_POINT('',#41836);
#7829=VERTEX_POINT('',#41909);
#7830=VERTEX_POINT('',#42052);
#7831=VERTEX_POINT('',#42125);
#7832=VERTEX_POINT('',#42268);
#7833=VERTEX_POINT('',#42341);
#7834=VERTEX_POINT('',#42484);
#7835=VERTEX_POINT('',#42557);
#7836=VERTEX_POINT('',#42700);
#7837=VERTEX_POINT('',#42773);
#7838=VERTEX_POINT('',#42916);
#7839=VERTEX_POINT('',#42989);
#7840=VERTEX_POINT('',#43132);
#7841=VERTEX_POINT('',#43205);
#7842=VERTEX_POINT('',#43348);
#7843=VERTEX_POINT('',#43421);
#7844=VERTEX_POINT('',#43564);
#7845=VERTEX_POINT('',#43637);
#7846=VERTEX_POINT('',#43780);
#7847=VERTEX_POINT('',#43853);
#7848=VERTEX_POINT('',#43996);
#7849=VERTEX_POINT('',#44069);
#7850=VERTEX_POINT('',#44212);
#7851=VERTEX_POINT('',#44285);
#7852=VERTEX_POINT('',#44428);
#7853=VERTEX_POINT('',#44501);
#7854=VERTEX_POINT('',#44644);
#7855=VERTEX_POINT('',#44717);
#7856=VERTEX_POINT('',#44860);
#7857=VERTEX_POINT('',#44933);
#7858=VERTEX_POINT('',#45076);
#7859=VERTEX_POINT('',#45149);
#7860=VERTEX_POINT('',#45292);
#7861=VERTEX_POINT('',#45365);
#7862=VERTEX_POINT('',#45508);
#7863=VERTEX_POINT('',#45581);
#7864=VERTEX_POINT('',#45724);
#7865=VERTEX_POINT('',#45797);
#7866=VERTEX_POINT('',#45940);
#7867=VERTEX_POINT('',#46013);
#7868=VERTEX_POINT('',#46156);
#7869=VERTEX_POINT('',#46229);
#7870=VERTEX_POINT('',#46372);
#7871=VERTEX_POINT('',#46445);
#7872=VERTEX_POINT('',#46588);
#7873=VERTEX_POINT('',#46661);
#7874=VERTEX_POINT('',#46804);
#7875=VERTEX_POINT('',#46877);
#7876=VERTEX_POINT('',#47020);
#7877=VERTEX_POINT('',#47093);
#7878=VERTEX_POINT('',#47236);
#7879=VERTEX_POINT('',#47309);
#7880=VERTEX_POINT('',#47452);
#7881=VERTEX_POINT('',#47525);
#7882=VERTEX_POINT('',#47668);
#7883=VERTEX_POINT('',#47741);
#7884=VERTEX_POINT('',#47884);
#7885=VERTEX_POINT('',#47957);
#7886=VERTEX_POINT('',#48100);
#7887=VERTEX_POINT('',#48173);
#7888=VERTEX_POINT('',#48316);
#7889=VERTEX_POINT('',#48389);
#7890=VERTEX_POINT('',#48532);
#7891=VERTEX_POINT('',#48605);
#7892=VERTEX_POINT('',#48748);
#7893=VERTEX_POINT('',#48821);
#7894=VERTEX_POINT('',#48964);
#7895=VERTEX_POINT('',#49037);
#7896=VERTEX_POINT('',#49180);
#7897=VERTEX_POINT('',#49258);
#7898=VERTEX_POINT('',#49259);
#7899=VERTEX_POINT('',#49261);
#7900=VERTEX_POINT('',#49263);
#7901=VERTEX_POINT('',#49267);
#7902=VERTEX_POINT('',#49269);
#7903=VERTEX_POINT('',#49273);
#7904=VERTEX_POINT('',#49275);
#7905=VERTEX_POINT('',#49283);
#7906=VERTEX_POINT('',#49285);
#7907=VERTEX_POINT('',#49292);
#7908=VERTEX_POINT('',#49293);
#7909=VERTEX_POINT('',#49297);
#7910=VERTEX_POINT('',#49312);
#7911=VERTEX_POINT('',#49314);
#7912=VERTEX_POINT('',#49316);
#7913=VERTEX_POINT('',#49353);
#7914=VERTEX_POINT('',#49372);
#7915=VERTEX_POINT('',#49374);
#7916=VERTEX_POINT('',#49378);
#7917=VERTEX_POINT('',#49380);
#7918=VERTEX_POINT('',#49387);
#7919=VERTEX_POINT('',#49388);
#7920=VERTEX_POINT('',#49392);
#7921=VERTEX_POINT('',#49407);
#7922=VERTEX_POINT('',#49409);
#7923=VERTEX_POINT('',#49411);
#7924=VERTEX_POINT('',#49448);
#7925=VERTEX_POINT('',#49467);
#7926=VERTEX_POINT('',#49469);
#7927=VERTEX_POINT('',#49473);
#7928=VERTEX_POINT('',#49475);
#7929=VERTEX_POINT('',#49482);
#7930=VERTEX_POINT('',#49484);
#7931=VERTEX_POINT('',#49488);
#7932=VERTEX_POINT('',#49490);
#7933=VERTEX_POINT('',#49497);
#7934=VERTEX_POINT('',#49499);
#7935=VERTEX_POINT('',#49503);
#7936=VERTEX_POINT('',#49505);
#7937=VERTEX_POINT('',#49512);
#7938=VERTEX_POINT('',#49514);
#7939=VERTEX_POINT('',#49518);
#7940=VERTEX_POINT('',#49520);
#7941=VERTEX_POINT('',#49527);
#7942=VERTEX_POINT('',#49529);
#7943=VERTEX_POINT('',#49533);
#7944=VERTEX_POINT('',#49535);
#7945=VERTEX_POINT('',#49542);
#7946=VERTEX_POINT('',#49543);
#7947=VERTEX_POINT('',#49545);
#7948=VERTEX_POINT('',#49547);
#7949=VERTEX_POINT('',#49551);
#7950=VERTEX_POINT('',#49553);
#7951=VERTEX_POINT('',#49557);
#7952=VERTEX_POINT('',#49559);
#7953=VERTEX_POINT('',#49563);
#7954=VERTEX_POINT('',#49565);
#7955=VERTEX_POINT('',#49569);
#7956=VERTEX_POINT('',#49571);
#7957=VERTEX_POINT('',#49579);
#7958=VERTEX_POINT('',#49582);
#7959=VERTEX_POINT('',#49586);
#7960=VERTEX_POINT('',#49590);
#7961=VERTEX_POINT('',#49607);
#7962=VERTEX_POINT('',#49608);
#7963=VERTEX_POINT('',#49610);
#7964=VERTEX_POINT('',#49612);
#7965=VERTEX_POINT('',#49616);
#7966=VERTEX_POINT('',#49618);
#7967=VERTEX_POINT('',#49622);
#7968=VERTEX_POINT('',#49624);
#7969=VERTEX_POINT('',#49628);
#7970=VERTEX_POINT('',#49629);
#7971=VERTEX_POINT('',#49631);
#7972=VERTEX_POINT('',#49702);
#7973=VERTEX_POINT('',#49704);
#7974=VERTEX_POINT('',#49775);
#7975=VERTEX_POINT('',#49777);
#7976=VERTEX_POINT('',#49848);
#7977=VERTEX_POINT('',#49850);
#7978=VERTEX_POINT('',#49921);
#7979=VERTEX_POINT('',#49923);
#7980=VERTEX_POINT('',#49994);
#7981=VERTEX_POINT('',#49996);
#7982=VERTEX_POINT('',#50067);
#7983=VERTEX_POINT('',#50069);
#7984=VERTEX_POINT('',#50140);
#7985=VERTEX_POINT('',#50142);
#7986=VERTEX_POINT('',#50213);
#7987=VERTEX_POINT('',#50215);
#7988=VERTEX_POINT('',#50286);
#7989=VERTEX_POINT('',#50288);
#7990=VERTEX_POINT('',#50359);
#7991=VERTEX_POINT('',#50361);
#7992=VERTEX_POINT('',#50432);
#7993=VERTEX_POINT('',#50434);
#7994=VERTEX_POINT('',#50505);
#7995=VERTEX_POINT('',#50507);
#7996=VERTEX_POINT('',#50578);
#7997=VERTEX_POINT('',#50580);
#7998=VERTEX_POINT('',#50651);
#7999=VERTEX_POINT('',#50653);
#8000=VERTEX_POINT('',#50724);
#8001=VERTEX_POINT('',#50726);
#8002=VERTEX_POINT('',#50797);
#8003=VERTEX_POINT('',#50799);
#8004=VERTEX_POINT('',#50870);
#8005=VERTEX_POINT('',#50872);
#8006=VERTEX_POINT('',#50943);
#8007=VERTEX_POINT('',#50945);
#8008=VERTEX_POINT('',#51016);
#8009=VERTEX_POINT('',#51018);
#8010=VERTEX_POINT('',#51089);
#8011=VERTEX_POINT('',#51091);
#8012=VERTEX_POINT('',#51162);
#8013=VERTEX_POINT('',#51164);
#8014=VERTEX_POINT('',#51235);
#8015=VERTEX_POINT('',#51237);
#8016=VERTEX_POINT('',#51308);
#8017=VERTEX_POINT('',#51310);
#8018=VERTEX_POINT('',#51381);
#8019=VERTEX_POINT('',#51383);
#8020=VERTEX_POINT('',#51454);
#8021=VERTEX_POINT('',#51456);
#8022=VERTEX_POINT('',#51527);
#8023=VERTEX_POINT('',#51529);
#8024=VERTEX_POINT('',#51600);
#8025=VERTEX_POINT('',#51602);
#8026=VERTEX_POINT('',#51673);
#8027=VERTEX_POINT('',#51675);
#8028=VERTEX_POINT('',#51746);
#8029=VERTEX_POINT('',#51748);
#8030=VERTEX_POINT('',#51819);
#8031=VERTEX_POINT('',#51821);
#8032=VERTEX_POINT('',#51892);
#8033=VERTEX_POINT('',#51894);
#8034=VERTEX_POINT('',#51965);
#8035=VERTEX_POINT('',#51967);
#8036=VERTEX_POINT('',#52038);
#8037=VERTEX_POINT('',#52040);
#8038=VERTEX_POINT('',#52111);
#8039=VERTEX_POINT('',#52113);
#8040=VERTEX_POINT('',#52184);
#8041=VERTEX_POINT('',#52186);
#8042=VERTEX_POINT('',#52257);
#8043=VERTEX_POINT('',#52259);
#8044=VERTEX_POINT('',#52330);
#8045=VERTEX_POINT('',#52332);
#8046=VERTEX_POINT('',#52403);
#8047=VERTEX_POINT('',#52405);
#8048=VERTEX_POINT('',#52476);
#8049=VERTEX_POINT('',#52478);
#8050=VERTEX_POINT('',#52549);
#8051=VERTEX_POINT('',#52551);
#8052=VERTEX_POINT('',#52622);
#8053=VERTEX_POINT('',#52624);
#8054=VERTEX_POINT('',#52695);
#8055=VERTEX_POINT('',#52697);
#8056=VERTEX_POINT('',#52768);
#8057=VERTEX_POINT('',#52770);
#8058=VERTEX_POINT('',#52841);
#8059=VERTEX_POINT('',#52843);
#8060=VERTEX_POINT('',#52914);
#8061=VERTEX_POINT('',#52916);
#8062=VERTEX_POINT('',#52987);
#8063=VERTEX_POINT('',#52989);
#8064=VERTEX_POINT('',#53060);
#8065=VERTEX_POINT('',#53062);
#8066=VERTEX_POINT('',#53133);
#8067=VERTEX_POINT('',#53135);
#8068=VERTEX_POINT('',#53206);
#8069=VERTEX_POINT('',#53208);
#8070=VERTEX_POINT('',#53279);
#8071=VERTEX_POINT('',#53281);
#8072=VERTEX_POINT('',#53352);
#8073=VERTEX_POINT('',#53354);
#8074=VERTEX_POINT('',#53425);
#8075=VERTEX_POINT('',#53427);
#8076=VERTEX_POINT('',#53498);
#8077=VERTEX_POINT('',#53500);
#8078=VERTEX_POINT('',#53571);
#8079=VERTEX_POINT('',#53573);
#8080=VERTEX_POINT('',#53644);
#8081=VERTEX_POINT('',#53646);
#8082=VERTEX_POINT('',#53717);
#8083=VERTEX_POINT('',#53719);
#8084=VERTEX_POINT('',#53790);
#8085=VERTEX_POINT('',#53792);
#8086=VERTEX_POINT('',#53863);
#8087=VERTEX_POINT('',#53865);
#8088=VERTEX_POINT('',#53936);
#8089=VERTEX_POINT('',#53938);
#8090=VERTEX_POINT('',#54009);
#8091=VERTEX_POINT('',#54011);
#8092=VERTEX_POINT('',#54082);
#8093=VERTEX_POINT('',#54084);
#8094=VERTEX_POINT('',#54155);
#8095=VERTEX_POINT('',#54157);
#8096=VERTEX_POINT('',#54228);
#8097=VERTEX_POINT('',#54230);
#8098=VERTEX_POINT('',#54301);
#8099=VERTEX_POINT('',#54303);
#8100=VERTEX_POINT('',#54374);
#8101=VERTEX_POINT('',#54376);
#8102=VERTEX_POINT('',#54447);
#8103=VERTEX_POINT('',#54449);
#8104=VERTEX_POINT('',#54520);
#8105=VERTEX_POINT('',#54522);
#8106=VERTEX_POINT('',#54593);
#8107=VERTEX_POINT('',#54595);
#8108=VERTEX_POINT('',#54666);
#8109=VERTEX_POINT('',#54668);
#8110=VERTEX_POINT('',#54739);
#8111=VERTEX_POINT('',#54741);
#8112=VERTEX_POINT('',#54812);
#8113=VERTEX_POINT('',#54814);
#8114=VERTEX_POINT('',#54885);
#8115=VERTEX_POINT('',#54887);
#8116=VERTEX_POINT('',#54958);
#8117=VERTEX_POINT('',#54960);
#8118=VERTEX_POINT('',#55031);
#8119=VERTEX_POINT('',#55033);
#8120=VERTEX_POINT('',#55104);
#8121=VERTEX_POINT('',#55106);
#8122=VERTEX_POINT('',#55177);
#8123=VERTEX_POINT('',#55179);
#8124=VERTEX_POINT('',#55250);
#8125=VERTEX_POINT('',#55252);
#8126=VERTEX_POINT('',#55323);
#8127=VERTEX_POINT('',#55325);
#8128=VERTEX_POINT('',#55396);
#8129=VERTEX_POINT('',#55472);
#8130=VERTEX_POINT('',#55474);
#8131=VERTEX_POINT('',#55618);
#8132=VERTEX_POINT('',#55625);
#8133=VERTEX_POINT('',#55837);
#8134=VERTEX_POINT('',#55844);
#8135=VERTEX_POINT('',#55919);
#8136=VERTEX_POINT('',#56067);
#8137=VERTEX_POINT('',#56279);
#8138=VERTEX_POINT('',#56286);
#8139=VERTEX_POINT('',#56361);
#8140=VERTEX_POINT('',#56509);
#8141=VERTEX_POINT('',#56721);
#8142=VERTEX_POINT('',#56728);
#8143=VERTEX_POINT('',#56803);
#8144=VERTEX_POINT('',#56951);
#8145=VERTEX_POINT('',#57163);
#8146=VERTEX_POINT('',#57170);
#8147=VERTEX_POINT('',#57245);
#8148=VERTEX_POINT('',#57393);
#8149=VERTEX_POINT('',#57605);
#8150=VERTEX_POINT('',#57612);
#8151=VERTEX_POINT('',#57687);
#8152=VERTEX_POINT('',#57835);
#8153=VERTEX_POINT('',#58047);
#8154=VERTEX_POINT('',#58054);
#8155=VERTEX_POINT('',#58129);
#8156=VERTEX_POINT('',#58277);
#8157=VERTEX_POINT('',#58489);
#8158=VERTEX_POINT('',#58496);
#8159=VERTEX_POINT('',#58571);
#8160=VERTEX_POINT('',#58719);
#8161=VERTEX_POINT('',#58931);
#8162=VERTEX_POINT('',#58938);
#8163=VERTEX_POINT('',#59013);
#8164=VERTEX_POINT('',#59161);
#8165=VERTEX_POINT('',#59373);
#8166=VERTEX_POINT('',#59380);
#8167=VERTEX_POINT('',#59455);
#8168=VERTEX_POINT('',#59603);
#8169=VERTEX_POINT('',#59815);
#8170=VERTEX_POINT('',#59822);
#8171=VERTEX_POINT('',#59897);
#8172=VERTEX_POINT('',#60045);
#8173=VERTEX_POINT('',#60257);
#8174=VERTEX_POINT('',#60264);
#8175=VERTEX_POINT('',#60339);
#8176=VERTEX_POINT('',#60487);
#8177=VERTEX_POINT('',#60699);
#8178=VERTEX_POINT('',#60706);
#8179=VERTEX_POINT('',#60781);
#8180=VERTEX_POINT('',#60929);
#8181=VERTEX_POINT('',#61141);
#8182=VERTEX_POINT('',#61148);
#8183=VERTEX_POINT('',#61223);
#8184=VERTEX_POINT('',#61371);
#8185=VERTEX_POINT('',#61583);
#8186=VERTEX_POINT('',#61590);
#8187=VERTEX_POINT('',#61665);
#8188=VERTEX_POINT('',#61813);
#8189=VERTEX_POINT('',#62025);
#8190=VERTEX_POINT('',#62032);
#8191=VERTEX_POINT('',#62107);
#8192=VERTEX_POINT('',#62255);
#8193=VERTEX_POINT('',#62467);
#8194=VERTEX_POINT('',#62474);
#8195=VERTEX_POINT('',#62549);
#8196=VERTEX_POINT('',#62697);
#8197=VERTEX_POINT('',#62909);
#8198=VERTEX_POINT('',#62916);
#8199=VERTEX_POINT('',#62991);
#8200=VERTEX_POINT('',#63139);
#8201=VERTEX_POINT('',#63351);
#8202=VERTEX_POINT('',#63358);
#8203=VERTEX_POINT('',#63433);
#8204=VERTEX_POINT('',#63581);
#8205=VERTEX_POINT('',#63793);
#8206=VERTEX_POINT('',#63800);
#8207=VERTEX_POINT('',#63875);
#8208=VERTEX_POINT('',#64023);
#8209=VERTEX_POINT('',#64235);
#8210=VERTEX_POINT('',#64242);
#8211=VERTEX_POINT('',#64317);
#8212=VERTEX_POINT('',#64465);
#8213=VERTEX_POINT('',#64677);
#8214=VERTEX_POINT('',#64684);
#8215=VERTEX_POINT('',#64759);
#8216=VERTEX_POINT('',#64907);
#8217=VERTEX_POINT('',#65119);
#8218=VERTEX_POINT('',#65126);
#8219=VERTEX_POINT('',#65201);
#8220=VERTEX_POINT('',#65349);
#8221=VERTEX_POINT('',#65561);
#8222=VERTEX_POINT('',#65568);
#8223=VERTEX_POINT('',#65643);
#8224=VERTEX_POINT('',#65791);
#8225=VERTEX_POINT('',#66003);
#8226=VERTEX_POINT('',#66010);
#8227=VERTEX_POINT('',#66085);
#8228=VERTEX_POINT('',#66233);
#8229=VERTEX_POINT('',#66445);
#8230=VERTEX_POINT('',#66452);
#8231=VERTEX_POINT('',#66527);
#8232=VERTEX_POINT('',#66675);
#8233=VERTEX_POINT('',#66887);
#8234=VERTEX_POINT('',#66894);
#8235=VERTEX_POINT('',#66969);
#8236=VERTEX_POINT('',#67117);
#8237=VERTEX_POINT('',#67329);
#8238=VERTEX_POINT('',#67336);
#8239=VERTEX_POINT('',#67411);
#8240=VERTEX_POINT('',#67559);
#8241=VERTEX_POINT('',#67771);
#8242=VERTEX_POINT('',#67778);
#8243=VERTEX_POINT('',#67853);
#8244=VERTEX_POINT('',#68001);
#8245=VERTEX_POINT('',#68213);
#8246=VERTEX_POINT('',#68220);
#8247=VERTEX_POINT('',#68295);
#8248=VERTEX_POINT('',#68443);
#8249=VERTEX_POINT('',#68655);
#8250=VERTEX_POINT('',#68662);
#8251=VERTEX_POINT('',#68737);
#8252=VERTEX_POINT('',#68885);
#8253=VERTEX_POINT('',#69097);
#8254=VERTEX_POINT('',#69104);
#8255=VERTEX_POINT('',#69179);
#8256=VERTEX_POINT('',#69327);
#8257=VERTEX_POINT('',#69539);
#8258=VERTEX_POINT('',#69546);
#8259=VERTEX_POINT('',#69621);
#8260=VERTEX_POINT('',#69769);
#8261=VERTEX_POINT('',#69981);
#8262=VERTEX_POINT('',#69988);
#8263=VERTEX_POINT('',#70063);
#8264=VERTEX_POINT('',#70211);
#8265=VERTEX_POINT('',#70423);
#8266=VERTEX_POINT('',#70430);
#8267=VERTEX_POINT('',#70505);
#8268=VERTEX_POINT('',#70653);
#8269=VERTEX_POINT('',#70865);
#8270=VERTEX_POINT('',#70872);
#8271=VERTEX_POINT('',#70947);
#8272=VERTEX_POINT('',#71095);
#8273=VERTEX_POINT('',#71307);
#8274=VERTEX_POINT('',#71314);
#8275=VERTEX_POINT('',#71389);
#8276=VERTEX_POINT('',#71537);
#8277=VERTEX_POINT('',#71749);
#8278=VERTEX_POINT('',#71756);
#8279=VERTEX_POINT('',#71831);
#8280=VERTEX_POINT('',#71979);
#8281=VERTEX_POINT('',#72191);
#8282=VERTEX_POINT('',#72198);
#8283=VERTEX_POINT('',#72273);
#8284=VERTEX_POINT('',#72421);
#8285=VERTEX_POINT('',#72494);
#8286=VERTEX_POINT('',#72637);
#8287=VERTEX_POINT('',#72715);
#8288=VERTEX_POINT('',#72863);
#8289=VERTEX_POINT('',#72870);
#8290=VERTEX_POINT('',#73082);
#8291=VERTEX_POINT('',#73161);
#8292=VERTEX_POINT('',#73162);
#8293=VERTEX_POINT('',#73164);
#8294=VERTEX_POINT('',#73166);
#8295=VERTEX_POINT('',#73168);
#8296=VERTEX_POINT('',#73170);
#8297=VERTEX_POINT('',#73172);
#8298=VERTEX_POINT('',#73174);
#8299=VERTEX_POINT('',#73178);
#8300=VERTEX_POINT('',#73180);
#8301=VERTEX_POINT('',#73184);
#8302=VERTEX_POINT('',#73188);
#8303=VERTEX_POINT('',#73192);
#8304=VERTEX_POINT('',#73196);
#8305=VERTEX_POINT('',#73197);
#8306=VERTEX_POINT('',#73200);
#8307=EDGE_CURVE('',#6824,#6824,#6104,.T.);
#8308=EDGE_CURVE('',#6824,#6825,#4056,.T.);
#8309=EDGE_CURVE('',#6825,#6825,#6105,.T.);
#8310=EDGE_CURVE('',#6826,#6826,#6106,.T.);
#8311=EDGE_CURVE('',#6826,#6827,#4057,.T.);
#8312=EDGE_CURVE('',#6827,#6827,#6107,.T.);
#8313=EDGE_CURVE('',#6828,#6828,#6108,.T.);
#8314=EDGE_CURVE('',#6828,#6829,#4058,.T.);
#8315=EDGE_CURVE('',#6829,#6829,#6109,.T.);
#8316=EDGE_CURVE('',#6830,#6830,#6110,.T.);
#8317=EDGE_CURVE('',#6830,#6831,#4059,.T.);
#8318=EDGE_CURVE('',#6831,#6831,#6111,.T.);
#8319=EDGE_CURVE('',#6832,#6833,#4060,.T.);
#8320=EDGE_CURVE('',#6833,#6834,#4061,.T.);
#8321=EDGE_CURVE('',#6835,#6834,#4062,.T.);
#8322=EDGE_CURVE('',#6832,#6835,#4063,.T.);
#8323=EDGE_CURVE('',#6836,#6832,#4064,.T.);
#8324=EDGE_CURVE('',#6837,#6835,#4065,.T.);
#8325=EDGE_CURVE('',#6836,#6837,#4066,.T.);
#8326=EDGE_CURVE('',#6838,#6836,#4067,.T.);
#8327=EDGE_CURVE('',#6839,#6837,#4068,.T.);
#8328=EDGE_CURVE('',#6838,#6839,#4069,.T.);
#8329=EDGE_CURVE('',#6833,#6838,#4070,.T.);
#8330=EDGE_CURVE('',#6834,#6839,#4071,.T.);
#8331=EDGE_CURVE('',#6840,#6840,#6112,.T.);
#8332=EDGE_CURVE('',#6840,#6841,#4072,.T.);
#8333=EDGE_CURVE('',#6841,#6841,#6113,.T.);
#8334=EDGE_CURVE('',#6842,#6842,#6114,.T.);
#8335=EDGE_CURVE('',#6842,#6843,#4073,.T.);
#8336=EDGE_CURVE('',#6843,#6843,#6115,.T.);
#8337=EDGE_CURVE('',#6844,#6844,#6116,.T.);
#8338=EDGE_CURVE('',#6844,#6845,#4074,.T.);
#8339=EDGE_CURVE('',#6845,#6845,#6117,.T.);
#8340=EDGE_CURVE('',#6846,#6846,#6118,.T.);
#8341=EDGE_CURVE('',#6846,#6847,#4075,.T.);
#8342=EDGE_CURVE('',#6847,#6847,#6119,.T.);
#8343=EDGE_CURVE('',#6848,#6849,#4076,.T.);
#8344=EDGE_CURVE('',#6850,#6848,#6120,.T.);
#8345=EDGE_CURVE('',#6851,#6850,#4077,.T.);
#8346=EDGE_CURVE('',#6849,#6851,#6121,.T.);
#8347=EDGE_CURVE('',#6852,#6848,#4078,.T.);
#8348=EDGE_CURVE('',#6853,#6852,#6122,.T.);
#8349=EDGE_CURVE('',#6850,#6853,#4079,.T.);
#8350=EDGE_CURVE('',#6854,#6851,#4080,.T.);
#8351=EDGE_CURVE('',#6855,#6854,#4081,.T.);
#8352=EDGE_CURVE('',#6855,#6856,#4082,.T.);
#8353=EDGE_CURVE('',#6857,#6856,#4083,.T.);
#8354=EDGE_CURVE('',#6857,#6858,#4084,.T.);
#8355=EDGE_CURVE('',#6858,#6859,#4085,.T.);
#8356=EDGE_CURVE('',#6859,#6860,#4086,.T.);
#8357=EDGE_CURVE('',#6860,#6861,#4087,.T.);
#8358=EDGE_CURVE('',#6862,#6861,#4088,.T.);
#8359=EDGE_CURVE('',#6862,#6863,#6123,.T.);
#8360=EDGE_CURVE('',#6864,#6863,#4089,.T.);
#8361=EDGE_CURVE('',#6864,#6865,#6124,.T.);
#8362=EDGE_CURVE('',#6849,#6865,#4090,.T.);
#8363=EDGE_CURVE('',#6866,#6866,#6125,.T.);
#8364=EDGE_CURVE('',#6867,#6867,#6126,.T.);
#8365=EDGE_CURVE('',#6868,#6868,#6127,.T.);
#8366=EDGE_CURVE('',#6869,#6869,#6128,.T.);
#8367=EDGE_CURVE('',#6853,#6870,#4091,.T.);
#8368=EDGE_CURVE('',#6870,#6871,#4092,.T.);
#8369=EDGE_CURVE('',#6871,#6872,#4093,.T.);
#8370=EDGE_CURVE('',#6872,#6873,#4094,.T.);
#8371=EDGE_CURVE('',#6873,#6874,#4095,.T.);
#8372=EDGE_CURVE('',#6874,#6875,#4096,.T.);
#8373=EDGE_CURVE('',#6875,#6876,#4097,.T.);
#8374=EDGE_CURVE('',#6876,#6877,#4098,.T.);
#8375=EDGE_CURVE('',#6877,#6854,#4099,.T.);
#8376=EDGE_CURVE('',#6878,#6878,#6129,.T.);
#8377=EDGE_CURVE('',#6879,#6879,#6130,.T.);
#8378=EDGE_CURVE('',#6880,#6880,#6131,.T.);
#8379=EDGE_CURVE('',#6881,#6881,#6132,.T.);
#8380=EDGE_CURVE('',#6882,#6882,#6133,.T.);
#8381=EDGE_CURVE('',#6875,#6883,#6134,.T.);
#8382=EDGE_CURVE('',#6884,#6883,#4100,.T.);
#8383=EDGE_CURVE('',#6876,#6884,#6135,.T.);
#8384=EDGE_CURVE('',#6885,#6874,#6136,.T.);
#8385=EDGE_CURVE('',#6883,#6885,#4101,.T.);
#8386=EDGE_CURVE('',#6886,#6884,#4102,.T.);
#8387=EDGE_CURVE('',#6886,#6887,#6137,.T.);
#8388=EDGE_CURVE('',#6888,#6887,#4103,.T.);
#8389=EDGE_CURVE('',#6888,#6889,#6138,.T.);
#8390=EDGE_CURVE('',#6890,#6889,#4104,.T.);
#8391=EDGE_CURVE('',#6891,#6890,#4105,.T.);
#8392=EDGE_CURVE('',#6891,#6892,#4106,.T.);
#8393=EDGE_CURVE('',#6893,#6892,#4107,.T.);
#8394=EDGE_CURVE('',#6893,#6894,#4108,.T.);
#8395=EDGE_CURVE('',#6894,#6895,#4109,.T.);
#8396=EDGE_CURVE('',#6895,#6896,#4110,.T.);
#8397=EDGE_CURVE('',#6896,#6877,#4111,.T.);
#8398=EDGE_CURVE('',#6897,#6897,#6139,.T.);
#8399=EDGE_CURVE('',#6898,#6898,#6140,.T.);
#8400=EDGE_CURVE('',#6899,#6899,#6141,.T.);
#8401=EDGE_CURVE('',#6900,#6900,#6142,.T.);
#8402=EDGE_CURVE('',#6885,#6901,#4112,.T.);
#8403=EDGE_CURVE('',#6901,#6902,#4113,.T.);
#8404=EDGE_CURVE('',#6902,#6903,#4114,.T.);
#8405=EDGE_CURVE('',#6903,#6904,#4115,.T.);
#8406=EDGE_CURVE('',#6904,#6886,#4116,.T.);
#8407=EDGE_CURVE('',#6901,#6873,#6143,.T.);
#8408=EDGE_CURVE('',#6905,#6852,#4117,.T.);
#8409=EDGE_CURVE('',#6870,#6905,#6144,.T.);
#8410=EDGE_CURVE('',#6906,#6905,#4118,.T.);
#8411=EDGE_CURVE('',#6906,#6907,#6145,.T.);
#8412=EDGE_CURVE('',#6908,#6907,#4119,.T.);
#8413=EDGE_CURVE('',#6908,#6909,#6146,.T.);
#8414=EDGE_CURVE('',#6910,#6909,#4120,.T.);
#8415=EDGE_CURVE('',#6911,#6910,#4121,.T.);
#8416=EDGE_CURVE('',#6912,#6911,#4122,.T.);
#8417=EDGE_CURVE('',#6912,#6871,#4123,.T.);
#8418=EDGE_CURVE('',#6865,#6913,#4124,.T.);
#8419=EDGE_CURVE('',#6913,#6914,#4125,.T.);
#8420=EDGE_CURVE('',#6914,#6906,#4126,.T.);
#8421=EDGE_CURVE('',#6915,#6915,#6147,.T.);
#8422=EDGE_CURVE('',#6915,#6869,#4127,.T.);
#8423=EDGE_CURVE('',#6916,#6916,#6148,.T.);
#8424=EDGE_CURVE('',#6916,#6868,#4128,.T.);
#8425=EDGE_CURVE('',#6897,#6917,#4129,.T.);
#8426=EDGE_CURVE('',#6917,#6917,#6149,.T.);
#8427=EDGE_CURVE('',#6898,#6918,#4130,.T.);
#8428=EDGE_CURVE('',#6918,#6918,#6150,.T.);
#8429=EDGE_CURVE('',#6919,#6864,#4131,.T.);
#8430=EDGE_CURVE('',#6913,#6919,#6151,.T.);
#8431=EDGE_CURVE('',#6920,#6919,#4132,.T.);
#8432=EDGE_CURVE('',#6914,#6920,#6152,.T.);
#8433=EDGE_CURVE('',#6904,#6921,#6153,.T.);
#8434=EDGE_CURVE('',#6887,#6921,#4133,.T.);
#8435=EDGE_CURVE('',#6922,#6903,#6154,.T.);
#8436=EDGE_CURVE('',#6921,#6922,#4134,.T.);
#8437=EDGE_CURVE('',#6922,#6923,#4135,.T.);
#8438=EDGE_CURVE('',#6923,#6924,#4136,.T.);
#8439=EDGE_CURVE('',#6924,#6925,#4137,.T.);
#8440=EDGE_CURVE('',#6925,#6926,#4138,.T.);
#8441=EDGE_CURVE('',#6926,#6888,#4139,.T.);
#8442=EDGE_CURVE('',#6907,#6920,#4140,.T.);
#8443=EDGE_CURVE('',#6923,#6902,#6155,.T.);
#8444=EDGE_CURVE('',#6927,#6872,#4141,.T.);
#8445=EDGE_CURVE('',#6928,#6927,#4142,.T.);
#8446=EDGE_CURVE('',#6928,#6929,#4143,.T.);
#8447=EDGE_CURVE('',#6930,#6929,#4144,.T.);
#8448=EDGE_CURVE('',#6930,#6924,#6156,.T.);
#8449=EDGE_CURVE('',#6863,#6931,#4145,.T.);
#8450=EDGE_CURVE('',#6931,#6932,#4146,.T.);
#8451=EDGE_CURVE('',#6932,#6908,#4147,.T.);
#8452=EDGE_CURVE('',#6933,#6933,#6157,.T.);
#8453=EDGE_CURVE('',#6933,#6867,#4148,.T.);
#8454=EDGE_CURVE('',#6934,#6934,#6158,.T.);
#8455=EDGE_CURVE('',#6934,#6866,#4149,.T.);
#8456=EDGE_CURVE('',#6900,#6935,#4150,.T.);
#8457=EDGE_CURVE('',#6935,#6935,#6159,.T.);
#8458=EDGE_CURVE('',#6899,#6936,#4151,.T.);
#8459=EDGE_CURVE('',#6936,#6936,#6160,.T.);
#8460=EDGE_CURVE('',#6937,#6862,#4152,.T.);
#8461=EDGE_CURVE('',#6931,#6937,#6161,.T.);
#8462=EDGE_CURVE('',#6938,#6937,#4153,.T.);
#8463=EDGE_CURVE('',#6932,#6938,#6162,.T.);
#8464=EDGE_CURVE('',#6861,#6890,#4154,.T.);
#8465=EDGE_CURVE('',#6889,#6939,#4155,.T.);
#8466=EDGE_CURVE('',#6939,#6940,#4156,.T.);
#8467=EDGE_CURVE('',#6940,#6930,#4157,.T.);
#8468=EDGE_CURVE('',#6929,#6910,#4158,.T.);
#8469=EDGE_CURVE('',#6909,#6938,#4159,.T.);
#8470=EDGE_CURVE('',#6941,#6941,#6163,.T.);
#8471=EDGE_CURVE('',#6942,#6942,#6164,.T.);
#8472=EDGE_CURVE('',#6943,#6943,#6165,.T.);
#8473=EDGE_CURVE('',#6944,#6944,#6166,.T.);
#8474=EDGE_CURVE('',#6945,#6945,#6167,.T.);
#8475=EDGE_CURVE('',#6926,#6939,#6168,.T.);
#8476=EDGE_CURVE('',#6940,#6925,#6169,.T.);
#8477=EDGE_CURVE('',#6946,#6946,#6170,.T.);
#8478=EDGE_CURVE('',#6946,#6947,#4160,.T.);
#8479=EDGE_CURVE('',#6947,#6947,#6171,.T.);
#8480=EDGE_CURVE('',#6948,#6948,#6172,.T.);
#8481=EDGE_CURVE('',#6949,#6949,#6173,.T.);
#8482=EDGE_CURVE('',#6949,#6950,#4161,.T.);
#8483=EDGE_CURVE('',#6950,#6950,#6174,.T.);
#8484=EDGE_CURVE('',#6951,#6951,#6175,.T.);
#8485=EDGE_CURVE('',#6952,#6952,#6176,.T.);
#8486=EDGE_CURVE('',#6952,#6953,#4162,.T.);
#8487=EDGE_CURVE('',#6953,#6953,#6177,.T.);
#8488=EDGE_CURVE('',#6954,#6954,#6178,.T.);
#8489=EDGE_CURVE('',#6955,#6955,#6179,.T.);
#8490=EDGE_CURVE('',#6955,#6956,#4163,.T.);
#8491=EDGE_CURVE('',#6956,#6956,#6180,.T.);
#8492=EDGE_CURVE('',#6957,#6957,#6181,.T.);
#8493=EDGE_CURVE('',#6958,#6958,#6182,.T.);
#8494=EDGE_CURVE('',#6958,#6948,#4164,.T.);
#8495=EDGE_CURVE('',#6959,#6959,#6183,.T.);
#8496=EDGE_CURVE('',#6959,#6951,#4165,.T.);
#8497=EDGE_CURVE('',#6960,#6960,#6184,.T.);
#8498=EDGE_CURVE('',#6960,#6954,#4166,.T.);
#8499=EDGE_CURVE('',#6961,#6961,#6185,.T.);
#8500=EDGE_CURVE('',#6961,#6957,#4167,.T.);
#8501=EDGE_CURVE('',#6962,#6962,#6186,.T.);
#8502=EDGE_CURVE('',#6962,#6878,#4168,.T.);
#8503=EDGE_CURVE('',#6963,#6963,#6187,.T.);
#8504=EDGE_CURVE('',#6963,#6882,#4169,.T.);
#8505=EDGE_CURVE('',#6964,#6964,#6188,.T.);
#8506=EDGE_CURVE('',#6964,#6941,#4170,.T.);
#8507=EDGE_CURVE('',#6965,#6965,#6189,.T.);
#8508=EDGE_CURVE('',#6965,#6945,#4171,.T.);
#8509=EDGE_CURVE('',#6966,#6966,#6190,.T.);
#8510=EDGE_CURVE('',#6966,#6879,#4172,.T.);
#8511=EDGE_CURVE('',#6967,#6967,#6191,.T.);
#8512=EDGE_CURVE('',#6967,#6942,#4173,.T.);
#8513=EDGE_CURVE('',#6968,#6968,#6192,.T.);
#8514=EDGE_CURVE('',#6968,#6943,#4174,.T.);
#8515=EDGE_CURVE('',#6969,#6969,#6193,.T.);
#8516=EDGE_CURVE('',#6969,#6944,#4175,.T.);
#8517=EDGE_CURVE('',#6970,#6970,#6194,.T.);
#8518=EDGE_CURVE('',#6970,#6880,#4176,.T.);
#8519=EDGE_CURVE('',#6971,#6971,#6195,.T.);
#8520=EDGE_CURVE('',#6971,#6881,#4177,.T.);
#8521=EDGE_CURVE('',#6896,#6855,#4178,.T.);
#8522=EDGE_CURVE('',#6856,#6895,#4179,.T.);
#8523=EDGE_CURVE('',#6894,#6857,#4180,.T.);
#8524=EDGE_CURVE('',#6860,#6891,#4181,.T.);
#8525=EDGE_CURVE('',#6892,#6859,#4182,.T.);
#8526=EDGE_CURVE('',#6911,#6928,#4183,.T.);
#8527=EDGE_CURVE('',#6927,#6912,#4184,.T.);
#8528=EDGE_CURVE('',#6858,#6893,#4185,.T.);
#8529=EDGE_CURVE('',#6972,#6972,#6196,.T.);
#8530=EDGE_CURVE('',#6972,#6973,#4186,.T.);
#8531=EDGE_CURVE('',#6973,#6973,#6197,.T.);
#8532=EDGE_CURVE('',#6974,#6974,#6198,.T.);
#8533=EDGE_CURVE('',#6974,#6975,#4187,.T.);
#8534=EDGE_CURVE('',#6975,#6975,#6199,.T.);
#8535=EDGE_CURVE('',#6976,#6976,#6200,.T.);
#8536=EDGE_CURVE('',#6976,#6977,#4188,.T.);
#8537=EDGE_CURVE('',#6977,#6977,#6201,.T.);
#8538=EDGE_CURVE('',#6978,#6978,#6202,.T.);
#8539=EDGE_CURVE('',#6978,#6979,#4189,.T.);
#8540=EDGE_CURVE('',#6979,#6979,#6203,.T.);
#8541=EDGE_CURVE('',#6980,#6981,#4190,.T.);
#8542=EDGE_CURVE('',#6980,#6982,#4191,.T.);
#8543=EDGE_CURVE('',#6983,#6982,#4192,.T.);
#8544=EDGE_CURVE('',#6981,#6983,#4193,.T.);
#8545=EDGE_CURVE('',#6981,#6984,#4194,.T.);
#8546=EDGE_CURVE('',#6985,#6983,#4195,.T.);
#8547=EDGE_CURVE('',#6984,#6985,#4196,.T.);
#8548=EDGE_CURVE('',#6984,#6986,#4197,.T.);
#8549=EDGE_CURVE('',#6987,#6985,#4198,.T.);
#8550=EDGE_CURVE('',#6986,#6987,#4199,.T.);
#8551=EDGE_CURVE('',#6986,#6980,#4200,.T.);
#8552=EDGE_CURVE('',#6982,#6987,#4201,.T.);
#8553=EDGE_CURVE('',#6988,#6988,#6204,.T.);
#8554=EDGE_CURVE('',#6988,#6989,#4202,.T.);
#8555=EDGE_CURVE('',#6989,#6989,#6205,.T.);
#8556=EDGE_CURVE('',#6990,#6990,#6206,.T.);
#8557=EDGE_CURVE('',#6990,#6991,#4203,.T.);
#8558=EDGE_CURVE('',#6991,#6991,#6207,.T.);
#8559=EDGE_CURVE('',#6992,#6992,#6208,.T.);
#8560=EDGE_CURVE('',#6992,#6993,#4204,.T.);
#8561=EDGE_CURVE('',#6993,#6993,#6209,.T.);
#8562=EDGE_CURVE('',#6994,#6994,#6210,.T.);
#8563=EDGE_CURVE('',#6994,#6995,#4205,.T.);
#8564=EDGE_CURVE('',#6995,#6995,#6211,.T.);
#8565=EDGE_CURVE('',#6996,#6997,#4206,.T.);
#8566=EDGE_CURVE('',#6996,#6998,#6212,.T.);
#8567=EDGE_CURVE('',#6999,#6998,#4207,.T.);
#8568=EDGE_CURVE('',#6997,#6999,#6213,.T.);
#8569=EDGE_CURVE('',#7000,#6996,#4208,.T.);
#8570=EDGE_CURVE('',#7001,#7000,#6214,.T.);
#8571=EDGE_CURVE('',#6998,#7001,#4209,.T.);
#8572=EDGE_CURVE('',#7002,#6999,#4210,.T.);
#8573=EDGE_CURVE('',#7003,#7002,#6215,.T.);
#8574=EDGE_CURVE('',#6997,#7003,#4211,.T.);
#8575=EDGE_CURVE('',#7004,#7001,#4212,.T.);
#8576=EDGE_CURVE('',#7005,#7004,#4213,.T.);
#8577=EDGE_CURVE('',#7006,#7005,#4214,.T.);
#8578=EDGE_CURVE('',#7006,#7007,#4215,.T.);
#8579=EDGE_CURVE('',#7007,#7008,#4216,.T.);
#8580=EDGE_CURVE('',#7008,#7009,#4217,.T.);
#8581=EDGE_CURVE('',#7009,#7010,#4218,.T.);
#8582=EDGE_CURVE('',#7010,#7011,#4219,.T.);
#8583=EDGE_CURVE('',#7011,#7002,#4220,.T.);
#8584=EDGE_CURVE('',#7012,#7012,#6216,.T.);
#8585=EDGE_CURVE('',#7013,#7013,#6217,.T.);
#8586=EDGE_CURVE('',#7014,#7014,#6218,.T.);
#8587=EDGE_CURVE('',#7015,#7015,#6219,.T.);
#8588=EDGE_CURVE('',#7016,#7016,#6220,.T.);
#8589=EDGE_CURVE('',#7017,#7018,#4221,.T.);
#8590=EDGE_CURVE('',#7017,#7007,#6221,.T.);
#8591=EDGE_CURVE('',#7018,#7006,#6222,.T.);
#8592=EDGE_CURVE('',#7019,#7017,#4222,.T.);
#8593=EDGE_CURVE('',#7008,#7019,#6223,.T.);
#8594=EDGE_CURVE('',#7005,#7020,#4223,.T.);
#8595=EDGE_CURVE('',#7021,#7020,#4224,.T.);
#8596=EDGE_CURVE('',#7021,#7022,#4225,.T.);
#8597=EDGE_CURVE('',#7023,#7022,#4226,.T.);
#8598=EDGE_CURVE('',#7024,#7023,#4227,.T.);
#8599=EDGE_CURVE('',#7025,#7024,#4228,.T.);
#8600=EDGE_CURVE('',#7026,#7025,#4229,.T.);
#8601=EDGE_CURVE('',#7026,#7027,#4230,.T.);
#8602=EDGE_CURVE('',#7027,#7028,#6224,.T.);
#8603=EDGE_CURVE('',#7028,#7029,#4231,.T.);
#8604=EDGE_CURVE('',#7029,#7030,#6225,.T.);
#8605=EDGE_CURVE('',#7030,#7018,#4232,.T.);
#8606=EDGE_CURVE('',#7031,#7031,#6226,.T.);
#8607=EDGE_CURVE('',#7032,#7032,#6227,.T.);
#8608=EDGE_CURVE('',#7033,#7033,#6228,.T.);
#8609=EDGE_CURVE('',#7034,#7034,#6229,.T.);
#8610=EDGE_CURVE('',#7035,#7019,#4233,.T.);
#8611=EDGE_CURVE('',#7009,#7035,#6230,.T.);
#8612=EDGE_CURVE('',#7000,#7036,#4234,.T.);
#8613=EDGE_CURVE('',#7036,#7037,#6231,.T.);
#8614=EDGE_CURVE('',#7037,#7038,#4235,.T.);
#8615=EDGE_CURVE('',#7038,#7039,#6232,.T.);
#8616=EDGE_CURVE('',#7039,#7040,#4236,.T.);
#8617=EDGE_CURVE('',#7040,#7041,#4237,.T.);
#8618=EDGE_CURVE('',#7042,#7041,#4238,.T.);
#8619=EDGE_CURVE('',#7042,#7043,#4239,.T.);
#8620=EDGE_CURVE('',#7044,#7043,#4240,.T.);
#8621=EDGE_CURVE('',#7045,#7044,#4241,.T.);
#8622=EDGE_CURVE('',#7046,#7045,#4242,.T.);
#8623=EDGE_CURVE('',#7004,#7046,#4243,.T.);
#8624=EDGE_CURVE('',#7047,#7047,#6233,.T.);
#8625=EDGE_CURVE('',#7048,#7048,#6234,.T.);
#8626=EDGE_CURVE('',#7049,#7049,#6235,.T.);
#8627=EDGE_CURVE('',#7050,#7050,#6236,.T.);
#8628=EDGE_CURVE('',#7051,#7035,#4244,.T.);
#8629=EDGE_CURVE('',#7051,#7052,#6237,.T.);
#8630=EDGE_CURVE('',#7053,#7052,#4245,.T.);
#8631=EDGE_CURVE('',#7053,#7054,#6238,.T.);
#8632=EDGE_CURVE('',#7055,#7054,#4246,.T.);
#8633=EDGE_CURVE('',#7055,#7056,#4247,.T.);
#8634=EDGE_CURVE('',#7056,#7057,#4248,.T.);
#8635=EDGE_CURVE('',#7010,#7057,#4249,.T.);
#8636=EDGE_CURVE('',#7030,#7058,#4250,.T.);
#8637=EDGE_CURVE('',#7058,#7059,#4251,.T.);
#8638=EDGE_CURVE('',#7059,#7051,#4252,.T.);
#8639=EDGE_CURVE('',#7003,#7060,#4253,.T.);
#8640=EDGE_CURVE('',#7060,#7061,#4254,.T.);
#8641=EDGE_CURVE('',#7061,#7062,#4255,.T.);
#8642=EDGE_CURVE('',#7062,#7036,#4256,.T.);
#8643=EDGE_CURVE('',#7063,#7063,#6239,.T.);
#8644=EDGE_CURVE('',#7063,#7050,#4257,.T.);
#8645=EDGE_CURVE('',#7064,#7064,#6240,.T.);
#8646=EDGE_CURVE('',#7064,#7049,#4258,.T.);
#8647=EDGE_CURVE('',#7034,#7065,#4259,.T.);
#8648=EDGE_CURVE('',#7065,#7065,#6241,.T.);
#8649=EDGE_CURVE('',#7033,#7066,#4260,.T.);
#8650=EDGE_CURVE('',#7066,#7066,#6242,.T.);
#8651=EDGE_CURVE('',#7067,#7068,#4261,.T.);
#8652=EDGE_CURVE('',#7067,#7062,#6243,.T.);
#8653=EDGE_CURVE('',#7068,#7061,#6244,.T.);
#8654=EDGE_CURVE('',#7037,#7067,#4262,.T.);
#8655=EDGE_CURVE('',#7069,#7060,#6245,.T.);
#8656=EDGE_CURVE('',#7068,#7069,#4263,.T.);
#8657=EDGE_CURVE('',#7070,#7029,#4264,.T.);
#8658=EDGE_CURVE('',#7070,#7058,#6246,.T.);
#8659=EDGE_CURVE('',#7071,#7070,#4265,.T.);
#8660=EDGE_CURVE('',#7059,#7071,#6247,.T.);
#8661=EDGE_CURVE('',#7052,#7071,#4266,.T.);
#8662=EDGE_CURVE('',#7028,#7072,#4267,.T.);
#8663=EDGE_CURVE('',#7072,#7073,#4268,.T.);
#8664=EDGE_CURVE('',#7073,#7053,#4269,.T.);
#8665=EDGE_CURVE('',#7069,#7074,#4270,.T.);
#8666=EDGE_CURVE('',#7074,#7075,#4271,.T.);
#8667=EDGE_CURVE('',#7075,#7076,#4272,.T.);
#8668=EDGE_CURVE('',#7076,#7038,#4273,.T.);
#8669=EDGE_CURVE('',#7077,#7077,#6248,.T.);
#8670=EDGE_CURVE('',#7077,#7047,#4274,.T.);
#8671=EDGE_CURVE('',#7078,#7078,#6249,.T.);
#8672=EDGE_CURVE('',#7078,#7048,#4275,.T.);
#8673=EDGE_CURVE('',#7031,#7079,#4276,.T.);
#8674=EDGE_CURVE('',#7079,#7079,#6250,.T.);
#8675=EDGE_CURVE('',#7032,#7080,#4277,.T.);
#8676=EDGE_CURVE('',#7080,#7080,#6251,.T.);
#8677=EDGE_CURVE('',#7081,#7076,#6252,.T.);
#8678=EDGE_CURVE('',#7039,#7081,#4278,.T.);
#8679=EDGE_CURVE('',#7082,#7075,#6253,.T.);
#8680=EDGE_CURVE('',#7081,#7082,#4279,.T.);
#8681=EDGE_CURVE('',#7083,#7027,#4280,.T.);
#8682=EDGE_CURVE('',#7083,#7072,#6254,.T.);
#8683=EDGE_CURVE('',#7084,#7083,#4281,.T.);
#8684=EDGE_CURVE('',#7073,#7084,#6255,.T.);
#8685=EDGE_CURVE('',#7054,#7084,#4282,.T.);
#8686=EDGE_CURVE('',#7085,#7074,#6256,.T.);
#8687=EDGE_CURVE('',#7082,#7085,#4283,.T.);
#8688=EDGE_CURVE('',#7011,#7086,#4284,.T.);
#8689=EDGE_CURVE('',#7086,#7087,#4285,.T.);
#8690=EDGE_CURVE('',#7088,#7087,#4286,.T.);
#8691=EDGE_CURVE('',#7085,#7088,#4287,.T.);
#8692=EDGE_CURVE('',#7088,#7055,#4288,.T.);
#8693=EDGE_CURVE('',#7040,#7026,#4289,.T.);
#8694=EDGE_CURVE('',#7089,#7089,#6257,.T.);
#8695=EDGE_CURVE('',#7090,#7090,#6258,.T.);
#8696=EDGE_CURVE('',#7091,#7091,#6259,.T.);
#8697=EDGE_CURVE('',#7092,#7092,#6260,.T.);
#8698=EDGE_CURVE('',#7093,#7093,#6261,.T.);
#8699=EDGE_CURVE('',#7012,#7094,#4290,.T.);
#8700=EDGE_CURVE('',#7094,#7094,#6262,.T.);
#8701=EDGE_CURVE('',#7016,#7095,#4291,.T.);
#8702=EDGE_CURVE('',#7095,#7095,#6263,.T.);
#8703=EDGE_CURVE('',#7089,#7096,#4292,.T.);
#8704=EDGE_CURVE('',#7096,#7096,#6264,.T.);
#8705=EDGE_CURVE('',#7093,#7097,#4293,.T.);
#8706=EDGE_CURVE('',#7097,#7097,#6265,.T.);
#8707=EDGE_CURVE('',#7013,#7098,#4294,.T.);
#8708=EDGE_CURVE('',#7098,#7098,#6266,.T.);
#8709=EDGE_CURVE('',#7090,#7099,#4295,.T.);
#8710=EDGE_CURVE('',#7099,#7099,#6267,.T.);
#8711=EDGE_CURVE('',#7091,#7100,#4296,.T.);
#8712=EDGE_CURVE('',#7100,#7100,#6268,.T.);
#8713=EDGE_CURVE('',#7092,#7101,#4297,.T.);
#8714=EDGE_CURVE('',#7101,#7101,#6269,.T.);
#8715=EDGE_CURVE('',#7014,#7102,#4298,.T.);
#8716=EDGE_CURVE('',#7102,#7102,#6270,.T.);
#8717=EDGE_CURVE('',#7015,#7103,#4299,.T.);
#8718=EDGE_CURVE('',#7103,#7103,#6271,.T.);
#8719=EDGE_CURVE('',#7020,#7046,#4300,.T.);
#8720=EDGE_CURVE('',#7021,#7045,#4301,.T.);
#8721=EDGE_CURVE('',#7041,#7025,#4302,.T.);
#8722=EDGE_CURVE('',#7042,#7024,#4303,.T.);
#8723=EDGE_CURVE('',#7043,#7023,#4304,.T.);
#8724=EDGE_CURVE('',#7057,#7086,#4305,.T.);
#8725=EDGE_CURVE('',#7087,#7056,#4306,.T.);
#8726=EDGE_CURVE('',#7022,#7044,#4307,.T.);
#8727=EDGE_CURVE('',#7104,#7104,#6272,.T.);
#8728=EDGE_CURVE('',#7104,#7105,#4308,.T.);
#8729=EDGE_CURVE('',#7105,#7105,#6273,.T.);
#8730=EDGE_CURVE('',#7106,#7106,#6274,.T.);
#8731=EDGE_CURVE('',#7106,#7107,#4309,.T.);
#8732=EDGE_CURVE('',#7107,#7107,#6275,.T.);
#8733=EDGE_CURVE('',#7108,#7108,#6276,.T.);
#8734=EDGE_CURVE('',#7108,#7109,#4310,.T.);
#8735=EDGE_CURVE('',#7109,#7109,#6277,.T.);
#8736=EDGE_CURVE('',#7110,#7110,#6278,.T.);
#8737=EDGE_CURVE('',#7110,#7111,#4311,.T.);
#8738=EDGE_CURVE('',#7111,#7111,#6279,.T.);
#8739=EDGE_CURVE('',#7112,#7113,#4312,.T.);
#8740=EDGE_CURVE('',#7114,#7112,#6280,.T.);
#8741=EDGE_CURVE('',#7115,#7114,#4313,.T.);
#8742=EDGE_CURVE('',#7113,#7115,#6281,.T.);
#8743=EDGE_CURVE('',#7116,#7117,#4314,.T.);
#8744=EDGE_CURVE('',#7118,#7116,#6282,.T.);
#8745=EDGE_CURVE('',#7119,#7118,#4315,.T.);
#8746=EDGE_CURVE('',#7117,#7119,#6283,.T.);
#8747=EDGE_CURVE('',#7120,#7121,#4316,.T.);
#8748=EDGE_CURVE('',#7122,#7120,#6284,.T.);
#8749=EDGE_CURVE('',#7123,#7122,#4317,.T.);
#8750=EDGE_CURVE('',#7121,#7123,#6285,.T.);
#8751=EDGE_CURVE('',#7124,#7125,#4318,.T.);
#8752=EDGE_CURVE('',#7126,#7124,#6286,.T.);
#8753=EDGE_CURVE('',#7127,#7126,#4319,.T.);
#8754=EDGE_CURVE('',#7125,#7127,#6287,.T.);
#8755=EDGE_CURVE('',#7126,#7112,#6288,.T.);
#8756=EDGE_CURVE('',#7122,#7124,#6289,.T.);
#8757=EDGE_CURVE('',#7118,#7120,#6290,.T.);
#8758=EDGE_CURVE('',#7114,#7116,#6291,.T.);
#8759=EDGE_CURVE('',#7128,#7128,#6292,.T.);
#8760=EDGE_CURVE('',#7123,#7125,#6293,.T.);
#8761=EDGE_CURVE('',#7119,#7121,#6294,.T.);
#8762=EDGE_CURVE('',#7127,#7113,#6295,.T.);
#8763=EDGE_CURVE('',#7115,#7117,#6296,.T.);
#8764=EDGE_CURVE('',#7129,#7129,#6297,.T.);
#8765=EDGE_CURVE('',#7129,#7130,#4320,.T.);
#8766=EDGE_CURVE('',#7130,#7130,#6298,.T.);
#8767=EDGE_CURVE('',#7131,#7131,#6299,.T.);
#8768=EDGE_CURVE('',#7131,#7128,#4321,.T.);
#8769=EDGE_CURVE('',#7132,#7133,#4322,.T.);
#8770=EDGE_CURVE('',#7134,#7132,#6300,.T.);
#8771=EDGE_CURVE('',#7135,#7134,#4323,.T.);
#8772=EDGE_CURVE('',#7133,#7135,#6301,.T.);
#8773=EDGE_CURVE('',#7136,#7137,#4324,.T.);
#8774=EDGE_CURVE('',#7138,#7136,#6302,.T.);
#8775=EDGE_CURVE('',#7139,#7138,#4325,.T.);
#8776=EDGE_CURVE('',#7137,#7139,#6303,.T.);
#8777=EDGE_CURVE('',#7140,#7141,#4326,.T.);
#8778=EDGE_CURVE('',#7142,#7140,#6304,.T.);
#8779=EDGE_CURVE('',#7143,#7142,#4327,.T.);
#8780=EDGE_CURVE('',#7141,#7143,#6305,.T.);
#8781=EDGE_CURVE('',#7144,#7145,#4328,.T.);
#8782=EDGE_CURVE('',#7146,#7144,#6306,.T.);
#8783=EDGE_CURVE('',#7147,#7146,#4329,.T.);
#8784=EDGE_CURVE('',#7145,#7147,#6307,.T.);
#8785=EDGE_CURVE('',#7146,#7132,#6308,.T.);
#8786=EDGE_CURVE('',#7142,#7144,#6309,.T.);
#8787=EDGE_CURVE('',#7138,#7140,#6310,.T.);
#8788=EDGE_CURVE('',#7134,#7136,#6311,.T.);
#8789=EDGE_CURVE('',#7148,#7148,#6312,.T.);
#8790=EDGE_CURVE('',#7143,#7145,#6313,.T.);
#8791=EDGE_CURVE('',#7139,#7141,#6314,.T.);
#8792=EDGE_CURVE('',#7147,#7133,#6315,.T.);
#8793=EDGE_CURVE('',#7135,#7137,#6316,.T.);
#8794=EDGE_CURVE('',#7148,#7149,#4330,.T.);
#8795=EDGE_CURVE('',#7149,#7149,#6317,.T.);
#8796=EDGE_CURVE('',#7150,#7150,#6318,.T.);
#8797=EDGE_CURVE('',#7151,#7151,#6319,.T.);
#8798=EDGE_CURVE('',#7151,#7150,#4331,.T.);
#8799=EDGE_CURVE('',#7152,#7152,#6320,.T.);
#8800=EDGE_CURVE('',#7152,#7153,#4332,.T.);
#8801=EDGE_CURVE('',#7153,#7153,#6321,.T.);
#8802=EDGE_CURVE('',#7154,#7154,#6322,.T.);
#8803=EDGE_CURVE('',#7154,#7155,#4333,.T.);
#8804=EDGE_CURVE('',#7155,#7155,#6323,.T.);
#8805=EDGE_CURVE('',#7156,#7156,#6324,.T.);
#8806=EDGE_CURVE('',#7156,#7157,#4334,.T.);
#8807=EDGE_CURVE('',#7157,#7157,#6325,.T.);
#8808=EDGE_CURVE('',#7158,#7158,#6326,.T.);
#8809=EDGE_CURVE('',#7158,#7159,#4335,.T.);
#8810=EDGE_CURVE('',#7159,#7159,#6327,.T.);
#8811=EDGE_CURVE('',#7160,#7160,#6328,.T.);
#8812=EDGE_CURVE('',#7160,#7161,#4336,.T.);
#8813=EDGE_CURVE('',#7161,#7161,#6329,.T.);
#8814=EDGE_CURVE('',#7162,#7162,#6330,.T.);
#8815=EDGE_CURVE('',#7162,#7163,#4337,.T.);
#8816=EDGE_CURVE('',#7163,#7163,#6331,.T.);
#8817=EDGE_CURVE('',#7164,#7164,#6332,.T.);
#8818=EDGE_CURVE('',#7164,#7165,#4338,.T.);
#8819=EDGE_CURVE('',#7165,#7165,#6333,.T.);
#8820=EDGE_CURVE('',#7166,#7166,#6334,.T.);
#8821=EDGE_CURVE('',#7166,#7167,#4339,.T.);
#8822=EDGE_CURVE('',#7167,#7167,#6335,.T.);
#8823=EDGE_CURVE('',#7168,#7168,#6336,.T.);
#8824=EDGE_CURVE('',#7168,#7169,#4340,.T.);
#8825=EDGE_CURVE('',#7169,#7169,#6337,.T.);
#8826=EDGE_CURVE('',#7170,#7170,#6338,.T.);
#8827=EDGE_CURVE('',#7170,#7171,#4341,.T.);
#8828=EDGE_CURVE('',#7171,#7171,#6339,.T.);
#8829=EDGE_CURVE('',#7172,#7172,#6340,.T.);
#8830=EDGE_CURVE('',#7172,#7173,#4342,.T.);
#8831=EDGE_CURVE('',#7173,#7173,#6341,.T.);
#8832=EDGE_CURVE('',#7174,#7174,#6342,.T.);
#8833=EDGE_CURVE('',#7174,#7175,#4343,.T.);
#8834=EDGE_CURVE('',#7175,#7175,#6343,.T.);
#8835=EDGE_CURVE('',#7176,#7176,#6344,.T.);
#8836=EDGE_CURVE('',#7177,#7177,#6345,.T.);
#8837=EDGE_CURVE('',#7177,#7176,#4344,.T.);
#8838=EDGE_CURVE('',#7178,#7178,#6346,.T.);
#8839=EDGE_CURVE('',#7178,#7179,#4345,.T.);
#8840=EDGE_CURVE('',#7179,#7179,#6347,.T.);
#8841=EDGE_CURVE('',#7180,#7180,#6348,.T.);
#8842=EDGE_CURVE('',#7180,#7181,#4346,.T.);
#8843=EDGE_CURVE('',#7181,#7181,#6349,.T.);
#8844=EDGE_CURVE('',#7182,#7182,#6350,.T.);
#8845=EDGE_CURVE('',#7182,#7183,#4347,.T.);
#8846=EDGE_CURVE('',#7183,#7183,#6351,.T.);
#8847=EDGE_CURVE('',#7184,#7184,#6352,.T.);
#8848=EDGE_CURVE('',#7184,#7185,#4348,.T.);
#8849=EDGE_CURVE('',#7185,#7185,#6353,.T.);
#8850=EDGE_CURVE('',#7186,#7186,#6354,.T.);
#8851=EDGE_CURVE('',#7186,#7187,#4349,.T.);
#8852=EDGE_CURVE('',#7187,#7187,#6355,.T.);
#8853=EDGE_CURVE('',#7188,#7188,#6356,.T.);
#8854=EDGE_CURVE('',#7188,#7189,#4350,.T.);
#8855=EDGE_CURVE('',#7189,#7189,#6357,.T.);
#8856=EDGE_CURVE('',#7190,#7190,#6358,.T.);
#8857=EDGE_CURVE('',#7190,#7191,#4351,.T.);
#8858=EDGE_CURVE('',#7191,#7191,#6359,.T.);
#8859=EDGE_CURVE('',#7192,#7192,#6360,.T.);
#8860=EDGE_CURVE('',#7192,#7193,#4352,.T.);
#8861=EDGE_CURVE('',#7193,#7193,#6361,.T.);
#8862=EDGE_CURVE('',#7194,#7194,#6362,.T.);
#8863=EDGE_CURVE('',#7194,#7195,#4353,.T.);
#8864=EDGE_CURVE('',#7195,#7195,#6363,.T.);
#8865=EDGE_CURVE('',#7196,#7196,#6364,.T.);
#8866=EDGE_CURVE('',#7196,#7197,#4354,.T.);
#8867=EDGE_CURVE('',#7197,#7197,#6365,.T.);
#8868=EDGE_CURVE('',#7198,#7198,#6366,.T.);
#8869=EDGE_CURVE('',#7198,#7199,#4355,.T.);
#8870=EDGE_CURVE('',#7199,#7199,#6367,.T.);
#8871=EDGE_CURVE('',#7200,#7200,#6368,.T.);
#8872=EDGE_CURVE('',#7200,#7201,#4356,.T.);
#8873=EDGE_CURVE('',#7201,#7201,#6369,.T.);
#8874=EDGE_CURVE('',#7202,#7202,#6370,.T.);
#8875=EDGE_CURVE('',#7202,#7203,#4357,.T.);
#8876=EDGE_CURVE('',#7203,#7203,#6371,.T.);
#8877=EDGE_CURVE('',#7204,#7204,#6372,.T.);
#8878=EDGE_CURVE('',#7205,#7205,#6373,.T.);
#8879=EDGE_CURVE('',#7205,#7204,#4358,.T.);
#8880=EDGE_CURVE('',#7206,#7206,#6374,.T.);
#8881=EDGE_CURVE('',#7206,#7207,#4359,.T.);
#8882=EDGE_CURVE('',#7207,#7207,#6375,.T.);
#8883=EDGE_CURVE('',#7208,#7208,#6376,.T.);
#8884=EDGE_CURVE('',#7208,#7209,#4360,.T.);
#8885=EDGE_CURVE('',#7209,#7209,#6377,.T.);
#8886=EDGE_CURVE('',#7210,#7210,#6378,.T.);
#8887=EDGE_CURVE('',#7210,#7211,#4361,.T.);
#8888=EDGE_CURVE('',#7211,#7211,#6379,.T.);
#8889=EDGE_CURVE('',#7212,#7212,#6380,.T.);
#8890=EDGE_CURVE('',#7212,#7213,#4362,.T.);
#8891=EDGE_CURVE('',#7213,#7213,#6381,.T.);
#8892=EDGE_CURVE('',#7214,#7214,#6382,.T.);
#8893=EDGE_CURVE('',#7214,#7215,#4363,.T.);
#8894=EDGE_CURVE('',#7215,#7215,#6383,.T.);
#8895=EDGE_CURVE('',#7216,#7217,#4364,.T.);
#8896=EDGE_CURVE('',#7217,#7218,#4365,.T.);
#8897=EDGE_CURVE('',#7219,#7218,#4366,.T.);
#8898=EDGE_CURVE('',#7216,#7219,#4367,.T.);
#8899=EDGE_CURVE('',#7220,#7216,#4368,.T.);
#8900=EDGE_CURVE('',#7221,#7219,#4369,.T.);
#8901=EDGE_CURVE('',#7220,#7221,#4370,.T.);
#8902=EDGE_CURVE('',#7222,#7220,#4371,.T.);
#8903=EDGE_CURVE('',#7223,#7221,#4372,.T.);
#8904=EDGE_CURVE('',#7222,#7223,#4373,.T.);
#8905=EDGE_CURVE('',#7217,#7222,#4374,.T.);
#8906=EDGE_CURVE('',#7218,#7223,#4375,.T.);
#8907=EDGE_CURVE('',#7224,#7225,#4376,.T.);
#8908=EDGE_CURVE('',#7225,#7226,#4377,.T.);
#8909=EDGE_CURVE('',#7227,#7226,#4378,.T.);
#8910=EDGE_CURVE('',#7224,#7227,#4379,.T.);
#8911=EDGE_CURVE('',#7228,#7224,#4380,.T.);
#8912=EDGE_CURVE('',#7229,#7227,#4381,.T.);
#8913=EDGE_CURVE('',#7228,#7229,#4382,.T.);
#8914=EDGE_CURVE('',#7230,#7228,#4383,.T.);
#8915=EDGE_CURVE('',#7231,#7229,#4384,.T.);
#8916=EDGE_CURVE('',#7230,#7231,#4385,.T.);
#8917=EDGE_CURVE('',#7225,#7230,#4386,.T.);
#8918=EDGE_CURVE('',#7226,#7231,#4387,.T.);
#8919=EDGE_CURVE('',#7232,#7233,#4388,.T.);
#8920=EDGE_CURVE('',#7233,#7234,#4389,.T.);
#8921=EDGE_CURVE('',#7235,#7234,#4390,.T.);
#8922=EDGE_CURVE('',#7232,#7235,#4391,.T.);
#8923=EDGE_CURVE('',#7236,#7232,#4392,.T.);
#8924=EDGE_CURVE('',#7237,#7235,#4393,.T.);
#8925=EDGE_CURVE('',#7236,#7237,#4394,.T.);
#8926=EDGE_CURVE('',#7238,#7236,#4395,.T.);
#8927=EDGE_CURVE('',#7239,#7237,#4396,.T.);
#8928=EDGE_CURVE('',#7238,#7239,#4397,.T.);
#8929=EDGE_CURVE('',#7233,#7238,#4398,.T.);
#8930=EDGE_CURVE('',#7234,#7239,#4399,.T.);
#8931=EDGE_CURVE('',#7240,#7241,#4400,.T.);
#8932=EDGE_CURVE('',#7241,#7242,#4401,.T.);
#8933=EDGE_CURVE('',#7242,#7243,#4402,.T.);
#8934=EDGE_CURVE('',#7240,#7243,#4403,.T.);
#8935=EDGE_CURVE('',#7241,#7244,#4404,.T.);
#8936=EDGE_CURVE('',#7244,#7245,#4405,.T.);
#8937=EDGE_CURVE('',#7245,#7242,#4406,.T.);
#8938=EDGE_CURVE('',#7244,#7246,#4407,.T.);
#8939=EDGE_CURVE('',#7246,#7247,#4408,.T.);
#8940=EDGE_CURVE('',#7247,#7245,#4409,.T.);
#8941=EDGE_CURVE('',#7246,#7248,#4410,.T.);
#8942=EDGE_CURVE('',#7248,#7249,#4411,.T.);
#8943=EDGE_CURVE('',#7249,#7247,#4412,.T.);
#8944=EDGE_CURVE('',#7248,#7250,#4413,.T.);
#8945=EDGE_CURVE('',#7250,#7251,#4414,.T.);
#8946=EDGE_CURVE('',#7251,#7249,#4415,.T.);
#8947=EDGE_CURVE('',#7250,#7240,#4416,.T.);
#8948=EDGE_CURVE('',#7243,#7251,#4417,.T.);
#8949=EDGE_CURVE('',#7252,#7252,#6384,.T.);
#8950=EDGE_CURVE('',#7253,#7253,#6385,.T.);
#8951=EDGE_CURVE('',#7254,#7254,#6386,.T.);
#8952=EDGE_CURVE('',#7254,#7253,#4418,.T.);
#8953=EDGE_CURVE('',#7255,#7255,#6387,.T.);
#8954=EDGE_CURVE('',#7255,#7254,#4419,.T.);
#8955=EDGE_CURVE('',#7256,#7256,#6388,.T.);
#8956=EDGE_CURVE('',#7256,#7255,#4420,.T.);
#8957=EDGE_CURVE('',#7257,#7257,#6389,.T.);
#8958=EDGE_CURVE('',#7258,#7258,#6390,.F.);
#8959=EDGE_CURVE('',#7258,#7257,#4421,.T.);
#8960=EDGE_CURVE('',#7252,#7258,#4422,.T.);
#8961=EDGE_CURVE('',#7259,#7260,#6391,.T.);
#8962=EDGE_CURVE('',#7260,#7259,#6392,.T.);
#8963=EDGE_CURVE('',#7260,#7261,#6393,.T.);
#8964=EDGE_CURVE('',#7262,#7261,#6394,.T.);
#8965=EDGE_CURVE('',#7261,#7262,#6395,.T.);
#8966=EDGE_CURVE('',#7262,#7263,#4423,.T.);
#8967=EDGE_CURVE('',#7263,#7263,#6396,.T.);
#8968=EDGE_CURVE('',#7264,#7264,#6397,.T.);
#8969=EDGE_CURVE('',#7264,#7265,#4424,.T.);
#8970=EDGE_CURVE('',#7265,#7265,#6398,.T.);
#8971=EDGE_CURVE('',#7265,#7266,#4425,.T.);
#8972=EDGE_CURVE('',#7266,#7266,#6399,.T.);
#8973=EDGE_CURVE('',#7267,#7267,#6400,.T.);
#8974=EDGE_CURVE('',#7267,#7259,#4426,.T.);
#8975=EDGE_CURVE('',#7268,#7268,#6401,.T.);
#8976=EDGE_CURVE('',#7268,#7264,#4427,.T.);
#8977=EDGE_CURVE('',#7269,#7270,#6402,.T.);
#8978=EDGE_CURVE('',#7270,#7269,#6403,.T.);
#8979=EDGE_CURVE('',#7270,#7271,#6404,.T.);
#8980=EDGE_CURVE('',#7272,#7271,#6405,.T.);
#8981=EDGE_CURVE('',#7271,#7272,#6406,.T.);
#8982=EDGE_CURVE('',#7273,#7273,#6407,.T.);
#8983=EDGE_CURVE('',#7273,#7272,#4428,.T.);
#8984=EDGE_CURVE('',#7274,#7274,#6408,.T.);
#8985=EDGE_CURVE('',#7275,#7275,#6409,.T.);
#8986=EDGE_CURVE('',#7276,#7276,#6410,.T.);
#8987=EDGE_CURVE('',#7276,#7274,#4429,.T.);
#8988=EDGE_CURVE('',#7277,#7277,#6411,.T.);
#8989=EDGE_CURVE('',#7277,#7276,#4430,.T.);
#8990=EDGE_CURVE('',#7278,#7278,#6412,.T.);
#8991=EDGE_CURVE('',#7278,#7277,#4431,.T.);
#8992=EDGE_CURVE('',#7269,#7275,#4432,.T.);
#8993=EDGE_CURVE('',#7279,#7280,#6413,.T.);
#8994=EDGE_CURVE('',#7281,#7282,#6414,.T.);
#8995=EDGE_CURVE('',#7283,#7284,#6415,.T.);
#8996=EDGE_CURVE('',#7285,#7286,#6416,.T.);
#8997=EDGE_CURVE('',#7287,#7288,#6417,.T.);
#8998=EDGE_CURVE('',#7289,#7290,#6418,.T.);
#8999=EDGE_CURVE('',#7291,#7292,#6419,.T.);
#9000=EDGE_CURVE('',#7293,#7294,#931,.T.);
#9001=EDGE_CURVE('',#7295,#7293,#6420,.T.);
#9002=EDGE_CURVE('',#7296,#7295,#932,.T.);
#9003=EDGE_CURVE('',#7294,#7296,#6421,.T.);
#9004=EDGE_CURVE('',#7297,#7295,#6422,.T.);
#9005=EDGE_CURVE('',#7297,#7298,#933,.T.);
#9006=EDGE_CURVE('',#7299,#7298,#6423,.T.);
#9007=EDGE_CURVE('',#7299,#7300,#934,.T.);
#9008=EDGE_CURVE('',#7301,#7300,#6424,.T.);
#9009=EDGE_CURVE('',#7301,#7302,#4433,.T.);
#9010=EDGE_CURVE('',#7302,#7302,#6425,.T.);
#9011=EDGE_CURVE('',#7303,#7301,#6426,.T.);
#9012=EDGE_CURVE('',#7303,#7304,#935,.T.);
#9013=EDGE_CURVE('',#7305,#7304,#6427,.T.);
#9014=EDGE_CURVE('',#7305,#7306,#936,.T.);
#9015=EDGE_CURVE('',#7307,#7306,#6428,.T.);
#9016=EDGE_CURVE('',#7307,#7308,#937,.T.);
#9017=EDGE_CURVE('',#7309,#7308,#6429,.T.);
#9018=EDGE_CURVE('',#7309,#7310,#938,.T.);
#9019=EDGE_CURVE('',#7296,#7310,#6430,.T.);
#9020=EDGE_CURVE('',#7293,#7311,#6431,.T.);
#9021=EDGE_CURVE('',#7311,#7297,#6432,.T.);
#9022=EDGE_CURVE('',#7312,#7311,#939,.T.);
#9023=EDGE_CURVE('',#7298,#7312,#6433,.T.);
#9024=EDGE_CURVE('',#7312,#7313,#6434,.T.);
#9025=EDGE_CURVE('',#7313,#7299,#6435,.T.);
#9026=EDGE_CURVE('',#7314,#7313,#940,.T.);
#9027=EDGE_CURVE('',#7300,#7314,#6436,.T.);
#9028=EDGE_CURVE('',#7314,#7315,#6437,.T.);
#9029=EDGE_CURVE('',#7315,#7316,#6438,.T.);
#9030=EDGE_CURVE('',#7316,#7303,#6439,.T.);
#9031=EDGE_CURVE('',#7317,#7316,#941,.T.);
#9032=EDGE_CURVE('',#7304,#7317,#6440,.T.);
#9033=EDGE_CURVE('',#7317,#7318,#6441,.T.);
#9034=EDGE_CURVE('',#7318,#7305,#6442,.T.);
#9035=EDGE_CURVE('',#7319,#7318,#942,.T.);
#9036=EDGE_CURVE('',#7306,#7319,#6443,.T.);
#9037=EDGE_CURVE('',#7319,#7320,#6444,.T.);
#9038=EDGE_CURVE('',#7320,#7307,#6445,.T.);
#9039=EDGE_CURVE('',#7321,#7320,#943,.T.);
#9040=EDGE_CURVE('',#7308,#7321,#6446,.T.);
#9041=EDGE_CURVE('',#7322,#7322,#6447,.T.);
#9042=EDGE_CURVE('',#7322,#7315,#4434,.T.);
#9043=EDGE_CURVE('',#7323,#7294,#6448,.T.);
#9044=EDGE_CURVE('',#7323,#7324,#944,.T.);
#9045=EDGE_CURVE('',#7321,#7324,#6449,.T.);
#9046=EDGE_CURVE('',#7310,#7323,#6450,.T.);
#9047=EDGE_CURVE('',#7324,#7309,#6451,.T.);
#9048=EDGE_CURVE('',#7325,#7325,#6452,.T.);
#9049=EDGE_CURVE('',#7326,#7326,#6453,.T.);
#9050=EDGE_CURVE('',#7327,#7327,#6454,.T.);
#9051=EDGE_CURVE('',#7327,#7325,#4435,.T.);
#9052=EDGE_CURVE('',#7328,#7328,#6455,.T.);
#9053=EDGE_CURVE('',#7328,#7326,#4436,.T.);
#9054=EDGE_CURVE('',#7329,#7329,#6456,.T.);
#9055=EDGE_CURVE('',#7330,#7330,#6457,.T.);
#9056=EDGE_CURVE('',#7331,#7331,#6458,.T.);
#9057=EDGE_CURVE('',#7331,#7329,#4437,.T.);
#9058=EDGE_CURVE('',#7332,#7332,#6459,.T.);
#9059=EDGE_CURVE('',#7332,#7330,#4438,.T.);
#9060=EDGE_CURVE('',#7333,#7334,#6460,.T.);
#9061=EDGE_CURVE('',#7334,#7333,#6461,.T.);
#9062=EDGE_CURVE('',#7334,#7335,#6462,.T.);
#9063=EDGE_CURVE('',#7336,#7335,#6463,.T.);
#9064=EDGE_CURVE('',#7335,#7336,#6464,.T.);
#9065=EDGE_CURVE('',#7336,#7337,#4439,.T.);
#9066=EDGE_CURVE('',#7337,#7337,#6465,.T.);
#9067=EDGE_CURVE('',#7338,#7338,#6466,.T.);
#9068=EDGE_CURVE('',#7338,#7339,#4440,.T.);
#9069=EDGE_CURVE('',#7339,#7339,#6467,.T.);
#9070=EDGE_CURVE('',#7339,#7340,#4441,.T.);
#9071=EDGE_CURVE('',#7340,#7340,#6468,.T.);
#9072=EDGE_CURVE('',#7341,#7341,#6469,.T.);
#9073=EDGE_CURVE('',#7341,#7333,#4442,.T.);
#9074=EDGE_CURVE('',#7342,#7342,#6470,.T.);
#9075=EDGE_CURVE('',#7342,#7338,#4443,.T.);
#9076=EDGE_CURVE('',#7343,#7344,#6471,.T.);
#9077=EDGE_CURVE('',#7344,#7343,#6472,.T.);
#9078=EDGE_CURVE('',#7344,#7345,#6473,.T.);
#9079=EDGE_CURVE('',#7346,#7345,#6474,.T.);
#9080=EDGE_CURVE('',#7345,#7346,#6475,.T.);
#9081=EDGE_CURVE('',#7347,#7347,#6476,.T.);
#9082=EDGE_CURVE('',#7347,#7346,#4444,.T.);
#9083=EDGE_CURVE('',#7348,#7348,#6477,.T.);
#9084=EDGE_CURVE('',#7349,#7349,#6478,.T.);
#9085=EDGE_CURVE('',#7350,#7350,#6479,.T.);
#9086=EDGE_CURVE('',#7350,#7348,#4445,.T.);
#9087=EDGE_CURVE('',#7351,#7351,#6480,.T.);
#9088=EDGE_CURVE('',#7351,#7350,#4446,.T.);
#9089=EDGE_CURVE('',#7352,#7352,#6481,.T.);
#9090=EDGE_CURVE('',#7352,#7351,#4447,.T.);
#9091=EDGE_CURVE('',#7343,#7349,#4448,.T.);
#9092=EDGE_CURVE('',#7353,#7354,#6482,.T.);
#9093=EDGE_CURVE('',#7355,#7356,#6483,.T.);
#9094=EDGE_CURVE('',#7357,#7358,#6484,.T.);
#9095=EDGE_CURVE('',#7359,#7360,#6485,.T.);
#9096=EDGE_CURVE('',#7361,#7362,#6486,.T.);
#9097=EDGE_CURVE('',#7363,#7364,#6487,.T.);
#9098=EDGE_CURVE('',#7365,#7366,#6488,.T.);
#9099=EDGE_CURVE('',#7367,#7368,#6489,.T.);
#9100=EDGE_CURVE('',#7369,#7370,#945,.T.);
#9101=EDGE_CURVE('',#7371,#7369,#6490,.T.);
#9102=EDGE_CURVE('',#7372,#7371,#946,.T.);
#9103=EDGE_CURVE('',#7370,#7372,#6491,.T.);
#9104=EDGE_CURVE('',#7373,#7371,#6492,.T.);
#9105=EDGE_CURVE('',#7373,#7374,#947,.T.);
#9106=EDGE_CURVE('',#7375,#7374,#6493,.T.);
#9107=EDGE_CURVE('',#7375,#7376,#948,.T.);
#9108=EDGE_CURVE('',#7377,#7376,#6494,.T.);
#9109=EDGE_CURVE('',#7377,#7378,#949,.T.);
#9110=EDGE_CURVE('',#7378,#7379,#4449,.T.);
#9111=EDGE_CURVE('',#7379,#7379,#6495,.T.);
#9112=EDGE_CURVE('',#7378,#7380,#950,.T.);
#9113=EDGE_CURVE('',#7381,#7380,#6496,.T.);
#9114=EDGE_CURVE('',#7381,#7382,#951,.T.);
#9115=EDGE_CURVE('',#7383,#7382,#6497,.T.);
#9116=EDGE_CURVE('',#7383,#7384,#952,.T.);
#9117=EDGE_CURVE('',#7385,#7384,#6498,.T.);
#9118=EDGE_CURVE('',#7385,#7386,#953,.T.);
#9119=EDGE_CURVE('',#7387,#7386,#6499,.T.);
#9120=EDGE_CURVE('',#7387,#7388,#954,.T.);
#9121=EDGE_CURVE('',#7372,#7388,#6500,.T.);
#9122=EDGE_CURVE('',#7369,#7389,#6501,.T.);
#9123=EDGE_CURVE('',#7389,#7373,#6502,.T.);
#9124=EDGE_CURVE('',#7390,#7389,#955,.T.);
#9125=EDGE_CURVE('',#7374,#7390,#6503,.T.);
#9126=EDGE_CURVE('',#7390,#7391,#6504,.T.);
#9127=EDGE_CURVE('',#7391,#7375,#6505,.T.);
#9128=EDGE_CURVE('',#7392,#7391,#956,.T.);
#9129=EDGE_CURVE('',#7376,#7392,#6506,.T.);
#9130=EDGE_CURVE('',#7392,#7393,#6507,.T.);
#9131=EDGE_CURVE('',#7393,#7377,#6508,.T.);
#9132=EDGE_CURVE('',#7394,#7395,#957,.T.);
#9133=EDGE_CURVE('',#7380,#7394,#6509,.T.);
#9134=EDGE_CURVE('',#7395,#7393,#958,.T.);
#9135=EDGE_CURVE('',#7394,#7396,#6510,.T.);
#9136=EDGE_CURVE('',#7396,#7381,#6511,.T.);
#9137=EDGE_CURVE('',#7397,#7396,#959,.T.);
#9138=EDGE_CURVE('',#7382,#7397,#6512,.T.);
#9139=EDGE_CURVE('',#7397,#7398,#6513,.T.);
#9140=EDGE_CURVE('',#7398,#7383,#6514,.T.);
#9141=EDGE_CURVE('',#7399,#7398,#960,.T.);
#9142=EDGE_CURVE('',#7384,#7399,#6515,.T.);
#9143=EDGE_CURVE('',#7399,#7400,#6516,.T.);
#9144=EDGE_CURVE('',#7400,#7385,#6517,.T.);
#9145=EDGE_CURVE('',#7401,#7400,#961,.T.);
#9146=EDGE_CURVE('',#7386,#7401,#6518,.T.);
#9147=EDGE_CURVE('',#7402,#7402,#6519,.T.);
#9148=EDGE_CURVE('',#7402,#7395,#4450,.T.);
#9149=EDGE_CURVE('',#7403,#7370,#6520,.T.);
#9150=EDGE_CURVE('',#7403,#7404,#962,.T.);
#9151=EDGE_CURVE('',#7401,#7404,#6521,.T.);
#9152=EDGE_CURVE('',#7388,#7403,#6522,.T.);
#9153=EDGE_CURVE('',#7404,#7387,#6523,.T.);
#9154=EDGE_CURVE('',#7405,#7405,#6524,.T.);
#9155=EDGE_CURVE('',#7406,#7406,#6525,.T.);
#9156=EDGE_CURVE('',#7407,#7407,#6526,.T.);
#9157=EDGE_CURVE('',#7407,#7405,#4451,.T.);
#9158=EDGE_CURVE('',#7408,#7408,#6527,.T.);
#9159=EDGE_CURVE('',#7408,#7406,#4452,.T.);
#9160=EDGE_CURVE('',#7409,#7409,#6528,.T.);
#9161=EDGE_CURVE('',#7410,#7410,#6529,.T.);
#9162=EDGE_CURVE('',#7411,#7411,#6530,.T.);
#9163=EDGE_CURVE('',#7411,#7409,#4453,.T.);
#9164=EDGE_CURVE('',#7412,#7412,#6531,.T.);
#9165=EDGE_CURVE('',#7412,#7410,#4454,.T.);
#9166=EDGE_CURVE('',#7413,#7413,#6532,.T.);
#9167=EDGE_CURVE('',#7414,#7414,#6533,.T.);
#9168=EDGE_CURVE('',#7414,#7413,#4455,.T.);
#9169=EDGE_CURVE('',#7415,#7415,#6534,.T.);
#9170=EDGE_CURVE('',#7415,#7414,#4456,.T.);
#9171=EDGE_CURVE('',#7416,#7416,#6535,.T.);
#9172=EDGE_CURVE('',#7416,#7415,#4457,.T.);
#9173=EDGE_CURVE('',#7417,#7417,#6536,.T.);
#9174=EDGE_CURVE('',#7418,#7418,#6537,.F.);
#9175=EDGE_CURVE('',#7418,#7417,#4458,.T.);
#9176=EDGE_CURVE('',#7419,#7419,#6538,.F.);
#9177=EDGE_CURVE('',#7419,#7418,#4459,.T.);
#9178=EDGE_CURVE('',#7420,#7420,#6539,.T.);
#9179=EDGE_CURVE('',#7420,#7419,#4460,.T.);
#9180=EDGE_CURVE('',#7421,#7422,#4461,.T.);
#9181=EDGE_CURVE('',#7422,#7423,#4462,.T.);
#9182=EDGE_CURVE('',#7423,#7424,#4463,.T.);
#9183=EDGE_CURVE('',#7421,#7424,#4464,.T.);
#9184=EDGE_CURVE('',#7422,#7425,#4465,.T.);
#9185=EDGE_CURVE('',#7425,#7426,#4466,.T.);
#9186=EDGE_CURVE('',#7426,#7423,#4467,.T.);
#9187=EDGE_CURVE('',#7425,#7427,#4468,.T.);
#9188=EDGE_CURVE('',#7427,#7428,#4469,.T.);
#9189=EDGE_CURVE('',#7428,#7426,#4470,.T.);
#9190=EDGE_CURVE('',#7427,#7429,#4471,.T.);
#9191=EDGE_CURVE('',#7429,#7430,#4472,.T.);
#9192=EDGE_CURVE('',#7430,#7428,#4473,.T.);
#9193=EDGE_CURVE('',#7429,#7431,#4474,.T.);
#9194=EDGE_CURVE('',#7431,#7432,#4475,.T.);
#9195=EDGE_CURVE('',#7432,#7430,#4476,.T.);
#9196=EDGE_CURVE('',#7431,#7421,#4477,.T.);
#9197=EDGE_CURVE('',#7424,#7432,#4478,.T.);
#9198=EDGE_CURVE('',#7433,#7434,#4479,.T.);
#9199=EDGE_CURVE('',#7433,#7435,#4480,.T.);
#9200=EDGE_CURVE('',#7436,#7435,#4481,.T.);
#9201=EDGE_CURVE('',#7436,#7434,#4482,.T.);
#9202=EDGE_CURVE('',#7434,#7437,#6540,.T.);
#9203=EDGE_CURVE('',#7438,#7436,#4483,.T.);
#9204=EDGE_CURVE('',#7437,#7438,#4484,.T.);
#9205=EDGE_CURVE('',#7437,#7439,#4485,.T.);
#9206=EDGE_CURVE('',#7438,#7440,#4486,.T.);
#9207=EDGE_CURVE('',#7440,#7439,#4487,.T.);
#9208=EDGE_CURVE('',#7435,#7440,#4488,.T.);
#9209=EDGE_CURVE('',#7439,#7433,#6541,.T.);
#9210=EDGE_CURVE('',#7441,#7441,#6542,.T.);
#9211=EDGE_CURVE('',#7441,#7442,#4489,.T.);
#9212=EDGE_CURVE('',#7442,#7442,#6543,.T.);
#9213=EDGE_CURVE('',#7443,#7444,#4490,.T.);
#9214=EDGE_CURVE('',#7443,#7444,#6544,.T.);
#9215=EDGE_CURVE('',#7445,#7443,#963,.T.);
#9216=EDGE_CURVE('',#7446,#7445,#6545,.T.);
#9217=EDGE_CURVE('',#7446,#7447,#4491,.T.);
#9218=EDGE_CURVE('',#7448,#7447,#964,.T.);
#9219=EDGE_CURVE('',#7447,#7448,#965,.T.);
#9220=EDGE_CURVE('',#7449,#7446,#6546,.T.);
#9221=EDGE_CURVE('',#7444,#7449,#966,.T.);
#9222=EDGE_CURVE('',#7449,#7445,#4492,.T.);
#9223=EDGE_CURVE('',#7450,#7450,#6547,.T.);
#9224=EDGE_CURVE('',#7450,#7451,#4493,.T.);
#9225=EDGE_CURVE('',#7451,#7451,#6548,.T.);
#9226=EDGE_CURVE('',#7452,#7452,#6549,.T.);
#9227=EDGE_CURVE('',#7452,#7453,#4494,.T.);
#9228=EDGE_CURVE('',#7453,#7453,#6550,.T.);
#9229=EDGE_CURVE('',#7454,#7455,#4495,.T.);
#9230=EDGE_CURVE('',#7454,#7455,#6551,.T.);
#9231=EDGE_CURVE('',#7456,#7454,#967,.T.);
#9232=EDGE_CURVE('',#7457,#7456,#6552,.T.);
#9233=EDGE_CURVE('',#7457,#7458,#4496,.T.);
#9234=EDGE_CURVE('',#7459,#7458,#968,.T.);
#9235=EDGE_CURVE('',#7458,#7459,#969,.T.);
#9236=EDGE_CURVE('',#7460,#7457,#6553,.T.);
#9237=EDGE_CURVE('',#7455,#7460,#970,.T.);
#9238=EDGE_CURVE('',#7460,#7456,#4497,.T.);
#9239=EDGE_CURVE('',#7461,#7461,#6554,.T.);
#9240=EDGE_CURVE('',#7461,#7462,#4498,.T.);
#9241=EDGE_CURVE('',#7462,#7462,#6555,.T.);
#9242=EDGE_CURVE('',#7463,#7463,#6556,.T.);
#9243=EDGE_CURVE('',#7463,#7464,#4499,.T.);
#9244=EDGE_CURVE('',#7464,#7464,#6557,.T.);
#9245=EDGE_CURVE('',#7465,#7465,#6558,.T.);
#9246=EDGE_CURVE('',#7465,#7466,#4500,.T.);
#9247=EDGE_CURVE('',#7466,#7466,#6559,.T.);
#9248=EDGE_CURVE('',#7467,#7467,#6560,.T.);
#9249=EDGE_CURVE('',#7467,#7468,#4501,.T.);
#9250=EDGE_CURVE('',#7468,#7468,#6561,.T.);
#9251=EDGE_CURVE('',#7469,#7469,#6562,.T.);
#9252=EDGE_CURVE('',#7469,#7470,#4502,.T.);
#9253=EDGE_CURVE('',#7470,#7470,#6563,.T.);
#9254=EDGE_CURVE('',#7471,#7471,#6564,.T.);
#9255=EDGE_CURVE('',#7471,#7472,#4503,.T.);
#9256=EDGE_CURVE('',#7472,#7472,#6565,.T.);
#9257=EDGE_CURVE('',#7473,#7473,#6566,.T.);
#9258=EDGE_CURVE('',#7473,#7474,#4504,.T.);
#9259=EDGE_CURVE('',#7474,#7474,#6567,.T.);
#9260=EDGE_CURVE('',#7475,#7475,#6568,.T.);
#9261=EDGE_CURVE('',#7475,#7476,#4505,.T.);
#9262=EDGE_CURVE('',#7476,#7476,#6569,.T.);
#9263=EDGE_CURVE('',#7477,#7477,#6570,.T.);
#9264=EDGE_CURVE('',#7477,#7478,#4506,.T.);
#9265=EDGE_CURVE('',#7478,#7478,#6571,.T.);
#9266=EDGE_CURVE('',#7479,#7479,#6572,.T.);
#9267=EDGE_CURVE('',#7479,#7480,#4507,.T.);
#9268=EDGE_CURVE('',#7480,#7480,#6573,.T.);
#9269=EDGE_CURVE('',#7481,#7482,#4508,.T.);
#9270=EDGE_CURVE('',#7483,#7481,#4509,.T.);
#9271=EDGE_CURVE('',#7484,#7483,#4510,.T.);
#9272=EDGE_CURVE('',#7482,#7484,#4511,.T.);
#9273=EDGE_CURVE('',#7485,#7481,#4512,.T.);
#9274=EDGE_CURVE('',#7485,#7486,#4513,.T.);
#9275=EDGE_CURVE('',#7483,#7486,#4514,.T.);
#9276=EDGE_CURVE('',#7487,#7485,#4515,.T.);
#9277=EDGE_CURVE('',#7488,#7487,#4516,.T.);
#9278=EDGE_CURVE('',#7486,#7488,#4517,.T.);
#9279=EDGE_CURVE('',#7489,#7490,#6574,.T.);
#9280=EDGE_CURVE('',#7490,#7491,#171,.T.);
#9281=EDGE_CURVE('',#7491,#7492,#4518,.T.);
#9282=EDGE_CURVE('',#7492,#7493,#172,.T.);
#9283=EDGE_CURVE('',#7493,#7494,#6575,.T.);
#9284=EDGE_CURVE('',#7494,#7495,#173,.T.);
#9285=EDGE_CURVE('',#7495,#7496,#4519,.T.);
#9286=EDGE_CURVE('',#7496,#7497,#174,.T.);
#9287=EDGE_CURVE('',#7497,#7498,#6576,.T.);
#9288=EDGE_CURVE('',#7498,#7499,#175,.T.);
#9289=EDGE_CURVE('',#7499,#7500,#4520,.T.);
#9290=EDGE_CURVE('',#7500,#7501,#176,.T.);
#9291=EDGE_CURVE('',#7501,#7502,#6577,.T.);
#9292=EDGE_CURVE('',#7502,#7503,#177,.T.);
#9293=EDGE_CURVE('',#7503,#7504,#4521,.T.);
#9294=EDGE_CURVE('',#7504,#7505,#178,.T.);
#9295=EDGE_CURVE('',#7505,#7506,#6578,.T.);
#9296=EDGE_CURVE('',#7506,#7507,#179,.T.);
#9297=EDGE_CURVE('',#7507,#7508,#4522,.T.);
#9298=EDGE_CURVE('',#7508,#7509,#180,.T.);
#9299=EDGE_CURVE('',#7509,#7510,#6579,.T.);
#9300=EDGE_CURVE('',#7510,#7511,#181,.T.);
#9301=EDGE_CURVE('',#7511,#7512,#4523,.T.);
#9302=EDGE_CURVE('',#7512,#7513,#182,.T.);
#9303=EDGE_CURVE('',#7513,#7514,#6580,.T.);
#9304=EDGE_CURVE('',#7514,#7515,#183,.T.);
#9305=EDGE_CURVE('',#7515,#7516,#4524,.T.);
#9306=EDGE_CURVE('',#7516,#7517,#184,.T.);
#9307=EDGE_CURVE('',#7517,#7518,#6581,.T.);
#9308=EDGE_CURVE('',#7518,#7519,#185,.T.);
#9309=EDGE_CURVE('',#7519,#7520,#4525,.T.);
#9310=EDGE_CURVE('',#7520,#7521,#186,.T.);
#9311=EDGE_CURVE('',#7521,#7522,#6582,.T.);
#9312=EDGE_CURVE('',#7522,#7523,#187,.T.);
#9313=EDGE_CURVE('',#7523,#7524,#4526,.T.);
#9314=EDGE_CURVE('',#7524,#7525,#188,.T.);
#9315=EDGE_CURVE('',#7525,#7526,#6583,.T.);
#9316=EDGE_CURVE('',#7526,#7527,#189,.T.);
#9317=EDGE_CURVE('',#7527,#7528,#4527,.T.);
#9318=EDGE_CURVE('',#7528,#7529,#190,.T.);
#9319=EDGE_CURVE('',#7529,#7530,#6584,.T.);
#9320=EDGE_CURVE('',#7530,#7531,#191,.T.);
#9321=EDGE_CURVE('',#7531,#7532,#4528,.T.);
#9322=EDGE_CURVE('',#7532,#7533,#192,.T.);
#9323=EDGE_CURVE('',#7533,#7534,#6585,.T.);
#9324=EDGE_CURVE('',#7534,#7535,#193,.T.);
#9325=EDGE_CURVE('',#7535,#7536,#4529,.T.);
#9326=EDGE_CURVE('',#7536,#7537,#194,.T.);
#9327=EDGE_CURVE('',#7537,#7538,#6586,.T.);
#9328=EDGE_CURVE('',#7538,#7539,#195,.T.);
#9329=EDGE_CURVE('',#7539,#7540,#4530,.T.);
#9330=EDGE_CURVE('',#7540,#7541,#196,.T.);
#9331=EDGE_CURVE('',#7541,#7542,#6587,.T.);
#9332=EDGE_CURVE('',#7542,#7543,#197,.T.);
#9333=EDGE_CURVE('',#7543,#7544,#4531,.T.);
#9334=EDGE_CURVE('',#7544,#7545,#198,.T.);
#9335=EDGE_CURVE('',#7545,#7546,#6588,.T.);
#9336=EDGE_CURVE('',#7546,#7547,#199,.T.);
#9337=EDGE_CURVE('',#7547,#7548,#4532,.T.);
#9338=EDGE_CURVE('',#7548,#7549,#200,.T.);
#9339=EDGE_CURVE('',#7549,#7550,#6589,.T.);
#9340=EDGE_CURVE('',#7550,#7551,#201,.T.);
#9341=EDGE_CURVE('',#7551,#7552,#4533,.T.);
#9342=EDGE_CURVE('',#7552,#7553,#202,.T.);
#9343=EDGE_CURVE('',#7553,#7554,#6590,.T.);
#9344=EDGE_CURVE('',#7554,#7555,#203,.T.);
#9345=EDGE_CURVE('',#7555,#7556,#4534,.T.);
#9346=EDGE_CURVE('',#7556,#7557,#204,.T.);
#9347=EDGE_CURVE('',#7557,#7558,#6591,.T.);
#9348=EDGE_CURVE('',#7558,#7559,#205,.T.);
#9349=EDGE_CURVE('',#7559,#7560,#4535,.T.);
#9350=EDGE_CURVE('',#7560,#7561,#206,.T.);
#9351=EDGE_CURVE('',#7561,#7562,#6592,.T.);
#9352=EDGE_CURVE('',#7562,#7563,#207,.T.);
#9353=EDGE_CURVE('',#7563,#7564,#4536,.T.);
#9354=EDGE_CURVE('',#7564,#7565,#208,.T.);
#9355=EDGE_CURVE('',#7565,#7566,#6593,.T.);
#9356=EDGE_CURVE('',#7566,#7567,#209,.T.);
#9357=EDGE_CURVE('',#7567,#7568,#4537,.T.);
#9358=EDGE_CURVE('',#7568,#7489,#210,.T.);
#9359=EDGE_CURVE('',#7488,#7484,#6594,.T.);
#9360=EDGE_CURVE('',#7482,#7487,#6595,.T.);
#9361=EDGE_CURVE('',#7569,#7569,#6596,.T.);
#9362=EDGE_CURVE('',#7569,#7570,#4538,.T.);
#9363=EDGE_CURVE('',#7570,#7570,#6597,.T.);
#9364=EDGE_CURVE('',#7571,#7566,#4539,.T.);
#9365=EDGE_CURVE('',#7572,#7571,#211,.T.);
#9366=EDGE_CURVE('',#7567,#7572,#4540,.T.);
#9367=EDGE_CURVE('',#7573,#7572,#4541,.T.);
#9368=EDGE_CURVE('',#7568,#7573,#4542,.T.);
#9369=EDGE_CURVE('',#7574,#7573,#212,.T.);
#9370=EDGE_CURVE('',#7489,#7574,#4543,.T.);
#9371=EDGE_CURVE('',#7575,#7574,#6598,.T.);
#9372=EDGE_CURVE('',#7575,#7490,#4544,.T.);
#9373=EDGE_CURVE('',#7576,#7575,#213,.T.);
#9374=EDGE_CURVE('',#7491,#7576,#4545,.T.);
#9375=EDGE_CURVE('',#7577,#7576,#4546,.T.);
#9376=EDGE_CURVE('',#7492,#7577,#4547,.T.);
#9377=EDGE_CURVE('',#7578,#7577,#214,.T.);
#9378=EDGE_CURVE('',#7493,#7578,#4548,.T.);
#9379=EDGE_CURVE('',#7579,#7578,#6599,.T.);
#9380=EDGE_CURVE('',#7579,#7494,#4549,.T.);
#9381=EDGE_CURVE('',#7580,#7579,#215,.T.);
#9382=EDGE_CURVE('',#7495,#7580,#4550,.T.);
#9383=EDGE_CURVE('',#7581,#7580,#4551,.T.);
#9384=EDGE_CURVE('',#7496,#7581,#4552,.T.);
#9385=EDGE_CURVE('',#7582,#7581,#216,.T.);
#9386=EDGE_CURVE('',#7497,#7582,#4553,.T.);
#9387=EDGE_CURVE('',#7583,#7582,#6600,.T.);
#9388=EDGE_CURVE('',#7583,#7498,#4554,.T.);
#9389=EDGE_CURVE('',#7584,#7583,#217,.T.);
#9390=EDGE_CURVE('',#7499,#7584,#4555,.T.);
#9391=EDGE_CURVE('',#7585,#7584,#4556,.T.);
#9392=EDGE_CURVE('',#7500,#7585,#4557,.T.);
#9393=EDGE_CURVE('',#7586,#7585,#218,.T.);
#9394=EDGE_CURVE('',#7501,#7586,#4558,.T.);
#9395=EDGE_CURVE('',#7587,#7586,#6601,.T.);
#9396=EDGE_CURVE('',#7587,#7502,#4559,.T.);
#9397=EDGE_CURVE('',#7588,#7587,#219,.T.);
#9398=EDGE_CURVE('',#7503,#7588,#4560,.T.);
#9399=EDGE_CURVE('',#7589,#7588,#4561,.T.);
#9400=EDGE_CURVE('',#7504,#7589,#4562,.T.);
#9401=EDGE_CURVE('',#7590,#7589,#220,.T.);
#9402=EDGE_CURVE('',#7505,#7590,#4563,.T.);
#9403=EDGE_CURVE('',#7591,#7590,#6602,.T.);
#9404=EDGE_CURVE('',#7591,#7506,#4564,.T.);
#9405=EDGE_CURVE('',#7592,#7591,#221,.T.);
#9406=EDGE_CURVE('',#7507,#7592,#4565,.T.);
#9407=EDGE_CURVE('',#7593,#7592,#4566,.T.);
#9408=EDGE_CURVE('',#7508,#7593,#4567,.T.);
#9409=EDGE_CURVE('',#7594,#7593,#222,.T.);
#9410=EDGE_CURVE('',#7509,#7594,#4568,.T.);
#9411=EDGE_CURVE('',#7595,#7594,#6603,.T.);
#9412=EDGE_CURVE('',#7595,#7510,#4569,.T.);
#9413=EDGE_CURVE('',#7596,#7595,#223,.T.);
#9414=EDGE_CURVE('',#7511,#7596,#4570,.T.);
#9415=EDGE_CURVE('',#7597,#7596,#4571,.T.);
#9416=EDGE_CURVE('',#7512,#7597,#4572,.T.);
#9417=EDGE_CURVE('',#7598,#7597,#224,.T.);
#9418=EDGE_CURVE('',#7513,#7598,#4573,.T.);
#9419=EDGE_CURVE('',#7599,#7598,#6604,.T.);
#9420=EDGE_CURVE('',#7599,#7514,#4574,.T.);
#9421=EDGE_CURVE('',#7600,#7599,#225,.T.);
#9422=EDGE_CURVE('',#7515,#7600,#4575,.T.);
#9423=EDGE_CURVE('',#7601,#7600,#4576,.T.);
#9424=EDGE_CURVE('',#7516,#7601,#4577,.T.);
#9425=EDGE_CURVE('',#7602,#7601,#226,.T.);
#9426=EDGE_CURVE('',#7517,#7602,#4578,.T.);
#9427=EDGE_CURVE('',#7603,#7602,#6605,.T.);
#9428=EDGE_CURVE('',#7603,#7518,#4579,.T.);
#9429=EDGE_CURVE('',#7604,#7603,#227,.T.);
#9430=EDGE_CURVE('',#7519,#7604,#4580,.T.);
#9431=EDGE_CURVE('',#7605,#7604,#4581,.T.);
#9432=EDGE_CURVE('',#7520,#7605,#4582,.T.);
#9433=EDGE_CURVE('',#7606,#7605,#228,.T.);
#9434=EDGE_CURVE('',#7521,#7606,#4583,.T.);
#9435=EDGE_CURVE('',#7607,#7606,#6606,.T.);
#9436=EDGE_CURVE('',#7607,#7522,#4584,.T.);
#9437=EDGE_CURVE('',#7608,#7607,#229,.T.);
#9438=EDGE_CURVE('',#7523,#7608,#4585,.T.);
#9439=EDGE_CURVE('',#7609,#7608,#4586,.T.);
#9440=EDGE_CURVE('',#7524,#7609,#4587,.T.);
#9441=EDGE_CURVE('',#7610,#7609,#230,.T.);
#9442=EDGE_CURVE('',#7525,#7610,#4588,.T.);
#9443=EDGE_CURVE('',#7611,#7610,#6607,.T.);
#9444=EDGE_CURVE('',#7611,#7526,#4589,.T.);
#9445=EDGE_CURVE('',#7612,#7611,#231,.T.);
#9446=EDGE_CURVE('',#7527,#7612,#4590,.T.);
#9447=EDGE_CURVE('',#7613,#7612,#4591,.T.);
#9448=EDGE_CURVE('',#7528,#7613,#4592,.T.);
#9449=EDGE_CURVE('',#7614,#7613,#232,.T.);
#9450=EDGE_CURVE('',#7529,#7614,#4593,.T.);
#9451=EDGE_CURVE('',#7615,#7614,#6608,.T.);
#9452=EDGE_CURVE('',#7615,#7530,#4594,.T.);
#9453=EDGE_CURVE('',#7616,#7615,#233,.T.);
#9454=EDGE_CURVE('',#7531,#7616,#4595,.T.);
#9455=EDGE_CURVE('',#7617,#7616,#4596,.T.);
#9456=EDGE_CURVE('',#7532,#7617,#4597,.T.);
#9457=EDGE_CURVE('',#7618,#7617,#234,.T.);
#9458=EDGE_CURVE('',#7533,#7618,#4598,.T.);
#9459=EDGE_CURVE('',#7619,#7618,#6609,.T.);
#9460=EDGE_CURVE('',#7619,#7534,#4599,.T.);
#9461=EDGE_CURVE('',#7620,#7619,#235,.T.);
#9462=EDGE_CURVE('',#7535,#7620,#4600,.T.);
#9463=EDGE_CURVE('',#7621,#7620,#4601,.T.);
#9464=EDGE_CURVE('',#7536,#7621,#4602,.T.);
#9465=EDGE_CURVE('',#7622,#7621,#236,.T.);
#9466=EDGE_CURVE('',#7537,#7622,#4603,.T.);
#9467=EDGE_CURVE('',#7623,#7622,#6610,.T.);
#9468=EDGE_CURVE('',#7623,#7538,#4604,.T.);
#9469=EDGE_CURVE('',#7624,#7623,#237,.T.);
#9470=EDGE_CURVE('',#7539,#7624,#4605,.T.);
#9471=EDGE_CURVE('',#7625,#7624,#4606,.T.);
#9472=EDGE_CURVE('',#7540,#7625,#4607,.T.);
#9473=EDGE_CURVE('',#7626,#7625,#238,.T.);
#9474=EDGE_CURVE('',#7541,#7626,#4608,.T.);
#9475=EDGE_CURVE('',#7627,#7626,#6611,.T.);
#9476=EDGE_CURVE('',#7627,#7542,#4609,.T.);
#9477=EDGE_CURVE('',#7628,#7627,#239,.T.);
#9478=EDGE_CURVE('',#7543,#7628,#4610,.T.);
#9479=EDGE_CURVE('',#7629,#7628,#4611,.T.);
#9480=EDGE_CURVE('',#7544,#7629,#4612,.T.);
#9481=EDGE_CURVE('',#7630,#7629,#240,.T.);
#9482=EDGE_CURVE('',#7545,#7630,#4613,.T.);
#9483=EDGE_CURVE('',#7631,#7630,#6612,.T.);
#9484=EDGE_CURVE('',#7631,#7546,#4614,.T.);
#9485=EDGE_CURVE('',#7632,#7631,#241,.T.);
#9486=EDGE_CURVE('',#7547,#7632,#4615,.T.);
#9487=EDGE_CURVE('',#7633,#7632,#4616,.T.);
#9488=EDGE_CURVE('',#7548,#7633,#4617,.T.);
#9489=EDGE_CURVE('',#7634,#7633,#242,.T.);
#9490=EDGE_CURVE('',#7549,#7634,#4618,.T.);
#9491=EDGE_CURVE('',#7635,#7634,#6613,.T.);
#9492=EDGE_CURVE('',#7635,#7550,#4619,.T.);
#9493=EDGE_CURVE('',#7636,#7635,#243,.T.);
#9494=EDGE_CURVE('',#7551,#7636,#4620,.T.);
#9495=EDGE_CURVE('',#7637,#7636,#4621,.T.);
#9496=EDGE_CURVE('',#7552,#7637,#4622,.T.);
#9497=EDGE_CURVE('',#7638,#7637,#244,.T.);
#9498=EDGE_CURVE('',#7553,#7638,#4623,.T.);
#9499=EDGE_CURVE('',#7639,#7638,#6614,.T.);
#9500=EDGE_CURVE('',#7639,#7554,#4624,.T.);
#9501=EDGE_CURVE('',#7640,#7639,#245,.T.);
#9502=EDGE_CURVE('',#7555,#7640,#4625,.T.);
#9503=EDGE_CURVE('',#7641,#7640,#4626,.T.);
#9504=EDGE_CURVE('',#7556,#7641,#4627,.T.);
#9505=EDGE_CURVE('',#7642,#7641,#246,.T.);
#9506=EDGE_CURVE('',#7557,#7642,#4628,.T.);
#9507=EDGE_CURVE('',#7643,#7642,#6615,.T.);
#9508=EDGE_CURVE('',#7643,#7558,#4629,.T.);
#9509=EDGE_CURVE('',#7644,#7643,#247,.T.);
#9510=EDGE_CURVE('',#7559,#7644,#4630,.T.);
#9511=EDGE_CURVE('',#7645,#7644,#4631,.T.);
#9512=EDGE_CURVE('',#7560,#7645,#4632,.T.);
#9513=EDGE_CURVE('',#7646,#7645,#248,.T.);
#9514=EDGE_CURVE('',#7561,#7646,#4633,.T.);
#9515=EDGE_CURVE('',#7647,#7646,#6616,.T.);
#9516=EDGE_CURVE('',#7647,#7562,#4634,.T.);
#9517=EDGE_CURVE('',#7648,#7647,#249,.T.);
#9518=EDGE_CURVE('',#7563,#7648,#4635,.T.);
#9519=EDGE_CURVE('',#7649,#7648,#4636,.T.);
#9520=EDGE_CURVE('',#7564,#7649,#4637,.T.);
#9521=EDGE_CURVE('',#7650,#7649,#250,.T.);
#9522=EDGE_CURVE('',#7565,#7650,#4638,.T.);
#9523=EDGE_CURVE('',#7571,#7650,#6617,.T.);
#9524=EDGE_CURVE('',#7651,#7652,#4639,.T.);
#9525=EDGE_CURVE('',#7653,#7651,#4640,.T.);
#9526=EDGE_CURVE('',#7654,#7653,#4641,.T.);
#9527=EDGE_CURVE('',#7655,#7654,#4642,.T.);
#9528=EDGE_CURVE('',#7656,#7655,#4643,.T.);
#9529=EDGE_CURVE('',#7657,#7656,#4644,.T.);
#9530=EDGE_CURVE('',#7658,#7657,#4645,.T.);
#9531=EDGE_CURVE('',#7652,#7658,#4646,.T.);
#9532=EDGE_CURVE('',#7655,#7659,#4647,.T.);
#9533=EDGE_CURVE('',#7659,#7660,#4648,.T.);
#9534=EDGE_CURVE('',#7660,#7656,#4649,.T.);
#9535=EDGE_CURVE('',#7661,#7654,#4650,.T.);
#9536=EDGE_CURVE('',#7661,#7659,#4651,.T.);
#9537=EDGE_CURVE('',#7653,#7662,#4652,.T.);
#9538=EDGE_CURVE('',#7662,#7661,#4653,.T.);
#9539=EDGE_CURVE('',#7663,#7651,#4654,.T.);
#9540=EDGE_CURVE('',#7663,#7662,#4655,.T.);
#9541=EDGE_CURVE('',#7664,#7663,#4656,.T.);
#9542=EDGE_CURVE('',#7665,#7664,#4657,.T.);
#9543=EDGE_CURVE('',#7666,#7665,#4658,.T.);
#9544=EDGE_CURVE('',#7660,#7666,#4659,.T.);
#9545=EDGE_CURVE('',#7652,#7664,#4660,.T.);
#9546=EDGE_CURVE('',#7665,#7658,#4661,.T.);
#9547=EDGE_CURVE('',#7657,#7666,#4662,.T.);
#9548=EDGE_CURVE('',#7667,#7668,#4663,.T.);
#9549=EDGE_CURVE('',#7667,#7669,#4664,.T.);
#9550=EDGE_CURVE('',#7670,#7669,#4665,.T.);
#9551=EDGE_CURVE('',#7670,#7668,#4666,.T.);
#9552=EDGE_CURVE('',#7668,#7671,#6618,.T.);
#9553=EDGE_CURVE('',#7672,#7670,#4667,.T.);
#9554=EDGE_CURVE('',#7671,#7672,#4668,.T.);
#9555=EDGE_CURVE('',#7671,#7673,#4669,.T.);
#9556=EDGE_CURVE('',#7672,#7674,#4670,.T.);
#9557=EDGE_CURVE('',#7674,#7673,#4671,.T.);
#9558=EDGE_CURVE('',#7669,#7674,#4672,.T.);
#9559=EDGE_CURVE('',#7673,#7667,#6619,.T.);
#9560=EDGE_CURVE('',#7675,#7676,#4673,.T.);
#9561=EDGE_CURVE('',#7675,#7677,#4674,.T.);
#9562=EDGE_CURVE('',#7678,#7677,#4675,.T.);
#9563=EDGE_CURVE('',#7678,#7676,#4676,.T.);
#9564=EDGE_CURVE('',#7676,#7679,#6620,.T.);
#9565=EDGE_CURVE('',#7680,#7678,#4677,.T.);
#9566=EDGE_CURVE('',#7679,#7680,#4678,.T.);
#9567=EDGE_CURVE('',#7679,#7681,#4679,.T.);
#9568=EDGE_CURVE('',#7680,#7682,#4680,.T.);
#9569=EDGE_CURVE('',#7682,#7681,#4681,.T.);
#9570=EDGE_CURVE('',#7677,#7682,#4682,.T.);
#9571=EDGE_CURVE('',#7681,#7675,#6621,.T.);
#9572=EDGE_CURVE('',#7683,#7683,#6622,.T.);
#9573=EDGE_CURVE('',#7683,#7684,#4683,.T.);
#9574=EDGE_CURVE('',#7684,#7684,#6623,.T.);
#9575=EDGE_CURVE('',#7685,#7686,#4684,.T.);
#9576=EDGE_CURVE('',#7685,#7686,#6624,.T.);
#9577=EDGE_CURVE('',#7687,#7685,#971,.T.);
#9578=EDGE_CURVE('',#7688,#7687,#6625,.T.);
#9579=EDGE_CURVE('',#7688,#7689,#4685,.T.);
#9580=EDGE_CURVE('',#7690,#7689,#972,.T.);
#9581=EDGE_CURVE('',#7689,#7690,#973,.T.);
#9582=EDGE_CURVE('',#7691,#7688,#6626,.T.);
#9583=EDGE_CURVE('',#7686,#7691,#974,.T.);
#9584=EDGE_CURVE('',#7691,#7687,#4686,.T.);
#9585=EDGE_CURVE('',#7692,#7692,#6627,.T.);
#9586=EDGE_CURVE('',#7692,#7693,#4687,.T.);
#9587=EDGE_CURVE('',#7693,#7693,#6628,.T.);
#9588=EDGE_CURVE('',#7694,#7694,#6629,.T.);
#9589=EDGE_CURVE('',#7694,#7695,#4688,.T.);
#9590=EDGE_CURVE('',#7695,#7695,#6630,.T.);
#9591=EDGE_CURVE('',#7696,#7697,#4689,.T.);
#9592=EDGE_CURVE('',#7696,#7697,#6631,.T.);
#9593=EDGE_CURVE('',#7698,#7696,#975,.T.);
#9594=EDGE_CURVE('',#7699,#7698,#6632,.T.);
#9595=EDGE_CURVE('',#7699,#7700,#4690,.T.);
#9596=EDGE_CURVE('',#7701,#7700,#976,.T.);
#9597=EDGE_CURVE('',#7700,#7701,#977,.T.);
#9598=EDGE_CURVE('',#7702,#7699,#6633,.T.);
#9599=EDGE_CURVE('',#7697,#7702,#978,.T.);
#9600=EDGE_CURVE('',#7702,#7698,#4691,.T.);
#9601=EDGE_CURVE('',#7703,#7703,#6634,.T.);
#9602=EDGE_CURVE('',#7703,#7704,#4692,.T.);
#9603=EDGE_CURVE('',#7704,#7704,#6635,.T.);
#9604=EDGE_CURVE('',#7705,#7705,#6636,.T.);
#9605=EDGE_CURVE('',#7705,#7706,#4693,.T.);
#9606=EDGE_CURVE('',#7706,#7706,#6637,.T.);
#9607=EDGE_CURVE('',#7707,#7707,#6638,.T.);
#9608=EDGE_CURVE('',#7707,#7708,#4694,.T.);
#9609=EDGE_CURVE('',#7708,#7708,#6639,.T.);
#9610=EDGE_CURVE('',#7709,#7709,#6640,.T.);
#9611=EDGE_CURVE('',#7709,#7710,#4695,.T.);
#9612=EDGE_CURVE('',#7710,#7710,#6641,.T.);
#9613=EDGE_CURVE('',#7711,#7711,#6642,.T.);
#9614=EDGE_CURVE('',#7711,#7712,#4696,.T.);
#9615=EDGE_CURVE('',#7712,#7712,#6643,.T.);
#9616=EDGE_CURVE('',#7713,#7713,#6644,.T.);
#9617=EDGE_CURVE('',#7713,#7714,#4697,.T.);
#9618=EDGE_CURVE('',#7714,#7714,#6645,.T.);
#9619=EDGE_CURVE('',#7715,#7715,#6646,.T.);
#9620=EDGE_CURVE('',#7715,#7716,#4698,.T.);
#9621=EDGE_CURVE('',#7716,#7716,#6647,.T.);
#9622=EDGE_CURVE('',#7717,#7717,#6648,.T.);
#9623=EDGE_CURVE('',#7717,#7718,#4699,.T.);
#9624=EDGE_CURVE('',#7718,#7718,#6649,.T.);
#9625=EDGE_CURVE('',#7719,#7719,#6650,.T.);
#9626=EDGE_CURVE('',#7719,#7720,#4700,.T.);
#9627=EDGE_CURVE('',#7720,#7720,#6651,.T.);
#9628=EDGE_CURVE('',#7721,#7721,#6652,.T.);
#9629=EDGE_CURVE('',#7721,#7722,#4701,.T.);
#9630=EDGE_CURVE('',#7722,#7722,#6653,.T.);
#9631=EDGE_CURVE('',#7723,#7723,#6654,.T.);
#9632=EDGE_CURVE('',#7723,#7724,#4702,.T.);
#9633=EDGE_CURVE('',#7724,#7724,#6655,.T.);
#9634=EDGE_CURVE('',#7725,#7725,#6656,.T.);
#9635=EDGE_CURVE('',#7725,#7726,#4703,.T.);
#9636=EDGE_CURVE('',#7726,#7726,#6657,.T.);
#9637=EDGE_CURVE('',#7727,#7728,#4704,.T.);
#9638=EDGE_CURVE('',#7727,#7729,#4705,.T.);
#9639=EDGE_CURVE('',#7730,#7729,#4706,.T.);
#9640=EDGE_CURVE('',#7728,#7730,#4707,.T.);
#9641=EDGE_CURVE('',#7731,#7727,#4708,.T.);
#9642=EDGE_CURVE('',#7731,#7732,#4709,.T.);
#9643=EDGE_CURVE('',#7729,#7732,#4710,.T.);
#9644=EDGE_CURVE('',#7733,#7731,#4711,.T.);
#9645=EDGE_CURVE('',#7734,#7733,#4712,.T.);
#9646=EDGE_CURVE('',#7732,#7734,#4713,.T.);
#9647=EDGE_CURVE('',#7735,#7735,#6658,.T.);
#9648=EDGE_CURVE('',#7734,#7730,#6659,.T.);
#9649=EDGE_CURVE('',#7728,#7733,#6660,.T.);
#9650=EDGE_CURVE('',#7736,#7737,#6661,.T.);
#9651=EDGE_CURVE('',#7737,#7738,#251,.T.);
#9652=EDGE_CURVE('',#7738,#7739,#4714,.T.);
#9653=EDGE_CURVE('',#7739,#7740,#252,.T.);
#9654=EDGE_CURVE('',#7740,#7741,#6662,.T.);
#9655=EDGE_CURVE('',#7741,#7742,#253,.T.);
#9656=EDGE_CURVE('',#7742,#7743,#4715,.T.);
#9657=EDGE_CURVE('',#7743,#7744,#254,.T.);
#9658=EDGE_CURVE('',#7744,#7745,#6663,.T.);
#9659=EDGE_CURVE('',#7745,#7746,#255,.T.);
#9660=EDGE_CURVE('',#7746,#7747,#4716,.T.);
#9661=EDGE_CURVE('',#7747,#7748,#256,.T.);
#9662=EDGE_CURVE('',#7748,#7749,#6664,.T.);
#9663=EDGE_CURVE('',#7749,#7750,#257,.T.);
#9664=EDGE_CURVE('',#7750,#7751,#4717,.T.);
#9665=EDGE_CURVE('',#7751,#7752,#258,.T.);
#9666=EDGE_CURVE('',#7752,#7753,#6665,.T.);
#9667=EDGE_CURVE('',#7753,#7754,#259,.T.);
#9668=EDGE_CURVE('',#7754,#7755,#4718,.T.);
#9669=EDGE_CURVE('',#7755,#7756,#260,.T.);
#9670=EDGE_CURVE('',#7756,#7757,#6666,.T.);
#9671=EDGE_CURVE('',#7757,#7758,#261,.T.);
#9672=EDGE_CURVE('',#7758,#7759,#4719,.T.);
#9673=EDGE_CURVE('',#7759,#7760,#262,.T.);
#9674=EDGE_CURVE('',#7760,#7761,#6667,.T.);
#9675=EDGE_CURVE('',#7761,#7762,#263,.T.);
#9676=EDGE_CURVE('',#7762,#7763,#4720,.T.);
#9677=EDGE_CURVE('',#7763,#7764,#264,.T.);
#9678=EDGE_CURVE('',#7764,#7765,#6668,.T.);
#9679=EDGE_CURVE('',#7765,#7766,#265,.T.);
#9680=EDGE_CURVE('',#7766,#7767,#4721,.T.);
#9681=EDGE_CURVE('',#7767,#7768,#266,.T.);
#9682=EDGE_CURVE('',#7768,#7769,#6669,.T.);
#9683=EDGE_CURVE('',#7769,#7770,#267,.T.);
#9684=EDGE_CURVE('',#7770,#7771,#4722,.T.);
#9685=EDGE_CURVE('',#7771,#7772,#268,.T.);
#9686=EDGE_CURVE('',#7772,#7773,#6670,.T.);
#9687=EDGE_CURVE('',#7773,#7774,#269,.T.);
#9688=EDGE_CURVE('',#7774,#7775,#4723,.T.);
#9689=EDGE_CURVE('',#7775,#7776,#270,.T.);
#9690=EDGE_CURVE('',#7776,#7777,#6671,.T.);
#9691=EDGE_CURVE('',#7777,#7778,#271,.T.);
#9692=EDGE_CURVE('',#7778,#7779,#4724,.T.);
#9693=EDGE_CURVE('',#7779,#7780,#272,.T.);
#9694=EDGE_CURVE('',#7780,#7781,#6672,.T.);
#9695=EDGE_CURVE('',#7781,#7782,#273,.T.);
#9696=EDGE_CURVE('',#7782,#7783,#4725,.T.);
#9697=EDGE_CURVE('',#7783,#7784,#274,.T.);
#9698=EDGE_CURVE('',#7784,#7785,#6673,.T.);
#9699=EDGE_CURVE('',#7785,#7786,#275,.T.);
#9700=EDGE_CURVE('',#7786,#7787,#4726,.T.);
#9701=EDGE_CURVE('',#7787,#7788,#276,.T.);
#9702=EDGE_CURVE('',#7788,#7789,#6674,.T.);
#9703=EDGE_CURVE('',#7789,#7790,#277,.T.);
#9704=EDGE_CURVE('',#7790,#7791,#4727,.T.);
#9705=EDGE_CURVE('',#7791,#7792,#278,.T.);
#9706=EDGE_CURVE('',#7792,#7793,#6675,.T.);
#9707=EDGE_CURVE('',#7793,#7794,#279,.T.);
#9708=EDGE_CURVE('',#7794,#7795,#4728,.T.);
#9709=EDGE_CURVE('',#7795,#7796,#280,.T.);
#9710=EDGE_CURVE('',#7796,#7797,#6676,.T.);
#9711=EDGE_CURVE('',#7797,#7798,#281,.T.);
#9712=EDGE_CURVE('',#7798,#7799,#4729,.T.);
#9713=EDGE_CURVE('',#7799,#7800,#282,.T.);
#9714=EDGE_CURVE('',#7800,#7801,#6677,.T.);
#9715=EDGE_CURVE('',#7801,#7802,#283,.T.);
#9716=EDGE_CURVE('',#7802,#7803,#4730,.T.);
#9717=EDGE_CURVE('',#7803,#7804,#284,.T.);
#9718=EDGE_CURVE('',#7804,#7805,#6678,.T.);
#9719=EDGE_CURVE('',#7805,#7806,#285,.T.);
#9720=EDGE_CURVE('',#7806,#7807,#4731,.T.);
#9721=EDGE_CURVE('',#7807,#7808,#286,.T.);
#9722=EDGE_CURVE('',#7808,#7809,#6679,.T.);
#9723=EDGE_CURVE('',#7809,#7810,#287,.T.);
#9724=EDGE_CURVE('',#7810,#7811,#4732,.T.);
#9725=EDGE_CURVE('',#7811,#7812,#288,.T.);
#9726=EDGE_CURVE('',#7812,#7813,#6680,.T.);
#9727=EDGE_CURVE('',#7813,#7814,#289,.T.);
#9728=EDGE_CURVE('',#7814,#7815,#4733,.T.);
#9729=EDGE_CURVE('',#7815,#7736,#290,.T.);
#9730=EDGE_CURVE('',#7735,#7816,#4734,.T.);
#9731=EDGE_CURVE('',#7816,#7816,#6681,.T.);
#9732=EDGE_CURVE('',#7817,#7813,#4735,.T.);
#9733=EDGE_CURVE('',#7818,#7817,#291,.T.);
#9734=EDGE_CURVE('',#7814,#7818,#4736,.T.);
#9735=EDGE_CURVE('',#7819,#7818,#4737,.T.);
#9736=EDGE_CURVE('',#7815,#7819,#4738,.T.);
#9737=EDGE_CURVE('',#7820,#7819,#292,.T.);
#9738=EDGE_CURVE('',#7736,#7820,#4739,.T.);
#9739=EDGE_CURVE('',#7821,#7820,#6682,.T.);
#9740=EDGE_CURVE('',#7821,#7737,#4740,.T.);
#9741=EDGE_CURVE('',#7822,#7821,#293,.T.);
#9742=EDGE_CURVE('',#7738,#7822,#4741,.T.);
#9743=EDGE_CURVE('',#7823,#7822,#4742,.T.);
#9744=EDGE_CURVE('',#7739,#7823,#4743,.T.);
#9745=EDGE_CURVE('',#7824,#7823,#294,.T.);
#9746=EDGE_CURVE('',#7740,#7824,#4744,.T.);
#9747=EDGE_CURVE('',#7825,#7824,#6683,.T.);
#9748=EDGE_CURVE('',#7825,#7741,#4745,.T.);
#9749=EDGE_CURVE('',#7826,#7825,#295,.T.);
#9750=EDGE_CURVE('',#7742,#7826,#4746,.T.);
#9751=EDGE_CURVE('',#7827,#7826,#4747,.T.);
#9752=EDGE_CURVE('',#7743,#7827,#4748,.T.);
#9753=EDGE_CURVE('',#7828,#7827,#296,.T.);
#9754=EDGE_CURVE('',#7744,#7828,#4749,.T.);
#9755=EDGE_CURVE('',#7829,#7828,#6684,.T.);
#9756=EDGE_CURVE('',#7829,#7745,#4750,.T.);
#9757=EDGE_CURVE('',#7830,#7829,#297,.T.);
#9758=EDGE_CURVE('',#7746,#7830,#4751,.T.);
#9759=EDGE_CURVE('',#7831,#7830,#4752,.T.);
#9760=EDGE_CURVE('',#7747,#7831,#4753,.T.);
#9761=EDGE_CURVE('',#7832,#7831,#298,.T.);
#9762=EDGE_CURVE('',#7748,#7832,#4754,.T.);
#9763=EDGE_CURVE('',#7833,#7832,#6685,.T.);
#9764=EDGE_CURVE('',#7833,#7749,#4755,.T.);
#9765=EDGE_CURVE('',#7834,#7833,#299,.T.);
#9766=EDGE_CURVE('',#7750,#7834,#4756,.T.);
#9767=EDGE_CURVE('',#7835,#7834,#4757,.T.);
#9768=EDGE_CURVE('',#7751,#7835,#4758,.T.);
#9769=EDGE_CURVE('',#7836,#7835,#300,.T.);
#9770=EDGE_CURVE('',#7752,#7836,#4759,.T.);
#9771=EDGE_CURVE('',#7837,#7836,#6686,.T.);
#9772=EDGE_CURVE('',#7837,#7753,#4760,.T.);
#9773=EDGE_CURVE('',#7838,#7837,#301,.T.);
#9774=EDGE_CURVE('',#7754,#7838,#4761,.T.);
#9775=EDGE_CURVE('',#7839,#7838,#4762,.T.);
#9776=EDGE_CURVE('',#7755,#7839,#4763,.T.);
#9777=EDGE_CURVE('',#7840,#7839,#302,.T.);
#9778=EDGE_CURVE('',#7756,#7840,#4764,.T.);
#9779=EDGE_CURVE('',#7841,#7840,#6687,.T.);
#9780=EDGE_CURVE('',#7841,#7757,#4765,.T.);
#9781=EDGE_CURVE('',#7842,#7841,#303,.T.);
#9782=EDGE_CURVE('',#7758,#7842,#4766,.T.);
#9783=EDGE_CURVE('',#7843,#7842,#4767,.T.);
#9784=EDGE_CURVE('',#7759,#7843,#4768,.T.);
#9785=EDGE_CURVE('',#7844,#7843,#304,.T.);
#9786=EDGE_CURVE('',#7760,#7844,#4769,.T.);
#9787=EDGE_CURVE('',#7845,#7844,#6688,.T.);
#9788=EDGE_CURVE('',#7845,#7761,#4770,.T.);
#9789=EDGE_CURVE('',#7846,#7845,#305,.T.);
#9790=EDGE_CURVE('',#7762,#7846,#4771,.T.);
#9791=EDGE_CURVE('',#7847,#7846,#4772,.T.);
#9792=EDGE_CURVE('',#7763,#7847,#4773,.T.);
#9793=EDGE_CURVE('',#7848,#7847,#306,.T.);
#9794=EDGE_CURVE('',#7764,#7848,#4774,.T.);
#9795=EDGE_CURVE('',#7849,#7848,#6689,.T.);
#9796=EDGE_CURVE('',#7849,#7765,#4775,.T.);
#9797=EDGE_CURVE('',#7850,#7849,#307,.T.);
#9798=EDGE_CURVE('',#7766,#7850,#4776,.T.);
#9799=EDGE_CURVE('',#7851,#7850,#4777,.T.);
#9800=EDGE_CURVE('',#7767,#7851,#4778,.T.);
#9801=EDGE_CURVE('',#7852,#7851,#308,.T.);
#9802=EDGE_CURVE('',#7768,#7852,#4779,.T.);
#9803=EDGE_CURVE('',#7853,#7852,#6690,.T.);
#9804=EDGE_CURVE('',#7853,#7769,#4780,.T.);
#9805=EDGE_CURVE('',#7854,#7853,#309,.T.);
#9806=EDGE_CURVE('',#7770,#7854,#4781,.T.);
#9807=EDGE_CURVE('',#7855,#7854,#4782,.T.);
#9808=EDGE_CURVE('',#7771,#7855,#4783,.T.);
#9809=EDGE_CURVE('',#7856,#7855,#310,.T.);
#9810=EDGE_CURVE('',#7772,#7856,#4784,.T.);
#9811=EDGE_CURVE('',#7857,#7856,#6691,.T.);
#9812=EDGE_CURVE('',#7857,#7773,#4785,.T.);
#9813=EDGE_CURVE('',#7858,#7857,#311,.T.);
#9814=EDGE_CURVE('',#7774,#7858,#4786,.T.);
#9815=EDGE_CURVE('',#7859,#7858,#4787,.T.);
#9816=EDGE_CURVE('',#7775,#7859,#4788,.T.);
#9817=EDGE_CURVE('',#7860,#7859,#312,.T.);
#9818=EDGE_CURVE('',#7776,#7860,#4789,.T.);
#9819=EDGE_CURVE('',#7861,#7860,#6692,.T.);
#9820=EDGE_CURVE('',#7861,#7777,#4790,.T.);
#9821=EDGE_CURVE('',#7862,#7861,#313,.T.);
#9822=EDGE_CURVE('',#7778,#7862,#4791,.T.);
#9823=EDGE_CURVE('',#7863,#7862,#4792,.T.);
#9824=EDGE_CURVE('',#7779,#7863,#4793,.T.);
#9825=EDGE_CURVE('',#7864,#7863,#314,.T.);
#9826=EDGE_CURVE('',#7780,#7864,#4794,.T.);
#9827=EDGE_CURVE('',#7865,#7864,#6693,.T.);
#9828=EDGE_CURVE('',#7865,#7781,#4795,.T.);
#9829=EDGE_CURVE('',#7866,#7865,#315,.T.);
#9830=EDGE_CURVE('',#7782,#7866,#4796,.T.);
#9831=EDGE_CURVE('',#7867,#7866,#4797,.T.);
#9832=EDGE_CURVE('',#7783,#7867,#4798,.T.);
#9833=EDGE_CURVE('',#7868,#7867,#316,.T.);
#9834=EDGE_CURVE('',#7784,#7868,#4799,.T.);
#9835=EDGE_CURVE('',#7869,#7868,#6694,.T.);
#9836=EDGE_CURVE('',#7869,#7785,#4800,.T.);
#9837=EDGE_CURVE('',#7870,#7869,#317,.T.);
#9838=EDGE_CURVE('',#7786,#7870,#4801,.T.);
#9839=EDGE_CURVE('',#7871,#7870,#4802,.T.);
#9840=EDGE_CURVE('',#7787,#7871,#4803,.T.);
#9841=EDGE_CURVE('',#7872,#7871,#318,.T.);
#9842=EDGE_CURVE('',#7788,#7872,#4804,.T.);
#9843=EDGE_CURVE('',#7873,#7872,#6695,.T.);
#9844=EDGE_CURVE('',#7873,#7789,#4805,.T.);
#9845=EDGE_CURVE('',#7874,#7873,#319,.T.);
#9846=EDGE_CURVE('',#7790,#7874,#4806,.T.);
#9847=EDGE_CURVE('',#7875,#7874,#4807,.T.);
#9848=EDGE_CURVE('',#7791,#7875,#4808,.T.);
#9849=EDGE_CURVE('',#7876,#7875,#320,.T.);
#9850=EDGE_CURVE('',#7792,#7876,#4809,.T.);
#9851=EDGE_CURVE('',#7877,#7876,#6696,.T.);
#9852=EDGE_CURVE('',#7877,#7793,#4810,.T.);
#9853=EDGE_CURVE('',#7878,#7877,#321,.T.);
#9854=EDGE_CURVE('',#7794,#7878,#4811,.T.);
#9855=EDGE_CURVE('',#7879,#7878,#4812,.T.);
#9856=EDGE_CURVE('',#7795,#7879,#4813,.T.);
#9857=EDGE_CURVE('',#7880,#7879,#322,.T.);
#9858=EDGE_CURVE('',#7796,#7880,#4814,.T.);
#9859=EDGE_CURVE('',#7881,#7880,#6697,.T.);
#9860=EDGE_CURVE('',#7881,#7797,#4815,.T.);
#9861=EDGE_CURVE('',#7882,#7881,#323,.T.);
#9862=EDGE_CURVE('',#7798,#7882,#4816,.T.);
#9863=EDGE_CURVE('',#7883,#7882,#4817,.T.);
#9864=EDGE_CURVE('',#7799,#7883,#4818,.T.);
#9865=EDGE_CURVE('',#7884,#7883,#324,.T.);
#9866=EDGE_CURVE('',#7800,#7884,#4819,.T.);
#9867=EDGE_CURVE('',#7885,#7884,#6698,.T.);
#9868=EDGE_CURVE('',#7885,#7801,#4820,.T.);
#9869=EDGE_CURVE('',#7886,#7885,#325,.T.);
#9870=EDGE_CURVE('',#7802,#7886,#4821,.T.);
#9871=EDGE_CURVE('',#7887,#7886,#4822,.T.);
#9872=EDGE_CURVE('',#7803,#7887,#4823,.T.);
#9873=EDGE_CURVE('',#7888,#7887,#326,.T.);
#9874=EDGE_CURVE('',#7804,#7888,#4824,.T.);
#9875=EDGE_CURVE('',#7889,#7888,#6699,.T.);
#9876=EDGE_CURVE('',#7889,#7805,#4825,.T.);
#9877=EDGE_CURVE('',#7890,#7889,#327,.T.);
#9878=EDGE_CURVE('',#7806,#7890,#4826,.T.);
#9879=EDGE_CURVE('',#7891,#7890,#4827,.T.);
#9880=EDGE_CURVE('',#7807,#7891,#4828,.T.);
#9881=EDGE_CURVE('',#7892,#7891,#328,.T.);
#9882=EDGE_CURVE('',#7808,#7892,#4829,.T.);
#9883=EDGE_CURVE('',#7893,#7892,#6700,.T.);
#9884=EDGE_CURVE('',#7893,#7809,#4830,.T.);
#9885=EDGE_CURVE('',#7894,#7893,#329,.T.);
#9886=EDGE_CURVE('',#7810,#7894,#4831,.T.);
#9887=EDGE_CURVE('',#7895,#7894,#4832,.T.);
#9888=EDGE_CURVE('',#7811,#7895,#4833,.T.);
#9889=EDGE_CURVE('',#7896,#7895,#330,.T.);
#9890=EDGE_CURVE('',#7812,#7896,#4834,.T.);
#9891=EDGE_CURVE('',#7817,#7896,#6701,.T.);
#9892=EDGE_CURVE('',#7897,#7898,#4835,.T.);
#9893=EDGE_CURVE('',#7897,#7899,#4836,.T.);
#9894=EDGE_CURVE('',#7900,#7899,#4837,.T.);
#9895=EDGE_CURVE('',#7900,#7898,#4838,.T.);
#9896=EDGE_CURVE('',#7898,#7901,#6702,.T.);
#9897=EDGE_CURVE('',#7902,#7900,#4839,.T.);
#9898=EDGE_CURVE('',#7901,#7902,#4840,.T.);
#9899=EDGE_CURVE('',#7901,#7903,#4841,.T.);
#9900=EDGE_CURVE('',#7902,#7904,#4842,.T.);
#9901=EDGE_CURVE('',#7904,#7903,#4843,.T.);
#9902=EDGE_CURVE('',#7899,#7904,#4844,.T.);
#9903=EDGE_CURVE('',#7903,#7897,#6703,.T.);
#9904=EDGE_CURVE('',#7905,#7905,#6704,.T.);
#9905=EDGE_CURVE('',#7905,#7906,#4845,.T.);
#9906=EDGE_CURVE('',#7906,#7906,#6705,.T.);
#9907=EDGE_CURVE('',#7907,#7908,#4846,.T.);
#9908=EDGE_CURVE('',#7907,#7908,#6706,.T.);
#9909=EDGE_CURVE('',#7909,#7907,#979,.T.);
#9910=EDGE_CURVE('',#7910,#7909,#6707,.T.);
#9911=EDGE_CURVE('',#7910,#7911,#4847,.T.);
#9912=EDGE_CURVE('',#7912,#7911,#980,.T.);
#9913=EDGE_CURVE('',#7911,#7912,#981,.T.);
#9914=EDGE_CURVE('',#7913,#7910,#6708,.T.);
#9915=EDGE_CURVE('',#7908,#7913,#982,.T.);
#9916=EDGE_CURVE('',#7913,#7909,#4848,.T.);
#9917=EDGE_CURVE('',#7914,#7914,#6709,.T.);
#9918=EDGE_CURVE('',#7914,#7915,#4849,.T.);
#9919=EDGE_CURVE('',#7915,#7915,#6710,.T.);
#9920=EDGE_CURVE('',#7916,#7916,#6711,.T.);
#9921=EDGE_CURVE('',#7916,#7917,#4850,.T.);
#9922=EDGE_CURVE('',#7917,#7917,#6712,.T.);
#9923=EDGE_CURVE('',#7918,#7919,#4851,.T.);
#9924=EDGE_CURVE('',#7918,#7919,#6713,.T.);
#9925=EDGE_CURVE('',#7920,#7918,#983,.T.);
#9926=EDGE_CURVE('',#7921,#7920,#6714,.T.);
#9927=EDGE_CURVE('',#7921,#7922,#4852,.T.);
#9928=EDGE_CURVE('',#7923,#7922,#984,.T.);
#9929=EDGE_CURVE('',#7922,#7923,#985,.T.);
#9930=EDGE_CURVE('',#7924,#7921,#6715,.T.);
#9931=EDGE_CURVE('',#7919,#7924,#986,.T.);
#9932=EDGE_CURVE('',#7924,#7920,#4853,.T.);
#9933=EDGE_CURVE('',#7925,#7925,#6716,.T.);
#9934=EDGE_CURVE('',#7925,#7926,#4854,.T.);
#9935=EDGE_CURVE('',#7926,#7926,#6717,.T.);
#9936=EDGE_CURVE('',#7927,#7927,#6718,.T.);
#9937=EDGE_CURVE('',#7927,#7928,#4855,.T.);
#9938=EDGE_CURVE('',#7928,#7928,#6719,.T.);
#9939=EDGE_CURVE('',#7929,#7929,#6720,.T.);
#9940=EDGE_CURVE('',#7929,#7930,#4856,.T.);
#9941=EDGE_CURVE('',#7930,#7930,#6721,.T.);
#9942=EDGE_CURVE('',#7931,#7931,#6722,.T.);
#9943=EDGE_CURVE('',#7931,#7932,#4857,.T.);
#9944=EDGE_CURVE('',#7932,#7932,#6723,.T.);
#9945=EDGE_CURVE('',#7933,#7933,#6724,.T.);
#9946=EDGE_CURVE('',#7933,#7934,#4858,.T.);
#9947=EDGE_CURVE('',#7934,#7934,#6725,.T.);
#9948=EDGE_CURVE('',#7935,#7935,#6726,.T.);
#9949=EDGE_CURVE('',#7935,#7936,#4859,.T.);
#9950=EDGE_CURVE('',#7936,#7936,#6727,.T.);
#9951=EDGE_CURVE('',#7937,#7937,#6728,.T.);
#9952=EDGE_CURVE('',#7937,#7938,#4860,.T.);
#9953=EDGE_CURVE('',#7938,#7938,#6729,.T.);
#9954=EDGE_CURVE('',#7939,#7939,#6730,.T.);
#9955=EDGE_CURVE('',#7939,#7940,#4861,.T.);
#9956=EDGE_CURVE('',#7940,#7940,#6731,.T.);
#9957=EDGE_CURVE('',#7941,#7941,#6732,.T.);
#9958=EDGE_CURVE('',#7941,#7942,#4862,.T.);
#9959=EDGE_CURVE('',#7942,#7942,#6733,.T.);
#9960=EDGE_CURVE('',#7943,#7943,#6734,.T.);
#9961=EDGE_CURVE('',#7943,#7944,#4863,.T.);
#9962=EDGE_CURVE('',#7944,#7944,#6735,.T.);
#9963=EDGE_CURVE('',#7945,#7946,#4864,.T.);
#9964=EDGE_CURVE('',#7945,#7947,#4865,.T.);
#9965=EDGE_CURVE('',#7947,#7948,#4866,.T.);
#9966=EDGE_CURVE('',#7946,#7948,#4867,.T.);
#9967=EDGE_CURVE('',#7949,#7945,#4868,.T.);
#9968=EDGE_CURVE('',#7949,#7950,#4869,.T.);
#9969=EDGE_CURVE('',#7950,#7947,#4870,.T.);
#9970=EDGE_CURVE('',#7951,#7949,#4871,.T.);
#9971=EDGE_CURVE('',#7951,#7952,#4872,.T.);
#9972=EDGE_CURVE('',#7952,#7950,#4873,.T.);
#9973=EDGE_CURVE('',#7953,#7951,#4874,.T.);
#9974=EDGE_CURVE('',#7953,#7954,#4875,.T.);
#9975=EDGE_CURVE('',#7954,#7952,#4876,.T.);
#9976=EDGE_CURVE('',#7955,#7953,#4877,.T.);
#9977=EDGE_CURVE('',#7955,#7956,#4878,.T.);
#9978=EDGE_CURVE('',#7956,#7954,#4879,.T.);
#9979=EDGE_CURVE('',#7946,#7955,#4880,.T.);
#9980=EDGE_CURVE('',#7948,#7956,#4881,.T.);
#9981=EDGE_CURVE('',#7957,#7957,#6736,.T.);
#9982=EDGE_CURVE('',#7958,#7958,#6737,.T.);
#9983=EDGE_CURVE('',#7958,#7957,#4882,.T.);
#9984=EDGE_CURVE('',#7959,#7959,#6738,.F.);
#9985=EDGE_CURVE('',#7959,#7958,#4883,.T.);
#9986=EDGE_CURVE('',#7960,#7960,#6739,.T.);
#9987=EDGE_CURVE('',#7960,#7959,#4884,.T.);
#9988=EDGE_CURVE('',#7961,#7962,#4885,.T.);
#9989=EDGE_CURVE('',#7963,#7961,#4886,.T.);
#9990=EDGE_CURVE('',#7964,#7963,#4887,.T.);
#9991=EDGE_CURVE('',#7962,#7964,#4888,.T.);
#9992=EDGE_CURVE('',#7965,#7961,#4889,.T.);
#9993=EDGE_CURVE('',#7965,#7966,#4890,.T.);
#9994=EDGE_CURVE('',#7963,#7966,#4891,.T.);
#9995=EDGE_CURVE('',#7967,#7965,#4892,.T.);
#9996=EDGE_CURVE('',#7968,#7967,#4893,.T.);
#9997=EDGE_CURVE('',#7966,#7968,#4894,.T.);
#9998=EDGE_CURVE('',#7969,#7970,#6740,.T.);
#9999=EDGE_CURVE('',#7970,#7971,#331,.T.);
#10000=EDGE_CURVE('',#7971,#7972,#4895,.T.);
#10001=EDGE_CURVE('',#7972,#7973,#332,.T.);
#10002=EDGE_CURVE('',#7973,#7974,#6741,.T.);
#10003=EDGE_CURVE('',#7974,#7975,#333,.T.);
#10004=EDGE_CURVE('',#7975,#7976,#4896,.T.);
#10005=EDGE_CURVE('',#7976,#7977,#334,.T.);
#10006=EDGE_CURVE('',#7977,#7978,#6742,.T.);
#10007=EDGE_CURVE('',#7978,#7979,#335,.T.);
#10008=EDGE_CURVE('',#7979,#7980,#4897,.T.);
#10009=EDGE_CURVE('',#7980,#7981,#336,.T.);
#10010=EDGE_CURVE('',#7981,#7982,#6743,.T.);
#10011=EDGE_CURVE('',#7982,#7983,#337,.T.);
#10012=EDGE_CURVE('',#7983,#7984,#4898,.T.);
#10013=EDGE_CURVE('',#7984,#7985,#338,.T.);
#10014=EDGE_CURVE('',#7985,#7986,#6744,.T.);
#10015=EDGE_CURVE('',#7986,#7987,#339,.T.);
#10016=EDGE_CURVE('',#7987,#7988,#4899,.T.);
#10017=EDGE_CURVE('',#7988,#7989,#340,.T.);
#10018=EDGE_CURVE('',#7989,#7990,#6745,.T.);
#10019=EDGE_CURVE('',#7990,#7991,#341,.T.);
#10020=EDGE_CURVE('',#7991,#7992,#4900,.T.);
#10021=EDGE_CURVE('',#7992,#7993,#342,.T.);
#10022=EDGE_CURVE('',#7993,#7994,#6746,.T.);
#10023=EDGE_CURVE('',#7994,#7995,#343,.T.);
#10024=EDGE_CURVE('',#7995,#7996,#4901,.T.);
#10025=EDGE_CURVE('',#7996,#7997,#344,.T.);
#10026=EDGE_CURVE('',#7997,#7998,#6747,.T.);
#10027=EDGE_CURVE('',#7998,#7999,#345,.T.);
#10028=EDGE_CURVE('',#7999,#8000,#4902,.T.);
#10029=EDGE_CURVE('',#8000,#8001,#346,.T.);
#10030=EDGE_CURVE('',#8001,#8002,#6748,.T.);
#10031=EDGE_CURVE('',#8002,#8003,#347,.T.);
#10032=EDGE_CURVE('',#8003,#8004,#4903,.T.);
#10033=EDGE_CURVE('',#8004,#8005,#348,.T.);
#10034=EDGE_CURVE('',#8005,#8006,#6749,.T.);
#10035=EDGE_CURVE('',#8006,#8007,#349,.T.);
#10036=EDGE_CURVE('',#8007,#8008,#4904,.T.);
#10037=EDGE_CURVE('',#8008,#8009,#350,.T.);
#10038=EDGE_CURVE('',#8009,#8010,#6750,.T.);
#10039=EDGE_CURVE('',#8010,#8011,#351,.T.);
#10040=EDGE_CURVE('',#8011,#8012,#4905,.T.);
#10041=EDGE_CURVE('',#8012,#8013,#352,.T.);
#10042=EDGE_CURVE('',#8013,#8014,#6751,.T.);
#10043=EDGE_CURVE('',#8014,#8015,#353,.T.);
#10044=EDGE_CURVE('',#8015,#8016,#4906,.T.);
#10045=EDGE_CURVE('',#8016,#8017,#354,.T.);
#10046=EDGE_CURVE('',#8017,#8018,#6752,.T.);
#10047=EDGE_CURVE('',#8018,#8019,#355,.T.);
#10048=EDGE_CURVE('',#8019,#8020,#4907,.T.);
#10049=EDGE_CURVE('',#8020,#8021,#356,.T.);
#10050=EDGE_CURVE('',#8021,#8022,#6753,.T.);
#10051=EDGE_CURVE('',#8022,#8023,#357,.T.);
#10052=EDGE_CURVE('',#8023,#8024,#4908,.T.);
#10053=EDGE_CURVE('',#8024,#8025,#358,.T.);
#10054=EDGE_CURVE('',#8025,#8026,#6754,.T.);
#10055=EDGE_CURVE('',#8026,#8027,#359,.T.);
#10056=EDGE_CURVE('',#8027,#8028,#4909,.T.);
#10057=EDGE_CURVE('',#8028,#8029,#360,.T.);
#10058=EDGE_CURVE('',#8029,#8030,#6755,.T.);
#10059=EDGE_CURVE('',#8030,#8031,#361,.T.);
#10060=EDGE_CURVE('',#8031,#8032,#4910,.T.);
#10061=EDGE_CURVE('',#8032,#8033,#362,.T.);
#10062=EDGE_CURVE('',#8033,#8034,#6756,.T.);
#10063=EDGE_CURVE('',#8034,#8035,#363,.T.);
#10064=EDGE_CURVE('',#8035,#8036,#4911,.T.);
#10065=EDGE_CURVE('',#8036,#8037,#364,.T.);
#10066=EDGE_CURVE('',#8037,#8038,#6757,.T.);
#10067=EDGE_CURVE('',#8038,#8039,#365,.T.);
#10068=EDGE_CURVE('',#8039,#8040,#4912,.T.);
#10069=EDGE_CURVE('',#8040,#8041,#366,.T.);
#10070=EDGE_CURVE('',#8041,#8042,#6758,.T.);
#10071=EDGE_CURVE('',#8042,#8043,#367,.T.);
#10072=EDGE_CURVE('',#8043,#8044,#4913,.T.);
#10073=EDGE_CURVE('',#8044,#8045,#368,.T.);
#10074=EDGE_CURVE('',#8045,#8046,#6759,.T.);
#10075=EDGE_CURVE('',#8046,#8047,#369,.T.);
#10076=EDGE_CURVE('',#8047,#8048,#4914,.T.);
#10077=EDGE_CURVE('',#8048,#8049,#370,.T.);
#10078=EDGE_CURVE('',#8049,#8050,#6760,.T.);
#10079=EDGE_CURVE('',#8050,#8051,#371,.T.);
#10080=EDGE_CURVE('',#8051,#8052,#4915,.T.);
#10081=EDGE_CURVE('',#8052,#8053,#372,.T.);
#10082=EDGE_CURVE('',#8053,#8054,#6761,.T.);
#10083=EDGE_CURVE('',#8054,#8055,#373,.T.);
#10084=EDGE_CURVE('',#8055,#8056,#4916,.T.);
#10085=EDGE_CURVE('',#8056,#8057,#374,.T.);
#10086=EDGE_CURVE('',#8057,#8058,#6762,.T.);
#10087=EDGE_CURVE('',#8058,#8059,#375,.T.);
#10088=EDGE_CURVE('',#8059,#8060,#4917,.T.);
#10089=EDGE_CURVE('',#8060,#8061,#376,.T.);
#10090=EDGE_CURVE('',#8061,#8062,#6763,.T.);
#10091=EDGE_CURVE('',#8062,#8063,#377,.T.);
#10092=EDGE_CURVE('',#8063,#8064,#4918,.T.);
#10093=EDGE_CURVE('',#8064,#8065,#378,.T.);
#10094=EDGE_CURVE('',#8065,#8066,#6764,.T.);
#10095=EDGE_CURVE('',#8066,#8067,#379,.T.);
#10096=EDGE_CURVE('',#8067,#8068,#4919,.T.);
#10097=EDGE_CURVE('',#8068,#8069,#380,.T.);
#10098=EDGE_CURVE('',#8069,#8070,#6765,.T.);
#10099=EDGE_CURVE('',#8070,#8071,#381,.T.);
#10100=EDGE_CURVE('',#8071,#8072,#4920,.T.);
#10101=EDGE_CURVE('',#8072,#8073,#382,.T.);
#10102=EDGE_CURVE('',#8073,#8074,#6766,.T.);
#10103=EDGE_CURVE('',#8074,#8075,#383,.T.);
#10104=EDGE_CURVE('',#8075,#8076,#4921,.T.);
#10105=EDGE_CURVE('',#8076,#8077,#384,.T.);
#10106=EDGE_CURVE('',#8077,#8078,#6767,.T.);
#10107=EDGE_CURVE('',#8078,#8079,#385,.T.);
#10108=EDGE_CURVE('',#8079,#8080,#4922,.T.);
#10109=EDGE_CURVE('',#8080,#8081,#386,.T.);
#10110=EDGE_CURVE('',#8081,#8082,#6768,.T.);
#10111=EDGE_CURVE('',#8082,#8083,#387,.T.);
#10112=EDGE_CURVE('',#8083,#8084,#4923,.T.);
#10113=EDGE_CURVE('',#8084,#8085,#388,.T.);
#10114=EDGE_CURVE('',#8085,#8086,#6769,.T.);
#10115=EDGE_CURVE('',#8086,#8087,#389,.T.);
#10116=EDGE_CURVE('',#8087,#8088,#4924,.T.);
#10117=EDGE_CURVE('',#8088,#8089,#390,.T.);
#10118=EDGE_CURVE('',#8089,#8090,#6770,.T.);
#10119=EDGE_CURVE('',#8090,#8091,#391,.T.);
#10120=EDGE_CURVE('',#8091,#8092,#4925,.T.);
#10121=EDGE_CURVE('',#8092,#8093,#392,.T.);
#10122=EDGE_CURVE('',#8093,#8094,#6771,.T.);
#10123=EDGE_CURVE('',#8094,#8095,#393,.T.);
#10124=EDGE_CURVE('',#8095,#8096,#4926,.T.);
#10125=EDGE_CURVE('',#8096,#8097,#394,.T.);
#10126=EDGE_CURVE('',#8097,#8098,#6772,.T.);
#10127=EDGE_CURVE('',#8098,#8099,#395,.T.);
#10128=EDGE_CURVE('',#8099,#8100,#4927,.T.);
#10129=EDGE_CURVE('',#8100,#8101,#396,.T.);
#10130=EDGE_CURVE('',#8101,#8102,#6773,.T.);
#10131=EDGE_CURVE('',#8102,#8103,#397,.T.);
#10132=EDGE_CURVE('',#8103,#8104,#4928,.T.);
#10133=EDGE_CURVE('',#8104,#8105,#398,.T.);
#10134=EDGE_CURVE('',#8105,#8106,#6774,.T.);
#10135=EDGE_CURVE('',#8106,#8107,#399,.T.);
#10136=EDGE_CURVE('',#8107,#8108,#4929,.T.);
#10137=EDGE_CURVE('',#8108,#8109,#400,.T.);
#10138=EDGE_CURVE('',#8109,#8110,#6775,.T.);
#10139=EDGE_CURVE('',#8110,#8111,#401,.T.);
#10140=EDGE_CURVE('',#8111,#8112,#4930,.T.);
#10141=EDGE_CURVE('',#8112,#8113,#402,.T.);
#10142=EDGE_CURVE('',#8113,#8114,#6776,.T.);
#10143=EDGE_CURVE('',#8114,#8115,#403,.T.);
#10144=EDGE_CURVE('',#8115,#8116,#4931,.T.);
#10145=EDGE_CURVE('',#8116,#8117,#404,.T.);
#10146=EDGE_CURVE('',#8117,#8118,#6777,.T.);
#10147=EDGE_CURVE('',#8118,#8119,#405,.T.);
#10148=EDGE_CURVE('',#8119,#8120,#4932,.T.);
#10149=EDGE_CURVE('',#8120,#8121,#406,.T.);
#10150=EDGE_CURVE('',#8121,#8122,#6778,.T.);
#10151=EDGE_CURVE('',#8122,#8123,#407,.T.);
#10152=EDGE_CURVE('',#8123,#8124,#4933,.T.);
#10153=EDGE_CURVE('',#8124,#8125,#408,.T.);
#10154=EDGE_CURVE('',#8125,#8126,#6779,.T.);
#10155=EDGE_CURVE('',#8126,#8127,#409,.T.);
#10156=EDGE_CURVE('',#8127,#8128,#4934,.T.);
#10157=EDGE_CURVE('',#8128,#7969,#410,.T.);
#10158=EDGE_CURVE('',#7968,#7964,#6780,.T.);
#10159=EDGE_CURVE('',#7962,#7967,#6781,.T.);
#10160=EDGE_CURVE('',#8129,#8129,#6782,.T.);
#10161=EDGE_CURVE('',#8129,#8130,#4935,.T.);
#10162=EDGE_CURVE('',#8130,#8130,#6783,.T.);
#10163=EDGE_CURVE('',#8131,#8126,#987,.T.);
#10164=EDGE_CURVE('',#8132,#8131,#411,.T.);
#10165=EDGE_CURVE('',#8127,#8132,#4936,.T.);
#10166=EDGE_CURVE('',#7969,#8133,#988,.T.);
#10167=EDGE_CURVE('',#8128,#8134,#4937,.T.);
#10168=EDGE_CURVE('',#8133,#8134,#412,.T.);
#10169=EDGE_CURVE('',#8134,#8132,#4938,.T.);
#10170=EDGE_CURVE('',#8135,#8133,#6784,.T.);
#10171=EDGE_CURVE('',#8135,#7970,#989,.T.);
#10172=EDGE_CURVE('',#8136,#8135,#413,.T.);
#10173=EDGE_CURVE('',#7971,#8136,#4939,.T.);
#10174=EDGE_CURVE('',#7973,#8137,#990,.T.);
#10175=EDGE_CURVE('',#7972,#8138,#4940,.T.);
#10176=EDGE_CURVE('',#8137,#8138,#414,.T.);
#10177=EDGE_CURVE('',#8138,#8136,#4941,.T.);
#10178=EDGE_CURVE('',#8139,#8137,#6785,.T.);
#10179=EDGE_CURVE('',#8139,#7974,#991,.T.);
#10180=EDGE_CURVE('',#8140,#8139,#415,.T.);
#10181=EDGE_CURVE('',#7975,#8140,#4942,.T.);
#10182=EDGE_CURVE('',#7977,#8141,#992,.T.);
#10183=EDGE_CURVE('',#7976,#8142,#4943,.T.);
#10184=EDGE_CURVE('',#8141,#8142,#416,.T.);
#10185=EDGE_CURVE('',#8142,#8140,#4944,.T.);
#10186=EDGE_CURVE('',#8143,#8141,#6786,.T.);
#10187=EDGE_CURVE('',#8143,#7978,#993,.T.);
#10188=EDGE_CURVE('',#8144,#8143,#417,.T.);
#10189=EDGE_CURVE('',#7979,#8144,#4945,.T.);
#10190=EDGE_CURVE('',#7981,#8145,#994,.T.);
#10191=EDGE_CURVE('',#7980,#8146,#4946,.T.);
#10192=EDGE_CURVE('',#8145,#8146,#418,.T.);
#10193=EDGE_CURVE('',#8146,#8144,#4947,.T.);
#10194=EDGE_CURVE('',#8147,#8145,#6787,.T.);
#10195=EDGE_CURVE('',#8147,#7982,#995,.T.);
#10196=EDGE_CURVE('',#8148,#8147,#419,.T.);
#10197=EDGE_CURVE('',#7983,#8148,#4948,.T.);
#10198=EDGE_CURVE('',#7985,#8149,#996,.T.);
#10199=EDGE_CURVE('',#7984,#8150,#4949,.T.);
#10200=EDGE_CURVE('',#8149,#8150,#420,.T.);
#10201=EDGE_CURVE('',#8150,#8148,#4950,.T.);
#10202=EDGE_CURVE('',#8151,#8149,#6788,.T.);
#10203=EDGE_CURVE('',#8151,#7986,#997,.T.);
#10204=EDGE_CURVE('',#8152,#8151,#421,.T.);
#10205=EDGE_CURVE('',#7987,#8152,#4951,.T.);
#10206=EDGE_CURVE('',#7989,#8153,#998,.T.);
#10207=EDGE_CURVE('',#7988,#8154,#4952,.T.);
#10208=EDGE_CURVE('',#8153,#8154,#422,.T.);
#10209=EDGE_CURVE('',#8154,#8152,#4953,.T.);
#10210=EDGE_CURVE('',#8155,#8153,#6789,.T.);
#10211=EDGE_CURVE('',#8155,#7990,#999,.T.);
#10212=EDGE_CURVE('',#8156,#8155,#423,.T.);
#10213=EDGE_CURVE('',#7991,#8156,#4954,.T.);
#10214=EDGE_CURVE('',#7993,#8157,#1000,.T.);
#10215=EDGE_CURVE('',#7992,#8158,#4955,.T.);
#10216=EDGE_CURVE('',#8157,#8158,#424,.T.);
#10217=EDGE_CURVE('',#8158,#8156,#4956,.T.);
#10218=EDGE_CURVE('',#8159,#8157,#6790,.T.);
#10219=EDGE_CURVE('',#8159,#7994,#1001,.T.);
#10220=EDGE_CURVE('',#8160,#8159,#425,.T.);
#10221=EDGE_CURVE('',#7995,#8160,#4957,.T.);
#10222=EDGE_CURVE('',#7997,#8161,#1002,.T.);
#10223=EDGE_CURVE('',#7996,#8162,#4958,.T.);
#10224=EDGE_CURVE('',#8161,#8162,#426,.T.);
#10225=EDGE_CURVE('',#8162,#8160,#4959,.T.);
#10226=EDGE_CURVE('',#8163,#8161,#6791,.T.);
#10227=EDGE_CURVE('',#8163,#7998,#1003,.T.);
#10228=EDGE_CURVE('',#8164,#8163,#427,.T.);
#10229=EDGE_CURVE('',#7999,#8164,#4960,.T.);
#10230=EDGE_CURVE('',#8001,#8165,#1004,.T.);
#10231=EDGE_CURVE('',#8000,#8166,#4961,.T.);
#10232=EDGE_CURVE('',#8165,#8166,#428,.T.);
#10233=EDGE_CURVE('',#8166,#8164,#4962,.T.);
#10234=EDGE_CURVE('',#8167,#8165,#6792,.T.);
#10235=EDGE_CURVE('',#8167,#8002,#1005,.T.);
#10236=EDGE_CURVE('',#8168,#8167,#429,.T.);
#10237=EDGE_CURVE('',#8003,#8168,#4963,.T.);
#10238=EDGE_CURVE('',#8005,#8169,#1006,.T.);
#10239=EDGE_CURVE('',#8004,#8170,#4964,.T.);
#10240=EDGE_CURVE('',#8169,#8170,#430,.T.);
#10241=EDGE_CURVE('',#8170,#8168,#4965,.T.);
#10242=EDGE_CURVE('',#8171,#8169,#6793,.T.);
#10243=EDGE_CURVE('',#8171,#8006,#1007,.T.);
#10244=EDGE_CURVE('',#8172,#8171,#431,.T.);
#10245=EDGE_CURVE('',#8007,#8172,#4966,.T.);
#10246=EDGE_CURVE('',#8009,#8173,#1008,.T.);
#10247=EDGE_CURVE('',#8008,#8174,#4967,.T.);
#10248=EDGE_CURVE('',#8173,#8174,#432,.T.);
#10249=EDGE_CURVE('',#8174,#8172,#4968,.T.);
#10250=EDGE_CURVE('',#8175,#8173,#6794,.T.);
#10251=EDGE_CURVE('',#8175,#8010,#1009,.T.);
#10252=EDGE_CURVE('',#8176,#8175,#433,.T.);
#10253=EDGE_CURVE('',#8011,#8176,#4969,.T.);
#10254=EDGE_CURVE('',#8013,#8177,#1010,.T.);
#10255=EDGE_CURVE('',#8012,#8178,#4970,.T.);
#10256=EDGE_CURVE('',#8177,#8178,#434,.T.);
#10257=EDGE_CURVE('',#8178,#8176,#4971,.T.);
#10258=EDGE_CURVE('',#8179,#8177,#6795,.T.);
#10259=EDGE_CURVE('',#8179,#8014,#1011,.T.);
#10260=EDGE_CURVE('',#8180,#8179,#435,.T.);
#10261=EDGE_CURVE('',#8015,#8180,#4972,.T.);
#10262=EDGE_CURVE('',#8017,#8181,#1012,.T.);
#10263=EDGE_CURVE('',#8016,#8182,#4973,.T.);
#10264=EDGE_CURVE('',#8181,#8182,#436,.T.);
#10265=EDGE_CURVE('',#8182,#8180,#4974,.T.);
#10266=EDGE_CURVE('',#8183,#8181,#6796,.T.);
#10267=EDGE_CURVE('',#8183,#8018,#1013,.T.);
#10268=EDGE_CURVE('',#8184,#8183,#437,.T.);
#10269=EDGE_CURVE('',#8019,#8184,#4975,.T.);
#10270=EDGE_CURVE('',#8021,#8185,#1014,.T.);
#10271=EDGE_CURVE('',#8020,#8186,#4976,.T.);
#10272=EDGE_CURVE('',#8185,#8186,#438,.T.);
#10273=EDGE_CURVE('',#8186,#8184,#4977,.T.);
#10274=EDGE_CURVE('',#8187,#8185,#6797,.T.);
#10275=EDGE_CURVE('',#8187,#8022,#1015,.T.);
#10276=EDGE_CURVE('',#8188,#8187,#439,.T.);
#10277=EDGE_CURVE('',#8023,#8188,#4978,.T.);
#10278=EDGE_CURVE('',#8025,#8189,#1016,.T.);
#10279=EDGE_CURVE('',#8024,#8190,#4979,.T.);
#10280=EDGE_CURVE('',#8189,#8190,#440,.T.);
#10281=EDGE_CURVE('',#8190,#8188,#4980,.T.);
#10282=EDGE_CURVE('',#8191,#8189,#6798,.T.);
#10283=EDGE_CURVE('',#8191,#8026,#1017,.T.);
#10284=EDGE_CURVE('',#8192,#8191,#441,.T.);
#10285=EDGE_CURVE('',#8027,#8192,#4981,.T.);
#10286=EDGE_CURVE('',#8029,#8193,#1018,.T.);
#10287=EDGE_CURVE('',#8028,#8194,#4982,.T.);
#10288=EDGE_CURVE('',#8193,#8194,#442,.T.);
#10289=EDGE_CURVE('',#8194,#8192,#4983,.T.);
#10290=EDGE_CURVE('',#8195,#8193,#6799,.T.);
#10291=EDGE_CURVE('',#8195,#8030,#1019,.T.);
#10292=EDGE_CURVE('',#8196,#8195,#443,.T.);
#10293=EDGE_CURVE('',#8031,#8196,#4984,.T.);
#10294=EDGE_CURVE('',#8033,#8197,#1020,.T.);
#10295=EDGE_CURVE('',#8032,#8198,#4985,.T.);
#10296=EDGE_CURVE('',#8197,#8198,#444,.T.);
#10297=EDGE_CURVE('',#8198,#8196,#4986,.T.);
#10298=EDGE_CURVE('',#8199,#8197,#6800,.T.);
#10299=EDGE_CURVE('',#8199,#8034,#1021,.T.);
#10300=EDGE_CURVE('',#8200,#8199,#445,.T.);
#10301=EDGE_CURVE('',#8035,#8200,#4987,.T.);
#10302=EDGE_CURVE('',#8037,#8201,#1022,.T.);
#10303=EDGE_CURVE('',#8036,#8202,#4988,.T.);
#10304=EDGE_CURVE('',#8201,#8202,#446,.T.);
#10305=EDGE_CURVE('',#8202,#8200,#4989,.T.);
#10306=EDGE_CURVE('',#8203,#8201,#6801,.T.);
#10307=EDGE_CURVE('',#8203,#8038,#1023,.T.);
#10308=EDGE_CURVE('',#8204,#8203,#447,.T.);
#10309=EDGE_CURVE('',#8039,#8204,#4990,.T.);
#10310=EDGE_CURVE('',#8041,#8205,#1024,.T.);
#10311=EDGE_CURVE('',#8040,#8206,#4991,.T.);
#10312=EDGE_CURVE('',#8205,#8206,#448,.T.);
#10313=EDGE_CURVE('',#8206,#8204,#4992,.T.);
#10314=EDGE_CURVE('',#8207,#8205,#6802,.T.);
#10315=EDGE_CURVE('',#8207,#8042,#1025,.T.);
#10316=EDGE_CURVE('',#8208,#8207,#449,.T.);
#10317=EDGE_CURVE('',#8043,#8208,#4993,.T.);
#10318=EDGE_CURVE('',#8045,#8209,#1026,.T.);
#10319=EDGE_CURVE('',#8044,#8210,#4994,.T.);
#10320=EDGE_CURVE('',#8209,#8210,#450,.T.);
#10321=EDGE_CURVE('',#8210,#8208,#4995,.T.);
#10322=EDGE_CURVE('',#8211,#8209,#6803,.T.);
#10323=EDGE_CURVE('',#8211,#8046,#1027,.T.);
#10324=EDGE_CURVE('',#8212,#8211,#451,.T.);
#10325=EDGE_CURVE('',#8047,#8212,#4996,.T.);
#10326=EDGE_CURVE('',#8049,#8213,#1028,.T.);
#10327=EDGE_CURVE('',#8048,#8214,#4997,.T.);
#10328=EDGE_CURVE('',#8213,#8214,#452,.T.);
#10329=EDGE_CURVE('',#8214,#8212,#4998,.T.);
#10330=EDGE_CURVE('',#8215,#8213,#6804,.T.);
#10331=EDGE_CURVE('',#8215,#8050,#1029,.T.);
#10332=EDGE_CURVE('',#8216,#8215,#453,.T.);
#10333=EDGE_CURVE('',#8051,#8216,#4999,.T.);
#10334=EDGE_CURVE('',#8053,#8217,#1030,.T.);
#10335=EDGE_CURVE('',#8052,#8218,#5000,.T.);
#10336=EDGE_CURVE('',#8217,#8218,#454,.T.);
#10337=EDGE_CURVE('',#8218,#8216,#5001,.T.);
#10338=EDGE_CURVE('',#8219,#8217,#6805,.T.);
#10339=EDGE_CURVE('',#8219,#8054,#1031,.T.);
#10340=EDGE_CURVE('',#8220,#8219,#455,.T.);
#10341=EDGE_CURVE('',#8055,#8220,#5002,.T.);
#10342=EDGE_CURVE('',#8057,#8221,#1032,.T.);
#10343=EDGE_CURVE('',#8056,#8222,#5003,.T.);
#10344=EDGE_CURVE('',#8221,#8222,#456,.T.);
#10345=EDGE_CURVE('',#8222,#8220,#5004,.T.);
#10346=EDGE_CURVE('',#8223,#8221,#6806,.T.);
#10347=EDGE_CURVE('',#8223,#8058,#1033,.T.);
#10348=EDGE_CURVE('',#8224,#8223,#457,.T.);
#10349=EDGE_CURVE('',#8059,#8224,#5005,.T.);
#10350=EDGE_CURVE('',#8061,#8225,#1034,.T.);
#10351=EDGE_CURVE('',#8060,#8226,#5006,.T.);
#10352=EDGE_CURVE('',#8225,#8226,#458,.T.);
#10353=EDGE_CURVE('',#8226,#8224,#5007,.T.);
#10354=EDGE_CURVE('',#8227,#8225,#6807,.T.);
#10355=EDGE_CURVE('',#8227,#8062,#1035,.T.);
#10356=EDGE_CURVE('',#8228,#8227,#459,.T.);
#10357=EDGE_CURVE('',#8063,#8228,#5008,.T.);
#10358=EDGE_CURVE('',#8065,#8229,#1036,.T.);
#10359=EDGE_CURVE('',#8064,#8230,#5009,.T.);
#10360=EDGE_CURVE('',#8229,#8230,#460,.T.);
#10361=EDGE_CURVE('',#8230,#8228,#5010,.T.);
#10362=EDGE_CURVE('',#8231,#8229,#6808,.T.);
#10363=EDGE_CURVE('',#8231,#8066,#1037,.T.);
#10364=EDGE_CURVE('',#8232,#8231,#461,.T.);
#10365=EDGE_CURVE('',#8067,#8232,#5011,.T.);
#10366=EDGE_CURVE('',#8069,#8233,#1038,.T.);
#10367=EDGE_CURVE('',#8068,#8234,#5012,.T.);
#10368=EDGE_CURVE('',#8233,#8234,#462,.T.);
#10369=EDGE_CURVE('',#8234,#8232,#5013,.T.);
#10370=EDGE_CURVE('',#8235,#8233,#6809,.T.);
#10371=EDGE_CURVE('',#8235,#8070,#1039,.T.);
#10372=EDGE_CURVE('',#8236,#8235,#463,.T.);
#10373=EDGE_CURVE('',#8071,#8236,#5014,.T.);
#10374=EDGE_CURVE('',#8073,#8237,#1040,.T.);
#10375=EDGE_CURVE('',#8072,#8238,#5015,.T.);
#10376=EDGE_CURVE('',#8237,#8238,#464,.T.);
#10377=EDGE_CURVE('',#8238,#8236,#5016,.T.);
#10378=EDGE_CURVE('',#8239,#8237,#6810,.T.);
#10379=EDGE_CURVE('',#8239,#8074,#1041,.T.);
#10380=EDGE_CURVE('',#8240,#8239,#465,.T.);
#10381=EDGE_CURVE('',#8075,#8240,#5017,.T.);
#10382=EDGE_CURVE('',#8077,#8241,#1042,.T.);
#10383=EDGE_CURVE('',#8076,#8242,#5018,.T.);
#10384=EDGE_CURVE('',#8241,#8242,#466,.T.);
#10385=EDGE_CURVE('',#8242,#8240,#5019,.T.);
#10386=EDGE_CURVE('',#8243,#8241,#6811,.T.);
#10387=EDGE_CURVE('',#8243,#8078,#1043,.T.);
#10388=EDGE_CURVE('',#8244,#8243,#467,.T.);
#10389=EDGE_CURVE('',#8079,#8244,#5020,.T.);
#10390=EDGE_CURVE('',#8081,#8245,#1044,.T.);
#10391=EDGE_CURVE('',#8080,#8246,#5021,.T.);
#10392=EDGE_CURVE('',#8245,#8246,#468,.T.);
#10393=EDGE_CURVE('',#8246,#8244,#5022,.T.);
#10394=EDGE_CURVE('',#8247,#8245,#6812,.T.);
#10395=EDGE_CURVE('',#8247,#8082,#1045,.T.);
#10396=EDGE_CURVE('',#8248,#8247,#469,.T.);
#10397=EDGE_CURVE('',#8083,#8248,#5023,.T.);
#10398=EDGE_CURVE('',#8085,#8249,#1046,.T.);
#10399=EDGE_CURVE('',#8084,#8250,#5024,.T.);
#10400=EDGE_CURVE('',#8249,#8250,#470,.T.);
#10401=EDGE_CURVE('',#8250,#8248,#5025,.T.);
#10402=EDGE_CURVE('',#8251,#8249,#6813,.T.);
#10403=EDGE_CURVE('',#8251,#8086,#1047,.T.);
#10404=EDGE_CURVE('',#8252,#8251,#471,.T.);
#10405=EDGE_CURVE('',#8087,#8252,#5026,.T.);
#10406=EDGE_CURVE('',#8089,#8253,#1048,.T.);
#10407=EDGE_CURVE('',#8088,#8254,#5027,.T.);
#10408=EDGE_CURVE('',#8253,#8254,#472,.T.);
#10409=EDGE_CURVE('',#8254,#8252,#5028,.T.);
#10410=EDGE_CURVE('',#8255,#8253,#6814,.T.);
#10411=EDGE_CURVE('',#8255,#8090,#1049,.T.);
#10412=EDGE_CURVE('',#8256,#8255,#473,.T.);
#10413=EDGE_CURVE('',#8091,#8256,#5029,.T.);
#10414=EDGE_CURVE('',#8093,#8257,#1050,.T.);
#10415=EDGE_CURVE('',#8092,#8258,#5030,.T.);
#10416=EDGE_CURVE('',#8257,#8258,#474,.T.);
#10417=EDGE_CURVE('',#8258,#8256,#5031,.T.);
#10418=EDGE_CURVE('',#8259,#8257,#6815,.T.);
#10419=EDGE_CURVE('',#8259,#8094,#1051,.T.);
#10420=EDGE_CURVE('',#8260,#8259,#475,.T.);
#10421=EDGE_CURVE('',#8095,#8260,#5032,.T.);
#10422=EDGE_CURVE('',#8097,#8261,#1052,.T.);
#10423=EDGE_CURVE('',#8096,#8262,#5033,.T.);
#10424=EDGE_CURVE('',#8261,#8262,#476,.T.);
#10425=EDGE_CURVE('',#8262,#8260,#5034,.T.);
#10426=EDGE_CURVE('',#8263,#8261,#6816,.T.);
#10427=EDGE_CURVE('',#8263,#8098,#1053,.T.);
#10428=EDGE_CURVE('',#8264,#8263,#477,.T.);
#10429=EDGE_CURVE('',#8099,#8264,#5035,.T.);
#10430=EDGE_CURVE('',#8101,#8265,#1054,.T.);
#10431=EDGE_CURVE('',#8100,#8266,#5036,.T.);
#10432=EDGE_CURVE('',#8265,#8266,#478,.T.);
#10433=EDGE_CURVE('',#8266,#8264,#5037,.T.);
#10434=EDGE_CURVE('',#8267,#8265,#6817,.T.);
#10435=EDGE_CURVE('',#8267,#8102,#1055,.T.);
#10436=EDGE_CURVE('',#8268,#8267,#479,.T.);
#10437=EDGE_CURVE('',#8103,#8268,#5038,.T.);
#10438=EDGE_CURVE('',#8105,#8269,#1056,.T.);
#10439=EDGE_CURVE('',#8104,#8270,#5039,.T.);
#10440=EDGE_CURVE('',#8269,#8270,#480,.T.);
#10441=EDGE_CURVE('',#8270,#8268,#5040,.T.);
#10442=EDGE_CURVE('',#8271,#8269,#6818,.T.);
#10443=EDGE_CURVE('',#8271,#8106,#1057,.T.);
#10444=EDGE_CURVE('',#8272,#8271,#481,.T.);
#10445=EDGE_CURVE('',#8107,#8272,#5041,.T.);
#10446=EDGE_CURVE('',#8109,#8273,#1058,.T.);
#10447=EDGE_CURVE('',#8108,#8274,#5042,.T.);
#10448=EDGE_CURVE('',#8273,#8274,#482,.T.);
#10449=EDGE_CURVE('',#8274,#8272,#5043,.T.);
#10450=EDGE_CURVE('',#8275,#8273,#6819,.T.);
#10451=EDGE_CURVE('',#8275,#8110,#1059,.T.);
#10452=EDGE_CURVE('',#8276,#8275,#483,.T.);
#10453=EDGE_CURVE('',#8111,#8276,#5044,.T.);
#10454=EDGE_CURVE('',#8113,#8277,#1060,.T.);
#10455=EDGE_CURVE('',#8112,#8278,#5045,.T.);
#10456=EDGE_CURVE('',#8277,#8278,#484,.T.);
#10457=EDGE_CURVE('',#8278,#8276,#5046,.T.);
#10458=EDGE_CURVE('',#8279,#8277,#6820,.T.);
#10459=EDGE_CURVE('',#8279,#8114,#1061,.T.);
#10460=EDGE_CURVE('',#8280,#8279,#485,.T.);
#10461=EDGE_CURVE('',#8115,#8280,#5047,.T.);
#10462=EDGE_CURVE('',#8117,#8281,#1062,.T.);
#10463=EDGE_CURVE('',#8116,#8282,#5048,.T.);
#10464=EDGE_CURVE('',#8281,#8282,#486,.T.);
#10465=EDGE_CURVE('',#8282,#8280,#5049,.T.);
#10466=EDGE_CURVE('',#8283,#8281,#6821,.T.);
#10467=EDGE_CURVE('',#8283,#8118,#1063,.T.);
#10468=EDGE_CURVE('',#8284,#8283,#487,.T.);
#10469=EDGE_CURVE('',#8119,#8284,#5050,.T.);
#10470=EDGE_CURVE('',#8285,#8284,#5051,.T.);
#10471=EDGE_CURVE('',#8120,#8285,#5052,.T.);
#10472=EDGE_CURVE('',#8121,#8286,#1064,.T.);
#10473=EDGE_CURVE('',#8286,#8285,#488,.T.);
#10474=EDGE_CURVE('',#8287,#8286,#6822,.T.);
#10475=EDGE_CURVE('',#8287,#8122,#1065,.T.);
#10476=EDGE_CURVE('',#8125,#8288,#1066,.T.);
#10477=EDGE_CURVE('',#8124,#8289,#5053,.T.);
#10478=EDGE_CURVE('',#8288,#8289,#489,.T.);
#10479=EDGE_CURVE('',#8290,#8287,#490,.T.);
#10480=EDGE_CURVE('',#8123,#8290,#5054,.T.);
#10481=EDGE_CURVE('',#8289,#8290,#5055,.T.);
#10482=EDGE_CURVE('',#8131,#8288,#6823,.T.);
#10483=EDGE_CURVE('',#8291,#8292,#5056,.T.);
#10484=EDGE_CURVE('',#8293,#8291,#5057,.T.);
#10485=EDGE_CURVE('',#8294,#8293,#5058,.T.);
#10486=EDGE_CURVE('',#8295,#8294,#5059,.T.);
#10487=EDGE_CURVE('',#8296,#8295,#5060,.T.);
#10488=EDGE_CURVE('',#8297,#8296,#5061,.T.);
#10489=EDGE_CURVE('',#8298,#8297,#5062,.T.);
#10490=EDGE_CURVE('',#8292,#8298,#5063,.T.);
#10491=EDGE_CURVE('',#8295,#8299,#5064,.T.);
#10492=EDGE_CURVE('',#8299,#8300,#5065,.T.);
#10493=EDGE_CURVE('',#8300,#8296,#5066,.T.);
#10494=EDGE_CURVE('',#8301,#8294,#5067,.T.);
#10495=EDGE_CURVE('',#8301,#8299,#5068,.T.);
#10496=EDGE_CURVE('',#8293,#8302,#5069,.T.);
#10497=EDGE_CURVE('',#8302,#8301,#5070,.T.);
#10498=EDGE_CURVE('',#8303,#8291,#5071,.T.);
#10499=EDGE_CURVE('',#8303,#8302,#5072,.T.);
#10500=EDGE_CURVE('',#8304,#8305,#5073,.T.);
#10501=EDGE_CURVE('',#8300,#8304,#5074,.T.);
#10502=EDGE_CURVE('',#8306,#8303,#5075,.T.);
#10503=EDGE_CURVE('',#8305,#8306,#5076,.T.);
#10504=EDGE_CURVE('',#8297,#8304,#5077,.T.);
#10505=EDGE_CURVE('',#8292,#8306,#5078,.T.);
#10506=EDGE_CURVE('',#8305,#8298,#5079,.T.);
#10507=ORIENTED_EDGE('',*,*,#8307,.F.);
#10508=ORIENTED_EDGE('',*,*,#8308,.T.);
#10509=ORIENTED_EDGE('',*,*,#8309,.F.);
#10510=ORIENTED_EDGE('',*,*,#8308,.F.);
#10511=ORIENTED_EDGE('',*,*,#8310,.F.);
#10512=ORIENTED_EDGE('',*,*,#8311,.T.);
#10513=ORIENTED_EDGE('',*,*,#8312,.F.);
#10514=ORIENTED_EDGE('',*,*,#8311,.F.);
#10515=ORIENTED_EDGE('',*,*,#8313,.F.);
#10516=ORIENTED_EDGE('',*,*,#8314,.T.);
#10517=ORIENTED_EDGE('',*,*,#8315,.F.);
#10518=ORIENTED_EDGE('',*,*,#8314,.F.);
#10519=ORIENTED_EDGE('',*,*,#8316,.F.);
#10520=ORIENTED_EDGE('',*,*,#8317,.T.);
#10521=ORIENTED_EDGE('',*,*,#8318,.F.);
#10522=ORIENTED_EDGE('',*,*,#8317,.F.);
#10523=ORIENTED_EDGE('',*,*,#8319,.T.);
#10524=ORIENTED_EDGE('',*,*,#8320,.T.);
#10525=ORIENTED_EDGE('',*,*,#8321,.F.);
#10526=ORIENTED_EDGE('',*,*,#8322,.F.);
#10527=ORIENTED_EDGE('',*,*,#8323,.T.);
#10528=ORIENTED_EDGE('',*,*,#8322,.T.);
#10529=ORIENTED_EDGE('',*,*,#8324,.F.);
#10530=ORIENTED_EDGE('',*,*,#8325,.F.);
#10531=ORIENTED_EDGE('',*,*,#8326,.T.);
#10532=ORIENTED_EDGE('',*,*,#8325,.T.);
#10533=ORIENTED_EDGE('',*,*,#8327,.F.);
#10534=ORIENTED_EDGE('',*,*,#8328,.F.);
#10535=ORIENTED_EDGE('',*,*,#8329,.T.);
#10536=ORIENTED_EDGE('',*,*,#8328,.T.);
#10537=ORIENTED_EDGE('',*,*,#8330,.F.);
#10538=ORIENTED_EDGE('',*,*,#8320,.F.);
#10539=ORIENTED_EDGE('',*,*,#8330,.T.);
#10540=ORIENTED_EDGE('',*,*,#8327,.T.);
#10541=ORIENTED_EDGE('',*,*,#8324,.T.);
#10542=ORIENTED_EDGE('',*,*,#8321,.T.);
#10543=ORIENTED_EDGE('',*,*,#8309,.T.);
#10544=ORIENTED_EDGE('',*,*,#8312,.T.);
#10545=ORIENTED_EDGE('',*,*,#8315,.T.);
#10546=ORIENTED_EDGE('',*,*,#8318,.T.);
#10547=ORIENTED_EDGE('',*,*,#8329,.F.);
#10548=ORIENTED_EDGE('',*,*,#8319,.F.);
#10549=ORIENTED_EDGE('',*,*,#8323,.F.);
#10550=ORIENTED_EDGE('',*,*,#8326,.F.);
#10551=ORIENTED_EDGE('',*,*,#8307,.T.);
#10552=ORIENTED_EDGE('',*,*,#8310,.T.);
#10553=ORIENTED_EDGE('',*,*,#8313,.T.);
#10554=ORIENTED_EDGE('',*,*,#8316,.T.);
#10555=ORIENTED_EDGE('',*,*,#8331,.F.);
#10556=ORIENTED_EDGE('',*,*,#8332,.T.);
#10557=ORIENTED_EDGE('',*,*,#8333,.F.);
#10558=ORIENTED_EDGE('',*,*,#8332,.F.);
#10559=ORIENTED_EDGE('',*,*,#8331,.T.);
#10560=ORIENTED_EDGE('',*,*,#8334,.F.);
#10561=ORIENTED_EDGE('',*,*,#8335,.T.);
#10562=ORIENTED_EDGE('',*,*,#8336,.F.);
#10563=ORIENTED_EDGE('',*,*,#8335,.F.);
#10564=ORIENTED_EDGE('',*,*,#8334,.T.);
#10565=ORIENTED_EDGE('',*,*,#8337,.F.);
#10566=ORIENTED_EDGE('',*,*,#8338,.T.);
#10567=ORIENTED_EDGE('',*,*,#8339,.T.);
#10568=ORIENTED_EDGE('',*,*,#8338,.F.);
#10569=ORIENTED_EDGE('',*,*,#8339,.F.);
#10570=ORIENTED_EDGE('',*,*,#8340,.F.);
#10571=ORIENTED_EDGE('',*,*,#8341,.T.);
#10572=ORIENTED_EDGE('',*,*,#8342,.T.);
#10573=ORIENTED_EDGE('',*,*,#8341,.F.);
#10574=ORIENTED_EDGE('',*,*,#8342,.F.);
#10575=ORIENTED_EDGE('',*,*,#8343,.F.);
#10576=ORIENTED_EDGE('',*,*,#8344,.F.);
#10577=ORIENTED_EDGE('',*,*,#8345,.F.);
#10578=ORIENTED_EDGE('',*,*,#8346,.F.);
#10579=ORIENTED_EDGE('',*,*,#8347,.F.);
#10580=ORIENTED_EDGE('',*,*,#8348,.F.);
#10581=ORIENTED_EDGE('',*,*,#8349,.F.);
#10582=ORIENTED_EDGE('',*,*,#8344,.T.);
#10583=ORIENTED_EDGE('',*,*,#8346,.T.);
#10584=ORIENTED_EDGE('',*,*,#8350,.F.);
#10585=ORIENTED_EDGE('',*,*,#8351,.F.);
#10586=ORIENTED_EDGE('',*,*,#8352,.T.);
#10587=ORIENTED_EDGE('',*,*,#8353,.F.);
#10588=ORIENTED_EDGE('',*,*,#8354,.T.);
#10589=ORIENTED_EDGE('',*,*,#8355,.T.);
#10590=ORIENTED_EDGE('',*,*,#8356,.T.);
#10591=ORIENTED_EDGE('',*,*,#8357,.T.);
#10592=ORIENTED_EDGE('',*,*,#8358,.F.);
#10593=ORIENTED_EDGE('',*,*,#8359,.T.);
#10594=ORIENTED_EDGE('',*,*,#8360,.F.);
#10595=ORIENTED_EDGE('',*,*,#8361,.T.);
#10596=ORIENTED_EDGE('',*,*,#8362,.F.);
#10597=ORIENTED_EDGE('',*,*,#8333,.T.);
#10598=ORIENTED_EDGE('',*,*,#8336,.T.);
#10599=ORIENTED_EDGE('',*,*,#8363,.T.);
#10600=ORIENTED_EDGE('',*,*,#8364,.T.);
#10601=ORIENTED_EDGE('',*,*,#8365,.T.);
#10602=ORIENTED_EDGE('',*,*,#8366,.T.);
#10603=ORIENTED_EDGE('',*,*,#8345,.T.);
#10604=ORIENTED_EDGE('',*,*,#8349,.T.);
#10605=ORIENTED_EDGE('',*,*,#8367,.T.);
#10606=ORIENTED_EDGE('',*,*,#8368,.T.);
#10607=ORIENTED_EDGE('',*,*,#8369,.T.);
#10608=ORIENTED_EDGE('',*,*,#8370,.T.);
#10609=ORIENTED_EDGE('',*,*,#8371,.T.);
#10610=ORIENTED_EDGE('',*,*,#8372,.T.);
#10611=ORIENTED_EDGE('',*,*,#8373,.T.);
#10612=ORIENTED_EDGE('',*,*,#8374,.T.);
#10613=ORIENTED_EDGE('',*,*,#8375,.T.);
#10614=ORIENTED_EDGE('',*,*,#8350,.T.);
#10615=ORIENTED_EDGE('',*,*,#8376,.T.);
#10616=ORIENTED_EDGE('',*,*,#8377,.T.);
#10617=ORIENTED_EDGE('',*,*,#8378,.T.);
#10618=ORIENTED_EDGE('',*,*,#8379,.T.);
#10619=ORIENTED_EDGE('',*,*,#8380,.T.);
#10620=ORIENTED_EDGE('',*,*,#8373,.F.);
#10621=ORIENTED_EDGE('',*,*,#8381,.T.);
#10622=ORIENTED_EDGE('',*,*,#8382,.F.);
#10623=ORIENTED_EDGE('',*,*,#8383,.F.);
#10624=ORIENTED_EDGE('',*,*,#8372,.F.);
#10625=ORIENTED_EDGE('',*,*,#8384,.F.);
#10626=ORIENTED_EDGE('',*,*,#8385,.F.);
#10627=ORIENTED_EDGE('',*,*,#8381,.F.);
#10628=ORIENTED_EDGE('',*,*,#8383,.T.);
#10629=ORIENTED_EDGE('',*,*,#8386,.F.);
#10630=ORIENTED_EDGE('',*,*,#8387,.T.);
#10631=ORIENTED_EDGE('',*,*,#8388,.F.);
#10632=ORIENTED_EDGE('',*,*,#8389,.T.);
#10633=ORIENTED_EDGE('',*,*,#8390,.F.);
#10634=ORIENTED_EDGE('',*,*,#8391,.F.);
#10635=ORIENTED_EDGE('',*,*,#8392,.T.);
#10636=ORIENTED_EDGE('',*,*,#8393,.F.);
#10637=ORIENTED_EDGE('',*,*,#8394,.T.);
#10638=ORIENTED_EDGE('',*,*,#8395,.T.);
#10639=ORIENTED_EDGE('',*,*,#8396,.T.);
#10640=ORIENTED_EDGE('',*,*,#8397,.T.);
#10641=ORIENTED_EDGE('',*,*,#8374,.F.);
#10642=ORIENTED_EDGE('',*,*,#8337,.T.);
#10643=ORIENTED_EDGE('',*,*,#8340,.T.);
#10644=ORIENTED_EDGE('',*,*,#8398,.T.);
#10645=ORIENTED_EDGE('',*,*,#8399,.T.);
#10646=ORIENTED_EDGE('',*,*,#8400,.T.);
#10647=ORIENTED_EDGE('',*,*,#8401,.T.);
#10648=ORIENTED_EDGE('',*,*,#8382,.T.);
#10649=ORIENTED_EDGE('',*,*,#8385,.T.);
#10650=ORIENTED_EDGE('',*,*,#8402,.T.);
#10651=ORIENTED_EDGE('',*,*,#8403,.T.);
#10652=ORIENTED_EDGE('',*,*,#8404,.T.);
#10653=ORIENTED_EDGE('',*,*,#8405,.T.);
#10654=ORIENTED_EDGE('',*,*,#8406,.T.);
#10655=ORIENTED_EDGE('',*,*,#8386,.T.);
#10656=ORIENTED_EDGE('',*,*,#8384,.T.);
#10657=ORIENTED_EDGE('',*,*,#8371,.F.);
#10658=ORIENTED_EDGE('',*,*,#8407,.F.);
#10659=ORIENTED_EDGE('',*,*,#8402,.F.);
#10660=ORIENTED_EDGE('',*,*,#8348,.T.);
#10661=ORIENTED_EDGE('',*,*,#8408,.F.);
#10662=ORIENTED_EDGE('',*,*,#8409,.F.);
#10663=ORIENTED_EDGE('',*,*,#8367,.F.);
#10664=ORIENTED_EDGE('',*,*,#8409,.T.);
#10665=ORIENTED_EDGE('',*,*,#8410,.F.);
#10666=ORIENTED_EDGE('',*,*,#8411,.T.);
#10667=ORIENTED_EDGE('',*,*,#8412,.F.);
#10668=ORIENTED_EDGE('',*,*,#8413,.T.);
#10669=ORIENTED_EDGE('',*,*,#8414,.F.);
#10670=ORIENTED_EDGE('',*,*,#8415,.F.);
#10671=ORIENTED_EDGE('',*,*,#8416,.F.);
#10672=ORIENTED_EDGE('',*,*,#8417,.T.);
#10673=ORIENTED_EDGE('',*,*,#8368,.F.);
#10674=ORIENTED_EDGE('',*,*,#8343,.T.);
#10675=ORIENTED_EDGE('',*,*,#8362,.T.);
#10676=ORIENTED_EDGE('',*,*,#8418,.T.);
#10677=ORIENTED_EDGE('',*,*,#8419,.T.);
#10678=ORIENTED_EDGE('',*,*,#8420,.T.);
#10679=ORIENTED_EDGE('',*,*,#8410,.T.);
#10680=ORIENTED_EDGE('',*,*,#8408,.T.);
#10681=ORIENTED_EDGE('',*,*,#8347,.T.);
#10682=ORIENTED_EDGE('',*,*,#8421,.F.);
#10683=ORIENTED_EDGE('',*,*,#8422,.T.);
#10684=ORIENTED_EDGE('',*,*,#8366,.F.);
#10685=ORIENTED_EDGE('',*,*,#8422,.F.);
#10686=ORIENTED_EDGE('',*,*,#8421,.T.);
#10687=ORIENTED_EDGE('',*,*,#8423,.F.);
#10688=ORIENTED_EDGE('',*,*,#8424,.T.);
#10689=ORIENTED_EDGE('',*,*,#8365,.F.);
#10690=ORIENTED_EDGE('',*,*,#8424,.F.);
#10691=ORIENTED_EDGE('',*,*,#8423,.T.);
#10692=ORIENTED_EDGE('',*,*,#8398,.F.);
#10693=ORIENTED_EDGE('',*,*,#8425,.T.);
#10694=ORIENTED_EDGE('',*,*,#8426,.T.);
#10695=ORIENTED_EDGE('',*,*,#8425,.F.);
#10696=ORIENTED_EDGE('',*,*,#8426,.F.);
#10697=ORIENTED_EDGE('',*,*,#8399,.F.);
#10698=ORIENTED_EDGE('',*,*,#8427,.T.);
#10699=ORIENTED_EDGE('',*,*,#8428,.T.);
#10700=ORIENTED_EDGE('',*,*,#8427,.F.);
#10701=ORIENTED_EDGE('',*,*,#8428,.F.);
#10702=ORIENTED_EDGE('',*,*,#8429,.F.);
#10703=ORIENTED_EDGE('',*,*,#8430,.F.);
#10704=ORIENTED_EDGE('',*,*,#8418,.F.);
#10705=ORIENTED_EDGE('',*,*,#8361,.F.);
#10706=ORIENTED_EDGE('',*,*,#8431,.F.);
#10707=ORIENTED_EDGE('',*,*,#8432,.F.);
#10708=ORIENTED_EDGE('',*,*,#8419,.F.);
#10709=ORIENTED_EDGE('',*,*,#8430,.T.);
#10710=ORIENTED_EDGE('',*,*,#8406,.F.);
#10711=ORIENTED_EDGE('',*,*,#8433,.T.);
#10712=ORIENTED_EDGE('',*,*,#8434,.F.);
#10713=ORIENTED_EDGE('',*,*,#8387,.F.);
#10714=ORIENTED_EDGE('',*,*,#8405,.F.);
#10715=ORIENTED_EDGE('',*,*,#8435,.F.);
#10716=ORIENTED_EDGE('',*,*,#8436,.F.);
#10717=ORIENTED_EDGE('',*,*,#8433,.F.);
#10718=ORIENTED_EDGE('',*,*,#8434,.T.);
#10719=ORIENTED_EDGE('',*,*,#8436,.T.);
#10720=ORIENTED_EDGE('',*,*,#8437,.T.);
#10721=ORIENTED_EDGE('',*,*,#8438,.T.);
#10722=ORIENTED_EDGE('',*,*,#8439,.T.);
#10723=ORIENTED_EDGE('',*,*,#8440,.T.);
#10724=ORIENTED_EDGE('',*,*,#8441,.T.);
#10725=ORIENTED_EDGE('',*,*,#8388,.T.);
#10726=ORIENTED_EDGE('',*,*,#8432,.T.);
#10727=ORIENTED_EDGE('',*,*,#8442,.F.);
#10728=ORIENTED_EDGE('',*,*,#8411,.F.);
#10729=ORIENTED_EDGE('',*,*,#8420,.F.);
#10730=ORIENTED_EDGE('',*,*,#8435,.T.);
#10731=ORIENTED_EDGE('',*,*,#8404,.F.);
#10732=ORIENTED_EDGE('',*,*,#8443,.F.);
#10733=ORIENTED_EDGE('',*,*,#8437,.F.);
#10734=ORIENTED_EDGE('',*,*,#8407,.T.);
#10735=ORIENTED_EDGE('',*,*,#8370,.F.);
#10736=ORIENTED_EDGE('',*,*,#8444,.F.);
#10737=ORIENTED_EDGE('',*,*,#8445,.F.);
#10738=ORIENTED_EDGE('',*,*,#8446,.T.);
#10739=ORIENTED_EDGE('',*,*,#8447,.F.);
#10740=ORIENTED_EDGE('',*,*,#8448,.T.);
#10741=ORIENTED_EDGE('',*,*,#8438,.F.);
#10742=ORIENTED_EDGE('',*,*,#8443,.T.);
#10743=ORIENTED_EDGE('',*,*,#8403,.F.);
#10744=ORIENTED_EDGE('',*,*,#8429,.T.);
#10745=ORIENTED_EDGE('',*,*,#8360,.T.);
#10746=ORIENTED_EDGE('',*,*,#8449,.T.);
#10747=ORIENTED_EDGE('',*,*,#8450,.T.);
#10748=ORIENTED_EDGE('',*,*,#8451,.T.);
#10749=ORIENTED_EDGE('',*,*,#8412,.T.);
#10750=ORIENTED_EDGE('',*,*,#8442,.T.);
#10751=ORIENTED_EDGE('',*,*,#8431,.T.);
#10752=ORIENTED_EDGE('',*,*,#8452,.F.);
#10753=ORIENTED_EDGE('',*,*,#8453,.T.);
#10754=ORIENTED_EDGE('',*,*,#8364,.F.);
#10755=ORIENTED_EDGE('',*,*,#8453,.F.);
#10756=ORIENTED_EDGE('',*,*,#8452,.T.);
#10757=ORIENTED_EDGE('',*,*,#8454,.F.);
#10758=ORIENTED_EDGE('',*,*,#8455,.T.);
#10759=ORIENTED_EDGE('',*,*,#8363,.F.);
#10760=ORIENTED_EDGE('',*,*,#8455,.F.);
#10761=ORIENTED_EDGE('',*,*,#8454,.T.);
#10762=ORIENTED_EDGE('',*,*,#8401,.F.);
#10763=ORIENTED_EDGE('',*,*,#8456,.T.);
#10764=ORIENTED_EDGE('',*,*,#8457,.T.);
#10765=ORIENTED_EDGE('',*,*,#8456,.F.);
#10766=ORIENTED_EDGE('',*,*,#8457,.F.);
#10767=ORIENTED_EDGE('',*,*,#8400,.F.);
#10768=ORIENTED_EDGE('',*,*,#8458,.T.);
#10769=ORIENTED_EDGE('',*,*,#8459,.T.);
#10770=ORIENTED_EDGE('',*,*,#8458,.F.);
#10771=ORIENTED_EDGE('',*,*,#8459,.F.);
#10772=ORIENTED_EDGE('',*,*,#8460,.F.);
#10773=ORIENTED_EDGE('',*,*,#8461,.F.);
#10774=ORIENTED_EDGE('',*,*,#8449,.F.);
#10775=ORIENTED_EDGE('',*,*,#8359,.F.);
#10776=ORIENTED_EDGE('',*,*,#8462,.F.);
#10777=ORIENTED_EDGE('',*,*,#8463,.F.);
#10778=ORIENTED_EDGE('',*,*,#8450,.F.);
#10779=ORIENTED_EDGE('',*,*,#8461,.T.);
#10780=ORIENTED_EDGE('',*,*,#8462,.T.);
#10781=ORIENTED_EDGE('',*,*,#8460,.T.);
#10782=ORIENTED_EDGE('',*,*,#8358,.T.);
#10783=ORIENTED_EDGE('',*,*,#8464,.T.);
#10784=ORIENTED_EDGE('',*,*,#8390,.T.);
#10785=ORIENTED_EDGE('',*,*,#8465,.T.);
#10786=ORIENTED_EDGE('',*,*,#8466,.T.);
#10787=ORIENTED_EDGE('',*,*,#8467,.T.);
#10788=ORIENTED_EDGE('',*,*,#8447,.T.);
#10789=ORIENTED_EDGE('',*,*,#8468,.T.);
#10790=ORIENTED_EDGE('',*,*,#8414,.T.);
#10791=ORIENTED_EDGE('',*,*,#8469,.T.);
#10792=ORIENTED_EDGE('',*,*,#8470,.T.);
#10793=ORIENTED_EDGE('',*,*,#8471,.T.);
#10794=ORIENTED_EDGE('',*,*,#8472,.T.);
#10795=ORIENTED_EDGE('',*,*,#8473,.T.);
#10796=ORIENTED_EDGE('',*,*,#8474,.T.);
#10797=ORIENTED_EDGE('',*,*,#8441,.F.);
#10798=ORIENTED_EDGE('',*,*,#8475,.T.);
#10799=ORIENTED_EDGE('',*,*,#8465,.F.);
#10800=ORIENTED_EDGE('',*,*,#8389,.F.);
#10801=ORIENTED_EDGE('',*,*,#8440,.F.);
#10802=ORIENTED_EDGE('',*,*,#8476,.F.);
#10803=ORIENTED_EDGE('',*,*,#8466,.F.);
#10804=ORIENTED_EDGE('',*,*,#8475,.F.);
#10805=ORIENTED_EDGE('',*,*,#8476,.T.);
#10806=ORIENTED_EDGE('',*,*,#8439,.F.);
#10807=ORIENTED_EDGE('',*,*,#8448,.F.);
#10808=ORIENTED_EDGE('',*,*,#8467,.F.);
#10809=ORIENTED_EDGE('',*,*,#8463,.T.);
#10810=ORIENTED_EDGE('',*,*,#8469,.F.);
#10811=ORIENTED_EDGE('',*,*,#8413,.F.);
#10812=ORIENTED_EDGE('',*,*,#8451,.F.);
#10813=ORIENTED_EDGE('',*,*,#8477,.F.);
#10814=ORIENTED_EDGE('',*,*,#8478,.T.);
#10815=ORIENTED_EDGE('',*,*,#8479,.F.);
#10816=ORIENTED_EDGE('',*,*,#8478,.F.);
#10817=ORIENTED_EDGE('',*,*,#8477,.T.);
#10818=ORIENTED_EDGE('',*,*,#8480,.F.);
#10819=ORIENTED_EDGE('',*,*,#8481,.F.);
#10820=ORIENTED_EDGE('',*,*,#8482,.T.);
#10821=ORIENTED_EDGE('',*,*,#8483,.F.);
#10822=ORIENTED_EDGE('',*,*,#8482,.F.);
#10823=ORIENTED_EDGE('',*,*,#8481,.T.);
#10824=ORIENTED_EDGE('',*,*,#8484,.F.);
#10825=ORIENTED_EDGE('',*,*,#8485,.F.);
#10826=ORIENTED_EDGE('',*,*,#8486,.T.);
#10827=ORIENTED_EDGE('',*,*,#8487,.F.);
#10828=ORIENTED_EDGE('',*,*,#8486,.F.);
#10829=ORIENTED_EDGE('',*,*,#8485,.T.);
#10830=ORIENTED_EDGE('',*,*,#8488,.F.);
#10831=ORIENTED_EDGE('',*,*,#8489,.F.);
#10832=ORIENTED_EDGE('',*,*,#8490,.T.);
#10833=ORIENTED_EDGE('',*,*,#8491,.F.);
#10834=ORIENTED_EDGE('',*,*,#8490,.F.);
#10835=ORIENTED_EDGE('',*,*,#8489,.T.);
#10836=ORIENTED_EDGE('',*,*,#8492,.F.);
#10837=ORIENTED_EDGE('',*,*,#8493,.F.);
#10838=ORIENTED_EDGE('',*,*,#8494,.T.);
#10839=ORIENTED_EDGE('',*,*,#8480,.T.);
#10840=ORIENTED_EDGE('',*,*,#8494,.F.);
#10841=ORIENTED_EDGE('',*,*,#8495,.F.);
#10842=ORIENTED_EDGE('',*,*,#8496,.T.);
#10843=ORIENTED_EDGE('',*,*,#8484,.T.);
#10844=ORIENTED_EDGE('',*,*,#8496,.F.);
#10845=ORIENTED_EDGE('',*,*,#8497,.F.);
#10846=ORIENTED_EDGE('',*,*,#8498,.T.);
#10847=ORIENTED_EDGE('',*,*,#8488,.T.);
#10848=ORIENTED_EDGE('',*,*,#8498,.F.);
#10849=ORIENTED_EDGE('',*,*,#8499,.F.);
#10850=ORIENTED_EDGE('',*,*,#8500,.T.);
#10851=ORIENTED_EDGE('',*,*,#8492,.T.);
#10852=ORIENTED_EDGE('',*,*,#8500,.F.);
#10853=ORIENTED_EDGE('',*,*,#8501,.F.);
#10854=ORIENTED_EDGE('',*,*,#8502,.T.);
#10855=ORIENTED_EDGE('',*,*,#8376,.F.);
#10856=ORIENTED_EDGE('',*,*,#8502,.F.);
#10857=ORIENTED_EDGE('',*,*,#8501,.T.);
#10858=ORIENTED_EDGE('',*,*,#8503,.F.);
#10859=ORIENTED_EDGE('',*,*,#8504,.T.);
#10860=ORIENTED_EDGE('',*,*,#8380,.F.);
#10861=ORIENTED_EDGE('',*,*,#8504,.F.);
#10862=ORIENTED_EDGE('',*,*,#8503,.T.);
#10863=ORIENTED_EDGE('',*,*,#8505,.F.);
#10864=ORIENTED_EDGE('',*,*,#8506,.T.);
#10865=ORIENTED_EDGE('',*,*,#8470,.F.);
#10866=ORIENTED_EDGE('',*,*,#8506,.F.);
#10867=ORIENTED_EDGE('',*,*,#8505,.T.);
#10868=ORIENTED_EDGE('',*,*,#8507,.F.);
#10869=ORIENTED_EDGE('',*,*,#8508,.T.);
#10870=ORIENTED_EDGE('',*,*,#8474,.F.);
#10871=ORIENTED_EDGE('',*,*,#8508,.F.);
#10872=ORIENTED_EDGE('',*,*,#8507,.T.);
#10873=ORIENTED_EDGE('',*,*,#8509,.F.);
#10874=ORIENTED_EDGE('',*,*,#8510,.T.);
#10875=ORIENTED_EDGE('',*,*,#8377,.F.);
#10876=ORIENTED_EDGE('',*,*,#8510,.F.);
#10877=ORIENTED_EDGE('',*,*,#8511,.F.);
#10878=ORIENTED_EDGE('',*,*,#8512,.T.);
#10879=ORIENTED_EDGE('',*,*,#8471,.F.);
#10880=ORIENTED_EDGE('',*,*,#8512,.F.);
#10881=ORIENTED_EDGE('',*,*,#8513,.F.);
#10882=ORIENTED_EDGE('',*,*,#8514,.T.);
#10883=ORIENTED_EDGE('',*,*,#8472,.F.);
#10884=ORIENTED_EDGE('',*,*,#8514,.F.);
#10885=ORIENTED_EDGE('',*,*,#8515,.F.);
#10886=ORIENTED_EDGE('',*,*,#8516,.T.);
#10887=ORIENTED_EDGE('',*,*,#8473,.F.);
#10888=ORIENTED_EDGE('',*,*,#8516,.F.);
#10889=ORIENTED_EDGE('',*,*,#8517,.F.);
#10890=ORIENTED_EDGE('',*,*,#8518,.T.);
#10891=ORIENTED_EDGE('',*,*,#8378,.F.);
#10892=ORIENTED_EDGE('',*,*,#8518,.F.);
#10893=ORIENTED_EDGE('',*,*,#8519,.F.);
#10894=ORIENTED_EDGE('',*,*,#8520,.T.);
#10895=ORIENTED_EDGE('',*,*,#8379,.F.);
#10896=ORIENTED_EDGE('',*,*,#8520,.F.);
#10897=ORIENTED_EDGE('',*,*,#8521,.T.);
#10898=ORIENTED_EDGE('',*,*,#8351,.T.);
#10899=ORIENTED_EDGE('',*,*,#8375,.F.);
#10900=ORIENTED_EDGE('',*,*,#8397,.F.);
#10901=ORIENTED_EDGE('',*,*,#8522,.F.);
#10902=ORIENTED_EDGE('',*,*,#8352,.F.);
#10903=ORIENTED_EDGE('',*,*,#8521,.F.);
#10904=ORIENTED_EDGE('',*,*,#8396,.F.);
#10905=ORIENTED_EDGE('',*,*,#8509,.T.);
#10906=ORIENTED_EDGE('',*,*,#8517,.T.);
#10907=ORIENTED_EDGE('',*,*,#8519,.T.);
#10908=ORIENTED_EDGE('',*,*,#8522,.T.);
#10909=ORIENTED_EDGE('',*,*,#8395,.F.);
#10910=ORIENTED_EDGE('',*,*,#8523,.T.);
#10911=ORIENTED_EDGE('',*,*,#8353,.T.);
#10912=ORIENTED_EDGE('',*,*,#8524,.T.);
#10913=ORIENTED_EDGE('',*,*,#8391,.T.);
#10914=ORIENTED_EDGE('',*,*,#8464,.F.);
#10915=ORIENTED_EDGE('',*,*,#8357,.F.);
#10916=ORIENTED_EDGE('',*,*,#8524,.F.);
#10917=ORIENTED_EDGE('',*,*,#8356,.F.);
#10918=ORIENTED_EDGE('',*,*,#8525,.F.);
#10919=ORIENTED_EDGE('',*,*,#8392,.F.);
#10920=ORIENTED_EDGE('',*,*,#8511,.T.);
#10921=ORIENTED_EDGE('',*,*,#8513,.T.);
#10922=ORIENTED_EDGE('',*,*,#8515,.T.);
#10923=ORIENTED_EDGE('',*,*,#8468,.F.);
#10924=ORIENTED_EDGE('',*,*,#8446,.F.);
#10925=ORIENTED_EDGE('',*,*,#8526,.F.);
#10926=ORIENTED_EDGE('',*,*,#8415,.T.);
#10927=ORIENTED_EDGE('',*,*,#8369,.F.);
#10928=ORIENTED_EDGE('',*,*,#8417,.F.);
#10929=ORIENTED_EDGE('',*,*,#8527,.F.);
#10930=ORIENTED_EDGE('',*,*,#8444,.T.);
#10931=ORIENTED_EDGE('',*,*,#8526,.T.);
#10932=ORIENTED_EDGE('',*,*,#8445,.T.);
#10933=ORIENTED_EDGE('',*,*,#8527,.T.);
#10934=ORIENTED_EDGE('',*,*,#8416,.T.);
#10935=ORIENTED_EDGE('',*,*,#8491,.T.);
#10936=ORIENTED_EDGE('',*,*,#8487,.T.);
#10937=ORIENTED_EDGE('',*,*,#8483,.T.);
#10938=ORIENTED_EDGE('',*,*,#8479,.T.);
#10939=ORIENTED_EDGE('',*,*,#8525,.T.);
#10940=ORIENTED_EDGE('',*,*,#8355,.F.);
#10941=ORIENTED_EDGE('',*,*,#8528,.T.);
#10942=ORIENTED_EDGE('',*,*,#8393,.T.);
#10943=ORIENTED_EDGE('',*,*,#8528,.F.);
#10944=ORIENTED_EDGE('',*,*,#8354,.F.);
#10945=ORIENTED_EDGE('',*,*,#8523,.F.);
#10946=ORIENTED_EDGE('',*,*,#8394,.F.);
#10947=ORIENTED_EDGE('',*,*,#8493,.T.);
#10948=ORIENTED_EDGE('',*,*,#8495,.T.);
#10949=ORIENTED_EDGE('',*,*,#8497,.T.);
#10950=ORIENTED_EDGE('',*,*,#8499,.T.);
#10951=ORIENTED_EDGE('',*,*,#8529,.F.);
#10952=ORIENTED_EDGE('',*,*,#8530,.T.);
#10953=ORIENTED_EDGE('',*,*,#8531,.F.);
#10954=ORIENTED_EDGE('',*,*,#8530,.F.);
#10955=ORIENTED_EDGE('',*,*,#8532,.F.);
#10956=ORIENTED_EDGE('',*,*,#8533,.T.);
#10957=ORIENTED_EDGE('',*,*,#8534,.F.);
#10958=ORIENTED_EDGE('',*,*,#8533,.F.);
#10959=ORIENTED_EDGE('',*,*,#8535,.F.);
#10960=ORIENTED_EDGE('',*,*,#8536,.T.);
#10961=ORIENTED_EDGE('',*,*,#8537,.F.);
#10962=ORIENTED_EDGE('',*,*,#8536,.F.);
#10963=ORIENTED_EDGE('',*,*,#8538,.F.);
#10964=ORIENTED_EDGE('',*,*,#8539,.T.);
#10965=ORIENTED_EDGE('',*,*,#8540,.F.);
#10966=ORIENTED_EDGE('',*,*,#8539,.F.);
#10967=ORIENTED_EDGE('',*,*,#8541,.F.);
#10968=ORIENTED_EDGE('',*,*,#8542,.T.);
#10969=ORIENTED_EDGE('',*,*,#8543,.F.);
#10970=ORIENTED_EDGE('',*,*,#8544,.F.);
#10971=ORIENTED_EDGE('',*,*,#8545,.F.);
#10972=ORIENTED_EDGE('',*,*,#8544,.T.);
#10973=ORIENTED_EDGE('',*,*,#8546,.F.);
#10974=ORIENTED_EDGE('',*,*,#8547,.F.);
#10975=ORIENTED_EDGE('',*,*,#8548,.F.);
#10976=ORIENTED_EDGE('',*,*,#8547,.T.);
#10977=ORIENTED_EDGE('',*,*,#8549,.F.);
#10978=ORIENTED_EDGE('',*,*,#8550,.F.);
#10979=ORIENTED_EDGE('',*,*,#8551,.F.);
#10980=ORIENTED_EDGE('',*,*,#8550,.T.);
#10981=ORIENTED_EDGE('',*,*,#8552,.F.);
#10982=ORIENTED_EDGE('',*,*,#8542,.F.);
#10983=ORIENTED_EDGE('',*,*,#8553,.F.);
#10984=ORIENTED_EDGE('',*,*,#8554,.T.);
#10985=ORIENTED_EDGE('',*,*,#8555,.F.);
#10986=ORIENTED_EDGE('',*,*,#8554,.F.);
#10987=ORIENTED_EDGE('',*,*,#8553,.T.);
#10988=ORIENTED_EDGE('',*,*,#8556,.F.);
#10989=ORIENTED_EDGE('',*,*,#8557,.T.);
#10990=ORIENTED_EDGE('',*,*,#8558,.F.);
#10991=ORIENTED_EDGE('',*,*,#8557,.F.);
#10992=ORIENTED_EDGE('',*,*,#8556,.T.);
#10993=ORIENTED_EDGE('',*,*,#8559,.F.);
#10994=ORIENTED_EDGE('',*,*,#8560,.T.);
#10995=ORIENTED_EDGE('',*,*,#8561,.T.);
#10996=ORIENTED_EDGE('',*,*,#8560,.F.);
#10997=ORIENTED_EDGE('',*,*,#8561,.F.);
#10998=ORIENTED_EDGE('',*,*,#8562,.F.);
#10999=ORIENTED_EDGE('',*,*,#8563,.T.);
#11000=ORIENTED_EDGE('',*,*,#8564,.T.);
#11001=ORIENTED_EDGE('',*,*,#8563,.F.);
#11002=ORIENTED_EDGE('',*,*,#8564,.F.);
#11003=ORIENTED_EDGE('',*,*,#8565,.F.);
#11004=ORIENTED_EDGE('',*,*,#8566,.T.);
#11005=ORIENTED_EDGE('',*,*,#8567,.F.);
#11006=ORIENTED_EDGE('',*,*,#8568,.F.);
#11007=ORIENTED_EDGE('',*,*,#8569,.F.);
#11008=ORIENTED_EDGE('',*,*,#8570,.F.);
#11009=ORIENTED_EDGE('',*,*,#8571,.F.);
#11010=ORIENTED_EDGE('',*,*,#8566,.F.);
#11011=ORIENTED_EDGE('',*,*,#8568,.T.);
#11012=ORIENTED_EDGE('',*,*,#8572,.F.);
#11013=ORIENTED_EDGE('',*,*,#8573,.F.);
#11014=ORIENTED_EDGE('',*,*,#8574,.F.);
#11015=ORIENTED_EDGE('',*,*,#8567,.T.);
#11016=ORIENTED_EDGE('',*,*,#8571,.T.);
#11017=ORIENTED_EDGE('',*,*,#8575,.F.);
#11018=ORIENTED_EDGE('',*,*,#8576,.F.);
#11019=ORIENTED_EDGE('',*,*,#8577,.F.);
#11020=ORIENTED_EDGE('',*,*,#8578,.T.);
#11021=ORIENTED_EDGE('',*,*,#8579,.T.);
#11022=ORIENTED_EDGE('',*,*,#8580,.T.);
#11023=ORIENTED_EDGE('',*,*,#8581,.T.);
#11024=ORIENTED_EDGE('',*,*,#8582,.T.);
#11025=ORIENTED_EDGE('',*,*,#8583,.T.);
#11026=ORIENTED_EDGE('',*,*,#8572,.T.);
#11027=ORIENTED_EDGE('',*,*,#8584,.T.);
#11028=ORIENTED_EDGE('',*,*,#8585,.T.);
#11029=ORIENTED_EDGE('',*,*,#8586,.T.);
#11030=ORIENTED_EDGE('',*,*,#8587,.T.);
#11031=ORIENTED_EDGE('',*,*,#8588,.T.);
#11032=ORIENTED_EDGE('',*,*,#8589,.F.);
#11033=ORIENTED_EDGE('',*,*,#8590,.T.);
#11034=ORIENTED_EDGE('',*,*,#8578,.F.);
#11035=ORIENTED_EDGE('',*,*,#8591,.F.);
#11036=ORIENTED_EDGE('',*,*,#8592,.F.);
#11037=ORIENTED_EDGE('',*,*,#8593,.F.);
#11038=ORIENTED_EDGE('',*,*,#8579,.F.);
#11039=ORIENTED_EDGE('',*,*,#8590,.F.);
#11040=ORIENTED_EDGE('',*,*,#8591,.T.);
#11041=ORIENTED_EDGE('',*,*,#8577,.T.);
#11042=ORIENTED_EDGE('',*,*,#8594,.T.);
#11043=ORIENTED_EDGE('',*,*,#8595,.F.);
#11044=ORIENTED_EDGE('',*,*,#8596,.T.);
#11045=ORIENTED_EDGE('',*,*,#8597,.F.);
#11046=ORIENTED_EDGE('',*,*,#8598,.F.);
#11047=ORIENTED_EDGE('',*,*,#8599,.F.);
#11048=ORIENTED_EDGE('',*,*,#8600,.F.);
#11049=ORIENTED_EDGE('',*,*,#8601,.T.);
#11050=ORIENTED_EDGE('',*,*,#8602,.T.);
#11051=ORIENTED_EDGE('',*,*,#8603,.T.);
#11052=ORIENTED_EDGE('',*,*,#8604,.T.);
#11053=ORIENTED_EDGE('',*,*,#8605,.T.);
#11054=ORIENTED_EDGE('',*,*,#8559,.T.);
#11055=ORIENTED_EDGE('',*,*,#8562,.T.);
#11056=ORIENTED_EDGE('',*,*,#8606,.T.);
#11057=ORIENTED_EDGE('',*,*,#8607,.T.);
#11058=ORIENTED_EDGE('',*,*,#8608,.T.);
#11059=ORIENTED_EDGE('',*,*,#8609,.T.);
#11060=ORIENTED_EDGE('',*,*,#8593,.T.);
#11061=ORIENTED_EDGE('',*,*,#8610,.F.);
#11062=ORIENTED_EDGE('',*,*,#8611,.F.);
#11063=ORIENTED_EDGE('',*,*,#8580,.F.);
#11064=ORIENTED_EDGE('',*,*,#8570,.T.);
#11065=ORIENTED_EDGE('',*,*,#8612,.T.);
#11066=ORIENTED_EDGE('',*,*,#8613,.T.);
#11067=ORIENTED_EDGE('',*,*,#8614,.T.);
#11068=ORIENTED_EDGE('',*,*,#8615,.T.);
#11069=ORIENTED_EDGE('',*,*,#8616,.T.);
#11070=ORIENTED_EDGE('',*,*,#8617,.T.);
#11071=ORIENTED_EDGE('',*,*,#8618,.F.);
#11072=ORIENTED_EDGE('',*,*,#8619,.T.);
#11073=ORIENTED_EDGE('',*,*,#8620,.F.);
#11074=ORIENTED_EDGE('',*,*,#8621,.F.);
#11075=ORIENTED_EDGE('',*,*,#8622,.F.);
#11076=ORIENTED_EDGE('',*,*,#8623,.F.);
#11077=ORIENTED_EDGE('',*,*,#8575,.T.);
#11078=ORIENTED_EDGE('',*,*,#8555,.T.);
#11079=ORIENTED_EDGE('',*,*,#8558,.T.);
#11080=ORIENTED_EDGE('',*,*,#8624,.T.);
#11081=ORIENTED_EDGE('',*,*,#8625,.T.);
#11082=ORIENTED_EDGE('',*,*,#8626,.T.);
#11083=ORIENTED_EDGE('',*,*,#8627,.T.);
#11084=ORIENTED_EDGE('',*,*,#8611,.T.);
#11085=ORIENTED_EDGE('',*,*,#8628,.F.);
#11086=ORIENTED_EDGE('',*,*,#8629,.T.);
#11087=ORIENTED_EDGE('',*,*,#8630,.F.);
#11088=ORIENTED_EDGE('',*,*,#8631,.T.);
#11089=ORIENTED_EDGE('',*,*,#8632,.F.);
#11090=ORIENTED_EDGE('',*,*,#8633,.T.);
#11091=ORIENTED_EDGE('',*,*,#8634,.T.);
#11092=ORIENTED_EDGE('',*,*,#8635,.F.);
#11093=ORIENTED_EDGE('',*,*,#8581,.F.);
#11094=ORIENTED_EDGE('',*,*,#8589,.T.);
#11095=ORIENTED_EDGE('',*,*,#8605,.F.);
#11096=ORIENTED_EDGE('',*,*,#8636,.T.);
#11097=ORIENTED_EDGE('',*,*,#8637,.T.);
#11098=ORIENTED_EDGE('',*,*,#8638,.T.);
#11099=ORIENTED_EDGE('',*,*,#8628,.T.);
#11100=ORIENTED_EDGE('',*,*,#8610,.T.);
#11101=ORIENTED_EDGE('',*,*,#8592,.T.);
#11102=ORIENTED_EDGE('',*,*,#8565,.T.);
#11103=ORIENTED_EDGE('',*,*,#8574,.T.);
#11104=ORIENTED_EDGE('',*,*,#8639,.T.);
#11105=ORIENTED_EDGE('',*,*,#8640,.T.);
#11106=ORIENTED_EDGE('',*,*,#8641,.T.);
#11107=ORIENTED_EDGE('',*,*,#8642,.T.);
#11108=ORIENTED_EDGE('',*,*,#8612,.F.);
#11109=ORIENTED_EDGE('',*,*,#8569,.T.);
#11110=ORIENTED_EDGE('',*,*,#8643,.F.);
#11111=ORIENTED_EDGE('',*,*,#8644,.T.);
#11112=ORIENTED_EDGE('',*,*,#8627,.F.);
#11113=ORIENTED_EDGE('',*,*,#8644,.F.);
#11114=ORIENTED_EDGE('',*,*,#8643,.T.);
#11115=ORIENTED_EDGE('',*,*,#8645,.F.);
#11116=ORIENTED_EDGE('',*,*,#8646,.T.);
#11117=ORIENTED_EDGE('',*,*,#8626,.F.);
#11118=ORIENTED_EDGE('',*,*,#8646,.F.);
#11119=ORIENTED_EDGE('',*,*,#8645,.T.);
#11120=ORIENTED_EDGE('',*,*,#8609,.F.);
#11121=ORIENTED_EDGE('',*,*,#8647,.T.);
#11122=ORIENTED_EDGE('',*,*,#8648,.T.);
#11123=ORIENTED_EDGE('',*,*,#8647,.F.);
#11124=ORIENTED_EDGE('',*,*,#8648,.F.);
#11125=ORIENTED_EDGE('',*,*,#8608,.F.);
#11126=ORIENTED_EDGE('',*,*,#8649,.T.);
#11127=ORIENTED_EDGE('',*,*,#8650,.T.);
#11128=ORIENTED_EDGE('',*,*,#8649,.F.);
#11129=ORIENTED_EDGE('',*,*,#8650,.F.);
#11130=ORIENTED_EDGE('',*,*,#8651,.F.);
#11131=ORIENTED_EDGE('',*,*,#8652,.T.);
#11132=ORIENTED_EDGE('',*,*,#8641,.F.);
#11133=ORIENTED_EDGE('',*,*,#8653,.F.);
#11134=ORIENTED_EDGE('',*,*,#8654,.F.);
#11135=ORIENTED_EDGE('',*,*,#8613,.F.);
#11136=ORIENTED_EDGE('',*,*,#8642,.F.);
#11137=ORIENTED_EDGE('',*,*,#8652,.F.);
#11138=ORIENTED_EDGE('',*,*,#8653,.T.);
#11139=ORIENTED_EDGE('',*,*,#8640,.F.);
#11140=ORIENTED_EDGE('',*,*,#8655,.F.);
#11141=ORIENTED_EDGE('',*,*,#8656,.F.);
#11142=ORIENTED_EDGE('',*,*,#8657,.F.);
#11143=ORIENTED_EDGE('',*,*,#8658,.T.);
#11144=ORIENTED_EDGE('',*,*,#8636,.F.);
#11145=ORIENTED_EDGE('',*,*,#8604,.F.);
#11146=ORIENTED_EDGE('',*,*,#8659,.F.);
#11147=ORIENTED_EDGE('',*,*,#8660,.F.);
#11148=ORIENTED_EDGE('',*,*,#8637,.F.);
#11149=ORIENTED_EDGE('',*,*,#8658,.F.);
#11150=ORIENTED_EDGE('',*,*,#8660,.T.);
#11151=ORIENTED_EDGE('',*,*,#8661,.F.);
#11152=ORIENTED_EDGE('',*,*,#8629,.F.);
#11153=ORIENTED_EDGE('',*,*,#8638,.F.);
#11154=ORIENTED_EDGE('',*,*,#8657,.T.);
#11155=ORIENTED_EDGE('',*,*,#8603,.F.);
#11156=ORIENTED_EDGE('',*,*,#8662,.T.);
#11157=ORIENTED_EDGE('',*,*,#8663,.T.);
#11158=ORIENTED_EDGE('',*,*,#8664,.T.);
#11159=ORIENTED_EDGE('',*,*,#8630,.T.);
#11160=ORIENTED_EDGE('',*,*,#8661,.T.);
#11161=ORIENTED_EDGE('',*,*,#8659,.T.);
#11162=ORIENTED_EDGE('',*,*,#8651,.T.);
#11163=ORIENTED_EDGE('',*,*,#8656,.T.);
#11164=ORIENTED_EDGE('',*,*,#8665,.T.);
#11165=ORIENTED_EDGE('',*,*,#8666,.T.);
#11166=ORIENTED_EDGE('',*,*,#8667,.T.);
#11167=ORIENTED_EDGE('',*,*,#8668,.T.);
#11168=ORIENTED_EDGE('',*,*,#8614,.F.);
#11169=ORIENTED_EDGE('',*,*,#8654,.T.);
#11170=ORIENTED_EDGE('',*,*,#8669,.F.);
#11171=ORIENTED_EDGE('',*,*,#8670,.T.);
#11172=ORIENTED_EDGE('',*,*,#8624,.F.);
#11173=ORIENTED_EDGE('',*,*,#8670,.F.);
#11174=ORIENTED_EDGE('',*,*,#8669,.T.);
#11175=ORIENTED_EDGE('',*,*,#8671,.F.);
#11176=ORIENTED_EDGE('',*,*,#8672,.T.);
#11177=ORIENTED_EDGE('',*,*,#8625,.F.);
#11178=ORIENTED_EDGE('',*,*,#8672,.F.);
#11179=ORIENTED_EDGE('',*,*,#8671,.T.);
#11180=ORIENTED_EDGE('',*,*,#8606,.F.);
#11181=ORIENTED_EDGE('',*,*,#8673,.T.);
#11182=ORIENTED_EDGE('',*,*,#8674,.T.);
#11183=ORIENTED_EDGE('',*,*,#8673,.F.);
#11184=ORIENTED_EDGE('',*,*,#8674,.F.);
#11185=ORIENTED_EDGE('',*,*,#8607,.F.);
#11186=ORIENTED_EDGE('',*,*,#8675,.T.);
#11187=ORIENTED_EDGE('',*,*,#8676,.T.);
#11188=ORIENTED_EDGE('',*,*,#8675,.F.);
#11189=ORIENTED_EDGE('',*,*,#8676,.F.);
#11190=ORIENTED_EDGE('',*,*,#8668,.F.);
#11191=ORIENTED_EDGE('',*,*,#8677,.F.);
#11192=ORIENTED_EDGE('',*,*,#8678,.F.);
#11193=ORIENTED_EDGE('',*,*,#8615,.F.);
#11194=ORIENTED_EDGE('',*,*,#8667,.F.);
#11195=ORIENTED_EDGE('',*,*,#8679,.F.);
#11196=ORIENTED_EDGE('',*,*,#8680,.F.);
#11197=ORIENTED_EDGE('',*,*,#8677,.T.);
#11198=ORIENTED_EDGE('',*,*,#8681,.F.);
#11199=ORIENTED_EDGE('',*,*,#8682,.T.);
#11200=ORIENTED_EDGE('',*,*,#8662,.F.);
#11201=ORIENTED_EDGE('',*,*,#8602,.F.);
#11202=ORIENTED_EDGE('',*,*,#8683,.F.);
#11203=ORIENTED_EDGE('',*,*,#8684,.F.);
#11204=ORIENTED_EDGE('',*,*,#8663,.F.);
#11205=ORIENTED_EDGE('',*,*,#8682,.F.);
#11206=ORIENTED_EDGE('',*,*,#8684,.T.);
#11207=ORIENTED_EDGE('',*,*,#8685,.F.);
#11208=ORIENTED_EDGE('',*,*,#8631,.F.);
#11209=ORIENTED_EDGE('',*,*,#8664,.F.);
#11210=ORIENTED_EDGE('',*,*,#8679,.T.);
#11211=ORIENTED_EDGE('',*,*,#8666,.F.);
#11212=ORIENTED_EDGE('',*,*,#8686,.F.);
#11213=ORIENTED_EDGE('',*,*,#8687,.F.);
#11214=ORIENTED_EDGE('',*,*,#8573,.T.);
#11215=ORIENTED_EDGE('',*,*,#8583,.F.);
#11216=ORIENTED_EDGE('',*,*,#8688,.T.);
#11217=ORIENTED_EDGE('',*,*,#8689,.T.);
#11218=ORIENTED_EDGE('',*,*,#8690,.F.);
#11219=ORIENTED_EDGE('',*,*,#8691,.F.);
#11220=ORIENTED_EDGE('',*,*,#8686,.T.);
#11221=ORIENTED_EDGE('',*,*,#8665,.F.);
#11222=ORIENTED_EDGE('',*,*,#8655,.T.);
#11223=ORIENTED_EDGE('',*,*,#8639,.F.);
#11224=ORIENTED_EDGE('',*,*,#8680,.T.);
#11225=ORIENTED_EDGE('',*,*,#8687,.T.);
#11226=ORIENTED_EDGE('',*,*,#8691,.T.);
#11227=ORIENTED_EDGE('',*,*,#8692,.T.);
#11228=ORIENTED_EDGE('',*,*,#8632,.T.);
#11229=ORIENTED_EDGE('',*,*,#8685,.T.);
#11230=ORIENTED_EDGE('',*,*,#8683,.T.);
#11231=ORIENTED_EDGE('',*,*,#8681,.T.);
#11232=ORIENTED_EDGE('',*,*,#8601,.F.);
#11233=ORIENTED_EDGE('',*,*,#8693,.F.);
#11234=ORIENTED_EDGE('',*,*,#8616,.F.);
#11235=ORIENTED_EDGE('',*,*,#8678,.T.);
#11236=ORIENTED_EDGE('',*,*,#8694,.T.);
#11237=ORIENTED_EDGE('',*,*,#8695,.T.);
#11238=ORIENTED_EDGE('',*,*,#8696,.T.);
#11239=ORIENTED_EDGE('',*,*,#8697,.T.);
#11240=ORIENTED_EDGE('',*,*,#8698,.T.);
#11241=ORIENTED_EDGE('',*,*,#8584,.F.);
#11242=ORIENTED_EDGE('',*,*,#8699,.T.);
#11243=ORIENTED_EDGE('',*,*,#8700,.T.);
#11244=ORIENTED_EDGE('',*,*,#8699,.F.);
#11245=ORIENTED_EDGE('',*,*,#8700,.F.);
#11246=ORIENTED_EDGE('',*,*,#8588,.F.);
#11247=ORIENTED_EDGE('',*,*,#8701,.T.);
#11248=ORIENTED_EDGE('',*,*,#8702,.T.);
#11249=ORIENTED_EDGE('',*,*,#8701,.F.);
#11250=ORIENTED_EDGE('',*,*,#8702,.F.);
#11251=ORIENTED_EDGE('',*,*,#8694,.F.);
#11252=ORIENTED_EDGE('',*,*,#8703,.T.);
#11253=ORIENTED_EDGE('',*,*,#8704,.T.);
#11254=ORIENTED_EDGE('',*,*,#8703,.F.);
#11255=ORIENTED_EDGE('',*,*,#8704,.F.);
#11256=ORIENTED_EDGE('',*,*,#8698,.F.);
#11257=ORIENTED_EDGE('',*,*,#8705,.T.);
#11258=ORIENTED_EDGE('',*,*,#8706,.T.);
#11259=ORIENTED_EDGE('',*,*,#8705,.F.);
#11260=ORIENTED_EDGE('',*,*,#8706,.F.);
#11261=ORIENTED_EDGE('',*,*,#8585,.F.);
#11262=ORIENTED_EDGE('',*,*,#8707,.T.);
#11263=ORIENTED_EDGE('',*,*,#8708,.F.);
#11264=ORIENTED_EDGE('',*,*,#8707,.F.);
#11265=ORIENTED_EDGE('',*,*,#8695,.F.);
#11266=ORIENTED_EDGE('',*,*,#8709,.T.);
#11267=ORIENTED_EDGE('',*,*,#8710,.F.);
#11268=ORIENTED_EDGE('',*,*,#8709,.F.);
#11269=ORIENTED_EDGE('',*,*,#8696,.F.);
#11270=ORIENTED_EDGE('',*,*,#8711,.T.);
#11271=ORIENTED_EDGE('',*,*,#8712,.F.);
#11272=ORIENTED_EDGE('',*,*,#8711,.F.);
#11273=ORIENTED_EDGE('',*,*,#8697,.F.);
#11274=ORIENTED_EDGE('',*,*,#8713,.T.);
#11275=ORIENTED_EDGE('',*,*,#8714,.F.);
#11276=ORIENTED_EDGE('',*,*,#8713,.F.);
#11277=ORIENTED_EDGE('',*,*,#8586,.F.);
#11278=ORIENTED_EDGE('',*,*,#8715,.T.);
#11279=ORIENTED_EDGE('',*,*,#8716,.F.);
#11280=ORIENTED_EDGE('',*,*,#8715,.F.);
#11281=ORIENTED_EDGE('',*,*,#8587,.F.);
#11282=ORIENTED_EDGE('',*,*,#8717,.T.);
#11283=ORIENTED_EDGE('',*,*,#8718,.F.);
#11284=ORIENTED_EDGE('',*,*,#8717,.F.);
#11285=ORIENTED_EDGE('',*,*,#8576,.T.);
#11286=ORIENTED_EDGE('',*,*,#8623,.T.);
#11287=ORIENTED_EDGE('',*,*,#8719,.F.);
#11288=ORIENTED_EDGE('',*,*,#8594,.F.);
#11289=ORIENTED_EDGE('',*,*,#8720,.F.);
#11290=ORIENTED_EDGE('',*,*,#8595,.T.);
#11291=ORIENTED_EDGE('',*,*,#8719,.T.);
#11292=ORIENTED_EDGE('',*,*,#8622,.T.);
#11293=ORIENTED_EDGE('',*,*,#8708,.T.);
#11294=ORIENTED_EDGE('',*,*,#8716,.T.);
#11295=ORIENTED_EDGE('',*,*,#8718,.T.);
#11296=ORIENTED_EDGE('',*,*,#8693,.T.);
#11297=ORIENTED_EDGE('',*,*,#8600,.T.);
#11298=ORIENTED_EDGE('',*,*,#8721,.F.);
#11299=ORIENTED_EDGE('',*,*,#8617,.F.);
#11300=ORIENTED_EDGE('',*,*,#8721,.T.);
#11301=ORIENTED_EDGE('',*,*,#8599,.T.);
#11302=ORIENTED_EDGE('',*,*,#8722,.F.);
#11303=ORIENTED_EDGE('',*,*,#8618,.T.);
#11304=ORIENTED_EDGE('',*,*,#8710,.T.);
#11305=ORIENTED_EDGE('',*,*,#8712,.T.);
#11306=ORIENTED_EDGE('',*,*,#8714,.T.);
#11307=ORIENTED_EDGE('',*,*,#8722,.T.);
#11308=ORIENTED_EDGE('',*,*,#8598,.T.);
#11309=ORIENTED_EDGE('',*,*,#8723,.F.);
#11310=ORIENTED_EDGE('',*,*,#8619,.F.);
#11311=ORIENTED_EDGE('',*,*,#8582,.F.);
#11312=ORIENTED_EDGE('',*,*,#8635,.T.);
#11313=ORIENTED_EDGE('',*,*,#8724,.T.);
#11314=ORIENTED_EDGE('',*,*,#8688,.F.);
#11315=ORIENTED_EDGE('',*,*,#8692,.F.);
#11316=ORIENTED_EDGE('',*,*,#8690,.T.);
#11317=ORIENTED_EDGE('',*,*,#8725,.T.);
#11318=ORIENTED_EDGE('',*,*,#8633,.F.);
#11319=ORIENTED_EDGE('',*,*,#8725,.F.);
#11320=ORIENTED_EDGE('',*,*,#8689,.F.);
#11321=ORIENTED_EDGE('',*,*,#8724,.F.);
#11322=ORIENTED_EDGE('',*,*,#8634,.F.);
#11323=ORIENTED_EDGE('',*,*,#8548,.T.);
#11324=ORIENTED_EDGE('',*,*,#8551,.T.);
#11325=ORIENTED_EDGE('',*,*,#8541,.T.);
#11326=ORIENTED_EDGE('',*,*,#8545,.T.);
#11327=ORIENTED_EDGE('',*,*,#8538,.T.);
#11328=ORIENTED_EDGE('',*,*,#8535,.T.);
#11329=ORIENTED_EDGE('',*,*,#8532,.T.);
#11330=ORIENTED_EDGE('',*,*,#8529,.T.);
#11331=ORIENTED_EDGE('',*,*,#8720,.T.);
#11332=ORIENTED_EDGE('',*,*,#8621,.T.);
#11333=ORIENTED_EDGE('',*,*,#8726,.F.);
#11334=ORIENTED_EDGE('',*,*,#8596,.F.);
#11335=ORIENTED_EDGE('',*,*,#8723,.T.);
#11336=ORIENTED_EDGE('',*,*,#8597,.T.);
#11337=ORIENTED_EDGE('',*,*,#8726,.T.);
#11338=ORIENTED_EDGE('',*,*,#8620,.T.);
#11339=ORIENTED_EDGE('',*,*,#8549,.T.);
#11340=ORIENTED_EDGE('',*,*,#8546,.T.);
#11341=ORIENTED_EDGE('',*,*,#8543,.T.);
#11342=ORIENTED_EDGE('',*,*,#8552,.T.);
#11343=ORIENTED_EDGE('',*,*,#8540,.T.);
#11344=ORIENTED_EDGE('',*,*,#8537,.T.);
#11345=ORIENTED_EDGE('',*,*,#8534,.T.);
#11346=ORIENTED_EDGE('',*,*,#8531,.T.);
#11347=ORIENTED_EDGE('',*,*,#8727,.F.);
#11348=ORIENTED_EDGE('',*,*,#8728,.T.);
#11349=ORIENTED_EDGE('',*,*,#8729,.T.);
#11350=ORIENTED_EDGE('',*,*,#8728,.F.);
#11351=ORIENTED_EDGE('',*,*,#8727,.T.);
#11352=ORIENTED_EDGE('',*,*,#8729,.F.);
#11353=ORIENTED_EDGE('',*,*,#8730,.F.);
#11354=ORIENTED_EDGE('',*,*,#8731,.T.);
#11355=ORIENTED_EDGE('',*,*,#8732,.T.);
#11356=ORIENTED_EDGE('',*,*,#8731,.F.);
#11357=ORIENTED_EDGE('',*,*,#8730,.T.);
#11358=ORIENTED_EDGE('',*,*,#8732,.F.);
#11359=ORIENTED_EDGE('',*,*,#8733,.F.);
#11360=ORIENTED_EDGE('',*,*,#8734,.T.);
#11361=ORIENTED_EDGE('',*,*,#8735,.T.);
#11362=ORIENTED_EDGE('',*,*,#8734,.F.);
#11363=ORIENTED_EDGE('',*,*,#8733,.T.);
#11364=ORIENTED_EDGE('',*,*,#8735,.F.);
#11365=ORIENTED_EDGE('',*,*,#8736,.F.);
#11366=ORIENTED_EDGE('',*,*,#8737,.T.);
#11367=ORIENTED_EDGE('',*,*,#8738,.T.);
#11368=ORIENTED_EDGE('',*,*,#8737,.F.);
#11369=ORIENTED_EDGE('',*,*,#8736,.T.);
#11370=ORIENTED_EDGE('',*,*,#8738,.F.);
#11371=ORIENTED_EDGE('',*,*,#8739,.F.);
#11372=ORIENTED_EDGE('',*,*,#8740,.F.);
#11373=ORIENTED_EDGE('',*,*,#8741,.F.);
#11374=ORIENTED_EDGE('',*,*,#8742,.F.);
#11375=ORIENTED_EDGE('',*,*,#8743,.F.);
#11376=ORIENTED_EDGE('',*,*,#8744,.F.);
#11377=ORIENTED_EDGE('',*,*,#8745,.F.);
#11378=ORIENTED_EDGE('',*,*,#8746,.F.);
#11379=ORIENTED_EDGE('',*,*,#8747,.F.);
#11380=ORIENTED_EDGE('',*,*,#8748,.F.);
#11381=ORIENTED_EDGE('',*,*,#8749,.F.);
#11382=ORIENTED_EDGE('',*,*,#8750,.F.);
#11383=ORIENTED_EDGE('',*,*,#8751,.F.);
#11384=ORIENTED_EDGE('',*,*,#8752,.F.);
#11385=ORIENTED_EDGE('',*,*,#8753,.F.);
#11386=ORIENTED_EDGE('',*,*,#8754,.F.);
#11387=ORIENTED_EDGE('',*,*,#8740,.T.);
#11388=ORIENTED_EDGE('',*,*,#8755,.F.);
#11389=ORIENTED_EDGE('',*,*,#8752,.T.);
#11390=ORIENTED_EDGE('',*,*,#8756,.F.);
#11391=ORIENTED_EDGE('',*,*,#8748,.T.);
#11392=ORIENTED_EDGE('',*,*,#8757,.F.);
#11393=ORIENTED_EDGE('',*,*,#8744,.T.);
#11394=ORIENTED_EDGE('',*,*,#8758,.F.);
#11395=ORIENTED_EDGE('',*,*,#8759,.F.);
#11396=ORIENTED_EDGE('',*,*,#8749,.T.);
#11397=ORIENTED_EDGE('',*,*,#8756,.T.);
#11398=ORIENTED_EDGE('',*,*,#8751,.T.);
#11399=ORIENTED_EDGE('',*,*,#8760,.F.);
#11400=ORIENTED_EDGE('',*,*,#8745,.T.);
#11401=ORIENTED_EDGE('',*,*,#8757,.T.);
#11402=ORIENTED_EDGE('',*,*,#8747,.T.);
#11403=ORIENTED_EDGE('',*,*,#8761,.F.);
#11404=ORIENTED_EDGE('',*,*,#8739,.T.);
#11405=ORIENTED_EDGE('',*,*,#8762,.F.);
#11406=ORIENTED_EDGE('',*,*,#8753,.T.);
#11407=ORIENTED_EDGE('',*,*,#8755,.T.);
#11408=ORIENTED_EDGE('',*,*,#8741,.T.);
#11409=ORIENTED_EDGE('',*,*,#8758,.T.);
#11410=ORIENTED_EDGE('',*,*,#8743,.T.);
#11411=ORIENTED_EDGE('',*,*,#8763,.F.);
#11412=ORIENTED_EDGE('',*,*,#8764,.F.);
#11413=ORIENTED_EDGE('',*,*,#8765,.T.);
#11414=ORIENTED_EDGE('',*,*,#8766,.F.);
#11415=ORIENTED_EDGE('',*,*,#8765,.F.);
#11416=ORIENTED_EDGE('',*,*,#8764,.T.);
#11417=ORIENTED_EDGE('',*,*,#8767,.T.);
#11418=ORIENTED_EDGE('',*,*,#8767,.F.);
#11419=ORIENTED_EDGE('',*,*,#8768,.T.);
#11420=ORIENTED_EDGE('',*,*,#8759,.T.);
#11421=ORIENTED_EDGE('',*,*,#8768,.F.);
#11422=ORIENTED_EDGE('',*,*,#8742,.T.);
#11423=ORIENTED_EDGE('',*,*,#8763,.T.);
#11424=ORIENTED_EDGE('',*,*,#8746,.T.);
#11425=ORIENTED_EDGE('',*,*,#8761,.T.);
#11426=ORIENTED_EDGE('',*,*,#8750,.T.);
#11427=ORIENTED_EDGE('',*,*,#8760,.T.);
#11428=ORIENTED_EDGE('',*,*,#8754,.T.);
#11429=ORIENTED_EDGE('',*,*,#8762,.T.);
#11430=ORIENTED_EDGE('',*,*,#8766,.T.);
#11431=ORIENTED_EDGE('',*,*,#8769,.F.);
#11432=ORIENTED_EDGE('',*,*,#8770,.F.);
#11433=ORIENTED_EDGE('',*,*,#8771,.F.);
#11434=ORIENTED_EDGE('',*,*,#8772,.F.);
#11435=ORIENTED_EDGE('',*,*,#8773,.F.);
#11436=ORIENTED_EDGE('',*,*,#8774,.F.);
#11437=ORIENTED_EDGE('',*,*,#8775,.F.);
#11438=ORIENTED_EDGE('',*,*,#8776,.F.);
#11439=ORIENTED_EDGE('',*,*,#8777,.F.);
#11440=ORIENTED_EDGE('',*,*,#8778,.F.);
#11441=ORIENTED_EDGE('',*,*,#8779,.F.);
#11442=ORIENTED_EDGE('',*,*,#8780,.F.);
#11443=ORIENTED_EDGE('',*,*,#8781,.F.);
#11444=ORIENTED_EDGE('',*,*,#8782,.F.);
#11445=ORIENTED_EDGE('',*,*,#8783,.F.);
#11446=ORIENTED_EDGE('',*,*,#8784,.F.);
#11447=ORIENTED_EDGE('',*,*,#8770,.T.);
#11448=ORIENTED_EDGE('',*,*,#8785,.F.);
#11449=ORIENTED_EDGE('',*,*,#8782,.T.);
#11450=ORIENTED_EDGE('',*,*,#8786,.F.);
#11451=ORIENTED_EDGE('',*,*,#8778,.T.);
#11452=ORIENTED_EDGE('',*,*,#8787,.F.);
#11453=ORIENTED_EDGE('',*,*,#8774,.T.);
#11454=ORIENTED_EDGE('',*,*,#8788,.F.);
#11455=ORIENTED_EDGE('',*,*,#8789,.T.);
#11456=ORIENTED_EDGE('',*,*,#8779,.T.);
#11457=ORIENTED_EDGE('',*,*,#8786,.T.);
#11458=ORIENTED_EDGE('',*,*,#8781,.T.);
#11459=ORIENTED_EDGE('',*,*,#8790,.F.);
#11460=ORIENTED_EDGE('',*,*,#8775,.T.);
#11461=ORIENTED_EDGE('',*,*,#8787,.T.);
#11462=ORIENTED_EDGE('',*,*,#8777,.T.);
#11463=ORIENTED_EDGE('',*,*,#8791,.F.);
#11464=ORIENTED_EDGE('',*,*,#8769,.T.);
#11465=ORIENTED_EDGE('',*,*,#8792,.F.);
#11466=ORIENTED_EDGE('',*,*,#8783,.T.);
#11467=ORIENTED_EDGE('',*,*,#8785,.T.);
#11468=ORIENTED_EDGE('',*,*,#8771,.T.);
#11469=ORIENTED_EDGE('',*,*,#8788,.T.);
#11470=ORIENTED_EDGE('',*,*,#8773,.T.);
#11471=ORIENTED_EDGE('',*,*,#8793,.F.);
#11472=ORIENTED_EDGE('',*,*,#8789,.F.);
#11473=ORIENTED_EDGE('',*,*,#8794,.T.);
#11474=ORIENTED_EDGE('',*,*,#8795,.T.);
#11475=ORIENTED_EDGE('',*,*,#8794,.F.);
#11476=ORIENTED_EDGE('',*,*,#8795,.F.);
#11477=ORIENTED_EDGE('',*,*,#8796,.F.);
#11478=ORIENTED_EDGE('',*,*,#8797,.F.);
#11479=ORIENTED_EDGE('',*,*,#8798,.T.);
#11480=ORIENTED_EDGE('',*,*,#8796,.T.);
#11481=ORIENTED_EDGE('',*,*,#8798,.F.);
#11482=ORIENTED_EDGE('',*,*,#8772,.T.);
#11483=ORIENTED_EDGE('',*,*,#8793,.T.);
#11484=ORIENTED_EDGE('',*,*,#8776,.T.);
#11485=ORIENTED_EDGE('',*,*,#8791,.T.);
#11486=ORIENTED_EDGE('',*,*,#8780,.T.);
#11487=ORIENTED_EDGE('',*,*,#8790,.T.);
#11488=ORIENTED_EDGE('',*,*,#8784,.T.);
#11489=ORIENTED_EDGE('',*,*,#8792,.T.);
#11490=ORIENTED_EDGE('',*,*,#8797,.T.);
#11491=ORIENTED_EDGE('',*,*,#8799,.F.);
#11492=ORIENTED_EDGE('',*,*,#8800,.T.);
#11493=ORIENTED_EDGE('',*,*,#8801,.F.);
#11494=ORIENTED_EDGE('',*,*,#8800,.F.);
#11495=ORIENTED_EDGE('',*,*,#8802,.F.);
#11496=ORIENTED_EDGE('',*,*,#8803,.T.);
#11497=ORIENTED_EDGE('',*,*,#8804,.F.);
#11498=ORIENTED_EDGE('',*,*,#8803,.F.);
#11499=ORIENTED_EDGE('',*,*,#8805,.F.);
#11500=ORIENTED_EDGE('',*,*,#8806,.T.);
#11501=ORIENTED_EDGE('',*,*,#8807,.F.);
#11502=ORIENTED_EDGE('',*,*,#8806,.F.);
#11503=ORIENTED_EDGE('',*,*,#8808,.F.);
#11504=ORIENTED_EDGE('',*,*,#8809,.T.);
#11505=ORIENTED_EDGE('',*,*,#8810,.F.);
#11506=ORIENTED_EDGE('',*,*,#8809,.F.);
#11507=ORIENTED_EDGE('',*,*,#8811,.F.);
#11508=ORIENTED_EDGE('',*,*,#8812,.T.);
#11509=ORIENTED_EDGE('',*,*,#8813,.F.);
#11510=ORIENTED_EDGE('',*,*,#8812,.F.);
#11511=ORIENTED_EDGE('',*,*,#8811,.T.);
#11512=ORIENTED_EDGE('',*,*,#8814,.T.);
#11513=ORIENTED_EDGE('',*,*,#8814,.F.);
#11514=ORIENTED_EDGE('',*,*,#8815,.T.);
#11515=ORIENTED_EDGE('',*,*,#8816,.T.);
#11516=ORIENTED_EDGE('',*,*,#8815,.F.);
#11517=ORIENTED_EDGE('',*,*,#8817,.F.);
#11518=ORIENTED_EDGE('',*,*,#8818,.T.);
#11519=ORIENTED_EDGE('',*,*,#8819,.T.);
#11520=ORIENTED_EDGE('',*,*,#8818,.F.);
#11521=ORIENTED_EDGE('',*,*,#8817,.T.);
#11522=ORIENTED_EDGE('',*,*,#8813,.T.);
#11523=ORIENTED_EDGE('',*,*,#8810,.T.);
#11524=ORIENTED_EDGE('',*,*,#8807,.T.);
#11525=ORIENTED_EDGE('',*,*,#8804,.T.);
#11526=ORIENTED_EDGE('',*,*,#8801,.T.);
#11527=ORIENTED_EDGE('',*,*,#8819,.F.);
#11528=ORIENTED_EDGE('',*,*,#8816,.F.);
#11529=ORIENTED_EDGE('',*,*,#8808,.T.);
#11530=ORIENTED_EDGE('',*,*,#8805,.T.);
#11531=ORIENTED_EDGE('',*,*,#8802,.T.);
#11532=ORIENTED_EDGE('',*,*,#8799,.T.);
#11533=ORIENTED_EDGE('',*,*,#8820,.F.);
#11534=ORIENTED_EDGE('',*,*,#8821,.T.);
#11535=ORIENTED_EDGE('',*,*,#8822,.F.);
#11536=ORIENTED_EDGE('',*,*,#8821,.F.);
#11537=ORIENTED_EDGE('',*,*,#8823,.F.);
#11538=ORIENTED_EDGE('',*,*,#8824,.T.);
#11539=ORIENTED_EDGE('',*,*,#8825,.F.);
#11540=ORIENTED_EDGE('',*,*,#8824,.F.);
#11541=ORIENTED_EDGE('',*,*,#8826,.F.);
#11542=ORIENTED_EDGE('',*,*,#8827,.T.);
#11543=ORIENTED_EDGE('',*,*,#8828,.F.);
#11544=ORIENTED_EDGE('',*,*,#8827,.F.);
#11545=ORIENTED_EDGE('',*,*,#8829,.F.);
#11546=ORIENTED_EDGE('',*,*,#8830,.T.);
#11547=ORIENTED_EDGE('',*,*,#8831,.F.);
#11548=ORIENTED_EDGE('',*,*,#8830,.F.);
#11549=ORIENTED_EDGE('',*,*,#8832,.F.);
#11550=ORIENTED_EDGE('',*,*,#8833,.T.);
#11551=ORIENTED_EDGE('',*,*,#8834,.T.);
#11552=ORIENTED_EDGE('',*,*,#8833,.F.);
#11553=ORIENTED_EDGE('',*,*,#8834,.F.);
#11554=ORIENTED_EDGE('',*,*,#8835,.F.);
#11555=ORIENTED_EDGE('',*,*,#8836,.F.);
#11556=ORIENTED_EDGE('',*,*,#8837,.T.);
#11557=ORIENTED_EDGE('',*,*,#8835,.T.);
#11558=ORIENTED_EDGE('',*,*,#8837,.F.);
#11559=ORIENTED_EDGE('',*,*,#8838,.F.);
#11560=ORIENTED_EDGE('',*,*,#8839,.T.);
#11561=ORIENTED_EDGE('',*,*,#8840,.T.);
#11562=ORIENTED_EDGE('',*,*,#8839,.F.);
#11563=ORIENTED_EDGE('',*,*,#8838,.T.);
#11564=ORIENTED_EDGE('',*,*,#8836,.T.);
#11565=ORIENTED_EDGE('',*,*,#8831,.T.);
#11566=ORIENTED_EDGE('',*,*,#8828,.T.);
#11567=ORIENTED_EDGE('',*,*,#8825,.T.);
#11568=ORIENTED_EDGE('',*,*,#8822,.T.);
#11569=ORIENTED_EDGE('',*,*,#8840,.F.);
#11570=ORIENTED_EDGE('',*,*,#8832,.T.);
#11571=ORIENTED_EDGE('',*,*,#8829,.T.);
#11572=ORIENTED_EDGE('',*,*,#8826,.T.);
#11573=ORIENTED_EDGE('',*,*,#8823,.T.);
#11574=ORIENTED_EDGE('',*,*,#8820,.T.);
#11575=ORIENTED_EDGE('',*,*,#8841,.F.);
#11576=ORIENTED_EDGE('',*,*,#8842,.T.);
#11577=ORIENTED_EDGE('',*,*,#8843,.F.);
#11578=ORIENTED_EDGE('',*,*,#8842,.F.);
#11579=ORIENTED_EDGE('',*,*,#8844,.F.);
#11580=ORIENTED_EDGE('',*,*,#8845,.T.);
#11581=ORIENTED_EDGE('',*,*,#8846,.F.);
#11582=ORIENTED_EDGE('',*,*,#8845,.F.);
#11583=ORIENTED_EDGE('',*,*,#8847,.F.);
#11584=ORIENTED_EDGE('',*,*,#8848,.T.);
#11585=ORIENTED_EDGE('',*,*,#8849,.F.);
#11586=ORIENTED_EDGE('',*,*,#8848,.F.);
#11587=ORIENTED_EDGE('',*,*,#8850,.F.);
#11588=ORIENTED_EDGE('',*,*,#8851,.T.);
#11589=ORIENTED_EDGE('',*,*,#8852,.F.);
#11590=ORIENTED_EDGE('',*,*,#8851,.F.);
#11591=ORIENTED_EDGE('',*,*,#8853,.F.);
#11592=ORIENTED_EDGE('',*,*,#8854,.T.);
#11593=ORIENTED_EDGE('',*,*,#8855,.F.);
#11594=ORIENTED_EDGE('',*,*,#8854,.F.);
#11595=ORIENTED_EDGE('',*,*,#8853,.T.);
#11596=ORIENTED_EDGE('',*,*,#8856,.T.);
#11597=ORIENTED_EDGE('',*,*,#8856,.F.);
#11598=ORIENTED_EDGE('',*,*,#8857,.T.);
#11599=ORIENTED_EDGE('',*,*,#8858,.T.);
#11600=ORIENTED_EDGE('',*,*,#8857,.F.);
#11601=ORIENTED_EDGE('',*,*,#8859,.F.);
#11602=ORIENTED_EDGE('',*,*,#8860,.T.);
#11603=ORIENTED_EDGE('',*,*,#8861,.T.);
#11604=ORIENTED_EDGE('',*,*,#8860,.F.);
#11605=ORIENTED_EDGE('',*,*,#8859,.T.);
#11606=ORIENTED_EDGE('',*,*,#8855,.T.);
#11607=ORIENTED_EDGE('',*,*,#8852,.T.);
#11608=ORIENTED_EDGE('',*,*,#8849,.T.);
#11609=ORIENTED_EDGE('',*,*,#8846,.T.);
#11610=ORIENTED_EDGE('',*,*,#8843,.T.);
#11611=ORIENTED_EDGE('',*,*,#8861,.F.);
#11612=ORIENTED_EDGE('',*,*,#8858,.F.);
#11613=ORIENTED_EDGE('',*,*,#8850,.T.);
#11614=ORIENTED_EDGE('',*,*,#8847,.T.);
#11615=ORIENTED_EDGE('',*,*,#8844,.T.);
#11616=ORIENTED_EDGE('',*,*,#8841,.T.);
#11617=ORIENTED_EDGE('',*,*,#8862,.F.);
#11618=ORIENTED_EDGE('',*,*,#8863,.T.);
#11619=ORIENTED_EDGE('',*,*,#8864,.F.);
#11620=ORIENTED_EDGE('',*,*,#8863,.F.);
#11621=ORIENTED_EDGE('',*,*,#8865,.F.);
#11622=ORIENTED_EDGE('',*,*,#8866,.T.);
#11623=ORIENTED_EDGE('',*,*,#8867,.F.);
#11624=ORIENTED_EDGE('',*,*,#8866,.F.);
#11625=ORIENTED_EDGE('',*,*,#8868,.F.);
#11626=ORIENTED_EDGE('',*,*,#8869,.T.);
#11627=ORIENTED_EDGE('',*,*,#8870,.F.);
#11628=ORIENTED_EDGE('',*,*,#8869,.F.);
#11629=ORIENTED_EDGE('',*,*,#8871,.F.);
#11630=ORIENTED_EDGE('',*,*,#8872,.T.);
#11631=ORIENTED_EDGE('',*,*,#8873,.F.);
#11632=ORIENTED_EDGE('',*,*,#8872,.F.);
#11633=ORIENTED_EDGE('',*,*,#8874,.F.);
#11634=ORIENTED_EDGE('',*,*,#8875,.T.);
#11635=ORIENTED_EDGE('',*,*,#8876,.T.);
#11636=ORIENTED_EDGE('',*,*,#8875,.F.);
#11637=ORIENTED_EDGE('',*,*,#8876,.F.);
#11638=ORIENTED_EDGE('',*,*,#8877,.F.);
#11639=ORIENTED_EDGE('',*,*,#8878,.F.);
#11640=ORIENTED_EDGE('',*,*,#8879,.T.);
#11641=ORIENTED_EDGE('',*,*,#8877,.T.);
#11642=ORIENTED_EDGE('',*,*,#8879,.F.);
#11643=ORIENTED_EDGE('',*,*,#8880,.F.);
#11644=ORIENTED_EDGE('',*,*,#8881,.T.);
#11645=ORIENTED_EDGE('',*,*,#8882,.T.);
#11646=ORIENTED_EDGE('',*,*,#8881,.F.);
#11647=ORIENTED_EDGE('',*,*,#8880,.T.);
#11648=ORIENTED_EDGE('',*,*,#8878,.T.);
#11649=ORIENTED_EDGE('',*,*,#8873,.T.);
#11650=ORIENTED_EDGE('',*,*,#8870,.T.);
#11651=ORIENTED_EDGE('',*,*,#8867,.T.);
#11652=ORIENTED_EDGE('',*,*,#8864,.T.);
#11653=ORIENTED_EDGE('',*,*,#8882,.F.);
#11654=ORIENTED_EDGE('',*,*,#8874,.T.);
#11655=ORIENTED_EDGE('',*,*,#8871,.T.);
#11656=ORIENTED_EDGE('',*,*,#8868,.T.);
#11657=ORIENTED_EDGE('',*,*,#8865,.T.);
#11658=ORIENTED_EDGE('',*,*,#8862,.T.);
#11659=ORIENTED_EDGE('',*,*,#8883,.F.);
#11660=ORIENTED_EDGE('',*,*,#8884,.T.);
#11661=ORIENTED_EDGE('',*,*,#8885,.F.);
#11662=ORIENTED_EDGE('',*,*,#8884,.F.);
#11663=ORIENTED_EDGE('',*,*,#8886,.F.);
#11664=ORIENTED_EDGE('',*,*,#8887,.T.);
#11665=ORIENTED_EDGE('',*,*,#8888,.F.);
#11666=ORIENTED_EDGE('',*,*,#8887,.F.);
#11667=ORIENTED_EDGE('',*,*,#8889,.F.);
#11668=ORIENTED_EDGE('',*,*,#8890,.T.);
#11669=ORIENTED_EDGE('',*,*,#8891,.F.);
#11670=ORIENTED_EDGE('',*,*,#8890,.F.);
#11671=ORIENTED_EDGE('',*,*,#8892,.F.);
#11672=ORIENTED_EDGE('',*,*,#8893,.T.);
#11673=ORIENTED_EDGE('',*,*,#8894,.F.);
#11674=ORIENTED_EDGE('',*,*,#8893,.F.);
#11675=ORIENTED_EDGE('',*,*,#8895,.T.);
#11676=ORIENTED_EDGE('',*,*,#8896,.T.);
#11677=ORIENTED_EDGE('',*,*,#8897,.F.);
#11678=ORIENTED_EDGE('',*,*,#8898,.F.);
#11679=ORIENTED_EDGE('',*,*,#8899,.T.);
#11680=ORIENTED_EDGE('',*,*,#8898,.T.);
#11681=ORIENTED_EDGE('',*,*,#8900,.F.);
#11682=ORIENTED_EDGE('',*,*,#8901,.F.);
#11683=ORIENTED_EDGE('',*,*,#8902,.T.);
#11684=ORIENTED_EDGE('',*,*,#8901,.T.);
#11685=ORIENTED_EDGE('',*,*,#8903,.F.);
#11686=ORIENTED_EDGE('',*,*,#8904,.F.);
#11687=ORIENTED_EDGE('',*,*,#8905,.T.);
#11688=ORIENTED_EDGE('',*,*,#8904,.T.);
#11689=ORIENTED_EDGE('',*,*,#8906,.F.);
#11690=ORIENTED_EDGE('',*,*,#8896,.F.);
#11691=ORIENTED_EDGE('',*,*,#8906,.T.);
#11692=ORIENTED_EDGE('',*,*,#8903,.T.);
#11693=ORIENTED_EDGE('',*,*,#8900,.T.);
#11694=ORIENTED_EDGE('',*,*,#8897,.T.);
#11695=ORIENTED_EDGE('',*,*,#8885,.T.);
#11696=ORIENTED_EDGE('',*,*,#8888,.T.);
#11697=ORIENTED_EDGE('',*,*,#8891,.T.);
#11698=ORIENTED_EDGE('',*,*,#8894,.T.);
#11699=ORIENTED_EDGE('',*,*,#8905,.F.);
#11700=ORIENTED_EDGE('',*,*,#8895,.F.);
#11701=ORIENTED_EDGE('',*,*,#8899,.F.);
#11702=ORIENTED_EDGE('',*,*,#8902,.F.);
#11703=ORIENTED_EDGE('',*,*,#8883,.T.);
#11704=ORIENTED_EDGE('',*,*,#8886,.T.);
#11705=ORIENTED_EDGE('',*,*,#8889,.T.);
#11706=ORIENTED_EDGE('',*,*,#8892,.T.);
#11707=ORIENTED_EDGE('',*,*,#8907,.T.);
#11708=ORIENTED_EDGE('',*,*,#8908,.T.);
#11709=ORIENTED_EDGE('',*,*,#8909,.F.);
#11710=ORIENTED_EDGE('',*,*,#8910,.F.);
#11711=ORIENTED_EDGE('',*,*,#8911,.T.);
#11712=ORIENTED_EDGE('',*,*,#8910,.T.);
#11713=ORIENTED_EDGE('',*,*,#8912,.F.);
#11714=ORIENTED_EDGE('',*,*,#8913,.F.);
#11715=ORIENTED_EDGE('',*,*,#8914,.T.);
#11716=ORIENTED_EDGE('',*,*,#8913,.T.);
#11717=ORIENTED_EDGE('',*,*,#8915,.F.);
#11718=ORIENTED_EDGE('',*,*,#8916,.F.);
#11719=ORIENTED_EDGE('',*,*,#8917,.T.);
#11720=ORIENTED_EDGE('',*,*,#8916,.T.);
#11721=ORIENTED_EDGE('',*,*,#8918,.F.);
#11722=ORIENTED_EDGE('',*,*,#8908,.F.);
#11723=ORIENTED_EDGE('',*,*,#8918,.T.);
#11724=ORIENTED_EDGE('',*,*,#8915,.T.);
#11725=ORIENTED_EDGE('',*,*,#8912,.T.);
#11726=ORIENTED_EDGE('',*,*,#8909,.T.);
#11727=ORIENTED_EDGE('',*,*,#8917,.F.);
#11728=ORIENTED_EDGE('',*,*,#8907,.F.);
#11729=ORIENTED_EDGE('',*,*,#8911,.F.);
#11730=ORIENTED_EDGE('',*,*,#8914,.F.);
#11731=ORIENTED_EDGE('',*,*,#8919,.T.);
#11732=ORIENTED_EDGE('',*,*,#8920,.T.);
#11733=ORIENTED_EDGE('',*,*,#8921,.F.);
#11734=ORIENTED_EDGE('',*,*,#8922,.F.);
#11735=ORIENTED_EDGE('',*,*,#8923,.T.);
#11736=ORIENTED_EDGE('',*,*,#8922,.T.);
#11737=ORIENTED_EDGE('',*,*,#8924,.F.);
#11738=ORIENTED_EDGE('',*,*,#8925,.F.);
#11739=ORIENTED_EDGE('',*,*,#8926,.T.);
#11740=ORIENTED_EDGE('',*,*,#8925,.T.);
#11741=ORIENTED_EDGE('',*,*,#8927,.F.);
#11742=ORIENTED_EDGE('',*,*,#8928,.F.);
#11743=ORIENTED_EDGE('',*,*,#8929,.T.);
#11744=ORIENTED_EDGE('',*,*,#8928,.T.);
#11745=ORIENTED_EDGE('',*,*,#8930,.F.);
#11746=ORIENTED_EDGE('',*,*,#8920,.F.);
#11747=ORIENTED_EDGE('',*,*,#8930,.T.);
#11748=ORIENTED_EDGE('',*,*,#8927,.T.);
#11749=ORIENTED_EDGE('',*,*,#8924,.T.);
#11750=ORIENTED_EDGE('',*,*,#8921,.T.);
#11751=ORIENTED_EDGE('',*,*,#8929,.F.);
#11752=ORIENTED_EDGE('',*,*,#8919,.F.);
#11753=ORIENTED_EDGE('',*,*,#8923,.F.);
#11754=ORIENTED_EDGE('',*,*,#8926,.F.);
#11755=ORIENTED_EDGE('',*,*,#8931,.T.);
#11756=ORIENTED_EDGE('',*,*,#8932,.T.);
#11757=ORIENTED_EDGE('',*,*,#8933,.T.);
#11758=ORIENTED_EDGE('',*,*,#8934,.F.);
#11759=ORIENTED_EDGE('',*,*,#8935,.T.);
#11760=ORIENTED_EDGE('',*,*,#8936,.T.);
#11761=ORIENTED_EDGE('',*,*,#8937,.T.);
#11762=ORIENTED_EDGE('',*,*,#8932,.F.);
#11763=ORIENTED_EDGE('',*,*,#8938,.T.);
#11764=ORIENTED_EDGE('',*,*,#8939,.T.);
#11765=ORIENTED_EDGE('',*,*,#8940,.T.);
#11766=ORIENTED_EDGE('',*,*,#8936,.F.);
#11767=ORIENTED_EDGE('',*,*,#8941,.T.);
#11768=ORIENTED_EDGE('',*,*,#8942,.T.);
#11769=ORIENTED_EDGE('',*,*,#8943,.T.);
#11770=ORIENTED_EDGE('',*,*,#8939,.F.);
#11771=ORIENTED_EDGE('',*,*,#8944,.T.);
#11772=ORIENTED_EDGE('',*,*,#8945,.T.);
#11773=ORIENTED_EDGE('',*,*,#8946,.T.);
#11774=ORIENTED_EDGE('',*,*,#8942,.F.);
#11775=ORIENTED_EDGE('',*,*,#8947,.T.);
#11776=ORIENTED_EDGE('',*,*,#8934,.T.);
#11777=ORIENTED_EDGE('',*,*,#8948,.T.);
#11778=ORIENTED_EDGE('',*,*,#8945,.F.);
#11779=ORIENTED_EDGE('',*,*,#8947,.F.);
#11780=ORIENTED_EDGE('',*,*,#8944,.F.);
#11781=ORIENTED_EDGE('',*,*,#8941,.F.);
#11782=ORIENTED_EDGE('',*,*,#8938,.F.);
#11783=ORIENTED_EDGE('',*,*,#8935,.F.);
#11784=ORIENTED_EDGE('',*,*,#8931,.F.);
#11785=ORIENTED_EDGE('',*,*,#8948,.F.);
#11786=ORIENTED_EDGE('',*,*,#8933,.F.);
#11787=ORIENTED_EDGE('',*,*,#8937,.F.);
#11788=ORIENTED_EDGE('',*,*,#8940,.F.);
#11789=ORIENTED_EDGE('',*,*,#8943,.F.);
#11790=ORIENTED_EDGE('',*,*,#8946,.F.);
#11791=ORIENTED_EDGE('',*,*,#8949,.F.);
#11792=ORIENTED_EDGE('',*,*,#8950,.F.);
#11793=ORIENTED_EDGE('',*,*,#8951,.F.);
#11794=ORIENTED_EDGE('',*,*,#8952,.T.);
#11795=ORIENTED_EDGE('',*,*,#8950,.T.);
#11796=ORIENTED_EDGE('',*,*,#8952,.F.);
#11797=ORIENTED_EDGE('',*,*,#8953,.F.);
#11798=ORIENTED_EDGE('',*,*,#8954,.T.);
#11799=ORIENTED_EDGE('',*,*,#8951,.T.);
#11800=ORIENTED_EDGE('',*,*,#8954,.F.);
#11801=ORIENTED_EDGE('',*,*,#8955,.F.);
#11802=ORIENTED_EDGE('',*,*,#8956,.T.);
#11803=ORIENTED_EDGE('',*,*,#8953,.T.);
#11804=ORIENTED_EDGE('',*,*,#8956,.F.);
#11805=ORIENTED_EDGE('',*,*,#8955,.T.);
#11806=ORIENTED_EDGE('',*,*,#8957,.F.);
#11807=ORIENTED_EDGE('',*,*,#8958,.F.);
#11808=ORIENTED_EDGE('',*,*,#8959,.T.);
#11809=ORIENTED_EDGE('',*,*,#8957,.T.);
#11810=ORIENTED_EDGE('',*,*,#8959,.F.);
#11811=ORIENTED_EDGE('',*,*,#8949,.T.);
#11812=ORIENTED_EDGE('',*,*,#8960,.T.);
#11813=ORIENTED_EDGE('',*,*,#8958,.T.);
#11814=ORIENTED_EDGE('',*,*,#8960,.F.);
#11815=ORIENTED_EDGE('',*,*,#8961,.F.);
#11816=ORIENTED_EDGE('',*,*,#8962,.F.);
#11817=ORIENTED_EDGE('',*,*,#8963,.T.);
#11818=ORIENTED_EDGE('',*,*,#8964,.F.);
#11819=ORIENTED_EDGE('',*,*,#8965,.F.);
#11820=ORIENTED_EDGE('',*,*,#8963,.F.);
#11821=ORIENTED_EDGE('',*,*,#8964,.T.);
#11822=ORIENTED_EDGE('',*,*,#8965,.T.);
#11823=ORIENTED_EDGE('',*,*,#8966,.T.);
#11824=ORIENTED_EDGE('',*,*,#8967,.T.);
#11825=ORIENTED_EDGE('',*,*,#8966,.F.);
#11826=ORIENTED_EDGE('',*,*,#8968,.T.);
#11827=ORIENTED_EDGE('',*,*,#8969,.T.);
#11828=ORIENTED_EDGE('',*,*,#8970,.F.);
#11829=ORIENTED_EDGE('',*,*,#8969,.F.);
#11830=ORIENTED_EDGE('',*,*,#8970,.T.);
#11831=ORIENTED_EDGE('',*,*,#8971,.T.);
#11832=ORIENTED_EDGE('',*,*,#8972,.F.);
#11833=ORIENTED_EDGE('',*,*,#8971,.F.);
#11834=ORIENTED_EDGE('',*,*,#8967,.F.);
#11835=ORIENTED_EDGE('',*,*,#8972,.T.);
#11836=ORIENTED_EDGE('',*,*,#8973,.F.);
#11837=ORIENTED_EDGE('',*,*,#8974,.T.);
#11838=ORIENTED_EDGE('',*,*,#8961,.T.);
#11839=ORIENTED_EDGE('',*,*,#8962,.T.);
#11840=ORIENTED_EDGE('',*,*,#8974,.F.);
#11841=ORIENTED_EDGE('',*,*,#8973,.T.);
#11842=ORIENTED_EDGE('',*,*,#8975,.F.);
#11843=ORIENTED_EDGE('',*,*,#8975,.T.);
#11844=ORIENTED_EDGE('',*,*,#8976,.T.);
#11845=ORIENTED_EDGE('',*,*,#8968,.F.);
#11846=ORIENTED_EDGE('',*,*,#8976,.F.);
#11847=ORIENTED_EDGE('',*,*,#8977,.F.);
#11848=ORIENTED_EDGE('',*,*,#8978,.F.);
#11849=ORIENTED_EDGE('',*,*,#8979,.T.);
#11850=ORIENTED_EDGE('',*,*,#8980,.F.);
#11851=ORIENTED_EDGE('',*,*,#8981,.F.);
#11852=ORIENTED_EDGE('',*,*,#8979,.F.);
#11853=ORIENTED_EDGE('',*,*,#8982,.T.);
#11854=ORIENTED_EDGE('',*,*,#8983,.T.);
#11855=ORIENTED_EDGE('',*,*,#8980,.T.);
#11856=ORIENTED_EDGE('',*,*,#8981,.T.);
#11857=ORIENTED_EDGE('',*,*,#8983,.F.);
#11858=ORIENTED_EDGE('',*,*,#8984,.F.);
#11859=ORIENTED_EDGE('',*,*,#8985,.T.);
#11860=ORIENTED_EDGE('',*,*,#8986,.F.);
#11861=ORIENTED_EDGE('',*,*,#8987,.T.);
#11862=ORIENTED_EDGE('',*,*,#8984,.T.);
#11863=ORIENTED_EDGE('',*,*,#8987,.F.);
#11864=ORIENTED_EDGE('',*,*,#8988,.F.);
#11865=ORIENTED_EDGE('',*,*,#8989,.T.);
#11866=ORIENTED_EDGE('',*,*,#8986,.T.);
#11867=ORIENTED_EDGE('',*,*,#8989,.F.);
#11868=ORIENTED_EDGE('',*,*,#8990,.F.);
#11869=ORIENTED_EDGE('',*,*,#8991,.T.);
#11870=ORIENTED_EDGE('',*,*,#8988,.T.);
#11871=ORIENTED_EDGE('',*,*,#8991,.F.);
#11872=ORIENTED_EDGE('',*,*,#8990,.T.);
#11873=ORIENTED_EDGE('',*,*,#8982,.F.);
#11874=ORIENTED_EDGE('',*,*,#8977,.T.);
#11875=ORIENTED_EDGE('',*,*,#8978,.T.);
#11876=ORIENTED_EDGE('',*,*,#8992,.T.);
#11877=ORIENTED_EDGE('',*,*,#8985,.F.);
#11878=ORIENTED_EDGE('',*,*,#8992,.F.);
#11879=ORIENTED_EDGE('',*,*,#8993,.T.);
#11880=ORIENTED_EDGE('',*,*,#8993,.F.);
#11881=ORIENTED_EDGE('',*,*,#8994,.T.);
#11882=ORIENTED_EDGE('',*,*,#8994,.F.);
#11883=ORIENTED_EDGE('',*,*,#8995,.T.);
#11884=ORIENTED_EDGE('',*,*,#8995,.F.);
#11885=ORIENTED_EDGE('',*,*,#8996,.T.);
#11886=ORIENTED_EDGE('',*,*,#8996,.F.);
#11887=ORIENTED_EDGE('',*,*,#8997,.T.);
#11888=ORIENTED_EDGE('',*,*,#8997,.F.);
#11889=ORIENTED_EDGE('',*,*,#8998,.T.);
#11890=ORIENTED_EDGE('',*,*,#8998,.F.);
#11891=ORIENTED_EDGE('',*,*,#8999,.T.);
#11892=ORIENTED_EDGE('',*,*,#8999,.F.);
#11893=ORIENTED_EDGE('',*,*,#9000,.F.);
#11894=ORIENTED_EDGE('',*,*,#9001,.F.);
#11895=ORIENTED_EDGE('',*,*,#9002,.F.);
#11896=ORIENTED_EDGE('',*,*,#9003,.F.);
#11897=ORIENTED_EDGE('',*,*,#9002,.T.);
#11898=ORIENTED_EDGE('',*,*,#9004,.F.);
#11899=ORIENTED_EDGE('',*,*,#9005,.T.);
#11900=ORIENTED_EDGE('',*,*,#9006,.F.);
#11901=ORIENTED_EDGE('',*,*,#9007,.T.);
#11902=ORIENTED_EDGE('',*,*,#9008,.F.);
#11903=ORIENTED_EDGE('',*,*,#9009,.T.);
#11904=ORIENTED_EDGE('',*,*,#9010,.F.);
#11905=ORIENTED_EDGE('',*,*,#9009,.F.);
#11906=ORIENTED_EDGE('',*,*,#9011,.F.);
#11907=ORIENTED_EDGE('',*,*,#9012,.T.);
#11908=ORIENTED_EDGE('',*,*,#9013,.F.);
#11909=ORIENTED_EDGE('',*,*,#9014,.T.);
#11910=ORIENTED_EDGE('',*,*,#9015,.F.);
#11911=ORIENTED_EDGE('',*,*,#9016,.T.);
#11912=ORIENTED_EDGE('',*,*,#9017,.F.);
#11913=ORIENTED_EDGE('',*,*,#9018,.T.);
#11914=ORIENTED_EDGE('',*,*,#9019,.F.);
#11915=ORIENTED_EDGE('',*,*,#9001,.T.);
#11916=ORIENTED_EDGE('',*,*,#9020,.T.);
#11917=ORIENTED_EDGE('',*,*,#9021,.T.);
#11918=ORIENTED_EDGE('',*,*,#9004,.T.);
#11919=ORIENTED_EDGE('',*,*,#9022,.F.);
#11920=ORIENTED_EDGE('',*,*,#9023,.F.);
#11921=ORIENTED_EDGE('',*,*,#9005,.F.);
#11922=ORIENTED_EDGE('',*,*,#9021,.F.);
#11923=ORIENTED_EDGE('',*,*,#9023,.T.);
#11924=ORIENTED_EDGE('',*,*,#9024,.T.);
#11925=ORIENTED_EDGE('',*,*,#9025,.T.);
#11926=ORIENTED_EDGE('',*,*,#9006,.T.);
#11927=ORIENTED_EDGE('',*,*,#9026,.F.);
#11928=ORIENTED_EDGE('',*,*,#9027,.F.);
#11929=ORIENTED_EDGE('',*,*,#9007,.F.);
#11930=ORIENTED_EDGE('',*,*,#9025,.F.);
#11931=ORIENTED_EDGE('',*,*,#9027,.T.);
#11932=ORIENTED_EDGE('',*,*,#9028,.T.);
#11933=ORIENTED_EDGE('',*,*,#9029,.T.);
#11934=ORIENTED_EDGE('',*,*,#9030,.T.);
#11935=ORIENTED_EDGE('',*,*,#9011,.T.);
#11936=ORIENTED_EDGE('',*,*,#9008,.T.);
#11937=ORIENTED_EDGE('',*,*,#9031,.F.);
#11938=ORIENTED_EDGE('',*,*,#9032,.F.);
#11939=ORIENTED_EDGE('',*,*,#9012,.F.);
#11940=ORIENTED_EDGE('',*,*,#9030,.F.);
#11941=ORIENTED_EDGE('',*,*,#9032,.T.);
#11942=ORIENTED_EDGE('',*,*,#9033,.T.);
#11943=ORIENTED_EDGE('',*,*,#9034,.T.);
#11944=ORIENTED_EDGE('',*,*,#9013,.T.);
#11945=ORIENTED_EDGE('',*,*,#9035,.F.);
#11946=ORIENTED_EDGE('',*,*,#9036,.F.);
#11947=ORIENTED_EDGE('',*,*,#9014,.F.);
#11948=ORIENTED_EDGE('',*,*,#9034,.F.);
#11949=ORIENTED_EDGE('',*,*,#9036,.T.);
#11950=ORIENTED_EDGE('',*,*,#9037,.T.);
#11951=ORIENTED_EDGE('',*,*,#9038,.T.);
#11952=ORIENTED_EDGE('',*,*,#9015,.T.);
#11953=ORIENTED_EDGE('',*,*,#9016,.F.);
#11954=ORIENTED_EDGE('',*,*,#9038,.F.);
#11955=ORIENTED_EDGE('',*,*,#9039,.F.);
#11956=ORIENTED_EDGE('',*,*,#9040,.F.);
#11957=ORIENTED_EDGE('',*,*,#9041,.F.);
#11958=ORIENTED_EDGE('',*,*,#9042,.T.);
#11959=ORIENTED_EDGE('',*,*,#9028,.F.);
#11960=ORIENTED_EDGE('',*,*,#9026,.T.);
#11961=ORIENTED_EDGE('',*,*,#9024,.F.);
#11962=ORIENTED_EDGE('',*,*,#9022,.T.);
#11963=ORIENTED_EDGE('',*,*,#9020,.F.);
#11964=ORIENTED_EDGE('',*,*,#9000,.T.);
#11965=ORIENTED_EDGE('',*,*,#9043,.F.);
#11966=ORIENTED_EDGE('',*,*,#9044,.T.);
#11967=ORIENTED_EDGE('',*,*,#9045,.F.);
#11968=ORIENTED_EDGE('',*,*,#9039,.T.);
#11969=ORIENTED_EDGE('',*,*,#9037,.F.);
#11970=ORIENTED_EDGE('',*,*,#9035,.T.);
#11971=ORIENTED_EDGE('',*,*,#9033,.F.);
#11972=ORIENTED_EDGE('',*,*,#9031,.T.);
#11973=ORIENTED_EDGE('',*,*,#9029,.F.);
#11974=ORIENTED_EDGE('',*,*,#9042,.F.);
#11975=ORIENTED_EDGE('',*,*,#9003,.T.);
#11976=ORIENTED_EDGE('',*,*,#9019,.T.);
#11977=ORIENTED_EDGE('',*,*,#9046,.T.);
#11978=ORIENTED_EDGE('',*,*,#9043,.T.);
#11979=ORIENTED_EDGE('',*,*,#9018,.F.);
#11980=ORIENTED_EDGE('',*,*,#9047,.F.);
#11981=ORIENTED_EDGE('',*,*,#9044,.F.);
#11982=ORIENTED_EDGE('',*,*,#9046,.F.);
#11983=ORIENTED_EDGE('',*,*,#9010,.T.);
#11984=ORIENTED_EDGE('',*,*,#9041,.T.);
#11985=ORIENTED_EDGE('',*,*,#9040,.T.);
#11986=ORIENTED_EDGE('',*,*,#9045,.T.);
#11987=ORIENTED_EDGE('',*,*,#9047,.T.);
#11988=ORIENTED_EDGE('',*,*,#9017,.T.);
#11989=ORIENTED_EDGE('',*,*,#9048,.F.);
#11990=ORIENTED_EDGE('',*,*,#9049,.T.);
#11991=ORIENTED_EDGE('',*,*,#9050,.F.);
#11992=ORIENTED_EDGE('',*,*,#9051,.T.);
#11993=ORIENTED_EDGE('',*,*,#9048,.T.);
#11994=ORIENTED_EDGE('',*,*,#9051,.F.);
#11995=ORIENTED_EDGE('',*,*,#9050,.T.);
#11996=ORIENTED_EDGE('',*,*,#9052,.F.);
#11997=ORIENTED_EDGE('',*,*,#9052,.T.);
#11998=ORIENTED_EDGE('',*,*,#9053,.T.);
#11999=ORIENTED_EDGE('',*,*,#9049,.F.);
#12000=ORIENTED_EDGE('',*,*,#9053,.F.);
#12001=ORIENTED_EDGE('',*,*,#9054,.F.);
#12002=ORIENTED_EDGE('',*,*,#9055,.T.);
#12003=ORIENTED_EDGE('',*,*,#9056,.F.);
#12004=ORIENTED_EDGE('',*,*,#9057,.T.);
#12005=ORIENTED_EDGE('',*,*,#9054,.T.);
#12006=ORIENTED_EDGE('',*,*,#9057,.F.);
#12007=ORIENTED_EDGE('',*,*,#9056,.T.);
#12008=ORIENTED_EDGE('',*,*,#9058,.F.);
#12009=ORIENTED_EDGE('',*,*,#9058,.T.);
#12010=ORIENTED_EDGE('',*,*,#9059,.T.);
#12011=ORIENTED_EDGE('',*,*,#9055,.F.);
#12012=ORIENTED_EDGE('',*,*,#9059,.F.);
#12013=ORIENTED_EDGE('',*,*,#9060,.F.);
#12014=ORIENTED_EDGE('',*,*,#9061,.F.);
#12015=ORIENTED_EDGE('',*,*,#9062,.T.);
#12016=ORIENTED_EDGE('',*,*,#9063,.F.);
#12017=ORIENTED_EDGE('',*,*,#9064,.F.);
#12018=ORIENTED_EDGE('',*,*,#9062,.F.);
#12019=ORIENTED_EDGE('',*,*,#9063,.T.);
#12020=ORIENTED_EDGE('',*,*,#9064,.T.);
#12021=ORIENTED_EDGE('',*,*,#9065,.T.);
#12022=ORIENTED_EDGE('',*,*,#9066,.T.);
#12023=ORIENTED_EDGE('',*,*,#9065,.F.);
#12024=ORIENTED_EDGE('',*,*,#9067,.T.);
#12025=ORIENTED_EDGE('',*,*,#9068,.T.);
#12026=ORIENTED_EDGE('',*,*,#9069,.F.);
#12027=ORIENTED_EDGE('',*,*,#9068,.F.);
#12028=ORIENTED_EDGE('',*,*,#9069,.T.);
#12029=ORIENTED_EDGE('',*,*,#9070,.T.);
#12030=ORIENTED_EDGE('',*,*,#9071,.F.);
#12031=ORIENTED_EDGE('',*,*,#9070,.F.);
#12032=ORIENTED_EDGE('',*,*,#9066,.F.);
#12033=ORIENTED_EDGE('',*,*,#9071,.T.);
#12034=ORIENTED_EDGE('',*,*,#9072,.F.);
#12035=ORIENTED_EDGE('',*,*,#9073,.T.);
#12036=ORIENTED_EDGE('',*,*,#9060,.T.);
#12037=ORIENTED_EDGE('',*,*,#9061,.T.);
#12038=ORIENTED_EDGE('',*,*,#9073,.F.);
#12039=ORIENTED_EDGE('',*,*,#9072,.T.);
#12040=ORIENTED_EDGE('',*,*,#9074,.F.);
#12041=ORIENTED_EDGE('',*,*,#9074,.T.);
#12042=ORIENTED_EDGE('',*,*,#9075,.T.);
#12043=ORIENTED_EDGE('',*,*,#9067,.F.);
#12044=ORIENTED_EDGE('',*,*,#9075,.F.);
#12045=ORIENTED_EDGE('',*,*,#9076,.F.);
#12046=ORIENTED_EDGE('',*,*,#9077,.F.);
#12047=ORIENTED_EDGE('',*,*,#9078,.T.);
#12048=ORIENTED_EDGE('',*,*,#9079,.F.);
#12049=ORIENTED_EDGE('',*,*,#9080,.F.);
#12050=ORIENTED_EDGE('',*,*,#9078,.F.);
#12051=ORIENTED_EDGE('',*,*,#9081,.T.);
#12052=ORIENTED_EDGE('',*,*,#9082,.T.);
#12053=ORIENTED_EDGE('',*,*,#9079,.T.);
#12054=ORIENTED_EDGE('',*,*,#9080,.T.);
#12055=ORIENTED_EDGE('',*,*,#9082,.F.);
#12056=ORIENTED_EDGE('',*,*,#9083,.F.);
#12057=ORIENTED_EDGE('',*,*,#9084,.T.);
#12058=ORIENTED_EDGE('',*,*,#9085,.F.);
#12059=ORIENTED_EDGE('',*,*,#9086,.T.);
#12060=ORIENTED_EDGE('',*,*,#9083,.T.);
#12061=ORIENTED_EDGE('',*,*,#9086,.F.);
#12062=ORIENTED_EDGE('',*,*,#9087,.F.);
#12063=ORIENTED_EDGE('',*,*,#9088,.T.);
#12064=ORIENTED_EDGE('',*,*,#9085,.T.);
#12065=ORIENTED_EDGE('',*,*,#9088,.F.);
#12066=ORIENTED_EDGE('',*,*,#9089,.F.);
#12067=ORIENTED_EDGE('',*,*,#9090,.T.);
#12068=ORIENTED_EDGE('',*,*,#9087,.T.);
#12069=ORIENTED_EDGE('',*,*,#9090,.F.);
#12070=ORIENTED_EDGE('',*,*,#9089,.T.);
#12071=ORIENTED_EDGE('',*,*,#9081,.F.);
#12072=ORIENTED_EDGE('',*,*,#9076,.T.);
#12073=ORIENTED_EDGE('',*,*,#9077,.T.);
#12074=ORIENTED_EDGE('',*,*,#9091,.T.);
#12075=ORIENTED_EDGE('',*,*,#9084,.F.);
#12076=ORIENTED_EDGE('',*,*,#9091,.F.);
#12077=ORIENTED_EDGE('',*,*,#9092,.T.);
#12078=ORIENTED_EDGE('',*,*,#9092,.F.);
#12079=ORIENTED_EDGE('',*,*,#9093,.T.);
#12080=ORIENTED_EDGE('',*,*,#9093,.F.);
#12081=ORIENTED_EDGE('',*,*,#9094,.T.);
#12082=ORIENTED_EDGE('',*,*,#9094,.F.);
#12083=ORIENTED_EDGE('',*,*,#9095,.T.);
#12084=ORIENTED_EDGE('',*,*,#9095,.F.);
#12085=ORIENTED_EDGE('',*,*,#9096,.T.);
#12086=ORIENTED_EDGE('',*,*,#9096,.F.);
#12087=ORIENTED_EDGE('',*,*,#9097,.T.);
#12088=ORIENTED_EDGE('',*,*,#9097,.F.);
#12089=ORIENTED_EDGE('',*,*,#9098,.T.);
#12090=ORIENTED_EDGE('',*,*,#9098,.F.);
#12091=ORIENTED_EDGE('',*,*,#9099,.T.);
#12092=ORIENTED_EDGE('',*,*,#9099,.F.);
#12093=ORIENTED_EDGE('',*,*,#9100,.F.);
#12094=ORIENTED_EDGE('',*,*,#9101,.F.);
#12095=ORIENTED_EDGE('',*,*,#9102,.F.);
#12096=ORIENTED_EDGE('',*,*,#9103,.F.);
#12097=ORIENTED_EDGE('',*,*,#9102,.T.);
#12098=ORIENTED_EDGE('',*,*,#9104,.F.);
#12099=ORIENTED_EDGE('',*,*,#9105,.T.);
#12100=ORIENTED_EDGE('',*,*,#9106,.F.);
#12101=ORIENTED_EDGE('',*,*,#9107,.T.);
#12102=ORIENTED_EDGE('',*,*,#9108,.F.);
#12103=ORIENTED_EDGE('',*,*,#9109,.T.);
#12104=ORIENTED_EDGE('',*,*,#9110,.T.);
#12105=ORIENTED_EDGE('',*,*,#9111,.F.);
#12106=ORIENTED_EDGE('',*,*,#9110,.F.);
#12107=ORIENTED_EDGE('',*,*,#9112,.T.);
#12108=ORIENTED_EDGE('',*,*,#9113,.F.);
#12109=ORIENTED_EDGE('',*,*,#9114,.T.);
#12110=ORIENTED_EDGE('',*,*,#9115,.F.);
#12111=ORIENTED_EDGE('',*,*,#9116,.T.);
#12112=ORIENTED_EDGE('',*,*,#9117,.F.);
#12113=ORIENTED_EDGE('',*,*,#9118,.T.);
#12114=ORIENTED_EDGE('',*,*,#9119,.F.);
#12115=ORIENTED_EDGE('',*,*,#9120,.T.);
#12116=ORIENTED_EDGE('',*,*,#9121,.F.);
#12117=ORIENTED_EDGE('',*,*,#9101,.T.);
#12118=ORIENTED_EDGE('',*,*,#9122,.T.);
#12119=ORIENTED_EDGE('',*,*,#9123,.T.);
#12120=ORIENTED_EDGE('',*,*,#9104,.T.);
#12121=ORIENTED_EDGE('',*,*,#9124,.F.);
#12122=ORIENTED_EDGE('',*,*,#9125,.F.);
#12123=ORIENTED_EDGE('',*,*,#9105,.F.);
#12124=ORIENTED_EDGE('',*,*,#9123,.F.);
#12125=ORIENTED_EDGE('',*,*,#9125,.T.);
#12126=ORIENTED_EDGE('',*,*,#9126,.T.);
#12127=ORIENTED_EDGE('',*,*,#9127,.T.);
#12128=ORIENTED_EDGE('',*,*,#9106,.T.);
#12129=ORIENTED_EDGE('',*,*,#9128,.F.);
#12130=ORIENTED_EDGE('',*,*,#9129,.F.);
#12131=ORIENTED_EDGE('',*,*,#9107,.F.);
#12132=ORIENTED_EDGE('',*,*,#9127,.F.);
#12133=ORIENTED_EDGE('',*,*,#9129,.T.);
#12134=ORIENTED_EDGE('',*,*,#9130,.T.);
#12135=ORIENTED_EDGE('',*,*,#9131,.T.);
#12136=ORIENTED_EDGE('',*,*,#9108,.T.);
#12137=ORIENTED_EDGE('',*,*,#9132,.F.);
#12138=ORIENTED_EDGE('',*,*,#9133,.F.);
#12139=ORIENTED_EDGE('',*,*,#9112,.F.);
#12140=ORIENTED_EDGE('',*,*,#9109,.F.);
#12141=ORIENTED_EDGE('',*,*,#9131,.F.);
#12142=ORIENTED_EDGE('',*,*,#9134,.F.);
#12143=ORIENTED_EDGE('',*,*,#9133,.T.);
#12144=ORIENTED_EDGE('',*,*,#9135,.T.);
#12145=ORIENTED_EDGE('',*,*,#9136,.T.);
#12146=ORIENTED_EDGE('',*,*,#9113,.T.);
#12147=ORIENTED_EDGE('',*,*,#9137,.F.);
#12148=ORIENTED_EDGE('',*,*,#9138,.F.);
#12149=ORIENTED_EDGE('',*,*,#9114,.F.);
#12150=ORIENTED_EDGE('',*,*,#9136,.F.);
#12151=ORIENTED_EDGE('',*,*,#9138,.T.);
#12152=ORIENTED_EDGE('',*,*,#9139,.T.);
#12153=ORIENTED_EDGE('',*,*,#9140,.T.);
#12154=ORIENTED_EDGE('',*,*,#9115,.T.);
#12155=ORIENTED_EDGE('',*,*,#9141,.F.);
#12156=ORIENTED_EDGE('',*,*,#9142,.F.);
#12157=ORIENTED_EDGE('',*,*,#9116,.F.);
#12158=ORIENTED_EDGE('',*,*,#9140,.F.);
#12159=ORIENTED_EDGE('',*,*,#9142,.T.);
#12160=ORIENTED_EDGE('',*,*,#9143,.T.);
#12161=ORIENTED_EDGE('',*,*,#9144,.T.);
#12162=ORIENTED_EDGE('',*,*,#9117,.T.);
#12163=ORIENTED_EDGE('',*,*,#9118,.F.);
#12164=ORIENTED_EDGE('',*,*,#9144,.F.);
#12165=ORIENTED_EDGE('',*,*,#9145,.F.);
#12166=ORIENTED_EDGE('',*,*,#9146,.F.);
#12167=ORIENTED_EDGE('',*,*,#9147,.F.);
#12168=ORIENTED_EDGE('',*,*,#9148,.T.);
#12169=ORIENTED_EDGE('',*,*,#9134,.T.);
#12170=ORIENTED_EDGE('',*,*,#9130,.F.);
#12171=ORIENTED_EDGE('',*,*,#9128,.T.);
#12172=ORIENTED_EDGE('',*,*,#9126,.F.);
#12173=ORIENTED_EDGE('',*,*,#9124,.T.);
#12174=ORIENTED_EDGE('',*,*,#9122,.F.);
#12175=ORIENTED_EDGE('',*,*,#9100,.T.);
#12176=ORIENTED_EDGE('',*,*,#9149,.F.);
#12177=ORIENTED_EDGE('',*,*,#9150,.T.);
#12178=ORIENTED_EDGE('',*,*,#9151,.F.);
#12179=ORIENTED_EDGE('',*,*,#9145,.T.);
#12180=ORIENTED_EDGE('',*,*,#9143,.F.);
#12181=ORIENTED_EDGE('',*,*,#9141,.T.);
#12182=ORIENTED_EDGE('',*,*,#9139,.F.);
#12183=ORIENTED_EDGE('',*,*,#9137,.T.);
#12184=ORIENTED_EDGE('',*,*,#9135,.F.);
#12185=ORIENTED_EDGE('',*,*,#9132,.T.);
#12186=ORIENTED_EDGE('',*,*,#9148,.F.);
#12187=ORIENTED_EDGE('',*,*,#9103,.T.);
#12188=ORIENTED_EDGE('',*,*,#9121,.T.);
#12189=ORIENTED_EDGE('',*,*,#9152,.T.);
#12190=ORIENTED_EDGE('',*,*,#9149,.T.);
#12191=ORIENTED_EDGE('',*,*,#9120,.F.);
#12192=ORIENTED_EDGE('',*,*,#9153,.F.);
#12193=ORIENTED_EDGE('',*,*,#9150,.F.);
#12194=ORIENTED_EDGE('',*,*,#9152,.F.);
#12195=ORIENTED_EDGE('',*,*,#9111,.T.);
#12196=ORIENTED_EDGE('',*,*,#9147,.T.);
#12197=ORIENTED_EDGE('',*,*,#9146,.T.);
#12198=ORIENTED_EDGE('',*,*,#9151,.T.);
#12199=ORIENTED_EDGE('',*,*,#9153,.T.);
#12200=ORIENTED_EDGE('',*,*,#9119,.T.);
#12201=ORIENTED_EDGE('',*,*,#9154,.F.);
#12202=ORIENTED_EDGE('',*,*,#9155,.T.);
#12203=ORIENTED_EDGE('',*,*,#9156,.F.);
#12204=ORIENTED_EDGE('',*,*,#9157,.T.);
#12205=ORIENTED_EDGE('',*,*,#9154,.T.);
#12206=ORIENTED_EDGE('',*,*,#9157,.F.);
#12207=ORIENTED_EDGE('',*,*,#9156,.T.);
#12208=ORIENTED_EDGE('',*,*,#9158,.F.);
#12209=ORIENTED_EDGE('',*,*,#9158,.T.);
#12210=ORIENTED_EDGE('',*,*,#9159,.T.);
#12211=ORIENTED_EDGE('',*,*,#9155,.F.);
#12212=ORIENTED_EDGE('',*,*,#9159,.F.);
#12213=ORIENTED_EDGE('',*,*,#9160,.F.);
#12214=ORIENTED_EDGE('',*,*,#9161,.T.);
#12215=ORIENTED_EDGE('',*,*,#9162,.F.);
#12216=ORIENTED_EDGE('',*,*,#9163,.T.);
#12217=ORIENTED_EDGE('',*,*,#9160,.T.);
#12218=ORIENTED_EDGE('',*,*,#9163,.F.);
#12219=ORIENTED_EDGE('',*,*,#9162,.T.);
#12220=ORIENTED_EDGE('',*,*,#9164,.F.);
#12221=ORIENTED_EDGE('',*,*,#9164,.T.);
#12222=ORIENTED_EDGE('',*,*,#9165,.T.);
#12223=ORIENTED_EDGE('',*,*,#9161,.F.);
#12224=ORIENTED_EDGE('',*,*,#9165,.F.);
#12225=ORIENTED_EDGE('',*,*,#9166,.F.);
#12226=ORIENTED_EDGE('',*,*,#9167,.F.);
#12227=ORIENTED_EDGE('',*,*,#9168,.T.);
#12228=ORIENTED_EDGE('',*,*,#9166,.T.);
#12229=ORIENTED_EDGE('',*,*,#9168,.F.);
#12230=ORIENTED_EDGE('',*,*,#9169,.F.);
#12231=ORIENTED_EDGE('',*,*,#9170,.T.);
#12232=ORIENTED_EDGE('',*,*,#9167,.T.);
#12233=ORIENTED_EDGE('',*,*,#9170,.F.);
#12234=ORIENTED_EDGE('',*,*,#9171,.F.);
#12235=ORIENTED_EDGE('',*,*,#9172,.T.);
#12236=ORIENTED_EDGE('',*,*,#9169,.T.);
#12237=ORIENTED_EDGE('',*,*,#9172,.F.);
#12238=ORIENTED_EDGE('',*,*,#9171,.T.);
#12239=ORIENTED_EDGE('',*,*,#9173,.F.);
#12240=ORIENTED_EDGE('',*,*,#9174,.F.);
#12241=ORIENTED_EDGE('',*,*,#9175,.T.);
#12242=ORIENTED_EDGE('',*,*,#9173,.T.);
#12243=ORIENTED_EDGE('',*,*,#9175,.F.);
#12244=ORIENTED_EDGE('',*,*,#9176,.F.);
#12245=ORIENTED_EDGE('',*,*,#9177,.T.);
#12246=ORIENTED_EDGE('',*,*,#9174,.T.);
#12247=ORIENTED_EDGE('',*,*,#9177,.F.);
#12248=ORIENTED_EDGE('',*,*,#9178,.F.);
#12249=ORIENTED_EDGE('',*,*,#9179,.T.);
#12250=ORIENTED_EDGE('',*,*,#9176,.T.);
#12251=ORIENTED_EDGE('',*,*,#9179,.F.);
#12252=ORIENTED_EDGE('',*,*,#9178,.T.);
#12253=ORIENTED_EDGE('',*,*,#9180,.T.);
#12254=ORIENTED_EDGE('',*,*,#9181,.T.);
#12255=ORIENTED_EDGE('',*,*,#9182,.T.);
#12256=ORIENTED_EDGE('',*,*,#9183,.F.);
#12257=ORIENTED_EDGE('',*,*,#9184,.T.);
#12258=ORIENTED_EDGE('',*,*,#9185,.T.);
#12259=ORIENTED_EDGE('',*,*,#9186,.T.);
#12260=ORIENTED_EDGE('',*,*,#9181,.F.);
#12261=ORIENTED_EDGE('',*,*,#9187,.T.);
#12262=ORIENTED_EDGE('',*,*,#9188,.T.);
#12263=ORIENTED_EDGE('',*,*,#9189,.T.);
#12264=ORIENTED_EDGE('',*,*,#9185,.F.);
#12265=ORIENTED_EDGE('',*,*,#9190,.T.);
#12266=ORIENTED_EDGE('',*,*,#9191,.T.);
#12267=ORIENTED_EDGE('',*,*,#9192,.T.);
#12268=ORIENTED_EDGE('',*,*,#9188,.F.);
#12269=ORIENTED_EDGE('',*,*,#9193,.T.);
#12270=ORIENTED_EDGE('',*,*,#9194,.T.);
#12271=ORIENTED_EDGE('',*,*,#9195,.T.);
#12272=ORIENTED_EDGE('',*,*,#9191,.F.);
#12273=ORIENTED_EDGE('',*,*,#9196,.T.);
#12274=ORIENTED_EDGE('',*,*,#9183,.T.);
#12275=ORIENTED_EDGE('',*,*,#9197,.T.);
#12276=ORIENTED_EDGE('',*,*,#9194,.F.);
#12277=ORIENTED_EDGE('',*,*,#9196,.F.);
#12278=ORIENTED_EDGE('',*,*,#9193,.F.);
#12279=ORIENTED_EDGE('',*,*,#9190,.F.);
#12280=ORIENTED_EDGE('',*,*,#9187,.F.);
#12281=ORIENTED_EDGE('',*,*,#9184,.F.);
#12282=ORIENTED_EDGE('',*,*,#9180,.F.);
#12283=ORIENTED_EDGE('',*,*,#9197,.F.);
#12284=ORIENTED_EDGE('',*,*,#9182,.F.);
#12285=ORIENTED_EDGE('',*,*,#9186,.F.);
#12286=ORIENTED_EDGE('',*,*,#9189,.F.);
#12287=ORIENTED_EDGE('',*,*,#9192,.F.);
#12288=ORIENTED_EDGE('',*,*,#9195,.F.);
#12289=ORIENTED_EDGE('',*,*,#9198,.F.);
#12290=ORIENTED_EDGE('',*,*,#9199,.T.);
#12291=ORIENTED_EDGE('',*,*,#9200,.F.);
#12292=ORIENTED_EDGE('',*,*,#9201,.T.);
#12293=ORIENTED_EDGE('',*,*,#9202,.F.);
#12294=ORIENTED_EDGE('',*,*,#9201,.F.);
#12295=ORIENTED_EDGE('',*,*,#9203,.F.);
#12296=ORIENTED_EDGE('',*,*,#9204,.F.);
#12297=ORIENTED_EDGE('',*,*,#9205,.F.);
#12298=ORIENTED_EDGE('',*,*,#9204,.T.);
#12299=ORIENTED_EDGE('',*,*,#9206,.T.);
#12300=ORIENTED_EDGE('',*,*,#9207,.T.);
#12301=ORIENTED_EDGE('',*,*,#9203,.T.);
#12302=ORIENTED_EDGE('',*,*,#9200,.T.);
#12303=ORIENTED_EDGE('',*,*,#9208,.T.);
#12304=ORIENTED_EDGE('',*,*,#9206,.F.);
#12305=ORIENTED_EDGE('',*,*,#9209,.F.);
#12306=ORIENTED_EDGE('',*,*,#9207,.F.);
#12307=ORIENTED_EDGE('',*,*,#9208,.F.);
#12308=ORIENTED_EDGE('',*,*,#9199,.F.);
#12309=ORIENTED_EDGE('',*,*,#9210,.F.);
#12310=ORIENTED_EDGE('',*,*,#9211,.T.);
#12311=ORIENTED_EDGE('',*,*,#9212,.T.);
#12312=ORIENTED_EDGE('',*,*,#9211,.F.);
#12313=ORIENTED_EDGE('',*,*,#9205,.T.);
#12314=ORIENTED_EDGE('',*,*,#9209,.T.);
#12315=ORIENTED_EDGE('',*,*,#9198,.T.);
#12316=ORIENTED_EDGE('',*,*,#9202,.T.);
#12317=ORIENTED_EDGE('',*,*,#9210,.T.);
#12318=ORIENTED_EDGE('',*,*,#9212,.F.);
#12319=ORIENTED_EDGE('',*,*,#9213,.F.);
#12320=ORIENTED_EDGE('',*,*,#9214,.T.);
#12321=ORIENTED_EDGE('',*,*,#9215,.F.);
#12322=ORIENTED_EDGE('',*,*,#9216,.F.);
#12323=ORIENTED_EDGE('',*,*,#9217,.T.);
#12324=ORIENTED_EDGE('',*,*,#9218,.F.);
#12325=ORIENTED_EDGE('',*,*,#9219,.F.);
#12326=ORIENTED_EDGE('',*,*,#9217,.F.);
#12327=ORIENTED_EDGE('',*,*,#9220,.F.);
#12328=ORIENTED_EDGE('',*,*,#9221,.F.);
#12329=ORIENTED_EDGE('',*,*,#9214,.F.);
#12330=ORIENTED_EDGE('',*,*,#9222,.F.);
#12331=ORIENTED_EDGE('',*,*,#9220,.T.);
#12332=ORIENTED_EDGE('',*,*,#9216,.T.);
#12333=ORIENTED_EDGE('',*,*,#9223,.F.);
#12334=ORIENTED_EDGE('',*,*,#9224,.T.);
#12335=ORIENTED_EDGE('',*,*,#9225,.T.);
#12336=ORIENTED_EDGE('',*,*,#9224,.F.);
#12337=ORIENTED_EDGE('',*,*,#9221,.T.);
#12338=ORIENTED_EDGE('',*,*,#9222,.T.);
#12339=ORIENTED_EDGE('',*,*,#9215,.T.);
#12340=ORIENTED_EDGE('',*,*,#9213,.T.);
#12341=ORIENTED_EDGE('',*,*,#9226,.F.);
#12342=ORIENTED_EDGE('',*,*,#9227,.T.);
#12343=ORIENTED_EDGE('',*,*,#9228,.T.);
#12344=ORIENTED_EDGE('',*,*,#9227,.F.);
#12345=ORIENTED_EDGE('',*,*,#9218,.T.);
#12346=ORIENTED_EDGE('',*,*,#9219,.T.);
#12347=ORIENTED_EDGE('',*,*,#9226,.T.);
#12348=ORIENTED_EDGE('',*,*,#9223,.T.);
#12349=ORIENTED_EDGE('',*,*,#9228,.F.);
#12350=ORIENTED_EDGE('',*,*,#9225,.F.);
#12351=ORIENTED_EDGE('',*,*,#9229,.F.);
#12352=ORIENTED_EDGE('',*,*,#9230,.T.);
#12353=ORIENTED_EDGE('',*,*,#9231,.F.);
#12354=ORIENTED_EDGE('',*,*,#9232,.F.);
#12355=ORIENTED_EDGE('',*,*,#9233,.T.);
#12356=ORIENTED_EDGE('',*,*,#9234,.F.);
#12357=ORIENTED_EDGE('',*,*,#9235,.F.);
#12358=ORIENTED_EDGE('',*,*,#9233,.F.);
#12359=ORIENTED_EDGE('',*,*,#9236,.F.);
#12360=ORIENTED_EDGE('',*,*,#9237,.F.);
#12361=ORIENTED_EDGE('',*,*,#9230,.F.);
#12362=ORIENTED_EDGE('',*,*,#9238,.F.);
#12363=ORIENTED_EDGE('',*,*,#9236,.T.);
#12364=ORIENTED_EDGE('',*,*,#9232,.T.);
#12365=ORIENTED_EDGE('',*,*,#9239,.F.);
#12366=ORIENTED_EDGE('',*,*,#9240,.T.);
#12367=ORIENTED_EDGE('',*,*,#9241,.T.);
#12368=ORIENTED_EDGE('',*,*,#9240,.F.);
#12369=ORIENTED_EDGE('',*,*,#9237,.T.);
#12370=ORIENTED_EDGE('',*,*,#9238,.T.);
#12371=ORIENTED_EDGE('',*,*,#9231,.T.);
#12372=ORIENTED_EDGE('',*,*,#9229,.T.);
#12373=ORIENTED_EDGE('',*,*,#9242,.F.);
#12374=ORIENTED_EDGE('',*,*,#9243,.T.);
#12375=ORIENTED_EDGE('',*,*,#9244,.T.);
#12376=ORIENTED_EDGE('',*,*,#9243,.F.);
#12377=ORIENTED_EDGE('',*,*,#9234,.T.);
#12378=ORIENTED_EDGE('',*,*,#9235,.T.);
#12379=ORIENTED_EDGE('',*,*,#9242,.T.);
#12380=ORIENTED_EDGE('',*,*,#9239,.T.);
#12381=ORIENTED_EDGE('',*,*,#9244,.F.);
#12382=ORIENTED_EDGE('',*,*,#9241,.F.);
#12383=ORIENTED_EDGE('',*,*,#9245,.F.);
#12384=ORIENTED_EDGE('',*,*,#9246,.T.);
#12385=ORIENTED_EDGE('',*,*,#9247,.T.);
#12386=ORIENTED_EDGE('',*,*,#9246,.F.);
#12387=ORIENTED_EDGE('',*,*,#9248,.F.);
#12388=ORIENTED_EDGE('',*,*,#9249,.T.);
#12389=ORIENTED_EDGE('',*,*,#9250,.T.);
#12390=ORIENTED_EDGE('',*,*,#9249,.F.);
#12391=ORIENTED_EDGE('',*,*,#9248,.T.);
#12392=ORIENTED_EDGE('',*,*,#9245,.T.);
#12393=ORIENTED_EDGE('',*,*,#9250,.F.);
#12394=ORIENTED_EDGE('',*,*,#9247,.F.);
#12395=ORIENTED_EDGE('',*,*,#9251,.F.);
#12396=ORIENTED_EDGE('',*,*,#9252,.T.);
#12397=ORIENTED_EDGE('',*,*,#9253,.T.);
#12398=ORIENTED_EDGE('',*,*,#9252,.F.);
#12399=ORIENTED_EDGE('',*,*,#9254,.F.);
#12400=ORIENTED_EDGE('',*,*,#9255,.T.);
#12401=ORIENTED_EDGE('',*,*,#9256,.T.);
#12402=ORIENTED_EDGE('',*,*,#9255,.F.);
#12403=ORIENTED_EDGE('',*,*,#9254,.T.);
#12404=ORIENTED_EDGE('',*,*,#9251,.T.);
#12405=ORIENTED_EDGE('',*,*,#9256,.F.);
#12406=ORIENTED_EDGE('',*,*,#9253,.F.);
#12407=ORIENTED_EDGE('',*,*,#9257,.F.);
#12408=ORIENTED_EDGE('',*,*,#9258,.T.);
#12409=ORIENTED_EDGE('',*,*,#9259,.T.);
#12410=ORIENTED_EDGE('',*,*,#9258,.F.);
#12411=ORIENTED_EDGE('',*,*,#9260,.F.);
#12412=ORIENTED_EDGE('',*,*,#9261,.T.);
#12413=ORIENTED_EDGE('',*,*,#9262,.T.);
#12414=ORIENTED_EDGE('',*,*,#9261,.F.);
#12415=ORIENTED_EDGE('',*,*,#9260,.T.);
#12416=ORIENTED_EDGE('',*,*,#9257,.T.);
#12417=ORIENTED_EDGE('',*,*,#9262,.F.);
#12418=ORIENTED_EDGE('',*,*,#9259,.F.);
#12419=ORIENTED_EDGE('',*,*,#9263,.F.);
#12420=ORIENTED_EDGE('',*,*,#9264,.T.);
#12421=ORIENTED_EDGE('',*,*,#9265,.T.);
#12422=ORIENTED_EDGE('',*,*,#9264,.F.);
#12423=ORIENTED_EDGE('',*,*,#9266,.F.);
#12424=ORIENTED_EDGE('',*,*,#9267,.T.);
#12425=ORIENTED_EDGE('',*,*,#9268,.T.);
#12426=ORIENTED_EDGE('',*,*,#9267,.F.);
#12427=ORIENTED_EDGE('',*,*,#9266,.T.);
#12428=ORIENTED_EDGE('',*,*,#9263,.T.);
#12429=ORIENTED_EDGE('',*,*,#9268,.F.);
#12430=ORIENTED_EDGE('',*,*,#9265,.F.);
#12431=ORIENTED_EDGE('',*,*,#9269,.F.);
#12432=ORIENTED_EDGE('',*,*,#9270,.F.);
#12433=ORIENTED_EDGE('',*,*,#9271,.F.);
#12434=ORIENTED_EDGE('',*,*,#9272,.F.);
#12435=ORIENTED_EDGE('',*,*,#9273,.F.);
#12436=ORIENTED_EDGE('',*,*,#9274,.T.);
#12437=ORIENTED_EDGE('',*,*,#9275,.F.);
#12438=ORIENTED_EDGE('',*,*,#9270,.T.);
#12439=ORIENTED_EDGE('',*,*,#9276,.F.);
#12440=ORIENTED_EDGE('',*,*,#9277,.F.);
#12441=ORIENTED_EDGE('',*,*,#9278,.F.);
#12442=ORIENTED_EDGE('',*,*,#9274,.F.);
#12443=ORIENTED_EDGE('',*,*,#9279,.T.);
#12444=ORIENTED_EDGE('',*,*,#9280,.T.);
#12445=ORIENTED_EDGE('',*,*,#9281,.T.);
#12446=ORIENTED_EDGE('',*,*,#9282,.T.);
#12447=ORIENTED_EDGE('',*,*,#9283,.T.);
#12448=ORIENTED_EDGE('',*,*,#9284,.T.);
#12449=ORIENTED_EDGE('',*,*,#9285,.T.);
#12450=ORIENTED_EDGE('',*,*,#9286,.T.);
#12451=ORIENTED_EDGE('',*,*,#9287,.T.);
#12452=ORIENTED_EDGE('',*,*,#9288,.T.);
#12453=ORIENTED_EDGE('',*,*,#9289,.T.);
#12454=ORIENTED_EDGE('',*,*,#9290,.T.);
#12455=ORIENTED_EDGE('',*,*,#9291,.T.);
#12456=ORIENTED_EDGE('',*,*,#9292,.T.);
#12457=ORIENTED_EDGE('',*,*,#9293,.T.);
#12458=ORIENTED_EDGE('',*,*,#9294,.T.);
#12459=ORIENTED_EDGE('',*,*,#9295,.T.);
#12460=ORIENTED_EDGE('',*,*,#9296,.T.);
#12461=ORIENTED_EDGE('',*,*,#9297,.T.);
#12462=ORIENTED_EDGE('',*,*,#9298,.T.);
#12463=ORIENTED_EDGE('',*,*,#9299,.T.);
#12464=ORIENTED_EDGE('',*,*,#9300,.T.);
#12465=ORIENTED_EDGE('',*,*,#9301,.T.);
#12466=ORIENTED_EDGE('',*,*,#9302,.T.);
#12467=ORIENTED_EDGE('',*,*,#9303,.T.);
#12468=ORIENTED_EDGE('',*,*,#9304,.T.);
#12469=ORIENTED_EDGE('',*,*,#9305,.T.);
#12470=ORIENTED_EDGE('',*,*,#9306,.T.);
#12471=ORIENTED_EDGE('',*,*,#9307,.T.);
#12472=ORIENTED_EDGE('',*,*,#9308,.T.);
#12473=ORIENTED_EDGE('',*,*,#9309,.T.);
#12474=ORIENTED_EDGE('',*,*,#9310,.T.);
#12475=ORIENTED_EDGE('',*,*,#9311,.T.);
#12476=ORIENTED_EDGE('',*,*,#9312,.T.);
#12477=ORIENTED_EDGE('',*,*,#9313,.T.);
#12478=ORIENTED_EDGE('',*,*,#9314,.T.);
#12479=ORIENTED_EDGE('',*,*,#9315,.T.);
#12480=ORIENTED_EDGE('',*,*,#9316,.T.);
#12481=ORIENTED_EDGE('',*,*,#9317,.T.);
#12482=ORIENTED_EDGE('',*,*,#9318,.T.);
#12483=ORIENTED_EDGE('',*,*,#9319,.T.);
#12484=ORIENTED_EDGE('',*,*,#9320,.T.);
#12485=ORIENTED_EDGE('',*,*,#9321,.T.);
#12486=ORIENTED_EDGE('',*,*,#9322,.T.);
#12487=ORIENTED_EDGE('',*,*,#9323,.T.);
#12488=ORIENTED_EDGE('',*,*,#9324,.T.);
#12489=ORIENTED_EDGE('',*,*,#9325,.T.);
#12490=ORIENTED_EDGE('',*,*,#9326,.T.);
#12491=ORIENTED_EDGE('',*,*,#9327,.T.);
#12492=ORIENTED_EDGE('',*,*,#9328,.T.);
#12493=ORIENTED_EDGE('',*,*,#9329,.T.);
#12494=ORIENTED_EDGE('',*,*,#9330,.T.);
#12495=ORIENTED_EDGE('',*,*,#9331,.T.);
#12496=ORIENTED_EDGE('',*,*,#9332,.T.);
#12497=ORIENTED_EDGE('',*,*,#9333,.T.);
#12498=ORIENTED_EDGE('',*,*,#9334,.T.);
#12499=ORIENTED_EDGE('',*,*,#9335,.T.);
#12500=ORIENTED_EDGE('',*,*,#9336,.T.);
#12501=ORIENTED_EDGE('',*,*,#9337,.T.);
#12502=ORIENTED_EDGE('',*,*,#9338,.T.);
#12503=ORIENTED_EDGE('',*,*,#9339,.T.);
#12504=ORIENTED_EDGE('',*,*,#9340,.T.);
#12505=ORIENTED_EDGE('',*,*,#9341,.T.);
#12506=ORIENTED_EDGE('',*,*,#9342,.T.);
#12507=ORIENTED_EDGE('',*,*,#9343,.T.);
#12508=ORIENTED_EDGE('',*,*,#9344,.T.);
#12509=ORIENTED_EDGE('',*,*,#9345,.T.);
#12510=ORIENTED_EDGE('',*,*,#9346,.T.);
#12511=ORIENTED_EDGE('',*,*,#9347,.T.);
#12512=ORIENTED_EDGE('',*,*,#9348,.T.);
#12513=ORIENTED_EDGE('',*,*,#9349,.T.);
#12514=ORIENTED_EDGE('',*,*,#9350,.T.);
#12515=ORIENTED_EDGE('',*,*,#9351,.T.);
#12516=ORIENTED_EDGE('',*,*,#9352,.T.);
#12517=ORIENTED_EDGE('',*,*,#9353,.T.);
#12518=ORIENTED_EDGE('',*,*,#9354,.T.);
#12519=ORIENTED_EDGE('',*,*,#9355,.T.);
#12520=ORIENTED_EDGE('',*,*,#9356,.T.);
#12521=ORIENTED_EDGE('',*,*,#9357,.T.);
#12522=ORIENTED_EDGE('',*,*,#9358,.T.);
#12523=ORIENTED_EDGE('',*,*,#9271,.T.);
#12524=ORIENTED_EDGE('',*,*,#9275,.T.);
#12525=ORIENTED_EDGE('',*,*,#9278,.T.);
#12526=ORIENTED_EDGE('',*,*,#9359,.T.);
#12527=ORIENTED_EDGE('',*,*,#9272,.T.);
#12528=ORIENTED_EDGE('',*,*,#9359,.F.);
#12529=ORIENTED_EDGE('',*,*,#9277,.T.);
#12530=ORIENTED_EDGE('',*,*,#9360,.F.);
#12531=ORIENTED_EDGE('',*,*,#9361,.F.);
#12532=ORIENTED_EDGE('',*,*,#9362,.T.);
#12533=ORIENTED_EDGE('',*,*,#9363,.F.);
#12534=ORIENTED_EDGE('',*,*,#9362,.F.);
#12535=ORIENTED_EDGE('',*,*,#9361,.T.);
#12536=ORIENTED_EDGE('',*,*,#9269,.T.);
#12537=ORIENTED_EDGE('',*,*,#9360,.T.);
#12538=ORIENTED_EDGE('',*,*,#9276,.T.);
#12539=ORIENTED_EDGE('',*,*,#9273,.T.);
#12540=ORIENTED_EDGE('',*,*,#9364,.F.);
#12541=ORIENTED_EDGE('',*,*,#9365,.F.);
#12542=ORIENTED_EDGE('',*,*,#9366,.F.);
#12543=ORIENTED_EDGE('',*,*,#9356,.F.);
#12544=ORIENTED_EDGE('',*,*,#9366,.T.);
#12545=ORIENTED_EDGE('',*,*,#9367,.F.);
#12546=ORIENTED_EDGE('',*,*,#9368,.F.);
#12547=ORIENTED_EDGE('',*,*,#9357,.F.);
#12548=ORIENTED_EDGE('',*,*,#9368,.T.);
#12549=ORIENTED_EDGE('',*,*,#9369,.F.);
#12550=ORIENTED_EDGE('',*,*,#9370,.F.);
#12551=ORIENTED_EDGE('',*,*,#9358,.F.);
#12552=ORIENTED_EDGE('',*,*,#9370,.T.);
#12553=ORIENTED_EDGE('',*,*,#9371,.F.);
#12554=ORIENTED_EDGE('',*,*,#9372,.T.);
#12555=ORIENTED_EDGE('',*,*,#9279,.F.);
#12556=ORIENTED_EDGE('',*,*,#9372,.F.);
#12557=ORIENTED_EDGE('',*,*,#9373,.F.);
#12558=ORIENTED_EDGE('',*,*,#9374,.F.);
#12559=ORIENTED_EDGE('',*,*,#9280,.F.);
#12560=ORIENTED_EDGE('',*,*,#9374,.T.);
#12561=ORIENTED_EDGE('',*,*,#9375,.F.);
#12562=ORIENTED_EDGE('',*,*,#9376,.F.);
#12563=ORIENTED_EDGE('',*,*,#9281,.F.);
#12564=ORIENTED_EDGE('',*,*,#9376,.T.);
#12565=ORIENTED_EDGE('',*,*,#9377,.F.);
#12566=ORIENTED_EDGE('',*,*,#9378,.F.);
#12567=ORIENTED_EDGE('',*,*,#9282,.F.);
#12568=ORIENTED_EDGE('',*,*,#9378,.T.);
#12569=ORIENTED_EDGE('',*,*,#9379,.F.);
#12570=ORIENTED_EDGE('',*,*,#9380,.T.);
#12571=ORIENTED_EDGE('',*,*,#9283,.F.);
#12572=ORIENTED_EDGE('',*,*,#9380,.F.);
#12573=ORIENTED_EDGE('',*,*,#9381,.F.);
#12574=ORIENTED_EDGE('',*,*,#9382,.F.);
#12575=ORIENTED_EDGE('',*,*,#9284,.F.);
#12576=ORIENTED_EDGE('',*,*,#9382,.T.);
#12577=ORIENTED_EDGE('',*,*,#9383,.F.);
#12578=ORIENTED_EDGE('',*,*,#9384,.F.);
#12579=ORIENTED_EDGE('',*,*,#9285,.F.);
#12580=ORIENTED_EDGE('',*,*,#9384,.T.);
#12581=ORIENTED_EDGE('',*,*,#9385,.F.);
#12582=ORIENTED_EDGE('',*,*,#9386,.F.);
#12583=ORIENTED_EDGE('',*,*,#9286,.F.);
#12584=ORIENTED_EDGE('',*,*,#9386,.T.);
#12585=ORIENTED_EDGE('',*,*,#9387,.F.);
#12586=ORIENTED_EDGE('',*,*,#9388,.T.);
#12587=ORIENTED_EDGE('',*,*,#9287,.F.);
#12588=ORIENTED_EDGE('',*,*,#9388,.F.);
#12589=ORIENTED_EDGE('',*,*,#9389,.F.);
#12590=ORIENTED_EDGE('',*,*,#9390,.F.);
#12591=ORIENTED_EDGE('',*,*,#9288,.F.);
#12592=ORIENTED_EDGE('',*,*,#9390,.T.);
#12593=ORIENTED_EDGE('',*,*,#9391,.F.);
#12594=ORIENTED_EDGE('',*,*,#9392,.F.);
#12595=ORIENTED_EDGE('',*,*,#9289,.F.);
#12596=ORIENTED_EDGE('',*,*,#9392,.T.);
#12597=ORIENTED_EDGE('',*,*,#9393,.F.);
#12598=ORIENTED_EDGE('',*,*,#9394,.F.);
#12599=ORIENTED_EDGE('',*,*,#9290,.F.);
#12600=ORIENTED_EDGE('',*,*,#9394,.T.);
#12601=ORIENTED_EDGE('',*,*,#9395,.F.);
#12602=ORIENTED_EDGE('',*,*,#9396,.T.);
#12603=ORIENTED_EDGE('',*,*,#9291,.F.);
#12604=ORIENTED_EDGE('',*,*,#9396,.F.);
#12605=ORIENTED_EDGE('',*,*,#9397,.F.);
#12606=ORIENTED_EDGE('',*,*,#9398,.F.);
#12607=ORIENTED_EDGE('',*,*,#9292,.F.);
#12608=ORIENTED_EDGE('',*,*,#9398,.T.);
#12609=ORIENTED_EDGE('',*,*,#9399,.F.);
#12610=ORIENTED_EDGE('',*,*,#9400,.F.);
#12611=ORIENTED_EDGE('',*,*,#9293,.F.);
#12612=ORIENTED_EDGE('',*,*,#9400,.T.);
#12613=ORIENTED_EDGE('',*,*,#9401,.F.);
#12614=ORIENTED_EDGE('',*,*,#9402,.F.);
#12615=ORIENTED_EDGE('',*,*,#9294,.F.);
#12616=ORIENTED_EDGE('',*,*,#9402,.T.);
#12617=ORIENTED_EDGE('',*,*,#9403,.F.);
#12618=ORIENTED_EDGE('',*,*,#9404,.T.);
#12619=ORIENTED_EDGE('',*,*,#9295,.F.);
#12620=ORIENTED_EDGE('',*,*,#9404,.F.);
#12621=ORIENTED_EDGE('',*,*,#9405,.F.);
#12622=ORIENTED_EDGE('',*,*,#9406,.F.);
#12623=ORIENTED_EDGE('',*,*,#9296,.F.);
#12624=ORIENTED_EDGE('',*,*,#9406,.T.);
#12625=ORIENTED_EDGE('',*,*,#9407,.F.);
#12626=ORIENTED_EDGE('',*,*,#9408,.F.);
#12627=ORIENTED_EDGE('',*,*,#9297,.F.);
#12628=ORIENTED_EDGE('',*,*,#9408,.T.);
#12629=ORIENTED_EDGE('',*,*,#9409,.F.);
#12630=ORIENTED_EDGE('',*,*,#9410,.F.);
#12631=ORIENTED_EDGE('',*,*,#9298,.F.);
#12632=ORIENTED_EDGE('',*,*,#9410,.T.);
#12633=ORIENTED_EDGE('',*,*,#9411,.F.);
#12634=ORIENTED_EDGE('',*,*,#9412,.T.);
#12635=ORIENTED_EDGE('',*,*,#9299,.F.);
#12636=ORIENTED_EDGE('',*,*,#9412,.F.);
#12637=ORIENTED_EDGE('',*,*,#9413,.F.);
#12638=ORIENTED_EDGE('',*,*,#9414,.F.);
#12639=ORIENTED_EDGE('',*,*,#9300,.F.);
#12640=ORIENTED_EDGE('',*,*,#9414,.T.);
#12641=ORIENTED_EDGE('',*,*,#9415,.F.);
#12642=ORIENTED_EDGE('',*,*,#9416,.F.);
#12643=ORIENTED_EDGE('',*,*,#9301,.F.);
#12644=ORIENTED_EDGE('',*,*,#9416,.T.);
#12645=ORIENTED_EDGE('',*,*,#9417,.F.);
#12646=ORIENTED_EDGE('',*,*,#9418,.F.);
#12647=ORIENTED_EDGE('',*,*,#9302,.F.);
#12648=ORIENTED_EDGE('',*,*,#9418,.T.);
#12649=ORIENTED_EDGE('',*,*,#9419,.F.);
#12650=ORIENTED_EDGE('',*,*,#9420,.T.);
#12651=ORIENTED_EDGE('',*,*,#9303,.F.);
#12652=ORIENTED_EDGE('',*,*,#9420,.F.);
#12653=ORIENTED_EDGE('',*,*,#9421,.F.);
#12654=ORIENTED_EDGE('',*,*,#9422,.F.);
#12655=ORIENTED_EDGE('',*,*,#9304,.F.);
#12656=ORIENTED_EDGE('',*,*,#9422,.T.);
#12657=ORIENTED_EDGE('',*,*,#9423,.F.);
#12658=ORIENTED_EDGE('',*,*,#9424,.F.);
#12659=ORIENTED_EDGE('',*,*,#9305,.F.);
#12660=ORIENTED_EDGE('',*,*,#9424,.T.);
#12661=ORIENTED_EDGE('',*,*,#9425,.F.);
#12662=ORIENTED_EDGE('',*,*,#9426,.F.);
#12663=ORIENTED_EDGE('',*,*,#9306,.F.);
#12664=ORIENTED_EDGE('',*,*,#9426,.T.);
#12665=ORIENTED_EDGE('',*,*,#9427,.F.);
#12666=ORIENTED_EDGE('',*,*,#9428,.T.);
#12667=ORIENTED_EDGE('',*,*,#9307,.F.);
#12668=ORIENTED_EDGE('',*,*,#9428,.F.);
#12669=ORIENTED_EDGE('',*,*,#9429,.F.);
#12670=ORIENTED_EDGE('',*,*,#9430,.F.);
#12671=ORIENTED_EDGE('',*,*,#9308,.F.);
#12672=ORIENTED_EDGE('',*,*,#9430,.T.);
#12673=ORIENTED_EDGE('',*,*,#9431,.F.);
#12674=ORIENTED_EDGE('',*,*,#9432,.F.);
#12675=ORIENTED_EDGE('',*,*,#9309,.F.);
#12676=ORIENTED_EDGE('',*,*,#9432,.T.);
#12677=ORIENTED_EDGE('',*,*,#9433,.F.);
#12678=ORIENTED_EDGE('',*,*,#9434,.F.);
#12679=ORIENTED_EDGE('',*,*,#9310,.F.);
#12680=ORIENTED_EDGE('',*,*,#9434,.T.);
#12681=ORIENTED_EDGE('',*,*,#9435,.F.);
#12682=ORIENTED_EDGE('',*,*,#9436,.T.);
#12683=ORIENTED_EDGE('',*,*,#9311,.F.);
#12684=ORIENTED_EDGE('',*,*,#9436,.F.);
#12685=ORIENTED_EDGE('',*,*,#9437,.F.);
#12686=ORIENTED_EDGE('',*,*,#9438,.F.);
#12687=ORIENTED_EDGE('',*,*,#9312,.F.);
#12688=ORIENTED_EDGE('',*,*,#9438,.T.);
#12689=ORIENTED_EDGE('',*,*,#9439,.F.);
#12690=ORIENTED_EDGE('',*,*,#9440,.F.);
#12691=ORIENTED_EDGE('',*,*,#9313,.F.);
#12692=ORIENTED_EDGE('',*,*,#9440,.T.);
#12693=ORIENTED_EDGE('',*,*,#9441,.F.);
#12694=ORIENTED_EDGE('',*,*,#9442,.F.);
#12695=ORIENTED_EDGE('',*,*,#9314,.F.);
#12696=ORIENTED_EDGE('',*,*,#9442,.T.);
#12697=ORIENTED_EDGE('',*,*,#9443,.F.);
#12698=ORIENTED_EDGE('',*,*,#9444,.T.);
#12699=ORIENTED_EDGE('',*,*,#9315,.F.);
#12700=ORIENTED_EDGE('',*,*,#9444,.F.);
#12701=ORIENTED_EDGE('',*,*,#9445,.F.);
#12702=ORIENTED_EDGE('',*,*,#9446,.F.);
#12703=ORIENTED_EDGE('',*,*,#9316,.F.);
#12704=ORIENTED_EDGE('',*,*,#9446,.T.);
#12705=ORIENTED_EDGE('',*,*,#9447,.F.);
#12706=ORIENTED_EDGE('',*,*,#9448,.F.);
#12707=ORIENTED_EDGE('',*,*,#9317,.F.);
#12708=ORIENTED_EDGE('',*,*,#9448,.T.);
#12709=ORIENTED_EDGE('',*,*,#9449,.F.);
#12710=ORIENTED_EDGE('',*,*,#9450,.F.);
#12711=ORIENTED_EDGE('',*,*,#9318,.F.);
#12712=ORIENTED_EDGE('',*,*,#9450,.T.);
#12713=ORIENTED_EDGE('',*,*,#9451,.F.);
#12714=ORIENTED_EDGE('',*,*,#9452,.T.);
#12715=ORIENTED_EDGE('',*,*,#9319,.F.);
#12716=ORIENTED_EDGE('',*,*,#9452,.F.);
#12717=ORIENTED_EDGE('',*,*,#9453,.F.);
#12718=ORIENTED_EDGE('',*,*,#9454,.F.);
#12719=ORIENTED_EDGE('',*,*,#9320,.F.);
#12720=ORIENTED_EDGE('',*,*,#9454,.T.);
#12721=ORIENTED_EDGE('',*,*,#9455,.F.);
#12722=ORIENTED_EDGE('',*,*,#9456,.F.);
#12723=ORIENTED_EDGE('',*,*,#9321,.F.);
#12724=ORIENTED_EDGE('',*,*,#9456,.T.);
#12725=ORIENTED_EDGE('',*,*,#9457,.F.);
#12726=ORIENTED_EDGE('',*,*,#9458,.F.);
#12727=ORIENTED_EDGE('',*,*,#9322,.F.);
#12728=ORIENTED_EDGE('',*,*,#9458,.T.);
#12729=ORIENTED_EDGE('',*,*,#9459,.F.);
#12730=ORIENTED_EDGE('',*,*,#9460,.T.);
#12731=ORIENTED_EDGE('',*,*,#9323,.F.);
#12732=ORIENTED_EDGE('',*,*,#9460,.F.);
#12733=ORIENTED_EDGE('',*,*,#9461,.F.);
#12734=ORIENTED_EDGE('',*,*,#9462,.F.);
#12735=ORIENTED_EDGE('',*,*,#9324,.F.);
#12736=ORIENTED_EDGE('',*,*,#9462,.T.);
#12737=ORIENTED_EDGE('',*,*,#9463,.F.);
#12738=ORIENTED_EDGE('',*,*,#9464,.F.);
#12739=ORIENTED_EDGE('',*,*,#9325,.F.);
#12740=ORIENTED_EDGE('',*,*,#9464,.T.);
#12741=ORIENTED_EDGE('',*,*,#9465,.F.);
#12742=ORIENTED_EDGE('',*,*,#9466,.F.);
#12743=ORIENTED_EDGE('',*,*,#9326,.F.);
#12744=ORIENTED_EDGE('',*,*,#9466,.T.);
#12745=ORIENTED_EDGE('',*,*,#9467,.F.);
#12746=ORIENTED_EDGE('',*,*,#9468,.T.);
#12747=ORIENTED_EDGE('',*,*,#9327,.F.);
#12748=ORIENTED_EDGE('',*,*,#9468,.F.);
#12749=ORIENTED_EDGE('',*,*,#9469,.F.);
#12750=ORIENTED_EDGE('',*,*,#9470,.F.);
#12751=ORIENTED_EDGE('',*,*,#9328,.F.);
#12752=ORIENTED_EDGE('',*,*,#9470,.T.);
#12753=ORIENTED_EDGE('',*,*,#9471,.F.);
#12754=ORIENTED_EDGE('',*,*,#9472,.F.);
#12755=ORIENTED_EDGE('',*,*,#9329,.F.);
#12756=ORIENTED_EDGE('',*,*,#9472,.T.);
#12757=ORIENTED_EDGE('',*,*,#9473,.F.);
#12758=ORIENTED_EDGE('',*,*,#9474,.F.);
#12759=ORIENTED_EDGE('',*,*,#9330,.F.);
#12760=ORIENTED_EDGE('',*,*,#9474,.T.);
#12761=ORIENTED_EDGE('',*,*,#9475,.F.);
#12762=ORIENTED_EDGE('',*,*,#9476,.T.);
#12763=ORIENTED_EDGE('',*,*,#9331,.F.);
#12764=ORIENTED_EDGE('',*,*,#9476,.F.);
#12765=ORIENTED_EDGE('',*,*,#9477,.F.);
#12766=ORIENTED_EDGE('',*,*,#9478,.F.);
#12767=ORIENTED_EDGE('',*,*,#9332,.F.);
#12768=ORIENTED_EDGE('',*,*,#9478,.T.);
#12769=ORIENTED_EDGE('',*,*,#9479,.F.);
#12770=ORIENTED_EDGE('',*,*,#9480,.F.);
#12771=ORIENTED_EDGE('',*,*,#9333,.F.);
#12772=ORIENTED_EDGE('',*,*,#9480,.T.);
#12773=ORIENTED_EDGE('',*,*,#9481,.F.);
#12774=ORIENTED_EDGE('',*,*,#9482,.F.);
#12775=ORIENTED_EDGE('',*,*,#9334,.F.);
#12776=ORIENTED_EDGE('',*,*,#9482,.T.);
#12777=ORIENTED_EDGE('',*,*,#9483,.F.);
#12778=ORIENTED_EDGE('',*,*,#9484,.T.);
#12779=ORIENTED_EDGE('',*,*,#9335,.F.);
#12780=ORIENTED_EDGE('',*,*,#9484,.F.);
#12781=ORIENTED_EDGE('',*,*,#9485,.F.);
#12782=ORIENTED_EDGE('',*,*,#9486,.F.);
#12783=ORIENTED_EDGE('',*,*,#9336,.F.);
#12784=ORIENTED_EDGE('',*,*,#9486,.T.);
#12785=ORIENTED_EDGE('',*,*,#9487,.F.);
#12786=ORIENTED_EDGE('',*,*,#9488,.F.);
#12787=ORIENTED_EDGE('',*,*,#9337,.F.);
#12788=ORIENTED_EDGE('',*,*,#9488,.T.);
#12789=ORIENTED_EDGE('',*,*,#9489,.F.);
#12790=ORIENTED_EDGE('',*,*,#9490,.F.);
#12791=ORIENTED_EDGE('',*,*,#9338,.F.);
#12792=ORIENTED_EDGE('',*,*,#9490,.T.);
#12793=ORIENTED_EDGE('',*,*,#9491,.F.);
#12794=ORIENTED_EDGE('',*,*,#9492,.T.);
#12795=ORIENTED_EDGE('',*,*,#9339,.F.);
#12796=ORIENTED_EDGE('',*,*,#9492,.F.);
#12797=ORIENTED_EDGE('',*,*,#9493,.F.);
#12798=ORIENTED_EDGE('',*,*,#9494,.F.);
#12799=ORIENTED_EDGE('',*,*,#9340,.F.);
#12800=ORIENTED_EDGE('',*,*,#9494,.T.);
#12801=ORIENTED_EDGE('',*,*,#9495,.F.);
#12802=ORIENTED_EDGE('',*,*,#9496,.F.);
#12803=ORIENTED_EDGE('',*,*,#9341,.F.);
#12804=ORIENTED_EDGE('',*,*,#9496,.T.);
#12805=ORIENTED_EDGE('',*,*,#9497,.F.);
#12806=ORIENTED_EDGE('',*,*,#9498,.F.);
#12807=ORIENTED_EDGE('',*,*,#9342,.F.);
#12808=ORIENTED_EDGE('',*,*,#9498,.T.);
#12809=ORIENTED_EDGE('',*,*,#9499,.F.);
#12810=ORIENTED_EDGE('',*,*,#9500,.T.);
#12811=ORIENTED_EDGE('',*,*,#9343,.F.);
#12812=ORIENTED_EDGE('',*,*,#9500,.F.);
#12813=ORIENTED_EDGE('',*,*,#9501,.F.);
#12814=ORIENTED_EDGE('',*,*,#9502,.F.);
#12815=ORIENTED_EDGE('',*,*,#9344,.F.);
#12816=ORIENTED_EDGE('',*,*,#9502,.T.);
#12817=ORIENTED_EDGE('',*,*,#9503,.F.);
#12818=ORIENTED_EDGE('',*,*,#9504,.F.);
#12819=ORIENTED_EDGE('',*,*,#9345,.F.);
#12820=ORIENTED_EDGE('',*,*,#9504,.T.);
#12821=ORIENTED_EDGE('',*,*,#9505,.F.);
#12822=ORIENTED_EDGE('',*,*,#9506,.F.);
#12823=ORIENTED_EDGE('',*,*,#9346,.F.);
#12824=ORIENTED_EDGE('',*,*,#9506,.T.);
#12825=ORIENTED_EDGE('',*,*,#9507,.F.);
#12826=ORIENTED_EDGE('',*,*,#9508,.T.);
#12827=ORIENTED_EDGE('',*,*,#9347,.F.);
#12828=ORIENTED_EDGE('',*,*,#9508,.F.);
#12829=ORIENTED_EDGE('',*,*,#9509,.F.);
#12830=ORIENTED_EDGE('',*,*,#9510,.F.);
#12831=ORIENTED_EDGE('',*,*,#9348,.F.);
#12832=ORIENTED_EDGE('',*,*,#9510,.T.);
#12833=ORIENTED_EDGE('',*,*,#9511,.F.);
#12834=ORIENTED_EDGE('',*,*,#9512,.F.);
#12835=ORIENTED_EDGE('',*,*,#9349,.F.);
#12836=ORIENTED_EDGE('',*,*,#9512,.T.);
#12837=ORIENTED_EDGE('',*,*,#9513,.F.);
#12838=ORIENTED_EDGE('',*,*,#9514,.F.);
#12839=ORIENTED_EDGE('',*,*,#9350,.F.);
#12840=ORIENTED_EDGE('',*,*,#9514,.T.);
#12841=ORIENTED_EDGE('',*,*,#9515,.F.);
#12842=ORIENTED_EDGE('',*,*,#9516,.T.);
#12843=ORIENTED_EDGE('',*,*,#9351,.F.);
#12844=ORIENTED_EDGE('',*,*,#9516,.F.);
#12845=ORIENTED_EDGE('',*,*,#9517,.F.);
#12846=ORIENTED_EDGE('',*,*,#9518,.F.);
#12847=ORIENTED_EDGE('',*,*,#9352,.F.);
#12848=ORIENTED_EDGE('',*,*,#9518,.T.);
#12849=ORIENTED_EDGE('',*,*,#9519,.F.);
#12850=ORIENTED_EDGE('',*,*,#9520,.F.);
#12851=ORIENTED_EDGE('',*,*,#9353,.F.);
#12852=ORIENTED_EDGE('',*,*,#9520,.T.);
#12853=ORIENTED_EDGE('',*,*,#9521,.F.);
#12854=ORIENTED_EDGE('',*,*,#9522,.F.);
#12855=ORIENTED_EDGE('',*,*,#9354,.F.);
#12856=ORIENTED_EDGE('',*,*,#9523,.T.);
#12857=ORIENTED_EDGE('',*,*,#9521,.T.);
#12858=ORIENTED_EDGE('',*,*,#9519,.T.);
#12859=ORIENTED_EDGE('',*,*,#9517,.T.);
#12860=ORIENTED_EDGE('',*,*,#9515,.T.);
#12861=ORIENTED_EDGE('',*,*,#9513,.T.);
#12862=ORIENTED_EDGE('',*,*,#9511,.T.);
#12863=ORIENTED_EDGE('',*,*,#9509,.T.);
#12864=ORIENTED_EDGE('',*,*,#9507,.T.);
#12865=ORIENTED_EDGE('',*,*,#9505,.T.);
#12866=ORIENTED_EDGE('',*,*,#9503,.T.);
#12867=ORIENTED_EDGE('',*,*,#9501,.T.);
#12868=ORIENTED_EDGE('',*,*,#9499,.T.);
#12869=ORIENTED_EDGE('',*,*,#9497,.T.);
#12870=ORIENTED_EDGE('',*,*,#9495,.T.);
#12871=ORIENTED_EDGE('',*,*,#9493,.T.);
#12872=ORIENTED_EDGE('',*,*,#9491,.T.);
#12873=ORIENTED_EDGE('',*,*,#9489,.T.);
#12874=ORIENTED_EDGE('',*,*,#9487,.T.);
#12875=ORIENTED_EDGE('',*,*,#9485,.T.);
#12876=ORIENTED_EDGE('',*,*,#9483,.T.);
#12877=ORIENTED_EDGE('',*,*,#9481,.T.);
#12878=ORIENTED_EDGE('',*,*,#9479,.T.);
#12879=ORIENTED_EDGE('',*,*,#9477,.T.);
#12880=ORIENTED_EDGE('',*,*,#9475,.T.);
#12881=ORIENTED_EDGE('',*,*,#9473,.T.);
#12882=ORIENTED_EDGE('',*,*,#9471,.T.);
#12883=ORIENTED_EDGE('',*,*,#9469,.T.);
#12884=ORIENTED_EDGE('',*,*,#9467,.T.);
#12885=ORIENTED_EDGE('',*,*,#9465,.T.);
#12886=ORIENTED_EDGE('',*,*,#9463,.T.);
#12887=ORIENTED_EDGE('',*,*,#9461,.T.);
#12888=ORIENTED_EDGE('',*,*,#9459,.T.);
#12889=ORIENTED_EDGE('',*,*,#9457,.T.);
#12890=ORIENTED_EDGE('',*,*,#9455,.T.);
#12891=ORIENTED_EDGE('',*,*,#9453,.T.);
#12892=ORIENTED_EDGE('',*,*,#9451,.T.);
#12893=ORIENTED_EDGE('',*,*,#9449,.T.);
#12894=ORIENTED_EDGE('',*,*,#9447,.T.);
#12895=ORIENTED_EDGE('',*,*,#9445,.T.);
#12896=ORIENTED_EDGE('',*,*,#9443,.T.);
#12897=ORIENTED_EDGE('',*,*,#9441,.T.);
#12898=ORIENTED_EDGE('',*,*,#9439,.T.);
#12899=ORIENTED_EDGE('',*,*,#9437,.T.);
#12900=ORIENTED_EDGE('',*,*,#9435,.T.);
#12901=ORIENTED_EDGE('',*,*,#9433,.T.);
#12902=ORIENTED_EDGE('',*,*,#9431,.T.);
#12903=ORIENTED_EDGE('',*,*,#9429,.T.);
#12904=ORIENTED_EDGE('',*,*,#9427,.T.);
#12905=ORIENTED_EDGE('',*,*,#9425,.T.);
#12906=ORIENTED_EDGE('',*,*,#9423,.T.);
#12907=ORIENTED_EDGE('',*,*,#9421,.T.);
#12908=ORIENTED_EDGE('',*,*,#9419,.T.);
#12909=ORIENTED_EDGE('',*,*,#9417,.T.);
#12910=ORIENTED_EDGE('',*,*,#9415,.T.);
#12911=ORIENTED_EDGE('',*,*,#9413,.T.);
#12912=ORIENTED_EDGE('',*,*,#9411,.T.);
#12913=ORIENTED_EDGE('',*,*,#9409,.T.);
#12914=ORIENTED_EDGE('',*,*,#9407,.T.);
#12915=ORIENTED_EDGE('',*,*,#9405,.T.);
#12916=ORIENTED_EDGE('',*,*,#9403,.T.);
#12917=ORIENTED_EDGE('',*,*,#9401,.T.);
#12918=ORIENTED_EDGE('',*,*,#9399,.T.);
#12919=ORIENTED_EDGE('',*,*,#9397,.T.);
#12920=ORIENTED_EDGE('',*,*,#9395,.T.);
#12921=ORIENTED_EDGE('',*,*,#9393,.T.);
#12922=ORIENTED_EDGE('',*,*,#9391,.T.);
#12923=ORIENTED_EDGE('',*,*,#9389,.T.);
#12924=ORIENTED_EDGE('',*,*,#9387,.T.);
#12925=ORIENTED_EDGE('',*,*,#9385,.T.);
#12926=ORIENTED_EDGE('',*,*,#9383,.T.);
#12927=ORIENTED_EDGE('',*,*,#9381,.T.);
#12928=ORIENTED_EDGE('',*,*,#9379,.T.);
#12929=ORIENTED_EDGE('',*,*,#9377,.T.);
#12930=ORIENTED_EDGE('',*,*,#9375,.T.);
#12931=ORIENTED_EDGE('',*,*,#9373,.T.);
#12932=ORIENTED_EDGE('',*,*,#9371,.T.);
#12933=ORIENTED_EDGE('',*,*,#9369,.T.);
#12934=ORIENTED_EDGE('',*,*,#9367,.T.);
#12935=ORIENTED_EDGE('',*,*,#9365,.T.);
#12936=ORIENTED_EDGE('',*,*,#9363,.T.);
#12937=ORIENTED_EDGE('',*,*,#9364,.T.);
#12938=ORIENTED_EDGE('',*,*,#9355,.F.);
#12939=ORIENTED_EDGE('',*,*,#9522,.T.);
#12940=ORIENTED_EDGE('',*,*,#9523,.F.);
#12941=ORIENTED_EDGE('',*,*,#9524,.F.);
#12942=ORIENTED_EDGE('',*,*,#9525,.F.);
#12943=ORIENTED_EDGE('',*,*,#9526,.F.);
#12944=ORIENTED_EDGE('',*,*,#9527,.F.);
#12945=ORIENTED_EDGE('',*,*,#9528,.F.);
#12946=ORIENTED_EDGE('',*,*,#9529,.F.);
#12947=ORIENTED_EDGE('',*,*,#9530,.F.);
#12948=ORIENTED_EDGE('',*,*,#9531,.F.);
#12949=ORIENTED_EDGE('',*,*,#9528,.T.);
#12950=ORIENTED_EDGE('',*,*,#9532,.T.);
#12951=ORIENTED_EDGE('',*,*,#9533,.T.);
#12952=ORIENTED_EDGE('',*,*,#9534,.T.);
#12953=ORIENTED_EDGE('',*,*,#9527,.T.);
#12954=ORIENTED_EDGE('',*,*,#9535,.F.);
#12955=ORIENTED_EDGE('',*,*,#9536,.T.);
#12956=ORIENTED_EDGE('',*,*,#9532,.F.);
#12957=ORIENTED_EDGE('',*,*,#9526,.T.);
#12958=ORIENTED_EDGE('',*,*,#9537,.T.);
#12959=ORIENTED_EDGE('',*,*,#9538,.T.);
#12960=ORIENTED_EDGE('',*,*,#9535,.T.);
#12961=ORIENTED_EDGE('',*,*,#9525,.T.);
#12962=ORIENTED_EDGE('',*,*,#9539,.F.);
#12963=ORIENTED_EDGE('',*,*,#9540,.T.);
#12964=ORIENTED_EDGE('',*,*,#9537,.F.);
#12965=ORIENTED_EDGE('',*,*,#9533,.F.);
#12966=ORIENTED_EDGE('',*,*,#9536,.F.);
#12967=ORIENTED_EDGE('',*,*,#9538,.F.);
#12968=ORIENTED_EDGE('',*,*,#9540,.F.);
#12969=ORIENTED_EDGE('',*,*,#9541,.F.);
#12970=ORIENTED_EDGE('',*,*,#9542,.F.);
#12971=ORIENTED_EDGE('',*,*,#9543,.F.);
#12972=ORIENTED_EDGE('',*,*,#9544,.F.);
#12973=ORIENTED_EDGE('',*,*,#9524,.T.);
#12974=ORIENTED_EDGE('',*,*,#9545,.T.);
#12975=ORIENTED_EDGE('',*,*,#9541,.T.);
#12976=ORIENTED_EDGE('',*,*,#9539,.T.);
#12977=ORIENTED_EDGE('',*,*,#9531,.T.);
#12978=ORIENTED_EDGE('',*,*,#9546,.F.);
#12979=ORIENTED_EDGE('',*,*,#9542,.T.);
#12980=ORIENTED_EDGE('',*,*,#9545,.F.);
#12981=ORIENTED_EDGE('',*,*,#9530,.T.);
#12982=ORIENTED_EDGE('',*,*,#9547,.T.);
#12983=ORIENTED_EDGE('',*,*,#9543,.T.);
#12984=ORIENTED_EDGE('',*,*,#9546,.T.);
#12985=ORIENTED_EDGE('',*,*,#9529,.T.);
#12986=ORIENTED_EDGE('',*,*,#9534,.F.);
#12987=ORIENTED_EDGE('',*,*,#9544,.T.);
#12988=ORIENTED_EDGE('',*,*,#9547,.F.);
#12989=ORIENTED_EDGE('',*,*,#9548,.F.);
#12990=ORIENTED_EDGE('',*,*,#9549,.T.);
#12991=ORIENTED_EDGE('',*,*,#9550,.F.);
#12992=ORIENTED_EDGE('',*,*,#9551,.T.);
#12993=ORIENTED_EDGE('',*,*,#9552,.F.);
#12994=ORIENTED_EDGE('',*,*,#9551,.F.);
#12995=ORIENTED_EDGE('',*,*,#9553,.F.);
#12996=ORIENTED_EDGE('',*,*,#9554,.F.);
#12997=ORIENTED_EDGE('',*,*,#9555,.F.);
#12998=ORIENTED_EDGE('',*,*,#9554,.T.);
#12999=ORIENTED_EDGE('',*,*,#9556,.T.);
#13000=ORIENTED_EDGE('',*,*,#9557,.T.);
#13001=ORIENTED_EDGE('',*,*,#9553,.T.);
#13002=ORIENTED_EDGE('',*,*,#9550,.T.);
#13003=ORIENTED_EDGE('',*,*,#9558,.T.);
#13004=ORIENTED_EDGE('',*,*,#9556,.F.);
#13005=ORIENTED_EDGE('',*,*,#9559,.F.);
#13006=ORIENTED_EDGE('',*,*,#9557,.F.);
#13007=ORIENTED_EDGE('',*,*,#9558,.F.);
#13008=ORIENTED_EDGE('',*,*,#9549,.F.);
#13009=ORIENTED_EDGE('',*,*,#9560,.F.);
#13010=ORIENTED_EDGE('',*,*,#9561,.T.);
#13011=ORIENTED_EDGE('',*,*,#9562,.F.);
#13012=ORIENTED_EDGE('',*,*,#9563,.T.);
#13013=ORIENTED_EDGE('',*,*,#9564,.F.);
#13014=ORIENTED_EDGE('',*,*,#9563,.F.);
#13015=ORIENTED_EDGE('',*,*,#9565,.F.);
#13016=ORIENTED_EDGE('',*,*,#9566,.F.);
#13017=ORIENTED_EDGE('',*,*,#9567,.F.);
#13018=ORIENTED_EDGE('',*,*,#9566,.T.);
#13019=ORIENTED_EDGE('',*,*,#9568,.T.);
#13020=ORIENTED_EDGE('',*,*,#9569,.T.);
#13021=ORIENTED_EDGE('',*,*,#9565,.T.);
#13022=ORIENTED_EDGE('',*,*,#9562,.T.);
#13023=ORIENTED_EDGE('',*,*,#9570,.T.);
#13024=ORIENTED_EDGE('',*,*,#9568,.F.);
#13025=ORIENTED_EDGE('',*,*,#9571,.F.);
#13026=ORIENTED_EDGE('',*,*,#9569,.F.);
#13027=ORIENTED_EDGE('',*,*,#9570,.F.);
#13028=ORIENTED_EDGE('',*,*,#9561,.F.);
#13029=ORIENTED_EDGE('',*,*,#9572,.F.);
#13030=ORIENTED_EDGE('',*,*,#9573,.T.);
#13031=ORIENTED_EDGE('',*,*,#9574,.T.);
#13032=ORIENTED_EDGE('',*,*,#9573,.F.);
#13033=ORIENTED_EDGE('',*,*,#9555,.T.);
#13034=ORIENTED_EDGE('',*,*,#9559,.T.);
#13035=ORIENTED_EDGE('',*,*,#9548,.T.);
#13036=ORIENTED_EDGE('',*,*,#9552,.T.);
#13037=ORIENTED_EDGE('',*,*,#9567,.T.);
#13038=ORIENTED_EDGE('',*,*,#9571,.T.);
#13039=ORIENTED_EDGE('',*,*,#9560,.T.);
#13040=ORIENTED_EDGE('',*,*,#9564,.T.);
#13041=ORIENTED_EDGE('',*,*,#9572,.T.);
#13042=ORIENTED_EDGE('',*,*,#9574,.F.);
#13043=ORIENTED_EDGE('',*,*,#9575,.F.);
#13044=ORIENTED_EDGE('',*,*,#9576,.T.);
#13045=ORIENTED_EDGE('',*,*,#9577,.F.);
#13046=ORIENTED_EDGE('',*,*,#9578,.F.);
#13047=ORIENTED_EDGE('',*,*,#9579,.T.);
#13048=ORIENTED_EDGE('',*,*,#9580,.F.);
#13049=ORIENTED_EDGE('',*,*,#9581,.F.);
#13050=ORIENTED_EDGE('',*,*,#9579,.F.);
#13051=ORIENTED_EDGE('',*,*,#9582,.F.);
#13052=ORIENTED_EDGE('',*,*,#9583,.F.);
#13053=ORIENTED_EDGE('',*,*,#9576,.F.);
#13054=ORIENTED_EDGE('',*,*,#9584,.F.);
#13055=ORIENTED_EDGE('',*,*,#9582,.T.);
#13056=ORIENTED_EDGE('',*,*,#9578,.T.);
#13057=ORIENTED_EDGE('',*,*,#9585,.F.);
#13058=ORIENTED_EDGE('',*,*,#9586,.T.);
#13059=ORIENTED_EDGE('',*,*,#9587,.T.);
#13060=ORIENTED_EDGE('',*,*,#9586,.F.);
#13061=ORIENTED_EDGE('',*,*,#9583,.T.);
#13062=ORIENTED_EDGE('',*,*,#9584,.T.);
#13063=ORIENTED_EDGE('',*,*,#9577,.T.);
#13064=ORIENTED_EDGE('',*,*,#9575,.T.);
#13065=ORIENTED_EDGE('',*,*,#9588,.F.);
#13066=ORIENTED_EDGE('',*,*,#9589,.T.);
#13067=ORIENTED_EDGE('',*,*,#9590,.T.);
#13068=ORIENTED_EDGE('',*,*,#9589,.F.);
#13069=ORIENTED_EDGE('',*,*,#9580,.T.);
#13070=ORIENTED_EDGE('',*,*,#9581,.T.);
#13071=ORIENTED_EDGE('',*,*,#9588,.T.);
#13072=ORIENTED_EDGE('',*,*,#9585,.T.);
#13073=ORIENTED_EDGE('',*,*,#9590,.F.);
#13074=ORIENTED_EDGE('',*,*,#9587,.F.);
#13075=ORIENTED_EDGE('',*,*,#9591,.F.);
#13076=ORIENTED_EDGE('',*,*,#9592,.T.);
#13077=ORIENTED_EDGE('',*,*,#9593,.F.);
#13078=ORIENTED_EDGE('',*,*,#9594,.F.);
#13079=ORIENTED_EDGE('',*,*,#9595,.T.);
#13080=ORIENTED_EDGE('',*,*,#9596,.F.);
#13081=ORIENTED_EDGE('',*,*,#9597,.F.);
#13082=ORIENTED_EDGE('',*,*,#9595,.F.);
#13083=ORIENTED_EDGE('',*,*,#9598,.F.);
#13084=ORIENTED_EDGE('',*,*,#9599,.F.);
#13085=ORIENTED_EDGE('',*,*,#9592,.F.);
#13086=ORIENTED_EDGE('',*,*,#9600,.F.);
#13087=ORIENTED_EDGE('',*,*,#9598,.T.);
#13088=ORIENTED_EDGE('',*,*,#9594,.T.);
#13089=ORIENTED_EDGE('',*,*,#9601,.F.);
#13090=ORIENTED_EDGE('',*,*,#9602,.T.);
#13091=ORIENTED_EDGE('',*,*,#9603,.T.);
#13092=ORIENTED_EDGE('',*,*,#9602,.F.);
#13093=ORIENTED_EDGE('',*,*,#9599,.T.);
#13094=ORIENTED_EDGE('',*,*,#9600,.T.);
#13095=ORIENTED_EDGE('',*,*,#9593,.T.);
#13096=ORIENTED_EDGE('',*,*,#9591,.T.);
#13097=ORIENTED_EDGE('',*,*,#9604,.F.);
#13098=ORIENTED_EDGE('',*,*,#9605,.T.);
#13099=ORIENTED_EDGE('',*,*,#9606,.T.);
#13100=ORIENTED_EDGE('',*,*,#9605,.F.);
#13101=ORIENTED_EDGE('',*,*,#9596,.T.);
#13102=ORIENTED_EDGE('',*,*,#9597,.T.);
#13103=ORIENTED_EDGE('',*,*,#9604,.T.);
#13104=ORIENTED_EDGE('',*,*,#9601,.T.);
#13105=ORIENTED_EDGE('',*,*,#9606,.F.);
#13106=ORIENTED_EDGE('',*,*,#9603,.F.);
#13107=ORIENTED_EDGE('',*,*,#9607,.F.);
#13108=ORIENTED_EDGE('',*,*,#9608,.T.);
#13109=ORIENTED_EDGE('',*,*,#9609,.T.);
#13110=ORIENTED_EDGE('',*,*,#9608,.F.);
#13111=ORIENTED_EDGE('',*,*,#9610,.F.);
#13112=ORIENTED_EDGE('',*,*,#9611,.T.);
#13113=ORIENTED_EDGE('',*,*,#9612,.T.);
#13114=ORIENTED_EDGE('',*,*,#9611,.F.);
#13115=ORIENTED_EDGE('',*,*,#9610,.T.);
#13116=ORIENTED_EDGE('',*,*,#9607,.T.);
#13117=ORIENTED_EDGE('',*,*,#9612,.F.);
#13118=ORIENTED_EDGE('',*,*,#9609,.F.);
#13119=ORIENTED_EDGE('',*,*,#9613,.F.);
#13120=ORIENTED_EDGE('',*,*,#9614,.T.);
#13121=ORIENTED_EDGE('',*,*,#9615,.T.);
#13122=ORIENTED_EDGE('',*,*,#9614,.F.);
#13123=ORIENTED_EDGE('',*,*,#9616,.F.);
#13124=ORIENTED_EDGE('',*,*,#9617,.T.);
#13125=ORIENTED_EDGE('',*,*,#9618,.T.);
#13126=ORIENTED_EDGE('',*,*,#9617,.F.);
#13127=ORIENTED_EDGE('',*,*,#9616,.T.);
#13128=ORIENTED_EDGE('',*,*,#9613,.T.);
#13129=ORIENTED_EDGE('',*,*,#9618,.F.);
#13130=ORIENTED_EDGE('',*,*,#9615,.F.);
#13131=ORIENTED_EDGE('',*,*,#9619,.F.);
#13132=ORIENTED_EDGE('',*,*,#9620,.T.);
#13133=ORIENTED_EDGE('',*,*,#9621,.T.);
#13134=ORIENTED_EDGE('',*,*,#9620,.F.);
#13135=ORIENTED_EDGE('',*,*,#9622,.F.);
#13136=ORIENTED_EDGE('',*,*,#9623,.T.);
#13137=ORIENTED_EDGE('',*,*,#9624,.T.);
#13138=ORIENTED_EDGE('',*,*,#9623,.F.);
#13139=ORIENTED_EDGE('',*,*,#9622,.T.);
#13140=ORIENTED_EDGE('',*,*,#9619,.T.);
#13141=ORIENTED_EDGE('',*,*,#9624,.F.);
#13142=ORIENTED_EDGE('',*,*,#9621,.F.);
#13143=ORIENTED_EDGE('',*,*,#9625,.F.);
#13144=ORIENTED_EDGE('',*,*,#9626,.T.);
#13145=ORIENTED_EDGE('',*,*,#9627,.T.);
#13146=ORIENTED_EDGE('',*,*,#9626,.F.);
#13147=ORIENTED_EDGE('',*,*,#9628,.F.);
#13148=ORIENTED_EDGE('',*,*,#9629,.T.);
#13149=ORIENTED_EDGE('',*,*,#9630,.T.);
#13150=ORIENTED_EDGE('',*,*,#9629,.F.);
#13151=ORIENTED_EDGE('',*,*,#9628,.T.);
#13152=ORIENTED_EDGE('',*,*,#9625,.T.);
#13153=ORIENTED_EDGE('',*,*,#9630,.F.);
#13154=ORIENTED_EDGE('',*,*,#9627,.F.);
#13155=ORIENTED_EDGE('',*,*,#9631,.F.);
#13156=ORIENTED_EDGE('',*,*,#9632,.T.);
#13157=ORIENTED_EDGE('',*,*,#9633,.T.);
#13158=ORIENTED_EDGE('',*,*,#9632,.F.);
#13159=ORIENTED_EDGE('',*,*,#9634,.F.);
#13160=ORIENTED_EDGE('',*,*,#9635,.T.);
#13161=ORIENTED_EDGE('',*,*,#9636,.T.);
#13162=ORIENTED_EDGE('',*,*,#9635,.F.);
#13163=ORIENTED_EDGE('',*,*,#9634,.T.);
#13164=ORIENTED_EDGE('',*,*,#9631,.T.);
#13165=ORIENTED_EDGE('',*,*,#9636,.F.);
#13166=ORIENTED_EDGE('',*,*,#9633,.F.);
#13167=ORIENTED_EDGE('',*,*,#9637,.F.);
#13168=ORIENTED_EDGE('',*,*,#9638,.T.);
#13169=ORIENTED_EDGE('',*,*,#9639,.F.);
#13170=ORIENTED_EDGE('',*,*,#9640,.F.);
#13171=ORIENTED_EDGE('',*,*,#9641,.F.);
#13172=ORIENTED_EDGE('',*,*,#9642,.T.);
#13173=ORIENTED_EDGE('',*,*,#9643,.F.);
#13174=ORIENTED_EDGE('',*,*,#9638,.F.);
#13175=ORIENTED_EDGE('',*,*,#9644,.F.);
#13176=ORIENTED_EDGE('',*,*,#9645,.F.);
#13177=ORIENTED_EDGE('',*,*,#9646,.F.);
#13178=ORIENTED_EDGE('',*,*,#9642,.F.);
#13179=ORIENTED_EDGE('',*,*,#9647,.T.);
#13180=ORIENTED_EDGE('',*,*,#9639,.T.);
#13181=ORIENTED_EDGE('',*,*,#9643,.T.);
#13182=ORIENTED_EDGE('',*,*,#9646,.T.);
#13183=ORIENTED_EDGE('',*,*,#9648,.T.);
#13184=ORIENTED_EDGE('',*,*,#9640,.T.);
#13185=ORIENTED_EDGE('',*,*,#9648,.F.);
#13186=ORIENTED_EDGE('',*,*,#9645,.T.);
#13187=ORIENTED_EDGE('',*,*,#9649,.F.);
#13188=ORIENTED_EDGE('',*,*,#9650,.T.);
#13189=ORIENTED_EDGE('',*,*,#9651,.T.);
#13190=ORIENTED_EDGE('',*,*,#9652,.T.);
#13191=ORIENTED_EDGE('',*,*,#9653,.T.);
#13192=ORIENTED_EDGE('',*,*,#9654,.T.);
#13193=ORIENTED_EDGE('',*,*,#9655,.T.);
#13194=ORIENTED_EDGE('',*,*,#9656,.T.);
#13195=ORIENTED_EDGE('',*,*,#9657,.T.);
#13196=ORIENTED_EDGE('',*,*,#9658,.T.);
#13197=ORIENTED_EDGE('',*,*,#9659,.T.);
#13198=ORIENTED_EDGE('',*,*,#9660,.T.);
#13199=ORIENTED_EDGE('',*,*,#9661,.T.);
#13200=ORIENTED_EDGE('',*,*,#9662,.T.);
#13201=ORIENTED_EDGE('',*,*,#9663,.T.);
#13202=ORIENTED_EDGE('',*,*,#9664,.T.);
#13203=ORIENTED_EDGE('',*,*,#9665,.T.);
#13204=ORIENTED_EDGE('',*,*,#9666,.T.);
#13205=ORIENTED_EDGE('',*,*,#9667,.T.);
#13206=ORIENTED_EDGE('',*,*,#9668,.T.);
#13207=ORIENTED_EDGE('',*,*,#9669,.T.);
#13208=ORIENTED_EDGE('',*,*,#9670,.T.);
#13209=ORIENTED_EDGE('',*,*,#9671,.T.);
#13210=ORIENTED_EDGE('',*,*,#9672,.T.);
#13211=ORIENTED_EDGE('',*,*,#9673,.T.);
#13212=ORIENTED_EDGE('',*,*,#9674,.T.);
#13213=ORIENTED_EDGE('',*,*,#9675,.T.);
#13214=ORIENTED_EDGE('',*,*,#9676,.T.);
#13215=ORIENTED_EDGE('',*,*,#9677,.T.);
#13216=ORIENTED_EDGE('',*,*,#9678,.T.);
#13217=ORIENTED_EDGE('',*,*,#9679,.T.);
#13218=ORIENTED_EDGE('',*,*,#9680,.T.);
#13219=ORIENTED_EDGE('',*,*,#9681,.T.);
#13220=ORIENTED_EDGE('',*,*,#9682,.T.);
#13221=ORIENTED_EDGE('',*,*,#9683,.T.);
#13222=ORIENTED_EDGE('',*,*,#9684,.T.);
#13223=ORIENTED_EDGE('',*,*,#9685,.T.);
#13224=ORIENTED_EDGE('',*,*,#9686,.T.);
#13225=ORIENTED_EDGE('',*,*,#9687,.T.);
#13226=ORIENTED_EDGE('',*,*,#9688,.T.);
#13227=ORIENTED_EDGE('',*,*,#9689,.T.);
#13228=ORIENTED_EDGE('',*,*,#9690,.T.);
#13229=ORIENTED_EDGE('',*,*,#9691,.T.);
#13230=ORIENTED_EDGE('',*,*,#9692,.T.);
#13231=ORIENTED_EDGE('',*,*,#9693,.T.);
#13232=ORIENTED_EDGE('',*,*,#9694,.T.);
#13233=ORIENTED_EDGE('',*,*,#9695,.T.);
#13234=ORIENTED_EDGE('',*,*,#9696,.T.);
#13235=ORIENTED_EDGE('',*,*,#9697,.T.);
#13236=ORIENTED_EDGE('',*,*,#9698,.T.);
#13237=ORIENTED_EDGE('',*,*,#9699,.T.);
#13238=ORIENTED_EDGE('',*,*,#9700,.T.);
#13239=ORIENTED_EDGE('',*,*,#9701,.T.);
#13240=ORIENTED_EDGE('',*,*,#9702,.T.);
#13241=ORIENTED_EDGE('',*,*,#9703,.T.);
#13242=ORIENTED_EDGE('',*,*,#9704,.T.);
#13243=ORIENTED_EDGE('',*,*,#9705,.T.);
#13244=ORIENTED_EDGE('',*,*,#9706,.T.);
#13245=ORIENTED_EDGE('',*,*,#9707,.T.);
#13246=ORIENTED_EDGE('',*,*,#9708,.T.);
#13247=ORIENTED_EDGE('',*,*,#9709,.T.);
#13248=ORIENTED_EDGE('',*,*,#9710,.T.);
#13249=ORIENTED_EDGE('',*,*,#9711,.T.);
#13250=ORIENTED_EDGE('',*,*,#9712,.T.);
#13251=ORIENTED_EDGE('',*,*,#9713,.T.);
#13252=ORIENTED_EDGE('',*,*,#9714,.T.);
#13253=ORIENTED_EDGE('',*,*,#9715,.T.);
#13254=ORIENTED_EDGE('',*,*,#9716,.T.);
#13255=ORIENTED_EDGE('',*,*,#9717,.T.);
#13256=ORIENTED_EDGE('',*,*,#9718,.T.);
#13257=ORIENTED_EDGE('',*,*,#9719,.T.);
#13258=ORIENTED_EDGE('',*,*,#9720,.T.);
#13259=ORIENTED_EDGE('',*,*,#9721,.T.);
#13260=ORIENTED_EDGE('',*,*,#9722,.T.);
#13261=ORIENTED_EDGE('',*,*,#9723,.T.);
#13262=ORIENTED_EDGE('',*,*,#9724,.T.);
#13263=ORIENTED_EDGE('',*,*,#9725,.T.);
#13264=ORIENTED_EDGE('',*,*,#9726,.T.);
#13265=ORIENTED_EDGE('',*,*,#9727,.T.);
#13266=ORIENTED_EDGE('',*,*,#9728,.T.);
#13267=ORIENTED_EDGE('',*,*,#9729,.T.);
#13268=ORIENTED_EDGE('',*,*,#9637,.T.);
#13269=ORIENTED_EDGE('',*,*,#9649,.T.);
#13270=ORIENTED_EDGE('',*,*,#9644,.T.);
#13271=ORIENTED_EDGE('',*,*,#9641,.T.);
#13272=ORIENTED_EDGE('',*,*,#9647,.F.);
#13273=ORIENTED_EDGE('',*,*,#9730,.T.);
#13274=ORIENTED_EDGE('',*,*,#9731,.F.);
#13275=ORIENTED_EDGE('',*,*,#9730,.F.);
#13276=ORIENTED_EDGE('',*,*,#9732,.F.);
#13277=ORIENTED_EDGE('',*,*,#9733,.F.);
#13278=ORIENTED_EDGE('',*,*,#9734,.F.);
#13279=ORIENTED_EDGE('',*,*,#9727,.F.);
#13280=ORIENTED_EDGE('',*,*,#9734,.T.);
#13281=ORIENTED_EDGE('',*,*,#9735,.F.);
#13282=ORIENTED_EDGE('',*,*,#9736,.F.);
#13283=ORIENTED_EDGE('',*,*,#9728,.F.);
#13284=ORIENTED_EDGE('',*,*,#9736,.T.);
#13285=ORIENTED_EDGE('',*,*,#9737,.F.);
#13286=ORIENTED_EDGE('',*,*,#9738,.F.);
#13287=ORIENTED_EDGE('',*,*,#9729,.F.);
#13288=ORIENTED_EDGE('',*,*,#9738,.T.);
#13289=ORIENTED_EDGE('',*,*,#9739,.F.);
#13290=ORIENTED_EDGE('',*,*,#9740,.T.);
#13291=ORIENTED_EDGE('',*,*,#9650,.F.);
#13292=ORIENTED_EDGE('',*,*,#9740,.F.);
#13293=ORIENTED_EDGE('',*,*,#9741,.F.);
#13294=ORIENTED_EDGE('',*,*,#9742,.F.);
#13295=ORIENTED_EDGE('',*,*,#9651,.F.);
#13296=ORIENTED_EDGE('',*,*,#9742,.T.);
#13297=ORIENTED_EDGE('',*,*,#9743,.F.);
#13298=ORIENTED_EDGE('',*,*,#9744,.F.);
#13299=ORIENTED_EDGE('',*,*,#9652,.F.);
#13300=ORIENTED_EDGE('',*,*,#9744,.T.);
#13301=ORIENTED_EDGE('',*,*,#9745,.F.);
#13302=ORIENTED_EDGE('',*,*,#9746,.F.);
#13303=ORIENTED_EDGE('',*,*,#9653,.F.);
#13304=ORIENTED_EDGE('',*,*,#9746,.T.);
#13305=ORIENTED_EDGE('',*,*,#9747,.F.);
#13306=ORIENTED_EDGE('',*,*,#9748,.T.);
#13307=ORIENTED_EDGE('',*,*,#9654,.F.);
#13308=ORIENTED_EDGE('',*,*,#9748,.F.);
#13309=ORIENTED_EDGE('',*,*,#9749,.F.);
#13310=ORIENTED_EDGE('',*,*,#9750,.F.);
#13311=ORIENTED_EDGE('',*,*,#9655,.F.);
#13312=ORIENTED_EDGE('',*,*,#9750,.T.);
#13313=ORIENTED_EDGE('',*,*,#9751,.F.);
#13314=ORIENTED_EDGE('',*,*,#9752,.F.);
#13315=ORIENTED_EDGE('',*,*,#9656,.F.);
#13316=ORIENTED_EDGE('',*,*,#9752,.T.);
#13317=ORIENTED_EDGE('',*,*,#9753,.F.);
#13318=ORIENTED_EDGE('',*,*,#9754,.F.);
#13319=ORIENTED_EDGE('',*,*,#9657,.F.);
#13320=ORIENTED_EDGE('',*,*,#9754,.T.);
#13321=ORIENTED_EDGE('',*,*,#9755,.F.);
#13322=ORIENTED_EDGE('',*,*,#9756,.T.);
#13323=ORIENTED_EDGE('',*,*,#9658,.F.);
#13324=ORIENTED_EDGE('',*,*,#9756,.F.);
#13325=ORIENTED_EDGE('',*,*,#9757,.F.);
#13326=ORIENTED_EDGE('',*,*,#9758,.F.);
#13327=ORIENTED_EDGE('',*,*,#9659,.F.);
#13328=ORIENTED_EDGE('',*,*,#9758,.T.);
#13329=ORIENTED_EDGE('',*,*,#9759,.F.);
#13330=ORIENTED_EDGE('',*,*,#9760,.F.);
#13331=ORIENTED_EDGE('',*,*,#9660,.F.);
#13332=ORIENTED_EDGE('',*,*,#9760,.T.);
#13333=ORIENTED_EDGE('',*,*,#9761,.F.);
#13334=ORIENTED_EDGE('',*,*,#9762,.F.);
#13335=ORIENTED_EDGE('',*,*,#9661,.F.);
#13336=ORIENTED_EDGE('',*,*,#9762,.T.);
#13337=ORIENTED_EDGE('',*,*,#9763,.F.);
#13338=ORIENTED_EDGE('',*,*,#9764,.T.);
#13339=ORIENTED_EDGE('',*,*,#9662,.F.);
#13340=ORIENTED_EDGE('',*,*,#9764,.F.);
#13341=ORIENTED_EDGE('',*,*,#9765,.F.);
#13342=ORIENTED_EDGE('',*,*,#9766,.F.);
#13343=ORIENTED_EDGE('',*,*,#9663,.F.);
#13344=ORIENTED_EDGE('',*,*,#9766,.T.);
#13345=ORIENTED_EDGE('',*,*,#9767,.F.);
#13346=ORIENTED_EDGE('',*,*,#9768,.F.);
#13347=ORIENTED_EDGE('',*,*,#9664,.F.);
#13348=ORIENTED_EDGE('',*,*,#9768,.T.);
#13349=ORIENTED_EDGE('',*,*,#9769,.F.);
#13350=ORIENTED_EDGE('',*,*,#9770,.F.);
#13351=ORIENTED_EDGE('',*,*,#9665,.F.);
#13352=ORIENTED_EDGE('',*,*,#9770,.T.);
#13353=ORIENTED_EDGE('',*,*,#9771,.F.);
#13354=ORIENTED_EDGE('',*,*,#9772,.T.);
#13355=ORIENTED_EDGE('',*,*,#9666,.F.);
#13356=ORIENTED_EDGE('',*,*,#9772,.F.);
#13357=ORIENTED_EDGE('',*,*,#9773,.F.);
#13358=ORIENTED_EDGE('',*,*,#9774,.F.);
#13359=ORIENTED_EDGE('',*,*,#9667,.F.);
#13360=ORIENTED_EDGE('',*,*,#9774,.T.);
#13361=ORIENTED_EDGE('',*,*,#9775,.F.);
#13362=ORIENTED_EDGE('',*,*,#9776,.F.);
#13363=ORIENTED_EDGE('',*,*,#9668,.F.);
#13364=ORIENTED_EDGE('',*,*,#9776,.T.);
#13365=ORIENTED_EDGE('',*,*,#9777,.F.);
#13366=ORIENTED_EDGE('',*,*,#9778,.F.);
#13367=ORIENTED_EDGE('',*,*,#9669,.F.);
#13368=ORIENTED_EDGE('',*,*,#9778,.T.);
#13369=ORIENTED_EDGE('',*,*,#9779,.F.);
#13370=ORIENTED_EDGE('',*,*,#9780,.T.);
#13371=ORIENTED_EDGE('',*,*,#9670,.F.);
#13372=ORIENTED_EDGE('',*,*,#9780,.F.);
#13373=ORIENTED_EDGE('',*,*,#9781,.F.);
#13374=ORIENTED_EDGE('',*,*,#9782,.F.);
#13375=ORIENTED_EDGE('',*,*,#9671,.F.);
#13376=ORIENTED_EDGE('',*,*,#9782,.T.);
#13377=ORIENTED_EDGE('',*,*,#9783,.F.);
#13378=ORIENTED_EDGE('',*,*,#9784,.F.);
#13379=ORIENTED_EDGE('',*,*,#9672,.F.);
#13380=ORIENTED_EDGE('',*,*,#9784,.T.);
#13381=ORIENTED_EDGE('',*,*,#9785,.F.);
#13382=ORIENTED_EDGE('',*,*,#9786,.F.);
#13383=ORIENTED_EDGE('',*,*,#9673,.F.);
#13384=ORIENTED_EDGE('',*,*,#9786,.T.);
#13385=ORIENTED_EDGE('',*,*,#9787,.F.);
#13386=ORIENTED_EDGE('',*,*,#9788,.T.);
#13387=ORIENTED_EDGE('',*,*,#9674,.F.);
#13388=ORIENTED_EDGE('',*,*,#9788,.F.);
#13389=ORIENTED_EDGE('',*,*,#9789,.F.);
#13390=ORIENTED_EDGE('',*,*,#9790,.F.);
#13391=ORIENTED_EDGE('',*,*,#9675,.F.);
#13392=ORIENTED_EDGE('',*,*,#9790,.T.);
#13393=ORIENTED_EDGE('',*,*,#9791,.F.);
#13394=ORIENTED_EDGE('',*,*,#9792,.F.);
#13395=ORIENTED_EDGE('',*,*,#9676,.F.);
#13396=ORIENTED_EDGE('',*,*,#9792,.T.);
#13397=ORIENTED_EDGE('',*,*,#9793,.F.);
#13398=ORIENTED_EDGE('',*,*,#9794,.F.);
#13399=ORIENTED_EDGE('',*,*,#9677,.F.);
#13400=ORIENTED_EDGE('',*,*,#9794,.T.);
#13401=ORIENTED_EDGE('',*,*,#9795,.F.);
#13402=ORIENTED_EDGE('',*,*,#9796,.T.);
#13403=ORIENTED_EDGE('',*,*,#9678,.F.);
#13404=ORIENTED_EDGE('',*,*,#9796,.F.);
#13405=ORIENTED_EDGE('',*,*,#9797,.F.);
#13406=ORIENTED_EDGE('',*,*,#9798,.F.);
#13407=ORIENTED_EDGE('',*,*,#9679,.F.);
#13408=ORIENTED_EDGE('',*,*,#9798,.T.);
#13409=ORIENTED_EDGE('',*,*,#9799,.F.);
#13410=ORIENTED_EDGE('',*,*,#9800,.F.);
#13411=ORIENTED_EDGE('',*,*,#9680,.F.);
#13412=ORIENTED_EDGE('',*,*,#9800,.T.);
#13413=ORIENTED_EDGE('',*,*,#9801,.F.);
#13414=ORIENTED_EDGE('',*,*,#9802,.F.);
#13415=ORIENTED_EDGE('',*,*,#9681,.F.);
#13416=ORIENTED_EDGE('',*,*,#9802,.T.);
#13417=ORIENTED_EDGE('',*,*,#9803,.F.);
#13418=ORIENTED_EDGE('',*,*,#9804,.T.);
#13419=ORIENTED_EDGE('',*,*,#9682,.F.);
#13420=ORIENTED_EDGE('',*,*,#9804,.F.);
#13421=ORIENTED_EDGE('',*,*,#9805,.F.);
#13422=ORIENTED_EDGE('',*,*,#9806,.F.);
#13423=ORIENTED_EDGE('',*,*,#9683,.F.);
#13424=ORIENTED_EDGE('',*,*,#9806,.T.);
#13425=ORIENTED_EDGE('',*,*,#9807,.F.);
#13426=ORIENTED_EDGE('',*,*,#9808,.F.);
#13427=ORIENTED_EDGE('',*,*,#9684,.F.);
#13428=ORIENTED_EDGE('',*,*,#9808,.T.);
#13429=ORIENTED_EDGE('',*,*,#9809,.F.);
#13430=ORIENTED_EDGE('',*,*,#9810,.F.);
#13431=ORIENTED_EDGE('',*,*,#9685,.F.);
#13432=ORIENTED_EDGE('',*,*,#9810,.T.);
#13433=ORIENTED_EDGE('',*,*,#9811,.F.);
#13434=ORIENTED_EDGE('',*,*,#9812,.T.);
#13435=ORIENTED_EDGE('',*,*,#9686,.F.);
#13436=ORIENTED_EDGE('',*,*,#9812,.F.);
#13437=ORIENTED_EDGE('',*,*,#9813,.F.);
#13438=ORIENTED_EDGE('',*,*,#9814,.F.);
#13439=ORIENTED_EDGE('',*,*,#9687,.F.);
#13440=ORIENTED_EDGE('',*,*,#9814,.T.);
#13441=ORIENTED_EDGE('',*,*,#9815,.F.);
#13442=ORIENTED_EDGE('',*,*,#9816,.F.);
#13443=ORIENTED_EDGE('',*,*,#9688,.F.);
#13444=ORIENTED_EDGE('',*,*,#9816,.T.);
#13445=ORIENTED_EDGE('',*,*,#9817,.F.);
#13446=ORIENTED_EDGE('',*,*,#9818,.F.);
#13447=ORIENTED_EDGE('',*,*,#9689,.F.);
#13448=ORIENTED_EDGE('',*,*,#9818,.T.);
#13449=ORIENTED_EDGE('',*,*,#9819,.F.);
#13450=ORIENTED_EDGE('',*,*,#9820,.T.);
#13451=ORIENTED_EDGE('',*,*,#9690,.F.);
#13452=ORIENTED_EDGE('',*,*,#9820,.F.);
#13453=ORIENTED_EDGE('',*,*,#9821,.F.);
#13454=ORIENTED_EDGE('',*,*,#9822,.F.);
#13455=ORIENTED_EDGE('',*,*,#9691,.F.);
#13456=ORIENTED_EDGE('',*,*,#9822,.T.);
#13457=ORIENTED_EDGE('',*,*,#9823,.F.);
#13458=ORIENTED_EDGE('',*,*,#9824,.F.);
#13459=ORIENTED_EDGE('',*,*,#9692,.F.);
#13460=ORIENTED_EDGE('',*,*,#9824,.T.);
#13461=ORIENTED_EDGE('',*,*,#9825,.F.);
#13462=ORIENTED_EDGE('',*,*,#9826,.F.);
#13463=ORIENTED_EDGE('',*,*,#9693,.F.);
#13464=ORIENTED_EDGE('',*,*,#9826,.T.);
#13465=ORIENTED_EDGE('',*,*,#9827,.F.);
#13466=ORIENTED_EDGE('',*,*,#9828,.T.);
#13467=ORIENTED_EDGE('',*,*,#9694,.F.);
#13468=ORIENTED_EDGE('',*,*,#9828,.F.);
#13469=ORIENTED_EDGE('',*,*,#9829,.F.);
#13470=ORIENTED_EDGE('',*,*,#9830,.F.);
#13471=ORIENTED_EDGE('',*,*,#9695,.F.);
#13472=ORIENTED_EDGE('',*,*,#9830,.T.);
#13473=ORIENTED_EDGE('',*,*,#9831,.F.);
#13474=ORIENTED_EDGE('',*,*,#9832,.F.);
#13475=ORIENTED_EDGE('',*,*,#9696,.F.);
#13476=ORIENTED_EDGE('',*,*,#9832,.T.);
#13477=ORIENTED_EDGE('',*,*,#9833,.F.);
#13478=ORIENTED_EDGE('',*,*,#9834,.F.);
#13479=ORIENTED_EDGE('',*,*,#9697,.F.);
#13480=ORIENTED_EDGE('',*,*,#9834,.T.);
#13481=ORIENTED_EDGE('',*,*,#9835,.F.);
#13482=ORIENTED_EDGE('',*,*,#9836,.T.);
#13483=ORIENTED_EDGE('',*,*,#9698,.F.);
#13484=ORIENTED_EDGE('',*,*,#9836,.F.);
#13485=ORIENTED_EDGE('',*,*,#9837,.F.);
#13486=ORIENTED_EDGE('',*,*,#9838,.F.);
#13487=ORIENTED_EDGE('',*,*,#9699,.F.);
#13488=ORIENTED_EDGE('',*,*,#9838,.T.);
#13489=ORIENTED_EDGE('',*,*,#9839,.F.);
#13490=ORIENTED_EDGE('',*,*,#9840,.F.);
#13491=ORIENTED_EDGE('',*,*,#9700,.F.);
#13492=ORIENTED_EDGE('',*,*,#9840,.T.);
#13493=ORIENTED_EDGE('',*,*,#9841,.F.);
#13494=ORIENTED_EDGE('',*,*,#9842,.F.);
#13495=ORIENTED_EDGE('',*,*,#9701,.F.);
#13496=ORIENTED_EDGE('',*,*,#9842,.T.);
#13497=ORIENTED_EDGE('',*,*,#9843,.F.);
#13498=ORIENTED_EDGE('',*,*,#9844,.T.);
#13499=ORIENTED_EDGE('',*,*,#9702,.F.);
#13500=ORIENTED_EDGE('',*,*,#9844,.F.);
#13501=ORIENTED_EDGE('',*,*,#9845,.F.);
#13502=ORIENTED_EDGE('',*,*,#9846,.F.);
#13503=ORIENTED_EDGE('',*,*,#9703,.F.);
#13504=ORIENTED_EDGE('',*,*,#9846,.T.);
#13505=ORIENTED_EDGE('',*,*,#9847,.F.);
#13506=ORIENTED_EDGE('',*,*,#9848,.F.);
#13507=ORIENTED_EDGE('',*,*,#9704,.F.);
#13508=ORIENTED_EDGE('',*,*,#9848,.T.);
#13509=ORIENTED_EDGE('',*,*,#9849,.F.);
#13510=ORIENTED_EDGE('',*,*,#9850,.F.);
#13511=ORIENTED_EDGE('',*,*,#9705,.F.);
#13512=ORIENTED_EDGE('',*,*,#9850,.T.);
#13513=ORIENTED_EDGE('',*,*,#9851,.F.);
#13514=ORIENTED_EDGE('',*,*,#9852,.T.);
#13515=ORIENTED_EDGE('',*,*,#9706,.F.);
#13516=ORIENTED_EDGE('',*,*,#9852,.F.);
#13517=ORIENTED_EDGE('',*,*,#9853,.F.);
#13518=ORIENTED_EDGE('',*,*,#9854,.F.);
#13519=ORIENTED_EDGE('',*,*,#9707,.F.);
#13520=ORIENTED_EDGE('',*,*,#9854,.T.);
#13521=ORIENTED_EDGE('',*,*,#9855,.F.);
#13522=ORIENTED_EDGE('',*,*,#9856,.F.);
#13523=ORIENTED_EDGE('',*,*,#9708,.F.);
#13524=ORIENTED_EDGE('',*,*,#9856,.T.);
#13525=ORIENTED_EDGE('',*,*,#9857,.F.);
#13526=ORIENTED_EDGE('',*,*,#9858,.F.);
#13527=ORIENTED_EDGE('',*,*,#9709,.F.);
#13528=ORIENTED_EDGE('',*,*,#9858,.T.);
#13529=ORIENTED_EDGE('',*,*,#9859,.F.);
#13530=ORIENTED_EDGE('',*,*,#9860,.T.);
#13531=ORIENTED_EDGE('',*,*,#9710,.F.);
#13532=ORIENTED_EDGE('',*,*,#9860,.F.);
#13533=ORIENTED_EDGE('',*,*,#9861,.F.);
#13534=ORIENTED_EDGE('',*,*,#9862,.F.);
#13535=ORIENTED_EDGE('',*,*,#9711,.F.);
#13536=ORIENTED_EDGE('',*,*,#9862,.T.);
#13537=ORIENTED_EDGE('',*,*,#9863,.F.);
#13538=ORIENTED_EDGE('',*,*,#9864,.F.);
#13539=ORIENTED_EDGE('',*,*,#9712,.F.);
#13540=ORIENTED_EDGE('',*,*,#9864,.T.);
#13541=ORIENTED_EDGE('',*,*,#9865,.F.);
#13542=ORIENTED_EDGE('',*,*,#9866,.F.);
#13543=ORIENTED_EDGE('',*,*,#9713,.F.);
#13544=ORIENTED_EDGE('',*,*,#9866,.T.);
#13545=ORIENTED_EDGE('',*,*,#9867,.F.);
#13546=ORIENTED_EDGE('',*,*,#9868,.T.);
#13547=ORIENTED_EDGE('',*,*,#9714,.F.);
#13548=ORIENTED_EDGE('',*,*,#9868,.F.);
#13549=ORIENTED_EDGE('',*,*,#9869,.F.);
#13550=ORIENTED_EDGE('',*,*,#9870,.F.);
#13551=ORIENTED_EDGE('',*,*,#9715,.F.);
#13552=ORIENTED_EDGE('',*,*,#9870,.T.);
#13553=ORIENTED_EDGE('',*,*,#9871,.F.);
#13554=ORIENTED_EDGE('',*,*,#9872,.F.);
#13555=ORIENTED_EDGE('',*,*,#9716,.F.);
#13556=ORIENTED_EDGE('',*,*,#9872,.T.);
#13557=ORIENTED_EDGE('',*,*,#9873,.F.);
#13558=ORIENTED_EDGE('',*,*,#9874,.F.);
#13559=ORIENTED_EDGE('',*,*,#9717,.F.);
#13560=ORIENTED_EDGE('',*,*,#9874,.T.);
#13561=ORIENTED_EDGE('',*,*,#9875,.F.);
#13562=ORIENTED_EDGE('',*,*,#9876,.T.);
#13563=ORIENTED_EDGE('',*,*,#9718,.F.);
#13564=ORIENTED_EDGE('',*,*,#9876,.F.);
#13565=ORIENTED_EDGE('',*,*,#9877,.F.);
#13566=ORIENTED_EDGE('',*,*,#9878,.F.);
#13567=ORIENTED_EDGE('',*,*,#9719,.F.);
#13568=ORIENTED_EDGE('',*,*,#9878,.T.);
#13569=ORIENTED_EDGE('',*,*,#9879,.F.);
#13570=ORIENTED_EDGE('',*,*,#9880,.F.);
#13571=ORIENTED_EDGE('',*,*,#9720,.F.);
#13572=ORIENTED_EDGE('',*,*,#9880,.T.);
#13573=ORIENTED_EDGE('',*,*,#9881,.F.);
#13574=ORIENTED_EDGE('',*,*,#9882,.F.);
#13575=ORIENTED_EDGE('',*,*,#9721,.F.);
#13576=ORIENTED_EDGE('',*,*,#9882,.T.);
#13577=ORIENTED_EDGE('',*,*,#9883,.F.);
#13578=ORIENTED_EDGE('',*,*,#9884,.T.);
#13579=ORIENTED_EDGE('',*,*,#9722,.F.);
#13580=ORIENTED_EDGE('',*,*,#9884,.F.);
#13581=ORIENTED_EDGE('',*,*,#9885,.F.);
#13582=ORIENTED_EDGE('',*,*,#9886,.F.);
#13583=ORIENTED_EDGE('',*,*,#9723,.F.);
#13584=ORIENTED_EDGE('',*,*,#9886,.T.);
#13585=ORIENTED_EDGE('',*,*,#9887,.F.);
#13586=ORIENTED_EDGE('',*,*,#9888,.F.);
#13587=ORIENTED_EDGE('',*,*,#9724,.F.);
#13588=ORIENTED_EDGE('',*,*,#9888,.T.);
#13589=ORIENTED_EDGE('',*,*,#9889,.F.);
#13590=ORIENTED_EDGE('',*,*,#9890,.F.);
#13591=ORIENTED_EDGE('',*,*,#9725,.F.);
#13592=ORIENTED_EDGE('',*,*,#9891,.T.);
#13593=ORIENTED_EDGE('',*,*,#9889,.T.);
#13594=ORIENTED_EDGE('',*,*,#9887,.T.);
#13595=ORIENTED_EDGE('',*,*,#9885,.T.);
#13596=ORIENTED_EDGE('',*,*,#9883,.T.);
#13597=ORIENTED_EDGE('',*,*,#9881,.T.);
#13598=ORIENTED_EDGE('',*,*,#9879,.T.);
#13599=ORIENTED_EDGE('',*,*,#9877,.T.);
#13600=ORIENTED_EDGE('',*,*,#9875,.T.);
#13601=ORIENTED_EDGE('',*,*,#9873,.T.);
#13602=ORIENTED_EDGE('',*,*,#9871,.T.);
#13603=ORIENTED_EDGE('',*,*,#9869,.T.);
#13604=ORIENTED_EDGE('',*,*,#9867,.T.);
#13605=ORIENTED_EDGE('',*,*,#9865,.T.);
#13606=ORIENTED_EDGE('',*,*,#9863,.T.);
#13607=ORIENTED_EDGE('',*,*,#9861,.T.);
#13608=ORIENTED_EDGE('',*,*,#9859,.T.);
#13609=ORIENTED_EDGE('',*,*,#9857,.T.);
#13610=ORIENTED_EDGE('',*,*,#9855,.T.);
#13611=ORIENTED_EDGE('',*,*,#9853,.T.);
#13612=ORIENTED_EDGE('',*,*,#9851,.T.);
#13613=ORIENTED_EDGE('',*,*,#9849,.T.);
#13614=ORIENTED_EDGE('',*,*,#9847,.T.);
#13615=ORIENTED_EDGE('',*,*,#9845,.T.);
#13616=ORIENTED_EDGE('',*,*,#9843,.T.);
#13617=ORIENTED_EDGE('',*,*,#9841,.T.);
#13618=ORIENTED_EDGE('',*,*,#9839,.T.);
#13619=ORIENTED_EDGE('',*,*,#9837,.T.);
#13620=ORIENTED_EDGE('',*,*,#9835,.T.);
#13621=ORIENTED_EDGE('',*,*,#9833,.T.);
#13622=ORIENTED_EDGE('',*,*,#9831,.T.);
#13623=ORIENTED_EDGE('',*,*,#9829,.T.);
#13624=ORIENTED_EDGE('',*,*,#9827,.T.);
#13625=ORIENTED_EDGE('',*,*,#9825,.T.);
#13626=ORIENTED_EDGE('',*,*,#9823,.T.);
#13627=ORIENTED_EDGE('',*,*,#9821,.T.);
#13628=ORIENTED_EDGE('',*,*,#9819,.T.);
#13629=ORIENTED_EDGE('',*,*,#9817,.T.);
#13630=ORIENTED_EDGE('',*,*,#9815,.T.);
#13631=ORIENTED_EDGE('',*,*,#9813,.T.);
#13632=ORIENTED_EDGE('',*,*,#9811,.T.);
#13633=ORIENTED_EDGE('',*,*,#9809,.T.);
#13634=ORIENTED_EDGE('',*,*,#9807,.T.);
#13635=ORIENTED_EDGE('',*,*,#9805,.T.);
#13636=ORIENTED_EDGE('',*,*,#9803,.T.);
#13637=ORIENTED_EDGE('',*,*,#9801,.T.);
#13638=ORIENTED_EDGE('',*,*,#9799,.T.);
#13639=ORIENTED_EDGE('',*,*,#9797,.T.);
#13640=ORIENTED_EDGE('',*,*,#9795,.T.);
#13641=ORIENTED_EDGE('',*,*,#9793,.T.);
#13642=ORIENTED_EDGE('',*,*,#9791,.T.);
#13643=ORIENTED_EDGE('',*,*,#9789,.T.);
#13644=ORIENTED_EDGE('',*,*,#9787,.T.);
#13645=ORIENTED_EDGE('',*,*,#9785,.T.);
#13646=ORIENTED_EDGE('',*,*,#9783,.T.);
#13647=ORIENTED_EDGE('',*,*,#9781,.T.);
#13648=ORIENTED_EDGE('',*,*,#9779,.T.);
#13649=ORIENTED_EDGE('',*,*,#9777,.T.);
#13650=ORIENTED_EDGE('',*,*,#9775,.T.);
#13651=ORIENTED_EDGE('',*,*,#9773,.T.);
#13652=ORIENTED_EDGE('',*,*,#9771,.T.);
#13653=ORIENTED_EDGE('',*,*,#9769,.T.);
#13654=ORIENTED_EDGE('',*,*,#9767,.T.);
#13655=ORIENTED_EDGE('',*,*,#9765,.T.);
#13656=ORIENTED_EDGE('',*,*,#9763,.T.);
#13657=ORIENTED_EDGE('',*,*,#9761,.T.);
#13658=ORIENTED_EDGE('',*,*,#9759,.T.);
#13659=ORIENTED_EDGE('',*,*,#9757,.T.);
#13660=ORIENTED_EDGE('',*,*,#9755,.T.);
#13661=ORIENTED_EDGE('',*,*,#9753,.T.);
#13662=ORIENTED_EDGE('',*,*,#9751,.T.);
#13663=ORIENTED_EDGE('',*,*,#9749,.T.);
#13664=ORIENTED_EDGE('',*,*,#9747,.T.);
#13665=ORIENTED_EDGE('',*,*,#9745,.T.);
#13666=ORIENTED_EDGE('',*,*,#9743,.T.);
#13667=ORIENTED_EDGE('',*,*,#9741,.T.);
#13668=ORIENTED_EDGE('',*,*,#9739,.T.);
#13669=ORIENTED_EDGE('',*,*,#9737,.T.);
#13670=ORIENTED_EDGE('',*,*,#9735,.T.);
#13671=ORIENTED_EDGE('',*,*,#9733,.T.);
#13672=ORIENTED_EDGE('',*,*,#9731,.T.);
#13673=ORIENTED_EDGE('',*,*,#9732,.T.);
#13674=ORIENTED_EDGE('',*,*,#9726,.F.);
#13675=ORIENTED_EDGE('',*,*,#9890,.T.);
#13676=ORIENTED_EDGE('',*,*,#9891,.F.);
#13677=ORIENTED_EDGE('',*,*,#9892,.F.);
#13678=ORIENTED_EDGE('',*,*,#9893,.T.);
#13679=ORIENTED_EDGE('',*,*,#9894,.F.);
#13680=ORIENTED_EDGE('',*,*,#9895,.T.);
#13681=ORIENTED_EDGE('',*,*,#9896,.F.);
#13682=ORIENTED_EDGE('',*,*,#9895,.F.);
#13683=ORIENTED_EDGE('',*,*,#9897,.F.);
#13684=ORIENTED_EDGE('',*,*,#9898,.F.);
#13685=ORIENTED_EDGE('',*,*,#9899,.F.);
#13686=ORIENTED_EDGE('',*,*,#9898,.T.);
#13687=ORIENTED_EDGE('',*,*,#9900,.T.);
#13688=ORIENTED_EDGE('',*,*,#9901,.T.);
#13689=ORIENTED_EDGE('',*,*,#9897,.T.);
#13690=ORIENTED_EDGE('',*,*,#9894,.T.);
#13691=ORIENTED_EDGE('',*,*,#9902,.T.);
#13692=ORIENTED_EDGE('',*,*,#9900,.F.);
#13693=ORIENTED_EDGE('',*,*,#9903,.F.);
#13694=ORIENTED_EDGE('',*,*,#9901,.F.);
#13695=ORIENTED_EDGE('',*,*,#9902,.F.);
#13696=ORIENTED_EDGE('',*,*,#9893,.F.);
#13697=ORIENTED_EDGE('',*,*,#9904,.F.);
#13698=ORIENTED_EDGE('',*,*,#9905,.T.);
#13699=ORIENTED_EDGE('',*,*,#9906,.T.);
#13700=ORIENTED_EDGE('',*,*,#9905,.F.);
#13701=ORIENTED_EDGE('',*,*,#9899,.T.);
#13702=ORIENTED_EDGE('',*,*,#9903,.T.);
#13703=ORIENTED_EDGE('',*,*,#9892,.T.);
#13704=ORIENTED_EDGE('',*,*,#9896,.T.);
#13705=ORIENTED_EDGE('',*,*,#9904,.T.);
#13706=ORIENTED_EDGE('',*,*,#9906,.F.);
#13707=ORIENTED_EDGE('',*,*,#9907,.F.);
#13708=ORIENTED_EDGE('',*,*,#9908,.T.);
#13709=ORIENTED_EDGE('',*,*,#9909,.F.);
#13710=ORIENTED_EDGE('',*,*,#9910,.F.);
#13711=ORIENTED_EDGE('',*,*,#9911,.T.);
#13712=ORIENTED_EDGE('',*,*,#9912,.F.);
#13713=ORIENTED_EDGE('',*,*,#9913,.F.);
#13714=ORIENTED_EDGE('',*,*,#9911,.F.);
#13715=ORIENTED_EDGE('',*,*,#9914,.F.);
#13716=ORIENTED_EDGE('',*,*,#9915,.F.);
#13717=ORIENTED_EDGE('',*,*,#9908,.F.);
#13718=ORIENTED_EDGE('',*,*,#9916,.F.);
#13719=ORIENTED_EDGE('',*,*,#9914,.T.);
#13720=ORIENTED_EDGE('',*,*,#9910,.T.);
#13721=ORIENTED_EDGE('',*,*,#9917,.F.);
#13722=ORIENTED_EDGE('',*,*,#9918,.T.);
#13723=ORIENTED_EDGE('',*,*,#9919,.T.);
#13724=ORIENTED_EDGE('',*,*,#9918,.F.);
#13725=ORIENTED_EDGE('',*,*,#9915,.T.);
#13726=ORIENTED_EDGE('',*,*,#9916,.T.);
#13727=ORIENTED_EDGE('',*,*,#9909,.T.);
#13728=ORIENTED_EDGE('',*,*,#9907,.T.);
#13729=ORIENTED_EDGE('',*,*,#9920,.F.);
#13730=ORIENTED_EDGE('',*,*,#9921,.T.);
#13731=ORIENTED_EDGE('',*,*,#9922,.T.);
#13732=ORIENTED_EDGE('',*,*,#9921,.F.);
#13733=ORIENTED_EDGE('',*,*,#9912,.T.);
#13734=ORIENTED_EDGE('',*,*,#9913,.T.);
#13735=ORIENTED_EDGE('',*,*,#9920,.T.);
#13736=ORIENTED_EDGE('',*,*,#9917,.T.);
#13737=ORIENTED_EDGE('',*,*,#9922,.F.);
#13738=ORIENTED_EDGE('',*,*,#9919,.F.);
#13739=ORIENTED_EDGE('',*,*,#9923,.F.);
#13740=ORIENTED_EDGE('',*,*,#9924,.T.);
#13741=ORIENTED_EDGE('',*,*,#9925,.F.);
#13742=ORIENTED_EDGE('',*,*,#9926,.F.);
#13743=ORIENTED_EDGE('',*,*,#9927,.T.);
#13744=ORIENTED_EDGE('',*,*,#9928,.F.);
#13745=ORIENTED_EDGE('',*,*,#9929,.F.);
#13746=ORIENTED_EDGE('',*,*,#9927,.F.);
#13747=ORIENTED_EDGE('',*,*,#9930,.F.);
#13748=ORIENTED_EDGE('',*,*,#9931,.F.);
#13749=ORIENTED_EDGE('',*,*,#9924,.F.);
#13750=ORIENTED_EDGE('',*,*,#9932,.F.);
#13751=ORIENTED_EDGE('',*,*,#9930,.T.);
#13752=ORIENTED_EDGE('',*,*,#9926,.T.);
#13753=ORIENTED_EDGE('',*,*,#9933,.F.);
#13754=ORIENTED_EDGE('',*,*,#9934,.T.);
#13755=ORIENTED_EDGE('',*,*,#9935,.T.);
#13756=ORIENTED_EDGE('',*,*,#9934,.F.);
#13757=ORIENTED_EDGE('',*,*,#9931,.T.);
#13758=ORIENTED_EDGE('',*,*,#9932,.T.);
#13759=ORIENTED_EDGE('',*,*,#9925,.T.);
#13760=ORIENTED_EDGE('',*,*,#9923,.T.);
#13761=ORIENTED_EDGE('',*,*,#9936,.F.);
#13762=ORIENTED_EDGE('',*,*,#9937,.T.);
#13763=ORIENTED_EDGE('',*,*,#9938,.T.);
#13764=ORIENTED_EDGE('',*,*,#9937,.F.);
#13765=ORIENTED_EDGE('',*,*,#9928,.T.);
#13766=ORIENTED_EDGE('',*,*,#9929,.T.);
#13767=ORIENTED_EDGE('',*,*,#9936,.T.);
#13768=ORIENTED_EDGE('',*,*,#9933,.T.);
#13769=ORIENTED_EDGE('',*,*,#9938,.F.);
#13770=ORIENTED_EDGE('',*,*,#9935,.F.);
#13771=ORIENTED_EDGE('',*,*,#9939,.F.);
#13772=ORIENTED_EDGE('',*,*,#9940,.T.);
#13773=ORIENTED_EDGE('',*,*,#9941,.T.);
#13774=ORIENTED_EDGE('',*,*,#9940,.F.);
#13775=ORIENTED_EDGE('',*,*,#9942,.F.);
#13776=ORIENTED_EDGE('',*,*,#9943,.T.);
#13777=ORIENTED_EDGE('',*,*,#9944,.T.);
#13778=ORIENTED_EDGE('',*,*,#9943,.F.);
#13779=ORIENTED_EDGE('',*,*,#9942,.T.);
#13780=ORIENTED_EDGE('',*,*,#9939,.T.);
#13781=ORIENTED_EDGE('',*,*,#9944,.F.);
#13782=ORIENTED_EDGE('',*,*,#9941,.F.);
#13783=ORIENTED_EDGE('',*,*,#9945,.F.);
#13784=ORIENTED_EDGE('',*,*,#9946,.T.);
#13785=ORIENTED_EDGE('',*,*,#9947,.T.);
#13786=ORIENTED_EDGE('',*,*,#9946,.F.);
#13787=ORIENTED_EDGE('',*,*,#9948,.F.);
#13788=ORIENTED_EDGE('',*,*,#9949,.T.);
#13789=ORIENTED_EDGE('',*,*,#9950,.T.);
#13790=ORIENTED_EDGE('',*,*,#9949,.F.);
#13791=ORIENTED_EDGE('',*,*,#9948,.T.);
#13792=ORIENTED_EDGE('',*,*,#9945,.T.);
#13793=ORIENTED_EDGE('',*,*,#9950,.F.);
#13794=ORIENTED_EDGE('',*,*,#9947,.F.);
#13795=ORIENTED_EDGE('',*,*,#9951,.F.);
#13796=ORIENTED_EDGE('',*,*,#9952,.T.);
#13797=ORIENTED_EDGE('',*,*,#9953,.T.);
#13798=ORIENTED_EDGE('',*,*,#9952,.F.);
#13799=ORIENTED_EDGE('',*,*,#9954,.F.);
#13800=ORIENTED_EDGE('',*,*,#9955,.T.);
#13801=ORIENTED_EDGE('',*,*,#9956,.T.);
#13802=ORIENTED_EDGE('',*,*,#9955,.F.);
#13803=ORIENTED_EDGE('',*,*,#9954,.T.);
#13804=ORIENTED_EDGE('',*,*,#9951,.T.);
#13805=ORIENTED_EDGE('',*,*,#9956,.F.);
#13806=ORIENTED_EDGE('',*,*,#9953,.F.);
#13807=ORIENTED_EDGE('',*,*,#9957,.F.);
#13808=ORIENTED_EDGE('',*,*,#9958,.T.);
#13809=ORIENTED_EDGE('',*,*,#9959,.T.);
#13810=ORIENTED_EDGE('',*,*,#9958,.F.);
#13811=ORIENTED_EDGE('',*,*,#9960,.F.);
#13812=ORIENTED_EDGE('',*,*,#9961,.T.);
#13813=ORIENTED_EDGE('',*,*,#9962,.T.);
#13814=ORIENTED_EDGE('',*,*,#9961,.F.);
#13815=ORIENTED_EDGE('',*,*,#9960,.T.);
#13816=ORIENTED_EDGE('',*,*,#9957,.T.);
#13817=ORIENTED_EDGE('',*,*,#9962,.F.);
#13818=ORIENTED_EDGE('',*,*,#9959,.F.);
#13819=ORIENTED_EDGE('',*,*,#9963,.F.);
#13820=ORIENTED_EDGE('',*,*,#9964,.T.);
#13821=ORIENTED_EDGE('',*,*,#9965,.T.);
#13822=ORIENTED_EDGE('',*,*,#9966,.F.);
#13823=ORIENTED_EDGE('',*,*,#9967,.F.);
#13824=ORIENTED_EDGE('',*,*,#9968,.T.);
#13825=ORIENTED_EDGE('',*,*,#9969,.T.);
#13826=ORIENTED_EDGE('',*,*,#9964,.F.);
#13827=ORIENTED_EDGE('',*,*,#9970,.F.);
#13828=ORIENTED_EDGE('',*,*,#9971,.T.);
#13829=ORIENTED_EDGE('',*,*,#9972,.T.);
#13830=ORIENTED_EDGE('',*,*,#9968,.F.);
#13831=ORIENTED_EDGE('',*,*,#9973,.F.);
#13832=ORIENTED_EDGE('',*,*,#9974,.T.);
#13833=ORIENTED_EDGE('',*,*,#9975,.T.);
#13834=ORIENTED_EDGE('',*,*,#9971,.F.);
#13835=ORIENTED_EDGE('',*,*,#9976,.F.);
#13836=ORIENTED_EDGE('',*,*,#9977,.T.);
#13837=ORIENTED_EDGE('',*,*,#9978,.T.);
#13838=ORIENTED_EDGE('',*,*,#9974,.F.);
#13839=ORIENTED_EDGE('',*,*,#9979,.F.);
#13840=ORIENTED_EDGE('',*,*,#9966,.T.);
#13841=ORIENTED_EDGE('',*,*,#9980,.T.);
#13842=ORIENTED_EDGE('',*,*,#9977,.F.);
#13843=ORIENTED_EDGE('',*,*,#9980,.F.);
#13844=ORIENTED_EDGE('',*,*,#9965,.F.);
#13845=ORIENTED_EDGE('',*,*,#9969,.F.);
#13846=ORIENTED_EDGE('',*,*,#9972,.F.);
#13847=ORIENTED_EDGE('',*,*,#9975,.F.);
#13848=ORIENTED_EDGE('',*,*,#9978,.F.);
#13849=ORIENTED_EDGE('',*,*,#9981,.F.);
#13850=ORIENTED_EDGE('',*,*,#9963,.T.);
#13851=ORIENTED_EDGE('',*,*,#9979,.T.);
#13852=ORIENTED_EDGE('',*,*,#9976,.T.);
#13853=ORIENTED_EDGE('',*,*,#9973,.T.);
#13854=ORIENTED_EDGE('',*,*,#9970,.T.);
#13855=ORIENTED_EDGE('',*,*,#9967,.T.);
#13856=ORIENTED_EDGE('',*,*,#9982,.F.);
#13857=ORIENTED_EDGE('',*,*,#9983,.T.);
#13858=ORIENTED_EDGE('',*,*,#9981,.T.);
#13859=ORIENTED_EDGE('',*,*,#9983,.F.);
#13860=ORIENTED_EDGE('',*,*,#9984,.F.);
#13861=ORIENTED_EDGE('',*,*,#9985,.T.);
#13862=ORIENTED_EDGE('',*,*,#9982,.T.);
#13863=ORIENTED_EDGE('',*,*,#9985,.F.);
#13864=ORIENTED_EDGE('',*,*,#9986,.F.);
#13865=ORIENTED_EDGE('',*,*,#9987,.T.);
#13866=ORIENTED_EDGE('',*,*,#9984,.T.);
#13867=ORIENTED_EDGE('',*,*,#9987,.F.);
#13868=ORIENTED_EDGE('',*,*,#9986,.T.);
#13869=ORIENTED_EDGE('',*,*,#9988,.F.);
#13870=ORIENTED_EDGE('',*,*,#9989,.F.);
#13871=ORIENTED_EDGE('',*,*,#9990,.F.);
#13872=ORIENTED_EDGE('',*,*,#9991,.F.);
#13873=ORIENTED_EDGE('',*,*,#9992,.F.);
#13874=ORIENTED_EDGE('',*,*,#9993,.T.);
#13875=ORIENTED_EDGE('',*,*,#9994,.F.);
#13876=ORIENTED_EDGE('',*,*,#9989,.T.);
#13877=ORIENTED_EDGE('',*,*,#9995,.F.);
#13878=ORIENTED_EDGE('',*,*,#9996,.F.);
#13879=ORIENTED_EDGE('',*,*,#9997,.F.);
#13880=ORIENTED_EDGE('',*,*,#9993,.F.);
#13881=ORIENTED_EDGE('',*,*,#9998,.T.);
#13882=ORIENTED_EDGE('',*,*,#9999,.T.);
#13883=ORIENTED_EDGE('',*,*,#10000,.T.);
#13884=ORIENTED_EDGE('',*,*,#10001,.T.);
#13885=ORIENTED_EDGE('',*,*,#10002,.T.);
#13886=ORIENTED_EDGE('',*,*,#10003,.T.);
#13887=ORIENTED_EDGE('',*,*,#10004,.T.);
#13888=ORIENTED_EDGE('',*,*,#10005,.T.);
#13889=ORIENTED_EDGE('',*,*,#10006,.T.);
#13890=ORIENTED_EDGE('',*,*,#10007,.T.);
#13891=ORIENTED_EDGE('',*,*,#10008,.T.);
#13892=ORIENTED_EDGE('',*,*,#10009,.T.);
#13893=ORIENTED_EDGE('',*,*,#10010,.T.);
#13894=ORIENTED_EDGE('',*,*,#10011,.T.);
#13895=ORIENTED_EDGE('',*,*,#10012,.T.);
#13896=ORIENTED_EDGE('',*,*,#10013,.T.);
#13897=ORIENTED_EDGE('',*,*,#10014,.T.);
#13898=ORIENTED_EDGE('',*,*,#10015,.T.);
#13899=ORIENTED_EDGE('',*,*,#10016,.T.);
#13900=ORIENTED_EDGE('',*,*,#10017,.T.);
#13901=ORIENTED_EDGE('',*,*,#10018,.T.);
#13902=ORIENTED_EDGE('',*,*,#10019,.T.);
#13903=ORIENTED_EDGE('',*,*,#10020,.T.);
#13904=ORIENTED_EDGE('',*,*,#10021,.T.);
#13905=ORIENTED_EDGE('',*,*,#10022,.T.);
#13906=ORIENTED_EDGE('',*,*,#10023,.T.);
#13907=ORIENTED_EDGE('',*,*,#10024,.T.);
#13908=ORIENTED_EDGE('',*,*,#10025,.T.);
#13909=ORIENTED_EDGE('',*,*,#10026,.T.);
#13910=ORIENTED_EDGE('',*,*,#10027,.T.);
#13911=ORIENTED_EDGE('',*,*,#10028,.T.);
#13912=ORIENTED_EDGE('',*,*,#10029,.T.);
#13913=ORIENTED_EDGE('',*,*,#10030,.T.);
#13914=ORIENTED_EDGE('',*,*,#10031,.T.);
#13915=ORIENTED_EDGE('',*,*,#10032,.T.);
#13916=ORIENTED_EDGE('',*,*,#10033,.T.);
#13917=ORIENTED_EDGE('',*,*,#10034,.T.);
#13918=ORIENTED_EDGE('',*,*,#10035,.T.);
#13919=ORIENTED_EDGE('',*,*,#10036,.T.);
#13920=ORIENTED_EDGE('',*,*,#10037,.T.);
#13921=ORIENTED_EDGE('',*,*,#10038,.T.);
#13922=ORIENTED_EDGE('',*,*,#10039,.T.);
#13923=ORIENTED_EDGE('',*,*,#10040,.T.);
#13924=ORIENTED_EDGE('',*,*,#10041,.T.);
#13925=ORIENTED_EDGE('',*,*,#10042,.T.);
#13926=ORIENTED_EDGE('',*,*,#10043,.T.);
#13927=ORIENTED_EDGE('',*,*,#10044,.T.);
#13928=ORIENTED_EDGE('',*,*,#10045,.T.);
#13929=ORIENTED_EDGE('',*,*,#10046,.T.);
#13930=ORIENTED_EDGE('',*,*,#10047,.T.);
#13931=ORIENTED_EDGE('',*,*,#10048,.T.);
#13932=ORIENTED_EDGE('',*,*,#10049,.T.);
#13933=ORIENTED_EDGE('',*,*,#10050,.T.);
#13934=ORIENTED_EDGE('',*,*,#10051,.T.);
#13935=ORIENTED_EDGE('',*,*,#10052,.T.);
#13936=ORIENTED_EDGE('',*,*,#10053,.T.);
#13937=ORIENTED_EDGE('',*,*,#10054,.T.);
#13938=ORIENTED_EDGE('',*,*,#10055,.T.);
#13939=ORIENTED_EDGE('',*,*,#10056,.T.);
#13940=ORIENTED_EDGE('',*,*,#10057,.T.);
#13941=ORIENTED_EDGE('',*,*,#10058,.T.);
#13942=ORIENTED_EDGE('',*,*,#10059,.T.);
#13943=ORIENTED_EDGE('',*,*,#10060,.T.);
#13944=ORIENTED_EDGE('',*,*,#10061,.T.);
#13945=ORIENTED_EDGE('',*,*,#10062,.T.);
#13946=ORIENTED_EDGE('',*,*,#10063,.T.);
#13947=ORIENTED_EDGE('',*,*,#10064,.T.);
#13948=ORIENTED_EDGE('',*,*,#10065,.T.);
#13949=ORIENTED_EDGE('',*,*,#10066,.T.);
#13950=ORIENTED_EDGE('',*,*,#10067,.T.);
#13951=ORIENTED_EDGE('',*,*,#10068,.T.);
#13952=ORIENTED_EDGE('',*,*,#10069,.T.);
#13953=ORIENTED_EDGE('',*,*,#10070,.T.);
#13954=ORIENTED_EDGE('',*,*,#10071,.T.);
#13955=ORIENTED_EDGE('',*,*,#10072,.T.);
#13956=ORIENTED_EDGE('',*,*,#10073,.T.);
#13957=ORIENTED_EDGE('',*,*,#10074,.T.);
#13958=ORIENTED_EDGE('',*,*,#10075,.T.);
#13959=ORIENTED_EDGE('',*,*,#10076,.T.);
#13960=ORIENTED_EDGE('',*,*,#10077,.T.);
#13961=ORIENTED_EDGE('',*,*,#10078,.T.);
#13962=ORIENTED_EDGE('',*,*,#10079,.T.);
#13963=ORIENTED_EDGE('',*,*,#10080,.T.);
#13964=ORIENTED_EDGE('',*,*,#10081,.T.);
#13965=ORIENTED_EDGE('',*,*,#10082,.T.);
#13966=ORIENTED_EDGE('',*,*,#10083,.T.);
#13967=ORIENTED_EDGE('',*,*,#10084,.T.);
#13968=ORIENTED_EDGE('',*,*,#10085,.T.);
#13969=ORIENTED_EDGE('',*,*,#10086,.T.);
#13970=ORIENTED_EDGE('',*,*,#10087,.T.);
#13971=ORIENTED_EDGE('',*,*,#10088,.T.);
#13972=ORIENTED_EDGE('',*,*,#10089,.T.);
#13973=ORIENTED_EDGE('',*,*,#10090,.T.);
#13974=ORIENTED_EDGE('',*,*,#10091,.T.);
#13975=ORIENTED_EDGE('',*,*,#10092,.T.);
#13976=ORIENTED_EDGE('',*,*,#10093,.T.);
#13977=ORIENTED_EDGE('',*,*,#10094,.T.);
#13978=ORIENTED_EDGE('',*,*,#10095,.T.);
#13979=ORIENTED_EDGE('',*,*,#10096,.T.);
#13980=ORIENTED_EDGE('',*,*,#10097,.T.);
#13981=ORIENTED_EDGE('',*,*,#10098,.T.);
#13982=ORIENTED_EDGE('',*,*,#10099,.T.);
#13983=ORIENTED_EDGE('',*,*,#10100,.T.);
#13984=ORIENTED_EDGE('',*,*,#10101,.T.);
#13985=ORIENTED_EDGE('',*,*,#10102,.T.);
#13986=ORIENTED_EDGE('',*,*,#10103,.T.);
#13987=ORIENTED_EDGE('',*,*,#10104,.T.);
#13988=ORIENTED_EDGE('',*,*,#10105,.T.);
#13989=ORIENTED_EDGE('',*,*,#10106,.T.);
#13990=ORIENTED_EDGE('',*,*,#10107,.T.);
#13991=ORIENTED_EDGE('',*,*,#10108,.T.);
#13992=ORIENTED_EDGE('',*,*,#10109,.T.);
#13993=ORIENTED_EDGE('',*,*,#10110,.T.);
#13994=ORIENTED_EDGE('',*,*,#10111,.T.);
#13995=ORIENTED_EDGE('',*,*,#10112,.T.);
#13996=ORIENTED_EDGE('',*,*,#10113,.T.);
#13997=ORIENTED_EDGE('',*,*,#10114,.T.);
#13998=ORIENTED_EDGE('',*,*,#10115,.T.);
#13999=ORIENTED_EDGE('',*,*,#10116,.T.);
#14000=ORIENTED_EDGE('',*,*,#10117,.T.);
#14001=ORIENTED_EDGE('',*,*,#10118,.T.);
#14002=ORIENTED_EDGE('',*,*,#10119,.T.);
#14003=ORIENTED_EDGE('',*,*,#10120,.T.);
#14004=ORIENTED_EDGE('',*,*,#10121,.T.);
#14005=ORIENTED_EDGE('',*,*,#10122,.T.);
#14006=ORIENTED_EDGE('',*,*,#10123,.T.);
#14007=ORIENTED_EDGE('',*,*,#10124,.T.);
#14008=ORIENTED_EDGE('',*,*,#10125,.T.);
#14009=ORIENTED_EDGE('',*,*,#10126,.T.);
#14010=ORIENTED_EDGE('',*,*,#10127,.T.);
#14011=ORIENTED_EDGE('',*,*,#10128,.T.);
#14012=ORIENTED_EDGE('',*,*,#10129,.T.);
#14013=ORIENTED_EDGE('',*,*,#10130,.T.);
#14014=ORIENTED_EDGE('',*,*,#10131,.T.);
#14015=ORIENTED_EDGE('',*,*,#10132,.T.);
#14016=ORIENTED_EDGE('',*,*,#10133,.T.);
#14017=ORIENTED_EDGE('',*,*,#10134,.T.);
#14018=ORIENTED_EDGE('',*,*,#10135,.T.);
#14019=ORIENTED_EDGE('',*,*,#10136,.T.);
#14020=ORIENTED_EDGE('',*,*,#10137,.T.);
#14021=ORIENTED_EDGE('',*,*,#10138,.T.);
#14022=ORIENTED_EDGE('',*,*,#10139,.T.);
#14023=ORIENTED_EDGE('',*,*,#10140,.T.);
#14024=ORIENTED_EDGE('',*,*,#10141,.T.);
#14025=ORIENTED_EDGE('',*,*,#10142,.T.);
#14026=ORIENTED_EDGE('',*,*,#10143,.T.);
#14027=ORIENTED_EDGE('',*,*,#10144,.T.);
#14028=ORIENTED_EDGE('',*,*,#10145,.T.);
#14029=ORIENTED_EDGE('',*,*,#10146,.T.);
#14030=ORIENTED_EDGE('',*,*,#10147,.T.);
#14031=ORIENTED_EDGE('',*,*,#10148,.T.);
#14032=ORIENTED_EDGE('',*,*,#10149,.T.);
#14033=ORIENTED_EDGE('',*,*,#10150,.T.);
#14034=ORIENTED_EDGE('',*,*,#10151,.T.);
#14035=ORIENTED_EDGE('',*,*,#10152,.T.);
#14036=ORIENTED_EDGE('',*,*,#10153,.T.);
#14037=ORIENTED_EDGE('',*,*,#10154,.T.);
#14038=ORIENTED_EDGE('',*,*,#10155,.T.);
#14039=ORIENTED_EDGE('',*,*,#10156,.T.);
#14040=ORIENTED_EDGE('',*,*,#10157,.T.);
#14041=ORIENTED_EDGE('',*,*,#9990,.T.);
#14042=ORIENTED_EDGE('',*,*,#9994,.T.);
#14043=ORIENTED_EDGE('',*,*,#9997,.T.);
#14044=ORIENTED_EDGE('',*,*,#10158,.T.);
#14045=ORIENTED_EDGE('',*,*,#9991,.T.);
#14046=ORIENTED_EDGE('',*,*,#10158,.F.);
#14047=ORIENTED_EDGE('',*,*,#9996,.T.);
#14048=ORIENTED_EDGE('',*,*,#10159,.F.);
#14049=ORIENTED_EDGE('',*,*,#10160,.F.);
#14050=ORIENTED_EDGE('',*,*,#10161,.T.);
#14051=ORIENTED_EDGE('',*,*,#10162,.F.);
#14052=ORIENTED_EDGE('',*,*,#10161,.F.);
#14053=ORIENTED_EDGE('',*,*,#10160,.T.);
#14054=ORIENTED_EDGE('',*,*,#9988,.T.);
#14055=ORIENTED_EDGE('',*,*,#10159,.T.);
#14056=ORIENTED_EDGE('',*,*,#9995,.T.);
#14057=ORIENTED_EDGE('',*,*,#9992,.T.);
#14058=ORIENTED_EDGE('',*,*,#10163,.F.);
#14059=ORIENTED_EDGE('',*,*,#10164,.F.);
#14060=ORIENTED_EDGE('',*,*,#10165,.F.);
#14061=ORIENTED_EDGE('',*,*,#10155,.F.);
#14062=ORIENTED_EDGE('',*,*,#10166,.F.);
#14063=ORIENTED_EDGE('',*,*,#10157,.F.);
#14064=ORIENTED_EDGE('',*,*,#10167,.T.);
#14065=ORIENTED_EDGE('',*,*,#10168,.F.);
#14066=ORIENTED_EDGE('',*,*,#10165,.T.);
#14067=ORIENTED_EDGE('',*,*,#10169,.F.);
#14068=ORIENTED_EDGE('',*,*,#10167,.F.);
#14069=ORIENTED_EDGE('',*,*,#10156,.F.);
#14070=ORIENTED_EDGE('',*,*,#10166,.T.);
#14071=ORIENTED_EDGE('',*,*,#10170,.F.);
#14072=ORIENTED_EDGE('',*,*,#10171,.T.);
#14073=ORIENTED_EDGE('',*,*,#9998,.F.);
#14074=ORIENTED_EDGE('',*,*,#10171,.F.);
#14075=ORIENTED_EDGE('',*,*,#10172,.F.);
#14076=ORIENTED_EDGE('',*,*,#10173,.F.);
#14077=ORIENTED_EDGE('',*,*,#9999,.F.);
#14078=ORIENTED_EDGE('',*,*,#10174,.F.);
#14079=ORIENTED_EDGE('',*,*,#10001,.F.);
#14080=ORIENTED_EDGE('',*,*,#10175,.T.);
#14081=ORIENTED_EDGE('',*,*,#10176,.F.);
#14082=ORIENTED_EDGE('',*,*,#10173,.T.);
#14083=ORIENTED_EDGE('',*,*,#10177,.F.);
#14084=ORIENTED_EDGE('',*,*,#10175,.F.);
#14085=ORIENTED_EDGE('',*,*,#10000,.F.);
#14086=ORIENTED_EDGE('',*,*,#10174,.T.);
#14087=ORIENTED_EDGE('',*,*,#10178,.F.);
#14088=ORIENTED_EDGE('',*,*,#10179,.T.);
#14089=ORIENTED_EDGE('',*,*,#10002,.F.);
#14090=ORIENTED_EDGE('',*,*,#10179,.F.);
#14091=ORIENTED_EDGE('',*,*,#10180,.F.);
#14092=ORIENTED_EDGE('',*,*,#10181,.F.);
#14093=ORIENTED_EDGE('',*,*,#10003,.F.);
#14094=ORIENTED_EDGE('',*,*,#10182,.F.);
#14095=ORIENTED_EDGE('',*,*,#10005,.F.);
#14096=ORIENTED_EDGE('',*,*,#10183,.T.);
#14097=ORIENTED_EDGE('',*,*,#10184,.F.);
#14098=ORIENTED_EDGE('',*,*,#10181,.T.);
#14099=ORIENTED_EDGE('',*,*,#10185,.F.);
#14100=ORIENTED_EDGE('',*,*,#10183,.F.);
#14101=ORIENTED_EDGE('',*,*,#10004,.F.);
#14102=ORIENTED_EDGE('',*,*,#10182,.T.);
#14103=ORIENTED_EDGE('',*,*,#10186,.F.);
#14104=ORIENTED_EDGE('',*,*,#10187,.T.);
#14105=ORIENTED_EDGE('',*,*,#10006,.F.);
#14106=ORIENTED_EDGE('',*,*,#10187,.F.);
#14107=ORIENTED_EDGE('',*,*,#10188,.F.);
#14108=ORIENTED_EDGE('',*,*,#10189,.F.);
#14109=ORIENTED_EDGE('',*,*,#10007,.F.);
#14110=ORIENTED_EDGE('',*,*,#10190,.F.);
#14111=ORIENTED_EDGE('',*,*,#10009,.F.);
#14112=ORIENTED_EDGE('',*,*,#10191,.T.);
#14113=ORIENTED_EDGE('',*,*,#10192,.F.);
#14114=ORIENTED_EDGE('',*,*,#10189,.T.);
#14115=ORIENTED_EDGE('',*,*,#10193,.F.);
#14116=ORIENTED_EDGE('',*,*,#10191,.F.);
#14117=ORIENTED_EDGE('',*,*,#10008,.F.);
#14118=ORIENTED_EDGE('',*,*,#10190,.T.);
#14119=ORIENTED_EDGE('',*,*,#10194,.F.);
#14120=ORIENTED_EDGE('',*,*,#10195,.T.);
#14121=ORIENTED_EDGE('',*,*,#10010,.F.);
#14122=ORIENTED_EDGE('',*,*,#10195,.F.);
#14123=ORIENTED_EDGE('',*,*,#10196,.F.);
#14124=ORIENTED_EDGE('',*,*,#10197,.F.);
#14125=ORIENTED_EDGE('',*,*,#10011,.F.);
#14126=ORIENTED_EDGE('',*,*,#10198,.F.);
#14127=ORIENTED_EDGE('',*,*,#10013,.F.);
#14128=ORIENTED_EDGE('',*,*,#10199,.T.);
#14129=ORIENTED_EDGE('',*,*,#10200,.F.);
#14130=ORIENTED_EDGE('',*,*,#10197,.T.);
#14131=ORIENTED_EDGE('',*,*,#10201,.F.);
#14132=ORIENTED_EDGE('',*,*,#10199,.F.);
#14133=ORIENTED_EDGE('',*,*,#10012,.F.);
#14134=ORIENTED_EDGE('',*,*,#10198,.T.);
#14135=ORIENTED_EDGE('',*,*,#10202,.F.);
#14136=ORIENTED_EDGE('',*,*,#10203,.T.);
#14137=ORIENTED_EDGE('',*,*,#10014,.F.);
#14138=ORIENTED_EDGE('',*,*,#10203,.F.);
#14139=ORIENTED_EDGE('',*,*,#10204,.F.);
#14140=ORIENTED_EDGE('',*,*,#10205,.F.);
#14141=ORIENTED_EDGE('',*,*,#10015,.F.);
#14142=ORIENTED_EDGE('',*,*,#10206,.F.);
#14143=ORIENTED_EDGE('',*,*,#10017,.F.);
#14144=ORIENTED_EDGE('',*,*,#10207,.T.);
#14145=ORIENTED_EDGE('',*,*,#10208,.F.);
#14146=ORIENTED_EDGE('',*,*,#10205,.T.);
#14147=ORIENTED_EDGE('',*,*,#10209,.F.);
#14148=ORIENTED_EDGE('',*,*,#10207,.F.);
#14149=ORIENTED_EDGE('',*,*,#10016,.F.);
#14150=ORIENTED_EDGE('',*,*,#10206,.T.);
#14151=ORIENTED_EDGE('',*,*,#10210,.F.);
#14152=ORIENTED_EDGE('',*,*,#10211,.T.);
#14153=ORIENTED_EDGE('',*,*,#10018,.F.);
#14154=ORIENTED_EDGE('',*,*,#10211,.F.);
#14155=ORIENTED_EDGE('',*,*,#10212,.F.);
#14156=ORIENTED_EDGE('',*,*,#10213,.F.);
#14157=ORIENTED_EDGE('',*,*,#10019,.F.);
#14158=ORIENTED_EDGE('',*,*,#10214,.F.);
#14159=ORIENTED_EDGE('',*,*,#10021,.F.);
#14160=ORIENTED_EDGE('',*,*,#10215,.T.);
#14161=ORIENTED_EDGE('',*,*,#10216,.F.);
#14162=ORIENTED_EDGE('',*,*,#10213,.T.);
#14163=ORIENTED_EDGE('',*,*,#10217,.F.);
#14164=ORIENTED_EDGE('',*,*,#10215,.F.);
#14165=ORIENTED_EDGE('',*,*,#10020,.F.);
#14166=ORIENTED_EDGE('',*,*,#10214,.T.);
#14167=ORIENTED_EDGE('',*,*,#10218,.F.);
#14168=ORIENTED_EDGE('',*,*,#10219,.T.);
#14169=ORIENTED_EDGE('',*,*,#10022,.F.);
#14170=ORIENTED_EDGE('',*,*,#10219,.F.);
#14171=ORIENTED_EDGE('',*,*,#10220,.F.);
#14172=ORIENTED_EDGE('',*,*,#10221,.F.);
#14173=ORIENTED_EDGE('',*,*,#10023,.F.);
#14174=ORIENTED_EDGE('',*,*,#10222,.F.);
#14175=ORIENTED_EDGE('',*,*,#10025,.F.);
#14176=ORIENTED_EDGE('',*,*,#10223,.T.);
#14177=ORIENTED_EDGE('',*,*,#10224,.F.);
#14178=ORIENTED_EDGE('',*,*,#10221,.T.);
#14179=ORIENTED_EDGE('',*,*,#10225,.F.);
#14180=ORIENTED_EDGE('',*,*,#10223,.F.);
#14181=ORIENTED_EDGE('',*,*,#10024,.F.);
#14182=ORIENTED_EDGE('',*,*,#10222,.T.);
#14183=ORIENTED_EDGE('',*,*,#10226,.F.);
#14184=ORIENTED_EDGE('',*,*,#10227,.T.);
#14185=ORIENTED_EDGE('',*,*,#10026,.F.);
#14186=ORIENTED_EDGE('',*,*,#10227,.F.);
#14187=ORIENTED_EDGE('',*,*,#10228,.F.);
#14188=ORIENTED_EDGE('',*,*,#10229,.F.);
#14189=ORIENTED_EDGE('',*,*,#10027,.F.);
#14190=ORIENTED_EDGE('',*,*,#10230,.F.);
#14191=ORIENTED_EDGE('',*,*,#10029,.F.);
#14192=ORIENTED_EDGE('',*,*,#10231,.T.);
#14193=ORIENTED_EDGE('',*,*,#10232,.F.);
#14194=ORIENTED_EDGE('',*,*,#10229,.T.);
#14195=ORIENTED_EDGE('',*,*,#10233,.F.);
#14196=ORIENTED_EDGE('',*,*,#10231,.F.);
#14197=ORIENTED_EDGE('',*,*,#10028,.F.);
#14198=ORIENTED_EDGE('',*,*,#10230,.T.);
#14199=ORIENTED_EDGE('',*,*,#10234,.F.);
#14200=ORIENTED_EDGE('',*,*,#10235,.T.);
#14201=ORIENTED_EDGE('',*,*,#10030,.F.);
#14202=ORIENTED_EDGE('',*,*,#10235,.F.);
#14203=ORIENTED_EDGE('',*,*,#10236,.F.);
#14204=ORIENTED_EDGE('',*,*,#10237,.F.);
#14205=ORIENTED_EDGE('',*,*,#10031,.F.);
#14206=ORIENTED_EDGE('',*,*,#10238,.F.);
#14207=ORIENTED_EDGE('',*,*,#10033,.F.);
#14208=ORIENTED_EDGE('',*,*,#10239,.T.);
#14209=ORIENTED_EDGE('',*,*,#10240,.F.);
#14210=ORIENTED_EDGE('',*,*,#10237,.T.);
#14211=ORIENTED_EDGE('',*,*,#10241,.F.);
#14212=ORIENTED_EDGE('',*,*,#10239,.F.);
#14213=ORIENTED_EDGE('',*,*,#10032,.F.);
#14214=ORIENTED_EDGE('',*,*,#10238,.T.);
#14215=ORIENTED_EDGE('',*,*,#10242,.F.);
#14216=ORIENTED_EDGE('',*,*,#10243,.T.);
#14217=ORIENTED_EDGE('',*,*,#10034,.F.);
#14218=ORIENTED_EDGE('',*,*,#10243,.F.);
#14219=ORIENTED_EDGE('',*,*,#10244,.F.);
#14220=ORIENTED_EDGE('',*,*,#10245,.F.);
#14221=ORIENTED_EDGE('',*,*,#10035,.F.);
#14222=ORIENTED_EDGE('',*,*,#10246,.F.);
#14223=ORIENTED_EDGE('',*,*,#10037,.F.);
#14224=ORIENTED_EDGE('',*,*,#10247,.T.);
#14225=ORIENTED_EDGE('',*,*,#10248,.F.);
#14226=ORIENTED_EDGE('',*,*,#10245,.T.);
#14227=ORIENTED_EDGE('',*,*,#10249,.F.);
#14228=ORIENTED_EDGE('',*,*,#10247,.F.);
#14229=ORIENTED_EDGE('',*,*,#10036,.F.);
#14230=ORIENTED_EDGE('',*,*,#10246,.T.);
#14231=ORIENTED_EDGE('',*,*,#10250,.F.);
#14232=ORIENTED_EDGE('',*,*,#10251,.T.);
#14233=ORIENTED_EDGE('',*,*,#10038,.F.);
#14234=ORIENTED_EDGE('',*,*,#10251,.F.);
#14235=ORIENTED_EDGE('',*,*,#10252,.F.);
#14236=ORIENTED_EDGE('',*,*,#10253,.F.);
#14237=ORIENTED_EDGE('',*,*,#10039,.F.);
#14238=ORIENTED_EDGE('',*,*,#10254,.F.);
#14239=ORIENTED_EDGE('',*,*,#10041,.F.);
#14240=ORIENTED_EDGE('',*,*,#10255,.T.);
#14241=ORIENTED_EDGE('',*,*,#10256,.F.);
#14242=ORIENTED_EDGE('',*,*,#10253,.T.);
#14243=ORIENTED_EDGE('',*,*,#10257,.F.);
#14244=ORIENTED_EDGE('',*,*,#10255,.F.);
#14245=ORIENTED_EDGE('',*,*,#10040,.F.);
#14246=ORIENTED_EDGE('',*,*,#10254,.T.);
#14247=ORIENTED_EDGE('',*,*,#10258,.F.);
#14248=ORIENTED_EDGE('',*,*,#10259,.T.);
#14249=ORIENTED_EDGE('',*,*,#10042,.F.);
#14250=ORIENTED_EDGE('',*,*,#10259,.F.);
#14251=ORIENTED_EDGE('',*,*,#10260,.F.);
#14252=ORIENTED_EDGE('',*,*,#10261,.F.);
#14253=ORIENTED_EDGE('',*,*,#10043,.F.);
#14254=ORIENTED_EDGE('',*,*,#10262,.F.);
#14255=ORIENTED_EDGE('',*,*,#10045,.F.);
#14256=ORIENTED_EDGE('',*,*,#10263,.T.);
#14257=ORIENTED_EDGE('',*,*,#10264,.F.);
#14258=ORIENTED_EDGE('',*,*,#10261,.T.);
#14259=ORIENTED_EDGE('',*,*,#10265,.F.);
#14260=ORIENTED_EDGE('',*,*,#10263,.F.);
#14261=ORIENTED_EDGE('',*,*,#10044,.F.);
#14262=ORIENTED_EDGE('',*,*,#10262,.T.);
#14263=ORIENTED_EDGE('',*,*,#10266,.F.);
#14264=ORIENTED_EDGE('',*,*,#10267,.T.);
#14265=ORIENTED_EDGE('',*,*,#10046,.F.);
#14266=ORIENTED_EDGE('',*,*,#10267,.F.);
#14267=ORIENTED_EDGE('',*,*,#10268,.F.);
#14268=ORIENTED_EDGE('',*,*,#10269,.F.);
#14269=ORIENTED_EDGE('',*,*,#10047,.F.);
#14270=ORIENTED_EDGE('',*,*,#10270,.F.);
#14271=ORIENTED_EDGE('',*,*,#10049,.F.);
#14272=ORIENTED_EDGE('',*,*,#10271,.T.);
#14273=ORIENTED_EDGE('',*,*,#10272,.F.);
#14274=ORIENTED_EDGE('',*,*,#10269,.T.);
#14275=ORIENTED_EDGE('',*,*,#10273,.F.);
#14276=ORIENTED_EDGE('',*,*,#10271,.F.);
#14277=ORIENTED_EDGE('',*,*,#10048,.F.);
#14278=ORIENTED_EDGE('',*,*,#10270,.T.);
#14279=ORIENTED_EDGE('',*,*,#10274,.F.);
#14280=ORIENTED_EDGE('',*,*,#10275,.T.);
#14281=ORIENTED_EDGE('',*,*,#10050,.F.);
#14282=ORIENTED_EDGE('',*,*,#10275,.F.);
#14283=ORIENTED_EDGE('',*,*,#10276,.F.);
#14284=ORIENTED_EDGE('',*,*,#10277,.F.);
#14285=ORIENTED_EDGE('',*,*,#10051,.F.);
#14286=ORIENTED_EDGE('',*,*,#10278,.F.);
#14287=ORIENTED_EDGE('',*,*,#10053,.F.);
#14288=ORIENTED_EDGE('',*,*,#10279,.T.);
#14289=ORIENTED_EDGE('',*,*,#10280,.F.);
#14290=ORIENTED_EDGE('',*,*,#10277,.T.);
#14291=ORIENTED_EDGE('',*,*,#10281,.F.);
#14292=ORIENTED_EDGE('',*,*,#10279,.F.);
#14293=ORIENTED_EDGE('',*,*,#10052,.F.);
#14294=ORIENTED_EDGE('',*,*,#10278,.T.);
#14295=ORIENTED_EDGE('',*,*,#10282,.F.);
#14296=ORIENTED_EDGE('',*,*,#10283,.T.);
#14297=ORIENTED_EDGE('',*,*,#10054,.F.);
#14298=ORIENTED_EDGE('',*,*,#10283,.F.);
#14299=ORIENTED_EDGE('',*,*,#10284,.F.);
#14300=ORIENTED_EDGE('',*,*,#10285,.F.);
#14301=ORIENTED_EDGE('',*,*,#10055,.F.);
#14302=ORIENTED_EDGE('',*,*,#10286,.F.);
#14303=ORIENTED_EDGE('',*,*,#10057,.F.);
#14304=ORIENTED_EDGE('',*,*,#10287,.T.);
#14305=ORIENTED_EDGE('',*,*,#10288,.F.);
#14306=ORIENTED_EDGE('',*,*,#10285,.T.);
#14307=ORIENTED_EDGE('',*,*,#10289,.F.);
#14308=ORIENTED_EDGE('',*,*,#10287,.F.);
#14309=ORIENTED_EDGE('',*,*,#10056,.F.);
#14310=ORIENTED_EDGE('',*,*,#10286,.T.);
#14311=ORIENTED_EDGE('',*,*,#10290,.F.);
#14312=ORIENTED_EDGE('',*,*,#10291,.T.);
#14313=ORIENTED_EDGE('',*,*,#10058,.F.);
#14314=ORIENTED_EDGE('',*,*,#10291,.F.);
#14315=ORIENTED_EDGE('',*,*,#10292,.F.);
#14316=ORIENTED_EDGE('',*,*,#10293,.F.);
#14317=ORIENTED_EDGE('',*,*,#10059,.F.);
#14318=ORIENTED_EDGE('',*,*,#10294,.F.);
#14319=ORIENTED_EDGE('',*,*,#10061,.F.);
#14320=ORIENTED_EDGE('',*,*,#10295,.T.);
#14321=ORIENTED_EDGE('',*,*,#10296,.F.);
#14322=ORIENTED_EDGE('',*,*,#10293,.T.);
#14323=ORIENTED_EDGE('',*,*,#10297,.F.);
#14324=ORIENTED_EDGE('',*,*,#10295,.F.);
#14325=ORIENTED_EDGE('',*,*,#10060,.F.);
#14326=ORIENTED_EDGE('',*,*,#10294,.T.);
#14327=ORIENTED_EDGE('',*,*,#10298,.F.);
#14328=ORIENTED_EDGE('',*,*,#10299,.T.);
#14329=ORIENTED_EDGE('',*,*,#10062,.F.);
#14330=ORIENTED_EDGE('',*,*,#10299,.F.);
#14331=ORIENTED_EDGE('',*,*,#10300,.F.);
#14332=ORIENTED_EDGE('',*,*,#10301,.F.);
#14333=ORIENTED_EDGE('',*,*,#10063,.F.);
#14334=ORIENTED_EDGE('',*,*,#10302,.F.);
#14335=ORIENTED_EDGE('',*,*,#10065,.F.);
#14336=ORIENTED_EDGE('',*,*,#10303,.T.);
#14337=ORIENTED_EDGE('',*,*,#10304,.F.);
#14338=ORIENTED_EDGE('',*,*,#10301,.T.);
#14339=ORIENTED_EDGE('',*,*,#10305,.F.);
#14340=ORIENTED_EDGE('',*,*,#10303,.F.);
#14341=ORIENTED_EDGE('',*,*,#10064,.F.);
#14342=ORIENTED_EDGE('',*,*,#10302,.T.);
#14343=ORIENTED_EDGE('',*,*,#10306,.F.);
#14344=ORIENTED_EDGE('',*,*,#10307,.T.);
#14345=ORIENTED_EDGE('',*,*,#10066,.F.);
#14346=ORIENTED_EDGE('',*,*,#10307,.F.);
#14347=ORIENTED_EDGE('',*,*,#10308,.F.);
#14348=ORIENTED_EDGE('',*,*,#10309,.F.);
#14349=ORIENTED_EDGE('',*,*,#10067,.F.);
#14350=ORIENTED_EDGE('',*,*,#10310,.F.);
#14351=ORIENTED_EDGE('',*,*,#10069,.F.);
#14352=ORIENTED_EDGE('',*,*,#10311,.T.);
#14353=ORIENTED_EDGE('',*,*,#10312,.F.);
#14354=ORIENTED_EDGE('',*,*,#10309,.T.);
#14355=ORIENTED_EDGE('',*,*,#10313,.F.);
#14356=ORIENTED_EDGE('',*,*,#10311,.F.);
#14357=ORIENTED_EDGE('',*,*,#10068,.F.);
#14358=ORIENTED_EDGE('',*,*,#10310,.T.);
#14359=ORIENTED_EDGE('',*,*,#10314,.F.);
#14360=ORIENTED_EDGE('',*,*,#10315,.T.);
#14361=ORIENTED_EDGE('',*,*,#10070,.F.);
#14362=ORIENTED_EDGE('',*,*,#10315,.F.);
#14363=ORIENTED_EDGE('',*,*,#10316,.F.);
#14364=ORIENTED_EDGE('',*,*,#10317,.F.);
#14365=ORIENTED_EDGE('',*,*,#10071,.F.);
#14366=ORIENTED_EDGE('',*,*,#10318,.F.);
#14367=ORIENTED_EDGE('',*,*,#10073,.F.);
#14368=ORIENTED_EDGE('',*,*,#10319,.T.);
#14369=ORIENTED_EDGE('',*,*,#10320,.F.);
#14370=ORIENTED_EDGE('',*,*,#10317,.T.);
#14371=ORIENTED_EDGE('',*,*,#10321,.F.);
#14372=ORIENTED_EDGE('',*,*,#10319,.F.);
#14373=ORIENTED_EDGE('',*,*,#10072,.F.);
#14374=ORIENTED_EDGE('',*,*,#10318,.T.);
#14375=ORIENTED_EDGE('',*,*,#10322,.F.);
#14376=ORIENTED_EDGE('',*,*,#10323,.T.);
#14377=ORIENTED_EDGE('',*,*,#10074,.F.);
#14378=ORIENTED_EDGE('',*,*,#10323,.F.);
#14379=ORIENTED_EDGE('',*,*,#10324,.F.);
#14380=ORIENTED_EDGE('',*,*,#10325,.F.);
#14381=ORIENTED_EDGE('',*,*,#10075,.F.);
#14382=ORIENTED_EDGE('',*,*,#10326,.F.);
#14383=ORIENTED_EDGE('',*,*,#10077,.F.);
#14384=ORIENTED_EDGE('',*,*,#10327,.T.);
#14385=ORIENTED_EDGE('',*,*,#10328,.F.);
#14386=ORIENTED_EDGE('',*,*,#10325,.T.);
#14387=ORIENTED_EDGE('',*,*,#10329,.F.);
#14388=ORIENTED_EDGE('',*,*,#10327,.F.);
#14389=ORIENTED_EDGE('',*,*,#10076,.F.);
#14390=ORIENTED_EDGE('',*,*,#10326,.T.);
#14391=ORIENTED_EDGE('',*,*,#10330,.F.);
#14392=ORIENTED_EDGE('',*,*,#10331,.T.);
#14393=ORIENTED_EDGE('',*,*,#10078,.F.);
#14394=ORIENTED_EDGE('',*,*,#10331,.F.);
#14395=ORIENTED_EDGE('',*,*,#10332,.F.);
#14396=ORIENTED_EDGE('',*,*,#10333,.F.);
#14397=ORIENTED_EDGE('',*,*,#10079,.F.);
#14398=ORIENTED_EDGE('',*,*,#10334,.F.);
#14399=ORIENTED_EDGE('',*,*,#10081,.F.);
#14400=ORIENTED_EDGE('',*,*,#10335,.T.);
#14401=ORIENTED_EDGE('',*,*,#10336,.F.);
#14402=ORIENTED_EDGE('',*,*,#10333,.T.);
#14403=ORIENTED_EDGE('',*,*,#10337,.F.);
#14404=ORIENTED_EDGE('',*,*,#10335,.F.);
#14405=ORIENTED_EDGE('',*,*,#10080,.F.);
#14406=ORIENTED_EDGE('',*,*,#10334,.T.);
#14407=ORIENTED_EDGE('',*,*,#10338,.F.);
#14408=ORIENTED_EDGE('',*,*,#10339,.T.);
#14409=ORIENTED_EDGE('',*,*,#10082,.F.);
#14410=ORIENTED_EDGE('',*,*,#10339,.F.);
#14411=ORIENTED_EDGE('',*,*,#10340,.F.);
#14412=ORIENTED_EDGE('',*,*,#10341,.F.);
#14413=ORIENTED_EDGE('',*,*,#10083,.F.);
#14414=ORIENTED_EDGE('',*,*,#10342,.F.);
#14415=ORIENTED_EDGE('',*,*,#10085,.F.);
#14416=ORIENTED_EDGE('',*,*,#10343,.T.);
#14417=ORIENTED_EDGE('',*,*,#10344,.F.);
#14418=ORIENTED_EDGE('',*,*,#10341,.T.);
#14419=ORIENTED_EDGE('',*,*,#10345,.F.);
#14420=ORIENTED_EDGE('',*,*,#10343,.F.);
#14421=ORIENTED_EDGE('',*,*,#10084,.F.);
#14422=ORIENTED_EDGE('',*,*,#10342,.T.);
#14423=ORIENTED_EDGE('',*,*,#10346,.F.);
#14424=ORIENTED_EDGE('',*,*,#10347,.T.);
#14425=ORIENTED_EDGE('',*,*,#10086,.F.);
#14426=ORIENTED_EDGE('',*,*,#10347,.F.);
#14427=ORIENTED_EDGE('',*,*,#10348,.F.);
#14428=ORIENTED_EDGE('',*,*,#10349,.F.);
#14429=ORIENTED_EDGE('',*,*,#10087,.F.);
#14430=ORIENTED_EDGE('',*,*,#10350,.F.);
#14431=ORIENTED_EDGE('',*,*,#10089,.F.);
#14432=ORIENTED_EDGE('',*,*,#10351,.T.);
#14433=ORIENTED_EDGE('',*,*,#10352,.F.);
#14434=ORIENTED_EDGE('',*,*,#10349,.T.);
#14435=ORIENTED_EDGE('',*,*,#10353,.F.);
#14436=ORIENTED_EDGE('',*,*,#10351,.F.);
#14437=ORIENTED_EDGE('',*,*,#10088,.F.);
#14438=ORIENTED_EDGE('',*,*,#10350,.T.);
#14439=ORIENTED_EDGE('',*,*,#10354,.F.);
#14440=ORIENTED_EDGE('',*,*,#10355,.T.);
#14441=ORIENTED_EDGE('',*,*,#10090,.F.);
#14442=ORIENTED_EDGE('',*,*,#10355,.F.);
#14443=ORIENTED_EDGE('',*,*,#10356,.F.);
#14444=ORIENTED_EDGE('',*,*,#10357,.F.);
#14445=ORIENTED_EDGE('',*,*,#10091,.F.);
#14446=ORIENTED_EDGE('',*,*,#10358,.F.);
#14447=ORIENTED_EDGE('',*,*,#10093,.F.);
#14448=ORIENTED_EDGE('',*,*,#10359,.T.);
#14449=ORIENTED_EDGE('',*,*,#10360,.F.);
#14450=ORIENTED_EDGE('',*,*,#10357,.T.);
#14451=ORIENTED_EDGE('',*,*,#10361,.F.);
#14452=ORIENTED_EDGE('',*,*,#10359,.F.);
#14453=ORIENTED_EDGE('',*,*,#10092,.F.);
#14454=ORIENTED_EDGE('',*,*,#10358,.T.);
#14455=ORIENTED_EDGE('',*,*,#10362,.F.);
#14456=ORIENTED_EDGE('',*,*,#10363,.T.);
#14457=ORIENTED_EDGE('',*,*,#10094,.F.);
#14458=ORIENTED_EDGE('',*,*,#10363,.F.);
#14459=ORIENTED_EDGE('',*,*,#10364,.F.);
#14460=ORIENTED_EDGE('',*,*,#10365,.F.);
#14461=ORIENTED_EDGE('',*,*,#10095,.F.);
#14462=ORIENTED_EDGE('',*,*,#10366,.F.);
#14463=ORIENTED_EDGE('',*,*,#10097,.F.);
#14464=ORIENTED_EDGE('',*,*,#10367,.T.);
#14465=ORIENTED_EDGE('',*,*,#10368,.F.);
#14466=ORIENTED_EDGE('',*,*,#10365,.T.);
#14467=ORIENTED_EDGE('',*,*,#10369,.F.);
#14468=ORIENTED_EDGE('',*,*,#10367,.F.);
#14469=ORIENTED_EDGE('',*,*,#10096,.F.);
#14470=ORIENTED_EDGE('',*,*,#10366,.T.);
#14471=ORIENTED_EDGE('',*,*,#10370,.F.);
#14472=ORIENTED_EDGE('',*,*,#10371,.T.);
#14473=ORIENTED_EDGE('',*,*,#10098,.F.);
#14474=ORIENTED_EDGE('',*,*,#10371,.F.);
#14475=ORIENTED_EDGE('',*,*,#10372,.F.);
#14476=ORIENTED_EDGE('',*,*,#10373,.F.);
#14477=ORIENTED_EDGE('',*,*,#10099,.F.);
#14478=ORIENTED_EDGE('',*,*,#10374,.F.);
#14479=ORIENTED_EDGE('',*,*,#10101,.F.);
#14480=ORIENTED_EDGE('',*,*,#10375,.T.);
#14481=ORIENTED_EDGE('',*,*,#10376,.F.);
#14482=ORIENTED_EDGE('',*,*,#10373,.T.);
#14483=ORIENTED_EDGE('',*,*,#10377,.F.);
#14484=ORIENTED_EDGE('',*,*,#10375,.F.);
#14485=ORIENTED_EDGE('',*,*,#10100,.F.);
#14486=ORIENTED_EDGE('',*,*,#10374,.T.);
#14487=ORIENTED_EDGE('',*,*,#10378,.F.);
#14488=ORIENTED_EDGE('',*,*,#10379,.T.);
#14489=ORIENTED_EDGE('',*,*,#10102,.F.);
#14490=ORIENTED_EDGE('',*,*,#10379,.F.);
#14491=ORIENTED_EDGE('',*,*,#10380,.F.);
#14492=ORIENTED_EDGE('',*,*,#10381,.F.);
#14493=ORIENTED_EDGE('',*,*,#10103,.F.);
#14494=ORIENTED_EDGE('',*,*,#10382,.F.);
#14495=ORIENTED_EDGE('',*,*,#10105,.F.);
#14496=ORIENTED_EDGE('',*,*,#10383,.T.);
#14497=ORIENTED_EDGE('',*,*,#10384,.F.);
#14498=ORIENTED_EDGE('',*,*,#10381,.T.);
#14499=ORIENTED_EDGE('',*,*,#10385,.F.);
#14500=ORIENTED_EDGE('',*,*,#10383,.F.);
#14501=ORIENTED_EDGE('',*,*,#10104,.F.);
#14502=ORIENTED_EDGE('',*,*,#10382,.T.);
#14503=ORIENTED_EDGE('',*,*,#10386,.F.);
#14504=ORIENTED_EDGE('',*,*,#10387,.T.);
#14505=ORIENTED_EDGE('',*,*,#10106,.F.);
#14506=ORIENTED_EDGE('',*,*,#10387,.F.);
#14507=ORIENTED_EDGE('',*,*,#10388,.F.);
#14508=ORIENTED_EDGE('',*,*,#10389,.F.);
#14509=ORIENTED_EDGE('',*,*,#10107,.F.);
#14510=ORIENTED_EDGE('',*,*,#10390,.F.);
#14511=ORIENTED_EDGE('',*,*,#10109,.F.);
#14512=ORIENTED_EDGE('',*,*,#10391,.T.);
#14513=ORIENTED_EDGE('',*,*,#10392,.F.);
#14514=ORIENTED_EDGE('',*,*,#10389,.T.);
#14515=ORIENTED_EDGE('',*,*,#10393,.F.);
#14516=ORIENTED_EDGE('',*,*,#10391,.F.);
#14517=ORIENTED_EDGE('',*,*,#10108,.F.);
#14518=ORIENTED_EDGE('',*,*,#10390,.T.);
#14519=ORIENTED_EDGE('',*,*,#10394,.F.);
#14520=ORIENTED_EDGE('',*,*,#10395,.T.);
#14521=ORIENTED_EDGE('',*,*,#10110,.F.);
#14522=ORIENTED_EDGE('',*,*,#10395,.F.);
#14523=ORIENTED_EDGE('',*,*,#10396,.F.);
#14524=ORIENTED_EDGE('',*,*,#10397,.F.);
#14525=ORIENTED_EDGE('',*,*,#10111,.F.);
#14526=ORIENTED_EDGE('',*,*,#10398,.F.);
#14527=ORIENTED_EDGE('',*,*,#10113,.F.);
#14528=ORIENTED_EDGE('',*,*,#10399,.T.);
#14529=ORIENTED_EDGE('',*,*,#10400,.F.);
#14530=ORIENTED_EDGE('',*,*,#10397,.T.);
#14531=ORIENTED_EDGE('',*,*,#10401,.F.);
#14532=ORIENTED_EDGE('',*,*,#10399,.F.);
#14533=ORIENTED_EDGE('',*,*,#10112,.F.);
#14534=ORIENTED_EDGE('',*,*,#10398,.T.);
#14535=ORIENTED_EDGE('',*,*,#10402,.F.);
#14536=ORIENTED_EDGE('',*,*,#10403,.T.);
#14537=ORIENTED_EDGE('',*,*,#10114,.F.);
#14538=ORIENTED_EDGE('',*,*,#10403,.F.);
#14539=ORIENTED_EDGE('',*,*,#10404,.F.);
#14540=ORIENTED_EDGE('',*,*,#10405,.F.);
#14541=ORIENTED_EDGE('',*,*,#10115,.F.);
#14542=ORIENTED_EDGE('',*,*,#10406,.F.);
#14543=ORIENTED_EDGE('',*,*,#10117,.F.);
#14544=ORIENTED_EDGE('',*,*,#10407,.T.);
#14545=ORIENTED_EDGE('',*,*,#10408,.F.);
#14546=ORIENTED_EDGE('',*,*,#10405,.T.);
#14547=ORIENTED_EDGE('',*,*,#10409,.F.);
#14548=ORIENTED_EDGE('',*,*,#10407,.F.);
#14549=ORIENTED_EDGE('',*,*,#10116,.F.);
#14550=ORIENTED_EDGE('',*,*,#10406,.T.);
#14551=ORIENTED_EDGE('',*,*,#10410,.F.);
#14552=ORIENTED_EDGE('',*,*,#10411,.T.);
#14553=ORIENTED_EDGE('',*,*,#10118,.F.);
#14554=ORIENTED_EDGE('',*,*,#10411,.F.);
#14555=ORIENTED_EDGE('',*,*,#10412,.F.);
#14556=ORIENTED_EDGE('',*,*,#10413,.F.);
#14557=ORIENTED_EDGE('',*,*,#10119,.F.);
#14558=ORIENTED_EDGE('',*,*,#10414,.F.);
#14559=ORIENTED_EDGE('',*,*,#10121,.F.);
#14560=ORIENTED_EDGE('',*,*,#10415,.T.);
#14561=ORIENTED_EDGE('',*,*,#10416,.F.);
#14562=ORIENTED_EDGE('',*,*,#10413,.T.);
#14563=ORIENTED_EDGE('',*,*,#10417,.F.);
#14564=ORIENTED_EDGE('',*,*,#10415,.F.);
#14565=ORIENTED_EDGE('',*,*,#10120,.F.);
#14566=ORIENTED_EDGE('',*,*,#10414,.T.);
#14567=ORIENTED_EDGE('',*,*,#10418,.F.);
#14568=ORIENTED_EDGE('',*,*,#10419,.T.);
#14569=ORIENTED_EDGE('',*,*,#10122,.F.);
#14570=ORIENTED_EDGE('',*,*,#10419,.F.);
#14571=ORIENTED_EDGE('',*,*,#10420,.F.);
#14572=ORIENTED_EDGE('',*,*,#10421,.F.);
#14573=ORIENTED_EDGE('',*,*,#10123,.F.);
#14574=ORIENTED_EDGE('',*,*,#10422,.F.);
#14575=ORIENTED_EDGE('',*,*,#10125,.F.);
#14576=ORIENTED_EDGE('',*,*,#10423,.T.);
#14577=ORIENTED_EDGE('',*,*,#10424,.F.);
#14578=ORIENTED_EDGE('',*,*,#10421,.T.);
#14579=ORIENTED_EDGE('',*,*,#10425,.F.);
#14580=ORIENTED_EDGE('',*,*,#10423,.F.);
#14581=ORIENTED_EDGE('',*,*,#10124,.F.);
#14582=ORIENTED_EDGE('',*,*,#10422,.T.);
#14583=ORIENTED_EDGE('',*,*,#10426,.F.);
#14584=ORIENTED_EDGE('',*,*,#10427,.T.);
#14585=ORIENTED_EDGE('',*,*,#10126,.F.);
#14586=ORIENTED_EDGE('',*,*,#10427,.F.);
#14587=ORIENTED_EDGE('',*,*,#10428,.F.);
#14588=ORIENTED_EDGE('',*,*,#10429,.F.);
#14589=ORIENTED_EDGE('',*,*,#10127,.F.);
#14590=ORIENTED_EDGE('',*,*,#10430,.F.);
#14591=ORIENTED_EDGE('',*,*,#10129,.F.);
#14592=ORIENTED_EDGE('',*,*,#10431,.T.);
#14593=ORIENTED_EDGE('',*,*,#10432,.F.);
#14594=ORIENTED_EDGE('',*,*,#10429,.T.);
#14595=ORIENTED_EDGE('',*,*,#10433,.F.);
#14596=ORIENTED_EDGE('',*,*,#10431,.F.);
#14597=ORIENTED_EDGE('',*,*,#10128,.F.);
#14598=ORIENTED_EDGE('',*,*,#10430,.T.);
#14599=ORIENTED_EDGE('',*,*,#10434,.F.);
#14600=ORIENTED_EDGE('',*,*,#10435,.T.);
#14601=ORIENTED_EDGE('',*,*,#10130,.F.);
#14602=ORIENTED_EDGE('',*,*,#10435,.F.);
#14603=ORIENTED_EDGE('',*,*,#10436,.F.);
#14604=ORIENTED_EDGE('',*,*,#10437,.F.);
#14605=ORIENTED_EDGE('',*,*,#10131,.F.);
#14606=ORIENTED_EDGE('',*,*,#10438,.F.);
#14607=ORIENTED_EDGE('',*,*,#10133,.F.);
#14608=ORIENTED_EDGE('',*,*,#10439,.T.);
#14609=ORIENTED_EDGE('',*,*,#10440,.F.);
#14610=ORIENTED_EDGE('',*,*,#10437,.T.);
#14611=ORIENTED_EDGE('',*,*,#10441,.F.);
#14612=ORIENTED_EDGE('',*,*,#10439,.F.);
#14613=ORIENTED_EDGE('',*,*,#10132,.F.);
#14614=ORIENTED_EDGE('',*,*,#10438,.T.);
#14615=ORIENTED_EDGE('',*,*,#10442,.F.);
#14616=ORIENTED_EDGE('',*,*,#10443,.T.);
#14617=ORIENTED_EDGE('',*,*,#10134,.F.);
#14618=ORIENTED_EDGE('',*,*,#10443,.F.);
#14619=ORIENTED_EDGE('',*,*,#10444,.F.);
#14620=ORIENTED_EDGE('',*,*,#10445,.F.);
#14621=ORIENTED_EDGE('',*,*,#10135,.F.);
#14622=ORIENTED_EDGE('',*,*,#10446,.F.);
#14623=ORIENTED_EDGE('',*,*,#10137,.F.);
#14624=ORIENTED_EDGE('',*,*,#10447,.T.);
#14625=ORIENTED_EDGE('',*,*,#10448,.F.);
#14626=ORIENTED_EDGE('',*,*,#10445,.T.);
#14627=ORIENTED_EDGE('',*,*,#10449,.F.);
#14628=ORIENTED_EDGE('',*,*,#10447,.F.);
#14629=ORIENTED_EDGE('',*,*,#10136,.F.);
#14630=ORIENTED_EDGE('',*,*,#10446,.T.);
#14631=ORIENTED_EDGE('',*,*,#10450,.F.);
#14632=ORIENTED_EDGE('',*,*,#10451,.T.);
#14633=ORIENTED_EDGE('',*,*,#10138,.F.);
#14634=ORIENTED_EDGE('',*,*,#10451,.F.);
#14635=ORIENTED_EDGE('',*,*,#10452,.F.);
#14636=ORIENTED_EDGE('',*,*,#10453,.F.);
#14637=ORIENTED_EDGE('',*,*,#10139,.F.);
#14638=ORIENTED_EDGE('',*,*,#10454,.F.);
#14639=ORIENTED_EDGE('',*,*,#10141,.F.);
#14640=ORIENTED_EDGE('',*,*,#10455,.T.);
#14641=ORIENTED_EDGE('',*,*,#10456,.F.);
#14642=ORIENTED_EDGE('',*,*,#10453,.T.);
#14643=ORIENTED_EDGE('',*,*,#10457,.F.);
#14644=ORIENTED_EDGE('',*,*,#10455,.F.);
#14645=ORIENTED_EDGE('',*,*,#10140,.F.);
#14646=ORIENTED_EDGE('',*,*,#10454,.T.);
#14647=ORIENTED_EDGE('',*,*,#10458,.F.);
#14648=ORIENTED_EDGE('',*,*,#10459,.T.);
#14649=ORIENTED_EDGE('',*,*,#10142,.F.);
#14650=ORIENTED_EDGE('',*,*,#10459,.F.);
#14651=ORIENTED_EDGE('',*,*,#10460,.F.);
#14652=ORIENTED_EDGE('',*,*,#10461,.F.);
#14653=ORIENTED_EDGE('',*,*,#10143,.F.);
#14654=ORIENTED_EDGE('',*,*,#10462,.F.);
#14655=ORIENTED_EDGE('',*,*,#10145,.F.);
#14656=ORIENTED_EDGE('',*,*,#10463,.T.);
#14657=ORIENTED_EDGE('',*,*,#10464,.F.);
#14658=ORIENTED_EDGE('',*,*,#10461,.T.);
#14659=ORIENTED_EDGE('',*,*,#10465,.F.);
#14660=ORIENTED_EDGE('',*,*,#10463,.F.);
#14661=ORIENTED_EDGE('',*,*,#10144,.F.);
#14662=ORIENTED_EDGE('',*,*,#10462,.T.);
#14663=ORIENTED_EDGE('',*,*,#10466,.F.);
#14664=ORIENTED_EDGE('',*,*,#10467,.T.);
#14665=ORIENTED_EDGE('',*,*,#10146,.F.);
#14666=ORIENTED_EDGE('',*,*,#10467,.F.);
#14667=ORIENTED_EDGE('',*,*,#10468,.F.);
#14668=ORIENTED_EDGE('',*,*,#10469,.F.);
#14669=ORIENTED_EDGE('',*,*,#10147,.F.);
#14670=ORIENTED_EDGE('',*,*,#10469,.T.);
#14671=ORIENTED_EDGE('',*,*,#10470,.F.);
#14672=ORIENTED_EDGE('',*,*,#10471,.F.);
#14673=ORIENTED_EDGE('',*,*,#10148,.F.);
#14674=ORIENTED_EDGE('',*,*,#10472,.F.);
#14675=ORIENTED_EDGE('',*,*,#10149,.F.);
#14676=ORIENTED_EDGE('',*,*,#10471,.T.);
#14677=ORIENTED_EDGE('',*,*,#10473,.F.);
#14678=ORIENTED_EDGE('',*,*,#10472,.T.);
#14679=ORIENTED_EDGE('',*,*,#10474,.F.);
#14680=ORIENTED_EDGE('',*,*,#10475,.T.);
#14681=ORIENTED_EDGE('',*,*,#10150,.F.);
#14682=ORIENTED_EDGE('',*,*,#10476,.F.);
#14683=ORIENTED_EDGE('',*,*,#10153,.F.);
#14684=ORIENTED_EDGE('',*,*,#10477,.T.);
#14685=ORIENTED_EDGE('',*,*,#10478,.F.);
#14686=ORIENTED_EDGE('',*,*,#10475,.F.);
#14687=ORIENTED_EDGE('',*,*,#10479,.F.);
#14688=ORIENTED_EDGE('',*,*,#10480,.F.);
#14689=ORIENTED_EDGE('',*,*,#10151,.F.);
#14690=ORIENTED_EDGE('',*,*,#10480,.T.);
#14691=ORIENTED_EDGE('',*,*,#10481,.F.);
#14692=ORIENTED_EDGE('',*,*,#10477,.F.);
#14693=ORIENTED_EDGE('',*,*,#10152,.F.);
#14694=ORIENTED_EDGE('',*,*,#10168,.T.);
#14695=ORIENTED_EDGE('',*,*,#10169,.T.);
#14696=ORIENTED_EDGE('',*,*,#10164,.T.);
#14697=ORIENTED_EDGE('',*,*,#10482,.T.);
#14698=ORIENTED_EDGE('',*,*,#10478,.T.);
#14699=ORIENTED_EDGE('',*,*,#10481,.T.);
#14700=ORIENTED_EDGE('',*,*,#10479,.T.);
#14701=ORIENTED_EDGE('',*,*,#10474,.T.);
#14702=ORIENTED_EDGE('',*,*,#10473,.T.);
#14703=ORIENTED_EDGE('',*,*,#10470,.T.);
#14704=ORIENTED_EDGE('',*,*,#10468,.T.);
#14705=ORIENTED_EDGE('',*,*,#10466,.T.);
#14706=ORIENTED_EDGE('',*,*,#10464,.T.);
#14707=ORIENTED_EDGE('',*,*,#10465,.T.);
#14708=ORIENTED_EDGE('',*,*,#10460,.T.);
#14709=ORIENTED_EDGE('',*,*,#10458,.T.);
#14710=ORIENTED_EDGE('',*,*,#10456,.T.);
#14711=ORIENTED_EDGE('',*,*,#10457,.T.);
#14712=ORIENTED_EDGE('',*,*,#10452,.T.);
#14713=ORIENTED_EDGE('',*,*,#10450,.T.);
#14714=ORIENTED_EDGE('',*,*,#10448,.T.);
#14715=ORIENTED_EDGE('',*,*,#10449,.T.);
#14716=ORIENTED_EDGE('',*,*,#10444,.T.);
#14717=ORIENTED_EDGE('',*,*,#10442,.T.);
#14718=ORIENTED_EDGE('',*,*,#10440,.T.);
#14719=ORIENTED_EDGE('',*,*,#10441,.T.);
#14720=ORIENTED_EDGE('',*,*,#10436,.T.);
#14721=ORIENTED_EDGE('',*,*,#10434,.T.);
#14722=ORIENTED_EDGE('',*,*,#10432,.T.);
#14723=ORIENTED_EDGE('',*,*,#10433,.T.);
#14724=ORIENTED_EDGE('',*,*,#10428,.T.);
#14725=ORIENTED_EDGE('',*,*,#10426,.T.);
#14726=ORIENTED_EDGE('',*,*,#10424,.T.);
#14727=ORIENTED_EDGE('',*,*,#10425,.T.);
#14728=ORIENTED_EDGE('',*,*,#10420,.T.);
#14729=ORIENTED_EDGE('',*,*,#10418,.T.);
#14730=ORIENTED_EDGE('',*,*,#10416,.T.);
#14731=ORIENTED_EDGE('',*,*,#10417,.T.);
#14732=ORIENTED_EDGE('',*,*,#10412,.T.);
#14733=ORIENTED_EDGE('',*,*,#10410,.T.);
#14734=ORIENTED_EDGE('',*,*,#10408,.T.);
#14735=ORIENTED_EDGE('',*,*,#10409,.T.);
#14736=ORIENTED_EDGE('',*,*,#10404,.T.);
#14737=ORIENTED_EDGE('',*,*,#10402,.T.);
#14738=ORIENTED_EDGE('',*,*,#10400,.T.);
#14739=ORIENTED_EDGE('',*,*,#10401,.T.);
#14740=ORIENTED_EDGE('',*,*,#10396,.T.);
#14741=ORIENTED_EDGE('',*,*,#10394,.T.);
#14742=ORIENTED_EDGE('',*,*,#10392,.T.);
#14743=ORIENTED_EDGE('',*,*,#10393,.T.);
#14744=ORIENTED_EDGE('',*,*,#10388,.T.);
#14745=ORIENTED_EDGE('',*,*,#10386,.T.);
#14746=ORIENTED_EDGE('',*,*,#10384,.T.);
#14747=ORIENTED_EDGE('',*,*,#10385,.T.);
#14748=ORIENTED_EDGE('',*,*,#10380,.T.);
#14749=ORIENTED_EDGE('',*,*,#10378,.T.);
#14750=ORIENTED_EDGE('',*,*,#10376,.T.);
#14751=ORIENTED_EDGE('',*,*,#10377,.T.);
#14752=ORIENTED_EDGE('',*,*,#10372,.T.);
#14753=ORIENTED_EDGE('',*,*,#10370,.T.);
#14754=ORIENTED_EDGE('',*,*,#10368,.T.);
#14755=ORIENTED_EDGE('',*,*,#10369,.T.);
#14756=ORIENTED_EDGE('',*,*,#10364,.T.);
#14757=ORIENTED_EDGE('',*,*,#10362,.T.);
#14758=ORIENTED_EDGE('',*,*,#10360,.T.);
#14759=ORIENTED_EDGE('',*,*,#10361,.T.);
#14760=ORIENTED_EDGE('',*,*,#10356,.T.);
#14761=ORIENTED_EDGE('',*,*,#10354,.T.);
#14762=ORIENTED_EDGE('',*,*,#10352,.T.);
#14763=ORIENTED_EDGE('',*,*,#10353,.T.);
#14764=ORIENTED_EDGE('',*,*,#10348,.T.);
#14765=ORIENTED_EDGE('',*,*,#10346,.T.);
#14766=ORIENTED_EDGE('',*,*,#10344,.T.);
#14767=ORIENTED_EDGE('',*,*,#10345,.T.);
#14768=ORIENTED_EDGE('',*,*,#10340,.T.);
#14769=ORIENTED_EDGE('',*,*,#10338,.T.);
#14770=ORIENTED_EDGE('',*,*,#10336,.T.);
#14771=ORIENTED_EDGE('',*,*,#10337,.T.);
#14772=ORIENTED_EDGE('',*,*,#10332,.T.);
#14773=ORIENTED_EDGE('',*,*,#10330,.T.);
#14774=ORIENTED_EDGE('',*,*,#10328,.T.);
#14775=ORIENTED_EDGE('',*,*,#10329,.T.);
#14776=ORIENTED_EDGE('',*,*,#10324,.T.);
#14777=ORIENTED_EDGE('',*,*,#10322,.T.);
#14778=ORIENTED_EDGE('',*,*,#10320,.T.);
#14779=ORIENTED_EDGE('',*,*,#10321,.T.);
#14780=ORIENTED_EDGE('',*,*,#10316,.T.);
#14781=ORIENTED_EDGE('',*,*,#10314,.T.);
#14782=ORIENTED_EDGE('',*,*,#10312,.T.);
#14783=ORIENTED_EDGE('',*,*,#10313,.T.);
#14784=ORIENTED_EDGE('',*,*,#10308,.T.);
#14785=ORIENTED_EDGE('',*,*,#10306,.T.);
#14786=ORIENTED_EDGE('',*,*,#10304,.T.);
#14787=ORIENTED_EDGE('',*,*,#10305,.T.);
#14788=ORIENTED_EDGE('',*,*,#10300,.T.);
#14789=ORIENTED_EDGE('',*,*,#10298,.T.);
#14790=ORIENTED_EDGE('',*,*,#10296,.T.);
#14791=ORIENTED_EDGE('',*,*,#10297,.T.);
#14792=ORIENTED_EDGE('',*,*,#10292,.T.);
#14793=ORIENTED_EDGE('',*,*,#10290,.T.);
#14794=ORIENTED_EDGE('',*,*,#10288,.T.);
#14795=ORIENTED_EDGE('',*,*,#10289,.T.);
#14796=ORIENTED_EDGE('',*,*,#10284,.T.);
#14797=ORIENTED_EDGE('',*,*,#10282,.T.);
#14798=ORIENTED_EDGE('',*,*,#10280,.T.);
#14799=ORIENTED_EDGE('',*,*,#10281,.T.);
#14800=ORIENTED_EDGE('',*,*,#10276,.T.);
#14801=ORIENTED_EDGE('',*,*,#10274,.T.);
#14802=ORIENTED_EDGE('',*,*,#10272,.T.);
#14803=ORIENTED_EDGE('',*,*,#10273,.T.);
#14804=ORIENTED_EDGE('',*,*,#10268,.T.);
#14805=ORIENTED_EDGE('',*,*,#10266,.T.);
#14806=ORIENTED_EDGE('',*,*,#10264,.T.);
#14807=ORIENTED_EDGE('',*,*,#10265,.T.);
#14808=ORIENTED_EDGE('',*,*,#10260,.T.);
#14809=ORIENTED_EDGE('',*,*,#10258,.T.);
#14810=ORIENTED_EDGE('',*,*,#10256,.T.);
#14811=ORIENTED_EDGE('',*,*,#10257,.T.);
#14812=ORIENTED_EDGE('',*,*,#10252,.T.);
#14813=ORIENTED_EDGE('',*,*,#10250,.T.);
#14814=ORIENTED_EDGE('',*,*,#10248,.T.);
#14815=ORIENTED_EDGE('',*,*,#10249,.T.);
#14816=ORIENTED_EDGE('',*,*,#10244,.T.);
#14817=ORIENTED_EDGE('',*,*,#10242,.T.);
#14818=ORIENTED_EDGE('',*,*,#10240,.T.);
#14819=ORIENTED_EDGE('',*,*,#10241,.T.);
#14820=ORIENTED_EDGE('',*,*,#10236,.T.);
#14821=ORIENTED_EDGE('',*,*,#10234,.T.);
#14822=ORIENTED_EDGE('',*,*,#10232,.T.);
#14823=ORIENTED_EDGE('',*,*,#10233,.T.);
#14824=ORIENTED_EDGE('',*,*,#10228,.T.);
#14825=ORIENTED_EDGE('',*,*,#10226,.T.);
#14826=ORIENTED_EDGE('',*,*,#10224,.T.);
#14827=ORIENTED_EDGE('',*,*,#10225,.T.);
#14828=ORIENTED_EDGE('',*,*,#10220,.T.);
#14829=ORIENTED_EDGE('',*,*,#10218,.T.);
#14830=ORIENTED_EDGE('',*,*,#10216,.T.);
#14831=ORIENTED_EDGE('',*,*,#10217,.T.);
#14832=ORIENTED_EDGE('',*,*,#10212,.T.);
#14833=ORIENTED_EDGE('',*,*,#10210,.T.);
#14834=ORIENTED_EDGE('',*,*,#10208,.T.);
#14835=ORIENTED_EDGE('',*,*,#10209,.T.);
#14836=ORIENTED_EDGE('',*,*,#10204,.T.);
#14837=ORIENTED_EDGE('',*,*,#10202,.T.);
#14838=ORIENTED_EDGE('',*,*,#10200,.T.);
#14839=ORIENTED_EDGE('',*,*,#10201,.T.);
#14840=ORIENTED_EDGE('',*,*,#10196,.T.);
#14841=ORIENTED_EDGE('',*,*,#10194,.T.);
#14842=ORIENTED_EDGE('',*,*,#10192,.T.);
#14843=ORIENTED_EDGE('',*,*,#10193,.T.);
#14844=ORIENTED_EDGE('',*,*,#10188,.T.);
#14845=ORIENTED_EDGE('',*,*,#10186,.T.);
#14846=ORIENTED_EDGE('',*,*,#10184,.T.);
#14847=ORIENTED_EDGE('',*,*,#10185,.T.);
#14848=ORIENTED_EDGE('',*,*,#10180,.T.);
#14849=ORIENTED_EDGE('',*,*,#10178,.T.);
#14850=ORIENTED_EDGE('',*,*,#10176,.T.);
#14851=ORIENTED_EDGE('',*,*,#10177,.T.);
#14852=ORIENTED_EDGE('',*,*,#10172,.T.);
#14853=ORIENTED_EDGE('',*,*,#10170,.T.);
#14854=ORIENTED_EDGE('',*,*,#10162,.T.);
#14855=ORIENTED_EDGE('',*,*,#10163,.T.);
#14856=ORIENTED_EDGE('',*,*,#10154,.F.);
#14857=ORIENTED_EDGE('',*,*,#10476,.T.);
#14858=ORIENTED_EDGE('',*,*,#10482,.F.);
#14859=ORIENTED_EDGE('',*,*,#10483,.F.);
#14860=ORIENTED_EDGE('',*,*,#10484,.F.);
#14861=ORIENTED_EDGE('',*,*,#10485,.F.);
#14862=ORIENTED_EDGE('',*,*,#10486,.F.);
#14863=ORIENTED_EDGE('',*,*,#10487,.F.);
#14864=ORIENTED_EDGE('',*,*,#10488,.F.);
#14865=ORIENTED_EDGE('',*,*,#10489,.F.);
#14866=ORIENTED_EDGE('',*,*,#10490,.F.);
#14867=ORIENTED_EDGE('',*,*,#10487,.T.);
#14868=ORIENTED_EDGE('',*,*,#10491,.T.);
#14869=ORIENTED_EDGE('',*,*,#10492,.T.);
#14870=ORIENTED_EDGE('',*,*,#10493,.T.);
#14871=ORIENTED_EDGE('',*,*,#10486,.T.);
#14872=ORIENTED_EDGE('',*,*,#10494,.F.);
#14873=ORIENTED_EDGE('',*,*,#10495,.T.);
#14874=ORIENTED_EDGE('',*,*,#10491,.F.);
#14875=ORIENTED_EDGE('',*,*,#10485,.T.);
#14876=ORIENTED_EDGE('',*,*,#10496,.T.);
#14877=ORIENTED_EDGE('',*,*,#10497,.T.);
#14878=ORIENTED_EDGE('',*,*,#10494,.T.);
#14879=ORIENTED_EDGE('',*,*,#10484,.T.);
#14880=ORIENTED_EDGE('',*,*,#10498,.F.);
#14881=ORIENTED_EDGE('',*,*,#10499,.T.);
#14882=ORIENTED_EDGE('',*,*,#10496,.F.);
#14883=ORIENTED_EDGE('',*,*,#10500,.F.);
#14884=ORIENTED_EDGE('',*,*,#10501,.F.);
#14885=ORIENTED_EDGE('',*,*,#10492,.F.);
#14886=ORIENTED_EDGE('',*,*,#10495,.F.);
#14887=ORIENTED_EDGE('',*,*,#10497,.F.);
#14888=ORIENTED_EDGE('',*,*,#10499,.F.);
#14889=ORIENTED_EDGE('',*,*,#10502,.F.);
#14890=ORIENTED_EDGE('',*,*,#10503,.F.);
#14891=ORIENTED_EDGE('',*,*,#10488,.T.);
#14892=ORIENTED_EDGE('',*,*,#10493,.F.);
#14893=ORIENTED_EDGE('',*,*,#10501,.T.);
#14894=ORIENTED_EDGE('',*,*,#10504,.F.);
#14895=ORIENTED_EDGE('',*,*,#10483,.T.);
#14896=ORIENTED_EDGE('',*,*,#10505,.T.);
#14897=ORIENTED_EDGE('',*,*,#10502,.T.);
#14898=ORIENTED_EDGE('',*,*,#10498,.T.);
#14899=ORIENTED_EDGE('',*,*,#10489,.T.);
#14900=ORIENTED_EDGE('',*,*,#10504,.T.);
#14901=ORIENTED_EDGE('',*,*,#10500,.T.);
#14902=ORIENTED_EDGE('',*,*,#10506,.T.);
#14903=ORIENTED_EDGE('',*,*,#10490,.T.);
#14904=ORIENTED_EDGE('',*,*,#10506,.F.);
#14905=ORIENTED_EDGE('',*,*,#10503,.T.);
#14906=ORIENTED_EDGE('',*,*,#10505,.F.);
#14907=CYLINDRICAL_SURFACE('',#16815,0.25);
#14908=CYLINDRICAL_SURFACE('',#16818,0.25);
#14909=CYLINDRICAL_SURFACE('',#16821,0.25);
#14910=CYLINDRICAL_SURFACE('',#16824,0.25);
#14911=CYLINDRICAL_SURFACE('',#16834,0.164999999999999);
#14912=CYLINDRICAL_SURFACE('',#16838,0.164999999999999);
#14913=CYLINDRICAL_SURFACE('',#16842,0.164999999999999);
#14914=CYLINDRICAL_SURFACE('',#16846,0.164999999999999);
#14915=CYLINDRICAL_SURFACE('',#16850,2.35);
#14916=CYLINDRICAL_SURFACE('',#16868,2.35);
#14917=CYLINDRICAL_SURFACE('',#16881,1.9);
#14918=CYLINDRICAL_SURFACE('',#16883,1.9);
#14919=CYLINDRICAL_SURFACE('',#16889,0.165);
#14920=CYLINDRICAL_SURFACE('',#16892,0.165);
#14921=CYLINDRICAL_SURFACE('',#16895,0.165);
#14922=CYLINDRICAL_SURFACE('',#16898,0.165);
#14923=CYLINDRICAL_SURFACE('',#16901,2.35);
#14924=CYLINDRICAL_SURFACE('',#16905,2.35);
#14925=CYLINDRICAL_SURFACE('',#16910,1.9);
#14926=CYLINDRICAL_SURFACE('',#16911,1.9);
#14927=CYLINDRICAL_SURFACE('',#16916,0.165);
#14928=CYLINDRICAL_SURFACE('',#16919,0.165);
#14929=CYLINDRICAL_SURFACE('',#16922,0.165);
#14930=CYLINDRICAL_SURFACE('',#16925,0.165);
#14931=CYLINDRICAL_SURFACE('',#16928,1.6);
#14932=CYLINDRICAL_SURFACE('',#16938,1.6);
#14933=CYLINDRICAL_SURFACE('',#16942,1.2);
#14934=CYLINDRICAL_SURFACE('',#16943,1.2);
#14935=CYLINDRICAL_SURFACE('',#16944,0.6);
#14936=CYLINDRICAL_SURFACE('',#16949,0.6);
#14937=CYLINDRICAL_SURFACE('',#16954,0.6);
#14938=CYLINDRICAL_SURFACE('',#16959,0.6);
#14939=CYLINDRICAL_SURFACE('',#16964,0.33);
#14940=CYLINDRICAL_SURFACE('',#16966,0.33);
#14941=CYLINDRICAL_SURFACE('',#16968,0.33);
#14942=CYLINDRICAL_SURFACE('',#16970,0.33);
#14943=CYLINDRICAL_SURFACE('',#16972,0.149999999999999);
#14944=CYLINDRICAL_SURFACE('',#16975,0.149999999999999);
#14945=CYLINDRICAL_SURFACE('',#16978,0.15);
#14946=CYLINDRICAL_SURFACE('',#16981,0.15);
#14947=CYLINDRICAL_SURFACE('',#16984,0.25);
#14948=CYLINDRICAL_SURFACE('',#16986,0.25);
#14949=CYLINDRICAL_SURFACE('',#16988,0.25);
#14950=CYLINDRICAL_SURFACE('',#16990,0.25);
#14951=CYLINDRICAL_SURFACE('',#16992,0.25);
#14952=CYLINDRICAL_SURFACE('',#16994,0.25);
#14953=CYLINDRICAL_SURFACE('',#17007,0.164999999999999);
#14954=CYLINDRICAL_SURFACE('',#17010,0.165);
#14955=CYLINDRICAL_SURFACE('',#17013,0.165);
#14956=CYLINDRICAL_SURFACE('',#17016,0.164999999999999);
#14957=CYLINDRICAL_SURFACE('',#17023,0.164999999999999);
#14958=CYLINDRICAL_SURFACE('',#17027,0.164999999999999);
#14959=CYLINDRICAL_SURFACE('',#17031,0.164999999999999);
#14960=CYLINDRICAL_SURFACE('',#17035,0.164999999999999);
#14961=CYLINDRICAL_SURFACE('',#17042,2.35);
#14962=CYLINDRICAL_SURFACE('',#17044,1.9);
#14963=CYLINDRICAL_SURFACE('',#17052,2.35);
#14964=CYLINDRICAL_SURFACE('',#17064,1.9);
#14965=CYLINDRICAL_SURFACE('',#17078,0.165);
#14966=CYLINDRICAL_SURFACE('',#17081,0.165);
#14967=CYLINDRICAL_SURFACE('',#17084,0.165);
#14968=CYLINDRICAL_SURFACE('',#17087,0.165);
#14969=CYLINDRICAL_SURFACE('',#17093,2.35);
#14970=CYLINDRICAL_SURFACE('',#17094,1.9);
#14971=CYLINDRICAL_SURFACE('',#17096,2.35);
#14972=CYLINDRICAL_SURFACE('',#17100,1.9);
#14973=CYLINDRICAL_SURFACE('',#17103,0.165);
#14974=CYLINDRICAL_SURFACE('',#17106,0.165);
#14975=CYLINDRICAL_SURFACE('',#17109,0.165);
#14976=CYLINDRICAL_SURFACE('',#17112,0.165);
#14977=CYLINDRICAL_SURFACE('',#17115,1.6);
#14978=CYLINDRICAL_SURFACE('',#17119,1.6);
#14979=CYLINDRICAL_SURFACE('',#17123,1.2);
#14980=CYLINDRICAL_SURFACE('',#17124,1.2);
#14981=CYLINDRICAL_SURFACE('',#17133,0.149999999999999);
#14982=CYLINDRICAL_SURFACE('',#17136,0.149999999999999);
#14983=CYLINDRICAL_SURFACE('',#17139,0.15);
#14984=CYLINDRICAL_SURFACE('',#17142,0.15);
#14985=CYLINDRICAL_SURFACE('',#17145,0.329999999999998);
#14986=CYLINDRICAL_SURFACE('',#17147,0.33);
#14987=CYLINDRICAL_SURFACE('',#17149,0.33);
#14988=CYLINDRICAL_SURFACE('',#17151,0.33);
#14989=CYLINDRICAL_SURFACE('',#17153,0.329999999999998);
#14990=CYLINDRICAL_SURFACE('',#17155,0.329999999999998);
#14991=CYLINDRICAL_SURFACE('',#17168,0.15);
#14992=CYLINDRICAL_SURFACE('',#17174,0.15);
#14993=CYLINDRICAL_SURFACE('',#17180,0.149999999999999);
#14994=CYLINDRICAL_SURFACE('',#17186,0.149999999999999);
#14995=CYLINDRICAL_SURFACE('',#17192,0.225);
#14996=CYLINDRICAL_SURFACE('',#17195,0.225);
#14997=CYLINDRICAL_SURFACE('',#17198,0.225);
#14998=CYLINDRICAL_SURFACE('',#17201,0.225);
#14999=CYLINDRICAL_SURFACE('',#17210,2.2);
#15000=CYLINDRICAL_SURFACE('',#17212,2.2);
#15001=CYLINDRICAL_SURFACE('',#17214,2.2);
#15002=CYLINDRICAL_SURFACE('',#17216,2.2);
#15003=CYLINDRICAL_SURFACE('',#17218,1.59);
#15004=CYLINDRICAL_SURFACE('',#17223,1.2);
#15005=CYLINDRICAL_SURFACE('',#17226,0.225);
#15006=CYLINDRICAL_SURFACE('',#17229,0.225);
#15007=CYLINDRICAL_SURFACE('',#17232,0.225);
#15008=CYLINDRICAL_SURFACE('',#17235,0.225);
#15009=CYLINDRICAL_SURFACE('',#17244,2.2);
#15010=CYLINDRICAL_SURFACE('',#17246,2.2);
#15011=CYLINDRICAL_SURFACE('',#17248,2.2);
#15012=CYLINDRICAL_SURFACE('',#17250,2.2);
#15013=CYLINDRICAL_SURFACE('',#17252,1.59);
#15014=CYLINDRICAL_SURFACE('',#17256,1.2);
#15015=CYLINDRICAL_SURFACE('',#17260,0.225);
#15016=CYLINDRICAL_SURFACE('',#17263,0.225);
#15017=CYLINDRICAL_SURFACE('',#17266,0.225000000000001);
#15018=CYLINDRICAL_SURFACE('',#17269,0.225000000000001);
#15019=CYLINDRICAL_SURFACE('',#17272,2.34);
#15020=CYLINDRICAL_SURFACE('',#17277,1.9);
#15021=CYLINDRICAL_SURFACE('',#17279,2.9);
#15022=CYLINDRICAL_SURFACE('',#17285,0.225);
#15023=CYLINDRICAL_SURFACE('',#17288,0.225);
#15024=CYLINDRICAL_SURFACE('',#17291,0.225000000000001);
#15025=CYLINDRICAL_SURFACE('',#17294,0.225000000000001);
#15026=CYLINDRICAL_SURFACE('',#17297,2.34);
#15027=CYLINDRICAL_SURFACE('',#17302,1.9);
#15028=CYLINDRICAL_SURFACE('',#17304,2.9);
#15029=CYLINDRICAL_SURFACE('',#17310,0.225);
#15030=CYLINDRICAL_SURFACE('',#17313,0.225);
#15031=CYLINDRICAL_SURFACE('',#17316,0.225);
#15032=CYLINDRICAL_SURFACE('',#17319,0.225);
#15033=CYLINDRICAL_SURFACE('',#17322,2.34);
#15034=CYLINDRICAL_SURFACE('',#17327,1.9);
#15035=CYLINDRICAL_SURFACE('',#17329,2.9);
#15036=CYLINDRICAL_SURFACE('',#17335,0.225);
#15037=CYLINDRICAL_SURFACE('',#17338,0.225);
#15038=CYLINDRICAL_SURFACE('',#17341,0.225);
#15039=CYLINDRICAL_SURFACE('',#17344,0.225);
#15040=CYLINDRICAL_SURFACE('',#17347,2.34);
#15041=CYLINDRICAL_SURFACE('',#17352,1.9);
#15042=CYLINDRICAL_SURFACE('',#17354,2.9);
#15043=CYLINDRICAL_SURFACE('',#17360,0.225);
#15044=CYLINDRICAL_SURFACE('',#17363,0.225);
#15045=CYLINDRICAL_SURFACE('',#17366,0.225);
#15046=CYLINDRICAL_SURFACE('',#17369,0.225);
#15047=CYLINDRICAL_SURFACE('',#17407,0.5);
#15048=CYLINDRICAL_SURFACE('',#17415,0.2942);
#15049=CYLINDRICAL_SURFACE('',#17424,1.070235);
#15050=CYLINDRICAL_SURFACE('',#17426,0.6);
#15051=CYLINDRICAL_SURFACE('',#17432,1.070235);
#15052=CYLINDRICAL_SURFACE('',#17444,1.129765);
#15053=CYLINDRICAL_SURFACE('',#17451,1.6);
#15054=CYLINDRICAL_SURFACE('',#17456,1.129765);
#15055=CYLINDRICAL_SURFACE('',#17476,1.123812);
#15056=CYLINDRICAL_SURFACE('',#17512,1.076188);
#15057=CYLINDRICAL_SURFACE('',#17526,1.119765);
#15058=CYLINDRICAL_SURFACE('',#17530,1.085235);
#15059=CYLINDRICAL_SURFACE('',#17534,1.119765);
#15060=CYLINDRICAL_SURFACE('',#17538,1.085235);
#15061=CYLINDRICAL_SURFACE('',#17552,1.63531);
#15062=CYLINDRICAL_SURFACE('',#17554,1.);
#15063=CYLINDRICAL_SURFACE('',#17560,1.63531);
#15064=CYLINDRICAL_SURFACE('',#17572,1.71469);
#15065=CYLINDRICAL_SURFACE('',#17579,2.35);
#15066=CYLINDRICAL_SURFACE('',#17584,1.71469);
#15067=CYLINDRICAL_SURFACE('',#17606,1.706752);
#15068=CYLINDRICAL_SURFACE('',#17646,1.643248);
#15069=CYLINDRICAL_SURFACE('',#17660,1.70469);
#15070=CYLINDRICAL_SURFACE('',#17664,1.65031);
#15071=CYLINDRICAL_SURFACE('',#17668,1.70469);
#15072=CYLINDRICAL_SURFACE('',#17672,1.65031);
#15073=CYLINDRICAL_SURFACE('',#17683,0.35);
#15074=CYLINDRICAL_SURFACE('',#17691,0.1954);
#15075=CYLINDRICAL_SURFACE('',#17773,0.6);
#15076=CYLINDRICAL_SURFACE('',#17781,0.21);
#15077=CYLINDRICAL_SURFACE('',#17785,0.605);
#15078=CYLINDRICAL_SURFACE('',#17788,1.);
#15079=CYLINDRICAL_SURFACE('',#17796,0.21);
#15080=CYLINDRICAL_SURFACE('',#17800,0.605);
#15081=CYLINDRICAL_SURFACE('',#17803,1.);
#15082=CYLINDRICAL_SURFACE('',#17809,0.605);
#15083=CYLINDRICAL_SURFACE('',#17812,0.9);
#15084=CYLINDRICAL_SURFACE('',#17818,0.605);
#15085=CYLINDRICAL_SURFACE('',#17821,0.9);
#15086=CYLINDRICAL_SURFACE('',#17827,0.605);
#15087=CYLINDRICAL_SURFACE('',#17830,0.9);
#15088=CYLINDRICAL_SURFACE('',#17836,0.605);
#15089=CYLINDRICAL_SURFACE('',#17839,0.9);
#15090=CYLINDRICAL_SURFACE('',#17870,0.6);
#15091=CYLINDRICAL_SURFACE('',#17872,1.4);
#15092=CYLINDRICAL_SURFACE('',#17877,1.75);
#15093=CYLINDRICAL_SURFACE('',#17880,1.75);
#15094=CYLINDRICAL_SURFACE('',#17883,1.75);
#15095=CYLINDRICAL_SURFACE('',#17886,1.75);
#15096=CYLINDRICAL_SURFACE('',#17889,1.75);
#15097=CYLINDRICAL_SURFACE('',#17892,1.75);
#15098=CYLINDRICAL_SURFACE('',#17895,1.75);
#15099=CYLINDRICAL_SURFACE('',#17898,1.75);
#15100=CYLINDRICAL_SURFACE('',#17901,1.75);
#15101=CYLINDRICAL_SURFACE('',#17904,1.75);
#15102=CYLINDRICAL_SURFACE('',#17907,1.75);
#15103=CYLINDRICAL_SURFACE('',#17910,1.75);
#15104=CYLINDRICAL_SURFACE('',#17913,1.75);
#15105=CYLINDRICAL_SURFACE('',#17916,1.75);
#15106=CYLINDRICAL_SURFACE('',#17919,1.75);
#15107=CYLINDRICAL_SURFACE('',#17922,1.75);
#15108=CYLINDRICAL_SURFACE('',#17925,1.75);
#15109=CYLINDRICAL_SURFACE('',#17928,1.75);
#15110=CYLINDRICAL_SURFACE('',#17931,1.75);
#15111=CYLINDRICAL_SURFACE('',#17936,1.75);
#15112=CYLINDRICAL_SURFACE('',#17964,1.);
#15113=CYLINDRICAL_SURFACE('',#17972,0.21);
#15114=CYLINDRICAL_SURFACE('',#17976,1.005);
#15115=CYLINDRICAL_SURFACE('',#17979,1.4);
#15116=CYLINDRICAL_SURFACE('',#17987,0.21);
#15117=CYLINDRICAL_SURFACE('',#17991,1.005);
#15118=CYLINDRICAL_SURFACE('',#17994,1.4);
#15119=CYLINDRICAL_SURFACE('',#18000,1.005);
#15120=CYLINDRICAL_SURFACE('',#18003,1.3);
#15121=CYLINDRICAL_SURFACE('',#18009,1.005);
#15122=CYLINDRICAL_SURFACE('',#18012,1.3);
#15123=CYLINDRICAL_SURFACE('',#18018,1.005);
#15124=CYLINDRICAL_SURFACE('',#18021,1.3);
#15125=CYLINDRICAL_SURFACE('',#18027,1.005);
#15126=CYLINDRICAL_SURFACE('',#18030,1.3);
#15127=CYLINDRICAL_SURFACE('',#18036,1.005);
#15128=CYLINDRICAL_SURFACE('',#18039,1.3);
#15129=CYLINDRICAL_SURFACE('',#18051,1.);
#15130=CYLINDRICAL_SURFACE('',#18074,1.4);
#15131=CYLINDRICAL_SURFACE('',#18077,1.75);
#15132=CYLINDRICAL_SURFACE('',#18080,1.75);
#15133=CYLINDRICAL_SURFACE('',#18083,1.75);
#15134=CYLINDRICAL_SURFACE('',#18086,1.75);
#15135=CYLINDRICAL_SURFACE('',#18089,1.75);
#15136=CYLINDRICAL_SURFACE('',#18092,1.75);
#15137=CYLINDRICAL_SURFACE('',#18095,1.75);
#15138=CYLINDRICAL_SURFACE('',#18098,1.75);
#15139=CYLINDRICAL_SURFACE('',#18101,1.75);
#15140=CYLINDRICAL_SURFACE('',#18104,1.75);
#15141=CYLINDRICAL_SURFACE('',#18107,1.75);
#15142=CYLINDRICAL_SURFACE('',#18110,1.75);
#15143=CYLINDRICAL_SURFACE('',#18113,1.75);
#15144=CYLINDRICAL_SURFACE('',#18116,1.75);
#15145=CYLINDRICAL_SURFACE('',#18119,1.75);
#15146=CYLINDRICAL_SURFACE('',#18122,1.75);
#15147=CYLINDRICAL_SURFACE('',#18125,1.75);
#15148=CYLINDRICAL_SURFACE('',#18128,1.75);
#15149=CYLINDRICAL_SURFACE('',#18131,1.75);
#15150=CYLINDRICAL_SURFACE('',#18136,1.75);
#15151=CYLINDRICAL_SURFACE('',#18146,1.);
#15152=CYLINDRICAL_SURFACE('',#18154,0.210000000000001);
#15153=CYLINDRICAL_SURFACE('',#18158,1.005);
#15154=CYLINDRICAL_SURFACE('',#18161,1.4);
#15155=CYLINDRICAL_SURFACE('',#18169,0.210000000000001);
#15156=CYLINDRICAL_SURFACE('',#18173,1.005);
#15157=CYLINDRICAL_SURFACE('',#18176,1.4);
#15158=CYLINDRICAL_SURFACE('',#18182,1.005);
#15159=CYLINDRICAL_SURFACE('',#18185,1.3);
#15160=CYLINDRICAL_SURFACE('',#18191,1.005);
#15161=CYLINDRICAL_SURFACE('',#18194,1.3);
#15162=CYLINDRICAL_SURFACE('',#18200,1.005);
#15163=CYLINDRICAL_SURFACE('',#18203,1.3);
#15164=CYLINDRICAL_SURFACE('',#18209,1.005);
#15165=CYLINDRICAL_SURFACE('',#18212,1.3);
#15166=CYLINDRICAL_SURFACE('',#18229,0.24505);
#15167=CYLINDRICAL_SURFACE('',#18291,1.);
#15168=CYLINDRICAL_SURFACE('',#18293,2.);
#15169=CYLINDRICAL_SURFACE('',#18298,3.75);
#15170=CYLINDRICAL_SURFACE('',#18301,3.75);
#15171=CYLINDRICAL_SURFACE('',#18304,3.75);
#15172=CYLINDRICAL_SURFACE('',#18307,3.75);
#15173=CYLINDRICAL_SURFACE('',#18310,3.75);
#15174=CYLINDRICAL_SURFACE('',#18313,3.75);
#15175=CYLINDRICAL_SURFACE('',#18316,3.75);
#15176=CYLINDRICAL_SURFACE('',#18319,3.75);
#15177=CYLINDRICAL_SURFACE('',#18322,3.75);
#15178=CYLINDRICAL_SURFACE('',#18325,3.75);
#15179=CYLINDRICAL_SURFACE('',#18328,3.75);
#15180=CYLINDRICAL_SURFACE('',#18331,3.75);
#15181=CYLINDRICAL_SURFACE('',#18334,3.75);
#15182=CYLINDRICAL_SURFACE('',#18337,3.75);
#15183=CYLINDRICAL_SURFACE('',#18340,3.75);
#15184=CYLINDRICAL_SURFACE('',#18343,3.75);
#15185=CYLINDRICAL_SURFACE('',#18346,3.75);
#15186=CYLINDRICAL_SURFACE('',#18349,3.75);
#15187=CYLINDRICAL_SURFACE('',#18352,3.75);
#15188=CYLINDRICAL_SURFACE('',#18355,3.75);
#15189=CYLINDRICAL_SURFACE('',#18358,3.75);
#15190=CYLINDRICAL_SURFACE('',#18361,3.75);
#15191=CYLINDRICAL_SURFACE('',#18364,3.75);
#15192=CYLINDRICAL_SURFACE('',#18367,3.75);
#15193=CYLINDRICAL_SURFACE('',#18370,3.75);
#15194=CYLINDRICAL_SURFACE('',#18373,3.75);
#15195=CYLINDRICAL_SURFACE('',#18376,3.75);
#15196=CYLINDRICAL_SURFACE('',#18379,3.75);
#15197=CYLINDRICAL_SURFACE('',#18382,3.75);
#15198=CYLINDRICAL_SURFACE('',#18385,3.75);
#15199=CYLINDRICAL_SURFACE('',#18388,3.75);
#15200=CYLINDRICAL_SURFACE('',#18391,3.75);
#15201=CYLINDRICAL_SURFACE('',#18394,3.75);
#15202=CYLINDRICAL_SURFACE('',#18397,3.75);
#15203=CYLINDRICAL_SURFACE('',#18400,3.75);
#15204=CYLINDRICAL_SURFACE('',#18403,3.75);
#15205=CYLINDRICAL_SURFACE('',#18406,3.75);
#15206=CYLINDRICAL_SURFACE('',#18409,3.75);
#15207=CYLINDRICAL_SURFACE('',#18412,3.75);
#15208=CYLINDRICAL_SURFACE('',#18417,3.75);
#15209=ADVANCED_FACE('',(#2002),#14907,.F.);
#15210=ADVANCED_FACE('',(#2003),#14908,.F.);
#15211=ADVANCED_FACE('',(#2004),#14909,.F.);
#15212=ADVANCED_FACE('',(#2005),#14910,.F.);
#15213=ADVANCED_FACE('',(#2006),#1602,.T.);
#15214=ADVANCED_FACE('',(#2007),#1603,.T.);
#15215=ADVANCED_FACE('',(#2008),#1604,.T.);
#15216=ADVANCED_FACE('',(#2009),#1605,.T.);
#15217=ADVANCED_FACE('',(#2010,#1374,#1375,#1376,#1377),#1606,.T.);
#15218=ADVANCED_FACE('',(#2011,#1378,#1379,#1380,#1381),#1607,.F.);
#15219=ADVANCED_FACE('',(#2012),#14911,.F.);
#15220=ADVANCED_FACE('',(#2013),#1608,.T.);
#15221=ADVANCED_FACE('',(#2014),#14912,.F.);
#15222=ADVANCED_FACE('',(#2015),#1609,.T.);
#15223=ADVANCED_FACE('',(#2016),#14913,.F.);
#15224=ADVANCED_FACE('',(#2017),#1610,.F.);
#15225=ADVANCED_FACE('',(#2018),#14914,.F.);
#15226=ADVANCED_FACE('',(#2019),#1611,.F.);
#15227=ADVANCED_FACE('',(#2020),#14915,.F.);
#15228=ADVANCED_FACE('',(#2021),#1612,.T.);
#15229=ADVANCED_FACE('',(#2022,#1382,#1383,#1384,#1385,#1386,#1387),#1613,
 .T.);
#15230=ADVANCED_FACE('',(#2023,#1388,#1389,#1390,#1391,#1392),#1614,.T.);
#15231=ADVANCED_FACE('',(#2024),#14916,.F.);
#15232=ADVANCED_FACE('',(#2025),#1615,.F.);
#15233=ADVANCED_FACE('',(#2026,#1393,#1394,#1395,#1396,#1397,#1398),#1616,
 .T.);
#15234=ADVANCED_FACE('',(#2027),#1617,.T.);
#15235=ADVANCED_FACE('',(#2028),#14917,.F.);
#15236=ADVANCED_FACE('',(#2029),#14918,.F.);
#15237=ADVANCED_FACE('',(#2030),#1618,.F.);
#15238=ADVANCED_FACE('',(#2031),#1619,.T.);
#15239=ADVANCED_FACE('',(#2032),#14919,.F.);
#15240=ADVANCED_FACE('',(#2033),#1620,.T.);
#15241=ADVANCED_FACE('',(#2034),#14920,.F.);
#15242=ADVANCED_FACE('',(#2035),#1621,.T.);
#15243=ADVANCED_FACE('',(#2036),#14921,.F.);
#15244=ADVANCED_FACE('',(#2037),#1622,.F.);
#15245=ADVANCED_FACE('',(#2038),#14922,.F.);
#15246=ADVANCED_FACE('',(#2039),#1623,.F.);
#15247=ADVANCED_FACE('',(#2040),#14923,.F.);
#15248=ADVANCED_FACE('',(#2041),#1624,.T.);
#15249=ADVANCED_FACE('',(#2042),#14924,.F.);
#15250=ADVANCED_FACE('',(#2043),#1625,.F.);
#15251=ADVANCED_FACE('',(#2044),#1626,.T.);
#15252=ADVANCED_FACE('',(#2045),#14925,.F.);
#15253=ADVANCED_FACE('',(#2046),#14926,.F.);
#15254=ADVANCED_FACE('',(#2047),#1627,.F.);
#15255=ADVANCED_FACE('',(#2048),#1628,.T.);
#15256=ADVANCED_FACE('',(#2049),#14927,.F.);
#15257=ADVANCED_FACE('',(#2050),#1629,.T.);
#15258=ADVANCED_FACE('',(#2051),#14928,.F.);
#15259=ADVANCED_FACE('',(#2052),#1630,.T.);
#15260=ADVANCED_FACE('',(#2053),#14929,.F.);
#15261=ADVANCED_FACE('',(#2054),#1631,.F.);
#15262=ADVANCED_FACE('',(#2055),#14930,.F.);
#15263=ADVANCED_FACE('',(#2056),#1632,.F.);
#15264=ADVANCED_FACE('',(#2057),#14931,.F.);
#15265=ADVANCED_FACE('',(#2058),#1633,.T.);
#15266=ADVANCED_FACE('',(#2059,#1399,#1400,#1401,#1402,#1403),#1634,.T.);
#15267=ADVANCED_FACE('',(#2060),#14932,.F.);
#15268=ADVANCED_FACE('',(#2061),#1635,.F.);
#15269=ADVANCED_FACE('',(#2062),#14933,.F.);
#15270=ADVANCED_FACE('',(#2063),#14934,.F.);
#15271=ADVANCED_FACE('',(#2064),#14935,.F.);
#15272=ADVANCED_FACE('',(#2065,#1404),#1636,.T.);
#15273=ADVANCED_FACE('',(#2066),#14936,.F.);
#15274=ADVANCED_FACE('',(#2067,#1405),#1637,.T.);
#15275=ADVANCED_FACE('',(#2068),#14937,.F.);
#15276=ADVANCED_FACE('',(#2069,#1406),#1638,.T.);
#15277=ADVANCED_FACE('',(#2070),#14938,.F.);
#15278=ADVANCED_FACE('',(#2071,#1407),#1639,.T.);
#15279=ADVANCED_FACE('',(#2072),#14939,.F.);
#15280=ADVANCED_FACE('',(#2073),#14940,.F.);
#15281=ADVANCED_FACE('',(#2074),#14941,.F.);
#15282=ADVANCED_FACE('',(#2075),#14942,.F.);
#15283=ADVANCED_FACE('',(#2076),#14943,.F.);
#15284=ADVANCED_FACE('',(#2077),#1640,.T.);
#15285=ADVANCED_FACE('',(#2078),#14944,.F.);
#15286=ADVANCED_FACE('',(#2079),#1641,.T.);
#15287=ADVANCED_FACE('',(#2080),#14945,.F.);
#15288=ADVANCED_FACE('',(#2081),#1642,.T.);
#15289=ADVANCED_FACE('',(#2082),#14946,.F.);
#15290=ADVANCED_FACE('',(#2083),#1643,.T.);
#15291=ADVANCED_FACE('',(#2084),#14947,.F.);
#15292=ADVANCED_FACE('',(#2085),#14948,.F.);
#15293=ADVANCED_FACE('',(#2086),#14949,.F.);
#15294=ADVANCED_FACE('',(#2087),#14950,.F.);
#15295=ADVANCED_FACE('',(#2088),#14951,.F.);
#15296=ADVANCED_FACE('',(#2089),#14952,.F.);
#15297=ADVANCED_FACE('',(#2090),#1644,.T.);
#15298=ADVANCED_FACE('',(#2091,#1408,#1409,#1410),#1645,.F.);
#15299=ADVANCED_FACE('',(#2092),#1646,.T.);
#15300=ADVANCED_FACE('',(#2093),#1647,.T.);
#15301=ADVANCED_FACE('',(#2094,#1411,#1412,#1413),#1648,.F.);
#15302=ADVANCED_FACE('',(#2095),#1649,.F.);
#15303=ADVANCED_FACE('',(#2096),#1650,.F.);
#15304=ADVANCED_FACE('',(#2097,#1414,#1415,#1416,#1417),#1651,.T.);
#15305=ADVANCED_FACE('',(#2098),#1652,.T.);
#15306=ADVANCED_FACE('',(#2099,#1418,#1419,#1420,#1421),#1653,.F.);
#15307=ADVANCED_FACE('',(#2100),#14953,.F.);
#15308=ADVANCED_FACE('',(#2101),#14954,.F.);
#15309=ADVANCED_FACE('',(#2102),#14955,.F.);
#15310=ADVANCED_FACE('',(#2103),#14956,.F.);
#15311=ADVANCED_FACE('',(#2104),#1654,.F.);
#15312=ADVANCED_FACE('',(#2105),#1655,.F.);
#15313=ADVANCED_FACE('',(#2106),#1656,.F.);
#15314=ADVANCED_FACE('',(#2107),#1657,.F.);
#15315=ADVANCED_FACE('',(#2108),#14957,.F.);
#15316=ADVANCED_FACE('',(#2109),#1658,.T.);
#15317=ADVANCED_FACE('',(#2110),#14958,.F.);
#15318=ADVANCED_FACE('',(#2111),#1659,.T.);
#15319=ADVANCED_FACE('',(#2112),#14959,.F.);
#15320=ADVANCED_FACE('',(#2113),#1660,.F.);
#15321=ADVANCED_FACE('',(#2114),#14960,.F.);
#15322=ADVANCED_FACE('',(#2115),#1661,.F.);
#15323=ADVANCED_FACE('',(#2116),#1662,.T.);
#15324=ADVANCED_FACE('',(#2117),#14961,.F.);
#15325=ADVANCED_FACE('',(#2118),#14962,.F.);
#15326=ADVANCED_FACE('',(#2119,#1422,#1423,#1424,#1425,#1426),#1663,.F.);
#15327=ADVANCED_FACE('',(#2120),#14963,.F.);
#15328=ADVANCED_FACE('',(#2121),#1664,.F.);
#15329=ADVANCED_FACE('',(#2122,#1427,#1428,#1429,#1430,#1431,#1432),#1665,
 .T.);
#15330=ADVANCED_FACE('',(#2123),#14964,.F.);
#15331=ADVANCED_FACE('',(#2124,#1433,#1434,#1435,#1436,#1437,#1438),#1666,
 .T.);
#15332=ADVANCED_FACE('',(#2125),#1667,.F.);
#15333=ADVANCED_FACE('',(#2126),#1668,.F.);
#15334=ADVANCED_FACE('',(#2127),#1669,.F.);
#15335=ADVANCED_FACE('',(#2128),#14965,.F.);
#15336=ADVANCED_FACE('',(#2129),#1670,.T.);
#15337=ADVANCED_FACE('',(#2130),#14966,.F.);
#15338=ADVANCED_FACE('',(#2131),#1671,.T.);
#15339=ADVANCED_FACE('',(#2132),#14967,.F.);
#15340=ADVANCED_FACE('',(#2133),#1672,.F.);
#15341=ADVANCED_FACE('',(#2134),#14968,.F.);
#15342=ADVANCED_FACE('',(#2135),#1673,.F.);
#15343=ADVANCED_FACE('',(#2136),#1674,.T.);
#15344=ADVANCED_FACE('',(#2137),#14969,.F.);
#15345=ADVANCED_FACE('',(#2138),#14970,.F.);
#15346=ADVANCED_FACE('',(#2139),#14971,.F.);
#15347=ADVANCED_FACE('',(#2140),#1675,.F.);
#15348=ADVANCED_FACE('',(#2141),#14972,.F.);
#15349=ADVANCED_FACE('',(#2142),#1676,.F.);
#15350=ADVANCED_FACE('',(#2143),#1677,.F.);
#15351=ADVANCED_FACE('',(#2144),#14973,.F.);
#15352=ADVANCED_FACE('',(#2145),#1678,.T.);
#15353=ADVANCED_FACE('',(#2146),#14974,.F.);
#15354=ADVANCED_FACE('',(#2147),#1679,.T.);
#15355=ADVANCED_FACE('',(#2148),#14975,.F.);
#15356=ADVANCED_FACE('',(#2149),#1680,.F.);
#15357=ADVANCED_FACE('',(#2150),#14976,.F.);
#15358=ADVANCED_FACE('',(#2151),#1681,.F.);
#15359=ADVANCED_FACE('',(#2152),#14977,.F.);
#15360=ADVANCED_FACE('',(#2153),#1682,.T.);
#15361=ADVANCED_FACE('',(#2154),#14978,.F.);
#15362=ADVANCED_FACE('',(#2155),#1683,.F.);
#15363=ADVANCED_FACE('',(#2156),#14979,.F.);
#15364=ADVANCED_FACE('',(#2157),#14980,.F.);
#15365=ADVANCED_FACE('',(#2158),#1684,.F.);
#15366=ADVANCED_FACE('',(#2159,#1439,#1440,#1441,#1442,#1443),#1685,.F.);
#15367=ADVANCED_FACE('',(#2160),#14981,.F.);
#15368=ADVANCED_FACE('',(#2161),#1686,.F.);
#15369=ADVANCED_FACE('',(#2162),#14982,.F.);
#15370=ADVANCED_FACE('',(#2163),#1687,.F.);
#15371=ADVANCED_FACE('',(#2164),#14983,.F.);
#15372=ADVANCED_FACE('',(#2165),#1688,.F.);
#15373=ADVANCED_FACE('',(#2166),#14984,.F.);
#15374=ADVANCED_FACE('',(#2167),#1689,.F.);
#15375=ADVANCED_FACE('',(#2168),#14985,.F.);
#15376=ADVANCED_FACE('',(#2169),#14986,.F.);
#15377=ADVANCED_FACE('',(#2170),#14987,.F.);
#15378=ADVANCED_FACE('',(#2171),#14988,.F.);
#15379=ADVANCED_FACE('',(#2172),#14989,.F.);
#15380=ADVANCED_FACE('',(#2173),#14990,.F.);
#15381=ADVANCED_FACE('',(#2174),#1690,.T.);
#15382=ADVANCED_FACE('',(#2175,#1444,#1445,#1446),#1691,.T.);
#15383=ADVANCED_FACE('',(#2176),#1692,.T.);
#15384=ADVANCED_FACE('',(#2177,#1447,#1448,#1449),#1693,.T.);
#15385=ADVANCED_FACE('',(#2178),#1694,.T.);
#15386=ADVANCED_FACE('',(#2179),#1695,.F.);
#15387=ADVANCED_FACE('',(#2180),#1696,.F.);
#15388=ADVANCED_FACE('',(#2181,#1450,#1451,#1452,#1453,#1454),#1697,.F.);
#15389=ADVANCED_FACE('',(#2182),#1698,.T.);
#15390=ADVANCED_FACE('',(#2183,#1455,#1456,#1457,#1458,#1459),#1699,.T.);
#15391=ADVANCED_FACE('',(#2184),#14991,.T.);
#15392=ADVANCED_FACE('',(#2185),#1700,.T.);
#15393=ADVANCED_FACE('',(#2186),#1701,.F.);
#15394=ADVANCED_FACE('',(#2187),#14992,.T.);
#15395=ADVANCED_FACE('',(#2188),#1702,.T.);
#15396=ADVANCED_FACE('',(#2189),#1703,.F.);
#15397=ADVANCED_FACE('',(#2190),#14993,.T.);
#15398=ADVANCED_FACE('',(#2191),#1704,.T.);
#15399=ADVANCED_FACE('',(#2192),#1705,.F.);
#15400=ADVANCED_FACE('',(#2193),#14994,.T.);
#15401=ADVANCED_FACE('',(#2194),#1706,.T.);
#15402=ADVANCED_FACE('',(#2195),#1707,.F.);
#15403=ADVANCED_FACE('',(#2196),#14995,.F.);
#15404=ADVANCED_FACE('',(#2197),#14996,.F.);
#15405=ADVANCED_FACE('',(#2198),#14997,.F.);
#15406=ADVANCED_FACE('',(#2199),#14998,.F.);
#15407=ADVANCED_FACE('',(#2200,#1460),#1708,.F.);
#15408=ADVANCED_FACE('',(#2201),#14999,.T.);
#15409=ADVANCED_FACE('',(#2202),#15000,.T.);
#15410=ADVANCED_FACE('',(#2203),#15001,.T.);
#15411=ADVANCED_FACE('',(#2204),#15002,.T.);
#15412=ADVANCED_FACE('',(#2205),#15003,.T.);
#15413=ADVANCED_FACE('',(#2206,#1461),#1709,.T.);
#15414=ADVANCED_FACE('',(#2207),#15004,.F.);
#15415=ADVANCED_FACE('',(#2208,#1462),#1710,.T.);
#15416=ADVANCED_FACE('',(#2209),#15005,.F.);
#15417=ADVANCED_FACE('',(#2210),#15006,.F.);
#15418=ADVANCED_FACE('',(#2211),#15007,.F.);
#15419=ADVANCED_FACE('',(#2212),#15008,.F.);
#15420=ADVANCED_FACE('',(#2213,#1463),#1711,.F.);
#15421=ADVANCED_FACE('',(#2214),#15009,.T.);
#15422=ADVANCED_FACE('',(#2215),#15010,.T.);
#15423=ADVANCED_FACE('',(#2216),#15011,.T.);
#15424=ADVANCED_FACE('',(#2217),#15012,.T.);
#15425=ADVANCED_FACE('',(#2218),#15013,.T.);
#15426=ADVANCED_FACE('',(#2219,#1464),#1712,.F.);
#15427=ADVANCED_FACE('',(#2220),#15014,.F.);
#15428=ADVANCED_FACE('',(#2221,#1465),#1713,.T.);
#15429=ADVANCED_FACE('',(#2222),#15015,.F.);
#15430=ADVANCED_FACE('',(#2223),#15016,.F.);
#15431=ADVANCED_FACE('',(#2224),#15017,.F.);
#15432=ADVANCED_FACE('',(#2225),#15018,.F.);
#15433=ADVANCED_FACE('',(#2226),#15019,.T.);
#15434=ADVANCED_FACE('',(#2227,#1466),#1714,.T.);
#15435=ADVANCED_FACE('',(#2228),#15020,.F.);
#15436=ADVANCED_FACE('',(#2229),#15021,.T.);
#15437=ADVANCED_FACE('',(#2230,#1467,#1468,#1469,#1470,#1471),#1715,.T.);
#15438=ADVANCED_FACE('',(#2231,#1472,#1473,#1474,#1475,#1476),#1716,.F.);
#15439=ADVANCED_FACE('',(#2232),#15022,.F.);
#15440=ADVANCED_FACE('',(#2233),#15023,.F.);
#15441=ADVANCED_FACE('',(#2234),#15024,.F.);
#15442=ADVANCED_FACE('',(#2235),#15025,.F.);
#15443=ADVANCED_FACE('',(#2236),#15026,.T.);
#15444=ADVANCED_FACE('',(#2237,#1477),#1717,.F.);
#15445=ADVANCED_FACE('',(#2238),#15027,.F.);
#15446=ADVANCED_FACE('',(#2239),#15028,.T.);
#15447=ADVANCED_FACE('',(#2240,#1478,#1479,#1480,#1481,#1482),#1718,.T.);
#15448=ADVANCED_FACE('',(#2241,#1483,#1484,#1485,#1486,#1487),#1719,.F.);
#15449=ADVANCED_FACE('',(#2242),#15029,.F.);
#15450=ADVANCED_FACE('',(#2243),#15030,.F.);
#15451=ADVANCED_FACE('',(#2244),#15031,.F.);
#15452=ADVANCED_FACE('',(#2245),#15032,.F.);
#15453=ADVANCED_FACE('',(#2246),#15033,.T.);
#15454=ADVANCED_FACE('',(#2247,#1488),#1720,.T.);
#15455=ADVANCED_FACE('',(#2248),#15034,.F.);
#15456=ADVANCED_FACE('',(#2249),#15035,.T.);
#15457=ADVANCED_FACE('',(#2250,#1489,#1490,#1491,#1492,#1493),#1721,.T.);
#15458=ADVANCED_FACE('',(#2251,#1494,#1495,#1496,#1497,#1498),#1722,.F.);
#15459=ADVANCED_FACE('',(#2252),#15036,.F.);
#15460=ADVANCED_FACE('',(#2253),#15037,.F.);
#15461=ADVANCED_FACE('',(#2254),#15038,.F.);
#15462=ADVANCED_FACE('',(#2255),#15039,.F.);
#15463=ADVANCED_FACE('',(#2256),#15040,.T.);
#15464=ADVANCED_FACE('',(#2257,#1499),#1723,.F.);
#15465=ADVANCED_FACE('',(#2258),#15041,.F.);
#15466=ADVANCED_FACE('',(#2259),#15042,.T.);
#15467=ADVANCED_FACE('',(#2260,#1500,#1501,#1502,#1503,#1504),#1724,.T.);
#15468=ADVANCED_FACE('',(#2261,#1505,#1506,#1507,#1508,#1509),#1725,.F.);
#15469=ADVANCED_FACE('',(#2262),#15043,.F.);
#15470=ADVANCED_FACE('',(#2263),#15044,.F.);
#15471=ADVANCED_FACE('',(#2264),#15045,.F.);
#15472=ADVANCED_FACE('',(#2265),#15046,.F.);
#15473=ADVANCED_FACE('',(#2266),#1726,.T.);
#15474=ADVANCED_FACE('',(#2267),#1727,.T.);
#15475=ADVANCED_FACE('',(#2268),#1728,.T.);
#15476=ADVANCED_FACE('',(#2269),#1729,.T.);
#15477=ADVANCED_FACE('',(#2270,#1510,#1511,#1512,#1513),#1730,.T.);
#15478=ADVANCED_FACE('',(#2271,#1514,#1515,#1516,#1517),#1731,.F.);
#15479=ADVANCED_FACE('',(#2272),#1732,.T.);
#15480=ADVANCED_FACE('',(#2273),#1733,.T.);
#15481=ADVANCED_FACE('',(#2274),#1734,.T.);
#15482=ADVANCED_FACE('',(#2275),#1735,.T.);
#15483=ADVANCED_FACE('',(#2276),#1736,.T.);
#15484=ADVANCED_FACE('',(#2277),#1737,.F.);
#15485=ADVANCED_FACE('',(#2278),#1738,.T.);
#15486=ADVANCED_FACE('',(#2279),#1739,.T.);
#15487=ADVANCED_FACE('',(#2280),#1740,.T.);
#15488=ADVANCED_FACE('',(#2281),#1741,.T.);
#15489=ADVANCED_FACE('',(#2282),#1742,.T.);
#15490=ADVANCED_FACE('',(#2283),#1743,.F.);
#15491=ADVANCED_FACE('',(#2284),#1744,.F.);
#15492=ADVANCED_FACE('',(#2285),#1745,.F.);
#15493=ADVANCED_FACE('',(#2286),#1746,.F.);
#15494=ADVANCED_FACE('',(#2287),#1747,.F.);
#15495=ADVANCED_FACE('',(#2288),#1748,.F.);
#15496=ADVANCED_FACE('',(#2289),#1749,.F.);
#15497=ADVANCED_FACE('',(#2290),#1750,.F.);
#15498=ADVANCED_FACE('',(#2291),#1751,.F.);
#15499=ADVANCED_FACE('',(#2292),#1752,.F.);
#15500=ADVANCED_FACE('',(#2293),#1753,.T.);
#15501=ADVANCED_FACE('',(#2294),#1101,.T.);
#15502=ADVANCED_FACE('',(#2295),#15047,.T.);
#15503=ADVANCED_FACE('',(#2296),#1102,.T.);
#15504=ADVANCED_FACE('',(#2297,#1518),#1754,.T.);
#15505=ADVANCED_FACE('',(#2298),#1103,.T.);
#15506=ADVANCED_FACE('',(#2299),#15048,.T.);
#15507=ADVANCED_FACE('',(#2300),#1097,.F.);
#15508=ADVANCED_FACE('',(#2301),#15049,.T.);
#15509=ADVANCED_FACE('',(#2302),#15050,.F.);
#15510=ADVANCED_FACE('',(#2303),#1104,.F.);
#15511=ADVANCED_FACE('',(#2304,#1519),#1755,.T.);
#15512=ADVANCED_FACE('',(#2305),#15051,.T.);
#15513=ADVANCED_FACE('',(#2306,#1520),#1756,.T.);
#15514=ADVANCED_FACE('',(#2307),#1105,.F.);
#15515=ADVANCED_FACE('',(#2308),#1098,.F.);
#15516=ADVANCED_FACE('',(#2309),#15052,.F.);
#15517=ADVANCED_FACE('',(#2310,#1521),#1757,.T.);
#15518=ADVANCED_FACE('',(#2311),#1106,.T.);
#15519=ADVANCED_FACE('',(#2312),#15053,.T.);
#15520=ADVANCED_FACE('',(#2313),#1107,.T.);
#15521=ADVANCED_FACE('',(#2314,#1522),#1758,.T.);
#15522=ADVANCED_FACE('',(#2315),#15054,.F.);
#15523=ADVANCED_FACE('',(#2316),#1067,.T.);
#15524=ADVANCED_FACE('',(#2317),#1068,.T.);
#15525=ADVANCED_FACE('',(#2318),#1069,.T.);
#15526=ADVANCED_FACE('',(#2319),#1070,.T.);
#15527=ADVANCED_FACE('',(#2320),#1071,.T.);
#15528=ADVANCED_FACE('',(#2321),#1072,.T.);
#15529=ADVANCED_FACE('',(#2322),#1073,.T.);
#15530=ADVANCED_FACE('',(#2323),#1074,.F.);
#15531=ADVANCED_FACE('',(#2324),#15055,.T.);
#15532=ADVANCED_FACE('',(#2325),#1759,.T.);
#15533=ADVANCED_FACE('',(#2326),#1075,.F.);
#15534=ADVANCED_FACE('',(#2327),#1760,.T.);
#15535=ADVANCED_FACE('',(#2328),#1076,.F.);
#15536=ADVANCED_FACE('',(#2329),#1761,.T.);
#15537=ADVANCED_FACE('',(#2330),#1077,.F.);
#15538=ADVANCED_FACE('',(#2331),#1762,.T.);
#15539=ADVANCED_FACE('',(#2332),#1078,.F.);
#15540=ADVANCED_FACE('',(#2333),#1763,.T.);
#15541=ADVANCED_FACE('',(#2334),#1079,.F.);
#15542=ADVANCED_FACE('',(#2335),#15056,.F.);
#15543=ADVANCED_FACE('',(#2336),#1764,.T.);
#15544=ADVANCED_FACE('',(#2337),#1080,.F.);
#15545=ADVANCED_FACE('',(#2338,#1523),#1765,.T.);
#15546=ADVANCED_FACE('',(#2339),#1766,.T.);
#15547=ADVANCED_FACE('',(#2340,#1524),#1767,.T.);
#15548=ADVANCED_FACE('',(#2341),#15057,.T.);
#15549=ADVANCED_FACE('',(#2342,#1525),#1768,.T.);
#15550=ADVANCED_FACE('',(#2343),#15058,.F.);
#15551=ADVANCED_FACE('',(#2344,#1526),#1769,.T.);
#15552=ADVANCED_FACE('',(#2345),#15059,.T.);
#15553=ADVANCED_FACE('',(#2346,#1527),#1770,.T.);
#15554=ADVANCED_FACE('',(#2347),#15060,.F.);
#15555=ADVANCED_FACE('',(#2348),#1099,.F.);
#15556=ADVANCED_FACE('',(#2349),#15061,.T.);
#15557=ADVANCED_FACE('',(#2350),#15062,.F.);
#15558=ADVANCED_FACE('',(#2351),#1108,.F.);
#15559=ADVANCED_FACE('',(#2352,#1528),#1771,.T.);
#15560=ADVANCED_FACE('',(#2353),#15063,.T.);
#15561=ADVANCED_FACE('',(#2354,#1529),#1772,.T.);
#15562=ADVANCED_FACE('',(#2355),#1109,.F.);
#15563=ADVANCED_FACE('',(#2356),#1100,.F.);
#15564=ADVANCED_FACE('',(#2357),#15064,.F.);
#15565=ADVANCED_FACE('',(#2358,#1530),#1773,.T.);
#15566=ADVANCED_FACE('',(#2359),#1110,.T.);
#15567=ADVANCED_FACE('',(#2360),#15065,.T.);
#15568=ADVANCED_FACE('',(#2361),#1111,.T.);
#15569=ADVANCED_FACE('',(#2362,#1531),#1774,.T.);
#15570=ADVANCED_FACE('',(#2363),#15066,.F.);
#15571=ADVANCED_FACE('',(#2364),#1081,.T.);
#15572=ADVANCED_FACE('',(#2365),#1082,.T.);
#15573=ADVANCED_FACE('',(#2366),#1083,.T.);
#15574=ADVANCED_FACE('',(#2367),#1084,.T.);
#15575=ADVANCED_FACE('',(#2368),#1085,.T.);
#15576=ADVANCED_FACE('',(#2369),#1086,.T.);
#15577=ADVANCED_FACE('',(#2370),#1087,.T.);
#15578=ADVANCED_FACE('',(#2371),#1088,.T.);
#15579=ADVANCED_FACE('',(#2372),#1089,.F.);
#15580=ADVANCED_FACE('',(#2373),#15067,.T.);
#15581=ADVANCED_FACE('',(#2374),#1775,.T.);
#15582=ADVANCED_FACE('',(#2375),#1090,.F.);
#15583=ADVANCED_FACE('',(#2376),#1776,.T.);
#15584=ADVANCED_FACE('',(#2377),#1091,.F.);
#15585=ADVANCED_FACE('',(#2378),#1777,.T.);
#15586=ADVANCED_FACE('',(#2379),#1092,.F.);
#15587=ADVANCED_FACE('',(#2380),#1778,.T.);
#15588=ADVANCED_FACE('',(#2381),#1093,.F.);
#15589=ADVANCED_FACE('',(#2382),#1779,.T.);
#15590=ADVANCED_FACE('',(#2383),#1094,.F.);
#15591=ADVANCED_FACE('',(#2384),#1780,.T.);
#15592=ADVANCED_FACE('',(#2385),#1095,.F.);
#15593=ADVANCED_FACE('',(#2386),#15068,.F.);
#15594=ADVANCED_FACE('',(#2387),#1781,.T.);
#15595=ADVANCED_FACE('',(#2388),#1096,.F.);
#15596=ADVANCED_FACE('',(#2389,#1532),#1782,.T.);
#15597=ADVANCED_FACE('',(#2390),#1783,.T.);
#15598=ADVANCED_FACE('',(#2391,#1533),#1784,.T.);
#15599=ADVANCED_FACE('',(#2392),#15069,.T.);
#15600=ADVANCED_FACE('',(#2393,#1534),#1785,.T.);
#15601=ADVANCED_FACE('',(#2394),#15070,.F.);
#15602=ADVANCED_FACE('',(#2395,#1535),#1786,.T.);
#15603=ADVANCED_FACE('',(#2396),#15071,.T.);
#15604=ADVANCED_FACE('',(#2397,#1536),#1787,.T.);
#15605=ADVANCED_FACE('',(#2398),#15072,.F.);
#15606=ADVANCED_FACE('',(#2399),#1788,.T.);
#15607=ADVANCED_FACE('',(#2400),#1112,.T.);
#15608=ADVANCED_FACE('',(#2401),#15073,.T.);
#15609=ADVANCED_FACE('',(#2402),#1113,.T.);
#15610=ADVANCED_FACE('',(#2403,#1537),#1789,.T.);
#15611=ADVANCED_FACE('',(#2404),#1114,.T.);
#15612=ADVANCED_FACE('',(#2405),#15074,.T.);
#15613=ADVANCED_FACE('',(#2406),#1115,.T.);
#15614=ADVANCED_FACE('',(#2407),#1790,.T.);
#15615=ADVANCED_FACE('',(#2408),#1791,.F.);
#15616=ADVANCED_FACE('',(#2409),#1792,.F.);
#15617=ADVANCED_FACE('',(#2410),#1793,.F.);
#15618=ADVANCED_FACE('',(#2411),#1794,.F.);
#15619=ADVANCED_FACE('',(#2412),#1795,.F.);
#15620=ADVANCED_FACE('',(#2413),#1796,.F.);
#15621=ADVANCED_FACE('',(#2414),#1797,.F.);
#15622=ADVANCED_FACE('',(#2415),#1798,.F.);
#15623=ADVANCED_FACE('',(#2416),#1799,.F.);
#15624=ADVANCED_FACE('',(#2417),#1800,.T.);
#15625=ADVANCED_FACE('',(#2418),#1801,.F.);
#15626=ADVANCED_FACE('',(#2419),#1802,.F.);
#15627=ADVANCED_FACE('',(#2420),#1803,.F.);
#15628=ADVANCED_FACE('',(#2421,#1538),#15075,.T.);
#15629=ADVANCED_FACE('',(#2422),#1804,.T.);
#15630=ADVANCED_FACE('',(#2423),#1805,.F.);
#15631=ADVANCED_FACE('',(#2424),#1806,.T.);
#15632=ADVANCED_FACE('',(#2425),#15076,.F.);
#15633=ADVANCED_FACE('',(#2426),#1807,.T.);
#15634=ADVANCED_FACE('',(#2427,#1539),#15077,.F.);
#15635=ADVANCED_FACE('',(#2428,#1540),#15078,.T.);
#15636=ADVANCED_FACE('',(#2429,#1541),#1808,.T.);
#15637=ADVANCED_FACE('',(#2430,#1542),#1809,.F.);
#15638=ADVANCED_FACE('',(#2431),#1810,.T.);
#15639=ADVANCED_FACE('',(#2432),#15079,.F.);
#15640=ADVANCED_FACE('',(#2433),#1811,.T.);
#15641=ADVANCED_FACE('',(#2434,#1543),#15080,.F.);
#15642=ADVANCED_FACE('',(#2435,#1544),#15081,.T.);
#15643=ADVANCED_FACE('',(#2436,#1545),#1812,.T.);
#15644=ADVANCED_FACE('',(#2437,#1546),#1813,.F.);
#15645=ADVANCED_FACE('',(#2438),#15082,.F.);
#15646=ADVANCED_FACE('',(#2439),#15083,.T.);
#15647=ADVANCED_FACE('',(#2440,#1547),#1814,.T.);
#15648=ADVANCED_FACE('',(#2441,#1548),#1815,.F.);
#15649=ADVANCED_FACE('',(#2442),#15084,.F.);
#15650=ADVANCED_FACE('',(#2443),#15085,.T.);
#15651=ADVANCED_FACE('',(#2444,#1549),#1816,.T.);
#15652=ADVANCED_FACE('',(#2445,#1550),#1817,.F.);
#15653=ADVANCED_FACE('',(#2446),#15086,.F.);
#15654=ADVANCED_FACE('',(#2447),#15087,.T.);
#15655=ADVANCED_FACE('',(#2448,#1551),#1818,.T.);
#15656=ADVANCED_FACE('',(#2449,#1552),#1819,.F.);
#15657=ADVANCED_FACE('',(#2450),#15088,.F.);
#15658=ADVANCED_FACE('',(#2451),#15089,.T.);
#15659=ADVANCED_FACE('',(#2452,#1553),#1820,.T.);
#15660=ADVANCED_FACE('',(#2453,#1554),#1821,.F.);
#15661=ADVANCED_FACE('',(#2454),#1822,.F.);
#15662=ADVANCED_FACE('',(#2455),#1823,.F.);
#15663=ADVANCED_FACE('',(#2456),#1824,.F.);
#15664=ADVANCED_FACE('',(#2457,#1555),#1825,.F.);
#15665=ADVANCED_FACE('',(#2458),#15090,.F.);
#15666=ADVANCED_FACE('',(#2459),#15091,.T.);
#15667=ADVANCED_FACE('',(#2460,#1556),#1826,.T.);
#15668=ADVANCED_FACE('',(#2461),#11,.T.);
#15669=ADVANCED_FACE('',(#2462),#1827,.T.);
#15670=ADVANCED_FACE('',(#2463),#12,.T.);
#15671=ADVANCED_FACE('',(#2464),#15092,.T.);
#15672=ADVANCED_FACE('',(#2465),#13,.T.);
#15673=ADVANCED_FACE('',(#2466),#1828,.T.);
#15674=ADVANCED_FACE('',(#2467),#14,.T.);
#15675=ADVANCED_FACE('',(#2468),#15093,.T.);
#15676=ADVANCED_FACE('',(#2469),#15,.T.);
#15677=ADVANCED_FACE('',(#2470),#1829,.T.);
#15678=ADVANCED_FACE('',(#2471),#16,.T.);
#15679=ADVANCED_FACE('',(#2472),#15094,.T.);
#15680=ADVANCED_FACE('',(#2473),#17,.T.);
#15681=ADVANCED_FACE('',(#2474),#1830,.T.);
#15682=ADVANCED_FACE('',(#2475),#18,.T.);
#15683=ADVANCED_FACE('',(#2476),#15095,.T.);
#15684=ADVANCED_FACE('',(#2477),#19,.T.);
#15685=ADVANCED_FACE('',(#2478),#1831,.T.);
#15686=ADVANCED_FACE('',(#2479),#20,.T.);
#15687=ADVANCED_FACE('',(#2480),#15096,.T.);
#15688=ADVANCED_FACE('',(#2481),#21,.T.);
#15689=ADVANCED_FACE('',(#2482),#1832,.T.);
#15690=ADVANCED_FACE('',(#2483),#22,.T.);
#15691=ADVANCED_FACE('',(#2484),#15097,.T.);
#15692=ADVANCED_FACE('',(#2485),#23,.T.);
#15693=ADVANCED_FACE('',(#2486),#1833,.T.);
#15694=ADVANCED_FACE('',(#2487),#24,.T.);
#15695=ADVANCED_FACE('',(#2488),#15098,.T.);
#15696=ADVANCED_FACE('',(#2489),#25,.T.);
#15697=ADVANCED_FACE('',(#2490),#1834,.T.);
#15698=ADVANCED_FACE('',(#2491),#26,.T.);
#15699=ADVANCED_FACE('',(#2492),#15099,.T.);
#15700=ADVANCED_FACE('',(#2493),#27,.T.);
#15701=ADVANCED_FACE('',(#2494),#1835,.T.);
#15702=ADVANCED_FACE('',(#2495),#28,.T.);
#15703=ADVANCED_FACE('',(#2496),#15100,.T.);
#15704=ADVANCED_FACE('',(#2497),#29,.T.);
#15705=ADVANCED_FACE('',(#2498),#1836,.T.);
#15706=ADVANCED_FACE('',(#2499),#30,.T.);
#15707=ADVANCED_FACE('',(#2500),#15101,.T.);
#15708=ADVANCED_FACE('',(#2501),#31,.T.);
#15709=ADVANCED_FACE('',(#2502),#1837,.T.);
#15710=ADVANCED_FACE('',(#2503),#32,.T.);
#15711=ADVANCED_FACE('',(#2504),#15102,.T.);
#15712=ADVANCED_FACE('',(#2505),#33,.T.);
#15713=ADVANCED_FACE('',(#2506),#1838,.T.);
#15714=ADVANCED_FACE('',(#2507),#34,.T.);
#15715=ADVANCED_FACE('',(#2508),#15103,.T.);
#15716=ADVANCED_FACE('',(#2509),#35,.T.);
#15717=ADVANCED_FACE('',(#2510),#1839,.T.);
#15718=ADVANCED_FACE('',(#2511),#36,.T.);
#15719=ADVANCED_FACE('',(#2512),#15104,.T.);
#15720=ADVANCED_FACE('',(#2513),#37,.T.);
#15721=ADVANCED_FACE('',(#2514),#1840,.T.);
#15722=ADVANCED_FACE('',(#2515),#38,.T.);
#15723=ADVANCED_FACE('',(#2516),#15105,.T.);
#15724=ADVANCED_FACE('',(#2517),#39,.T.);
#15725=ADVANCED_FACE('',(#2518),#1841,.T.);
#15726=ADVANCED_FACE('',(#2519),#40,.T.);
#15727=ADVANCED_FACE('',(#2520),#15106,.T.);
#15728=ADVANCED_FACE('',(#2521),#41,.T.);
#15729=ADVANCED_FACE('',(#2522),#1842,.T.);
#15730=ADVANCED_FACE('',(#2523),#42,.T.);
#15731=ADVANCED_FACE('',(#2524),#15107,.T.);
#15732=ADVANCED_FACE('',(#2525),#43,.T.);
#15733=ADVANCED_FACE('',(#2526),#1843,.T.);
#15734=ADVANCED_FACE('',(#2527),#44,.T.);
#15735=ADVANCED_FACE('',(#2528),#15108,.T.);
#15736=ADVANCED_FACE('',(#2529),#45,.T.);
#15737=ADVANCED_FACE('',(#2530),#1844,.T.);
#15738=ADVANCED_FACE('',(#2531),#46,.T.);
#15739=ADVANCED_FACE('',(#2532),#15109,.T.);
#15740=ADVANCED_FACE('',(#2533),#47,.T.);
#15741=ADVANCED_FACE('',(#2534),#1845,.T.);
#15742=ADVANCED_FACE('',(#2535),#48,.T.);
#15743=ADVANCED_FACE('',(#2536),#15110,.T.);
#15744=ADVANCED_FACE('',(#2537),#49,.T.);
#15745=ADVANCED_FACE('',(#2538),#1846,.T.);
#15746=ADVANCED_FACE('',(#2539),#50,.T.);
#15747=ADVANCED_FACE('',(#2540,#1557),#1847,.T.);
#15748=ADVANCED_FACE('',(#2541),#15111,.T.);
#15749=ADVANCED_FACE('',(#2542),#1848,.T.);
#15750=ADVANCED_FACE('',(#2543),#1849,.T.);
#15751=ADVANCED_FACE('',(#2544),#1850,.T.);
#15752=ADVANCED_FACE('',(#2545),#1851,.T.);
#15753=ADVANCED_FACE('',(#2546),#1852,.T.);
#15754=ADVANCED_FACE('',(#2547),#1853,.F.);
#15755=ADVANCED_FACE('',(#2548),#1854,.T.);
#15756=ADVANCED_FACE('',(#2549),#1855,.T.);
#15757=ADVANCED_FACE('',(#2550),#1856,.T.);
#15758=ADVANCED_FACE('',(#2551),#1857,.F.);
#15759=ADVANCED_FACE('',(#2552),#1858,.F.);
#15760=ADVANCED_FACE('',(#2553),#1859,.T.);
#15761=ADVANCED_FACE('',(#2554),#1860,.F.);
#15762=ADVANCED_FACE('',(#2555),#1861,.F.);
#15763=ADVANCED_FACE('',(#2556),#1862,.F.);
#15764=ADVANCED_FACE('',(#2557),#1863,.F.);
#15765=ADVANCED_FACE('',(#2558),#1864,.T.);
#15766=ADVANCED_FACE('',(#2559),#1865,.F.);
#15767=ADVANCED_FACE('',(#2560),#1866,.F.);
#15768=ADVANCED_FACE('',(#2561),#1867,.F.);
#15769=ADVANCED_FACE('',(#2562,#1558,#1559),#15112,.T.);
#15770=ADVANCED_FACE('',(#2563),#1868,.T.);
#15771=ADVANCED_FACE('',(#2564),#1869,.F.);
#15772=ADVANCED_FACE('',(#2565),#1870,.T.);
#15773=ADVANCED_FACE('',(#2566),#15113,.F.);
#15774=ADVANCED_FACE('',(#2567),#1871,.T.);
#15775=ADVANCED_FACE('',(#2568,#1560),#15114,.F.);
#15776=ADVANCED_FACE('',(#2569,#1561),#15115,.T.);
#15777=ADVANCED_FACE('',(#2570,#1562),#1872,.T.);
#15778=ADVANCED_FACE('',(#2571,#1563),#1873,.F.);
#15779=ADVANCED_FACE('',(#2572),#1874,.T.);
#15780=ADVANCED_FACE('',(#2573),#15116,.F.);
#15781=ADVANCED_FACE('',(#2574),#1875,.T.);
#15782=ADVANCED_FACE('',(#2575,#1564),#15117,.F.);
#15783=ADVANCED_FACE('',(#2576,#1565),#15118,.T.);
#15784=ADVANCED_FACE('',(#2577,#1566),#1876,.T.);
#15785=ADVANCED_FACE('',(#2578,#1567),#1877,.F.);
#15786=ADVANCED_FACE('',(#2579),#15119,.F.);
#15787=ADVANCED_FACE('',(#2580),#15120,.T.);
#15788=ADVANCED_FACE('',(#2581,#1568),#1878,.T.);
#15789=ADVANCED_FACE('',(#2582,#1569),#1879,.F.);
#15790=ADVANCED_FACE('',(#2583),#15121,.F.);
#15791=ADVANCED_FACE('',(#2584),#15122,.T.);
#15792=ADVANCED_FACE('',(#2585,#1570),#1880,.T.);
#15793=ADVANCED_FACE('',(#2586,#1571),#1881,.F.);
#15794=ADVANCED_FACE('',(#2587),#15123,.F.);
#15795=ADVANCED_FACE('',(#2588),#15124,.T.);
#15796=ADVANCED_FACE('',(#2589,#1572),#1882,.T.);
#15797=ADVANCED_FACE('',(#2590,#1573),#1883,.F.);
#15798=ADVANCED_FACE('',(#2591),#15125,.F.);
#15799=ADVANCED_FACE('',(#2592),#15126,.T.);
#15800=ADVANCED_FACE('',(#2593,#1574),#1884,.T.);
#15801=ADVANCED_FACE('',(#2594,#1575),#1885,.F.);
#15802=ADVANCED_FACE('',(#2595),#15127,.F.);
#15803=ADVANCED_FACE('',(#2596),#15128,.T.);
#15804=ADVANCED_FACE('',(#2597,#1576),#1886,.T.);
#15805=ADVANCED_FACE('',(#2598,#1577),#1887,.F.);
#15806=ADVANCED_FACE('',(#2599),#1888,.F.);
#15807=ADVANCED_FACE('',(#2600),#1889,.F.);
#15808=ADVANCED_FACE('',(#2601),#1890,.F.);
#15809=ADVANCED_FACE('',(#2602,#1578),#1891,.T.);
#15810=ADVANCED_FACE('',(#2603),#15129,.F.);
#15811=ADVANCED_FACE('',(#2604,#1579),#1892,.F.);
#15812=ADVANCED_FACE('',(#2605),#15130,.T.);
#15813=ADVANCED_FACE('',(#2606),#51,.T.);
#15814=ADVANCED_FACE('',(#2607),#1893,.T.);
#15815=ADVANCED_FACE('',(#2608),#52,.T.);
#15816=ADVANCED_FACE('',(#2609),#15131,.T.);
#15817=ADVANCED_FACE('',(#2610),#53,.T.);
#15818=ADVANCED_FACE('',(#2611),#1894,.T.);
#15819=ADVANCED_FACE('',(#2612),#54,.T.);
#15820=ADVANCED_FACE('',(#2613),#15132,.T.);
#15821=ADVANCED_FACE('',(#2614),#55,.T.);
#15822=ADVANCED_FACE('',(#2615),#1895,.T.);
#15823=ADVANCED_FACE('',(#2616),#56,.T.);
#15824=ADVANCED_FACE('',(#2617),#15133,.T.);
#15825=ADVANCED_FACE('',(#2618),#57,.T.);
#15826=ADVANCED_FACE('',(#2619),#1896,.T.);
#15827=ADVANCED_FACE('',(#2620),#58,.T.);
#15828=ADVANCED_FACE('',(#2621),#15134,.T.);
#15829=ADVANCED_FACE('',(#2622),#59,.T.);
#15830=ADVANCED_FACE('',(#2623),#1897,.T.);
#15831=ADVANCED_FACE('',(#2624),#60,.T.);
#15832=ADVANCED_FACE('',(#2625),#15135,.T.);
#15833=ADVANCED_FACE('',(#2626),#61,.T.);
#15834=ADVANCED_FACE('',(#2627),#1898,.T.);
#15835=ADVANCED_FACE('',(#2628),#62,.T.);
#15836=ADVANCED_FACE('',(#2629),#15136,.T.);
#15837=ADVANCED_FACE('',(#2630),#63,.T.);
#15838=ADVANCED_FACE('',(#2631),#1899,.T.);
#15839=ADVANCED_FACE('',(#2632),#64,.T.);
#15840=ADVANCED_FACE('',(#2633),#15137,.T.);
#15841=ADVANCED_FACE('',(#2634),#65,.T.);
#15842=ADVANCED_FACE('',(#2635),#1900,.T.);
#15843=ADVANCED_FACE('',(#2636),#66,.T.);
#15844=ADVANCED_FACE('',(#2637),#15138,.T.);
#15845=ADVANCED_FACE('',(#2638),#67,.T.);
#15846=ADVANCED_FACE('',(#2639),#1901,.T.);
#15847=ADVANCED_FACE('',(#2640),#68,.T.);
#15848=ADVANCED_FACE('',(#2641),#15139,.T.);
#15849=ADVANCED_FACE('',(#2642),#69,.T.);
#15850=ADVANCED_FACE('',(#2643),#1902,.T.);
#15851=ADVANCED_FACE('',(#2644),#70,.T.);
#15852=ADVANCED_FACE('',(#2645),#15140,.T.);
#15853=ADVANCED_FACE('',(#2646),#71,.T.);
#15854=ADVANCED_FACE('',(#2647),#1903,.T.);
#15855=ADVANCED_FACE('',(#2648),#72,.T.);
#15856=ADVANCED_FACE('',(#2649),#15141,.T.);
#15857=ADVANCED_FACE('',(#2650),#73,.T.);
#15858=ADVANCED_FACE('',(#2651),#1904,.T.);
#15859=ADVANCED_FACE('',(#2652),#74,.T.);
#15860=ADVANCED_FACE('',(#2653),#15142,.T.);
#15861=ADVANCED_FACE('',(#2654),#75,.T.);
#15862=ADVANCED_FACE('',(#2655),#1905,.T.);
#15863=ADVANCED_FACE('',(#2656),#76,.T.);
#15864=ADVANCED_FACE('',(#2657),#15143,.T.);
#15865=ADVANCED_FACE('',(#2658),#77,.T.);
#15866=ADVANCED_FACE('',(#2659),#1906,.T.);
#15867=ADVANCED_FACE('',(#2660),#78,.T.);
#15868=ADVANCED_FACE('',(#2661),#15144,.T.);
#15869=ADVANCED_FACE('',(#2662),#79,.T.);
#15870=ADVANCED_FACE('',(#2663),#1907,.T.);
#15871=ADVANCED_FACE('',(#2664),#80,.T.);
#15872=ADVANCED_FACE('',(#2665),#15145,.T.);
#15873=ADVANCED_FACE('',(#2666),#81,.T.);
#15874=ADVANCED_FACE('',(#2667),#1908,.T.);
#15875=ADVANCED_FACE('',(#2668),#82,.T.);
#15876=ADVANCED_FACE('',(#2669),#15146,.T.);
#15877=ADVANCED_FACE('',(#2670),#83,.T.);
#15878=ADVANCED_FACE('',(#2671),#1909,.T.);
#15879=ADVANCED_FACE('',(#2672),#84,.T.);
#15880=ADVANCED_FACE('',(#2673),#15147,.T.);
#15881=ADVANCED_FACE('',(#2674),#85,.T.);
#15882=ADVANCED_FACE('',(#2675),#1910,.T.);
#15883=ADVANCED_FACE('',(#2676),#86,.T.);
#15884=ADVANCED_FACE('',(#2677),#15148,.T.);
#15885=ADVANCED_FACE('',(#2678),#87,.T.);
#15886=ADVANCED_FACE('',(#2679),#1911,.T.);
#15887=ADVANCED_FACE('',(#2680),#88,.T.);
#15888=ADVANCED_FACE('',(#2681),#15149,.T.);
#15889=ADVANCED_FACE('',(#2682),#89,.T.);
#15890=ADVANCED_FACE('',(#2683),#1912,.T.);
#15891=ADVANCED_FACE('',(#2684),#90,.T.);
#15892=ADVANCED_FACE('',(#2685,#1580),#1913,.T.);
#15893=ADVANCED_FACE('',(#2686),#15150,.T.);
#15894=ADVANCED_FACE('',(#2687),#1914,.F.);
#15895=ADVANCED_FACE('',(#2688),#1915,.T.);
#15896=ADVANCED_FACE('',(#2689),#1916,.F.);
#15897=ADVANCED_FACE('',(#2690),#1917,.F.);
#15898=ADVANCED_FACE('',(#2691),#1918,.F.);
#15899=ADVANCED_FACE('',(#2692,#1581),#15151,.T.);
#15900=ADVANCED_FACE('',(#2693),#1919,.T.);
#15901=ADVANCED_FACE('',(#2694),#1920,.F.);
#15902=ADVANCED_FACE('',(#2695),#1921,.T.);
#15903=ADVANCED_FACE('',(#2696),#15152,.F.);
#15904=ADVANCED_FACE('',(#2697),#1922,.T.);
#15905=ADVANCED_FACE('',(#2698,#1582),#15153,.F.);
#15906=ADVANCED_FACE('',(#2699,#1583),#15154,.T.);
#15907=ADVANCED_FACE('',(#2700,#1584),#1923,.T.);
#15908=ADVANCED_FACE('',(#2701,#1585),#1924,.F.);
#15909=ADVANCED_FACE('',(#2702),#1925,.T.);
#15910=ADVANCED_FACE('',(#2703),#15155,.F.);
#15911=ADVANCED_FACE('',(#2704),#1926,.T.);
#15912=ADVANCED_FACE('',(#2705,#1586),#15156,.F.);
#15913=ADVANCED_FACE('',(#2706,#1587),#15157,.T.);
#15914=ADVANCED_FACE('',(#2707,#1588),#1927,.T.);
#15915=ADVANCED_FACE('',(#2708,#1589),#1928,.F.);
#15916=ADVANCED_FACE('',(#2709),#15158,.F.);
#15917=ADVANCED_FACE('',(#2710),#15159,.T.);
#15918=ADVANCED_FACE('',(#2711,#1590),#1929,.T.);
#15919=ADVANCED_FACE('',(#2712,#1591),#1930,.F.);
#15920=ADVANCED_FACE('',(#2713),#15160,.F.);
#15921=ADVANCED_FACE('',(#2714),#15161,.T.);
#15922=ADVANCED_FACE('',(#2715,#1592),#1931,.T.);
#15923=ADVANCED_FACE('',(#2716,#1593),#1932,.F.);
#15924=ADVANCED_FACE('',(#2717),#15162,.F.);
#15925=ADVANCED_FACE('',(#2718),#15163,.T.);
#15926=ADVANCED_FACE('',(#2719,#1594),#1933,.T.);
#15927=ADVANCED_FACE('',(#2720,#1595),#1934,.F.);
#15928=ADVANCED_FACE('',(#2721),#15164,.F.);
#15929=ADVANCED_FACE('',(#2722),#15165,.T.);
#15930=ADVANCED_FACE('',(#2723,#1596),#1935,.T.);
#15931=ADVANCED_FACE('',(#2724,#1597),#1936,.F.);
#15932=ADVANCED_FACE('',(#2725),#1937,.F.);
#15933=ADVANCED_FACE('',(#2726),#1938,.F.);
#15934=ADVANCED_FACE('',(#2727),#1939,.F.);
#15935=ADVANCED_FACE('',(#2728),#1940,.F.);
#15936=ADVANCED_FACE('',(#2729),#1941,.F.);
#15937=ADVANCED_FACE('',(#2730),#1942,.F.);
#15938=ADVANCED_FACE('',(#2731),#1943,.F.);
#15939=ADVANCED_FACE('',(#2732,#1598),#1944,.T.);
#15940=ADVANCED_FACE('',(#2733),#1116,.T.);
#15941=ADVANCED_FACE('',(#2734),#15166,.T.);
#15942=ADVANCED_FACE('',(#2735),#1117,.T.);
#15943=ADVANCED_FACE('',(#2736),#1945,.T.);
#15944=ADVANCED_FACE('',(#2737),#1946,.F.);
#15945=ADVANCED_FACE('',(#2738),#1947,.F.);
#15946=ADVANCED_FACE('',(#2739),#1948,.F.);
#15947=ADVANCED_FACE('',(#2740,#1599),#1949,.F.);
#15948=ADVANCED_FACE('',(#2741),#15167,.F.);
#15949=ADVANCED_FACE('',(#2742),#15168,.T.);
#15950=ADVANCED_FACE('',(#2743,#1600),#1950,.T.);
#15951=ADVANCED_FACE('',(#2744),#91,.T.);
#15952=ADVANCED_FACE('',(#2745),#92,.T.);
#15953=ADVANCED_FACE('',(#2746),#1951,.T.);
#15954=ADVANCED_FACE('',(#2747),#15169,.T.);
#15955=ADVANCED_FACE('',(#2748),#93,.T.);
#15956=ADVANCED_FACE('',(#2749),#94,.T.);
#15957=ADVANCED_FACE('',(#2750),#1952,.T.);
#15958=ADVANCED_FACE('',(#2751),#15170,.T.);
#15959=ADVANCED_FACE('',(#2752),#95,.T.);
#15960=ADVANCED_FACE('',(#2753),#96,.T.);
#15961=ADVANCED_FACE('',(#2754),#1953,.T.);
#15962=ADVANCED_FACE('',(#2755),#15171,.T.);
#15963=ADVANCED_FACE('',(#2756),#97,.T.);
#15964=ADVANCED_FACE('',(#2757),#98,.T.);
#15965=ADVANCED_FACE('',(#2758),#1954,.T.);
#15966=ADVANCED_FACE('',(#2759),#15172,.T.);
#15967=ADVANCED_FACE('',(#2760),#99,.T.);
#15968=ADVANCED_FACE('',(#2761),#100,.T.);
#15969=ADVANCED_FACE('',(#2762),#1955,.T.);
#15970=ADVANCED_FACE('',(#2763),#15173,.T.);
#15971=ADVANCED_FACE('',(#2764),#101,.T.);
#15972=ADVANCED_FACE('',(#2765),#102,.T.);
#15973=ADVANCED_FACE('',(#2766),#1956,.T.);
#15974=ADVANCED_FACE('',(#2767),#15174,.T.);
#15975=ADVANCED_FACE('',(#2768),#103,.T.);
#15976=ADVANCED_FACE('',(#2769),#104,.T.);
#15977=ADVANCED_FACE('',(#2770),#1957,.T.);
#15978=ADVANCED_FACE('',(#2771),#15175,.T.);
#15979=ADVANCED_FACE('',(#2772),#105,.T.);
#15980=ADVANCED_FACE('',(#2773),#106,.T.);
#15981=ADVANCED_FACE('',(#2774),#1958,.T.);
#15982=ADVANCED_FACE('',(#2775),#15176,.T.);
#15983=ADVANCED_FACE('',(#2776),#107,.T.);
#15984=ADVANCED_FACE('',(#2777),#108,.T.);
#15985=ADVANCED_FACE('',(#2778),#1959,.T.);
#15986=ADVANCED_FACE('',(#2779),#15177,.T.);
#15987=ADVANCED_FACE('',(#2780),#109,.T.);
#15988=ADVANCED_FACE('',(#2781),#110,.T.);
#15989=ADVANCED_FACE('',(#2782),#1960,.T.);
#15990=ADVANCED_FACE('',(#2783),#15178,.T.);
#15991=ADVANCED_FACE('',(#2784),#111,.T.);
#15992=ADVANCED_FACE('',(#2785),#112,.T.);
#15993=ADVANCED_FACE('',(#2786),#1961,.T.);
#15994=ADVANCED_FACE('',(#2787),#15179,.T.);
#15995=ADVANCED_FACE('',(#2788),#113,.T.);
#15996=ADVANCED_FACE('',(#2789),#114,.T.);
#15997=ADVANCED_FACE('',(#2790),#1962,.T.);
#15998=ADVANCED_FACE('',(#2791),#15180,.T.);
#15999=ADVANCED_FACE('',(#2792),#115,.T.);
#16000=ADVANCED_FACE('',(#2793),#116,.T.);
#16001=ADVANCED_FACE('',(#2794),#1963,.T.);
#16002=ADVANCED_FACE('',(#2795),#15181,.T.);
#16003=ADVANCED_FACE('',(#2796),#117,.T.);
#16004=ADVANCED_FACE('',(#2797),#118,.T.);
#16005=ADVANCED_FACE('',(#2798),#1964,.T.);
#16006=ADVANCED_FACE('',(#2799),#15182,.T.);
#16007=ADVANCED_FACE('',(#2800),#119,.T.);
#16008=ADVANCED_FACE('',(#2801),#120,.T.);
#16009=ADVANCED_FACE('',(#2802),#1965,.T.);
#16010=ADVANCED_FACE('',(#2803),#15183,.T.);
#16011=ADVANCED_FACE('',(#2804),#121,.T.);
#16012=ADVANCED_FACE('',(#2805),#122,.T.);
#16013=ADVANCED_FACE('',(#2806),#1966,.T.);
#16014=ADVANCED_FACE('',(#2807),#15184,.T.);
#16015=ADVANCED_FACE('',(#2808),#123,.T.);
#16016=ADVANCED_FACE('',(#2809),#124,.T.);
#16017=ADVANCED_FACE('',(#2810),#1967,.T.);
#16018=ADVANCED_FACE('',(#2811),#15185,.T.);
#16019=ADVANCED_FACE('',(#2812),#125,.T.);
#16020=ADVANCED_FACE('',(#2813),#126,.T.);
#16021=ADVANCED_FACE('',(#2814),#1968,.T.);
#16022=ADVANCED_FACE('',(#2815),#15186,.T.);
#16023=ADVANCED_FACE('',(#2816),#127,.T.);
#16024=ADVANCED_FACE('',(#2817),#128,.T.);
#16025=ADVANCED_FACE('',(#2818),#1969,.T.);
#16026=ADVANCED_FACE('',(#2819),#15187,.T.);
#16027=ADVANCED_FACE('',(#2820),#129,.T.);
#16028=ADVANCED_FACE('',(#2821),#130,.T.);
#16029=ADVANCED_FACE('',(#2822),#1970,.T.);
#16030=ADVANCED_FACE('',(#2823),#15188,.T.);
#16031=ADVANCED_FACE('',(#2824),#131,.T.);
#16032=ADVANCED_FACE('',(#2825),#132,.T.);
#16033=ADVANCED_FACE('',(#2826),#1971,.T.);
#16034=ADVANCED_FACE('',(#2827),#15189,.T.);
#16035=ADVANCED_FACE('',(#2828),#133,.T.);
#16036=ADVANCED_FACE('',(#2829),#134,.T.);
#16037=ADVANCED_FACE('',(#2830),#1972,.T.);
#16038=ADVANCED_FACE('',(#2831),#15190,.T.);
#16039=ADVANCED_FACE('',(#2832),#135,.T.);
#16040=ADVANCED_FACE('',(#2833),#136,.T.);
#16041=ADVANCED_FACE('',(#2834),#1973,.T.);
#16042=ADVANCED_FACE('',(#2835),#15191,.T.);
#16043=ADVANCED_FACE('',(#2836),#137,.T.);
#16044=ADVANCED_FACE('',(#2837),#138,.T.);
#16045=ADVANCED_FACE('',(#2838),#1974,.T.);
#16046=ADVANCED_FACE('',(#2839),#15192,.T.);
#16047=ADVANCED_FACE('',(#2840),#139,.T.);
#16048=ADVANCED_FACE('',(#2841),#140,.T.);
#16049=ADVANCED_FACE('',(#2842),#1975,.T.);
#16050=ADVANCED_FACE('',(#2843),#15193,.T.);
#16051=ADVANCED_FACE('',(#2844),#141,.T.);
#16052=ADVANCED_FACE('',(#2845),#142,.T.);
#16053=ADVANCED_FACE('',(#2846),#1976,.T.);
#16054=ADVANCED_FACE('',(#2847),#15194,.T.);
#16055=ADVANCED_FACE('',(#2848),#143,.T.);
#16056=ADVANCED_FACE('',(#2849),#144,.T.);
#16057=ADVANCED_FACE('',(#2850),#1977,.T.);
#16058=ADVANCED_FACE('',(#2851),#15195,.T.);
#16059=ADVANCED_FACE('',(#2852),#145,.T.);
#16060=ADVANCED_FACE('',(#2853),#146,.T.);
#16061=ADVANCED_FACE('',(#2854),#1978,.T.);
#16062=ADVANCED_FACE('',(#2855),#15196,.T.);
#16063=ADVANCED_FACE('',(#2856),#147,.T.);
#16064=ADVANCED_FACE('',(#2857),#148,.T.);
#16065=ADVANCED_FACE('',(#2858),#1979,.T.);
#16066=ADVANCED_FACE('',(#2859),#15197,.T.);
#16067=ADVANCED_FACE('',(#2860),#149,.T.);
#16068=ADVANCED_FACE('',(#2861),#150,.T.);
#16069=ADVANCED_FACE('',(#2862),#1980,.T.);
#16070=ADVANCED_FACE('',(#2863),#15198,.T.);
#16071=ADVANCED_FACE('',(#2864),#151,.T.);
#16072=ADVANCED_FACE('',(#2865),#152,.T.);
#16073=ADVANCED_FACE('',(#2866),#1981,.T.);
#16074=ADVANCED_FACE('',(#2867),#15199,.T.);
#16075=ADVANCED_FACE('',(#2868),#153,.T.);
#16076=ADVANCED_FACE('',(#2869),#154,.T.);
#16077=ADVANCED_FACE('',(#2870),#1982,.T.);
#16078=ADVANCED_FACE('',(#2871),#15200,.T.);
#16079=ADVANCED_FACE('',(#2872),#155,.T.);
#16080=ADVANCED_FACE('',(#2873),#156,.T.);
#16081=ADVANCED_FACE('',(#2874),#1983,.T.);
#16082=ADVANCED_FACE('',(#2875),#15201,.T.);
#16083=ADVANCED_FACE('',(#2876),#157,.T.);
#16084=ADVANCED_FACE('',(#2877),#158,.T.);
#16085=ADVANCED_FACE('',(#2878),#1984,.T.);
#16086=ADVANCED_FACE('',(#2879),#15202,.T.);
#16087=ADVANCED_FACE('',(#2880),#159,.T.);
#16088=ADVANCED_FACE('',(#2881),#160,.T.);
#16089=ADVANCED_FACE('',(#2882),#1985,.T.);
#16090=ADVANCED_FACE('',(#2883),#15203,.T.);
#16091=ADVANCED_FACE('',(#2884),#161,.T.);
#16092=ADVANCED_FACE('',(#2885),#162,.T.);
#16093=ADVANCED_FACE('',(#2886),#1986,.T.);
#16094=ADVANCED_FACE('',(#2887),#15204,.T.);
#16095=ADVANCED_FACE('',(#2888),#163,.T.);
#16096=ADVANCED_FACE('',(#2889),#164,.T.);
#16097=ADVANCED_FACE('',(#2890),#1987,.T.);
#16098=ADVANCED_FACE('',(#2891),#15205,.T.);
#16099=ADVANCED_FACE('',(#2892),#165,.T.);
#16100=ADVANCED_FACE('',(#2893),#166,.T.);
#16101=ADVANCED_FACE('',(#2894),#1988,.T.);
#16102=ADVANCED_FACE('',(#2895),#15206,.T.);
#16103=ADVANCED_FACE('',(#2896),#167,.T.);
#16104=ADVANCED_FACE('',(#2897),#1989,.T.);
#16105=ADVANCED_FACE('',(#2898),#168,.T.);
#16106=ADVANCED_FACE('',(#2899),#15207,.T.);
#16107=ADVANCED_FACE('',(#2900),#169,.T.);
#16108=ADVANCED_FACE('',(#2901),#170,.T.);
#16109=ADVANCED_FACE('',(#2902),#1990,.T.);
#16110=ADVANCED_FACE('',(#2903,#1601),#1991,.T.);
#16111=ADVANCED_FACE('',(#2904),#15208,.T.);
#16112=ADVANCED_FACE('',(#2905),#1992,.F.);
#16113=ADVANCED_FACE('',(#2906),#1993,.T.);
#16114=ADVANCED_FACE('',(#2907),#1994,.T.);
#16115=ADVANCED_FACE('',(#2908),#1995,.T.);
#16116=ADVANCED_FACE('',(#2909),#1996,.T.);
#16117=ADVANCED_FACE('',(#2910),#1997,.T.);
#16118=ADVANCED_FACE('',(#2911),#1998,.F.);
#16119=ADVANCED_FACE('',(#2912),#1999,.T.);
#16120=ADVANCED_FACE('',(#2913),#2000,.T.);
#16121=ADVANCED_FACE('',(#2914),#2001,.T.);
#16122=CLOSED_SHELL('',(#15209,#15210,#15211,#15212,#15213,#15214,#15215,
#15216,#15217,#15218));
#16123=CLOSED_SHELL('',(#15219,#15220,#15221,#15222,#15223,#15224,#15225,
#15226,#15227,#15228,#15229,#15230,#15231,#15232,#15233,#15234,#15235,#15236,
#15237,#15238,#15239,#15240,#15241,#15242,#15243,#15244,#15245,#15246,#15247,
#15248,#15249,#15250,#15251,#15252,#15253,#15254,#15255,#15256,#15257,#15258,
#15259,#15260,#15261,#15262,#15263,#15264,#15265,#15266,#15267,#15268,#15269,
#15270,#15271,#15272,#15273,#15274,#15275,#15276,#15277,#15278,#15279,#15280,
#15281,#15282,#15283,#15284,#15285,#15286,#15287,#15288,#15289,#15290,#15291,
#15292,#15293,#15294,#15295,#15296,#15297,#15298,#15299,#15300,#15301,#15302,
#15303,#15304,#15305,#15306));
#16124=CLOSED_SHELL('',(#15307,#15308,#15309,#15310,#15311,#15312,#15313,
#15314,#15315,#15316,#15317,#15318,#15319,#15320,#15321,#15322,#15323,#15324,
#15325,#15326,#15327,#15328,#15329,#15330,#15331,#15332,#15333,#15334,#15335,
#15336,#15337,#15338,#15339,#15340,#15341,#15342,#15343,#15344,#15345,#15346,
#15347,#15348,#15349,#15350,#15351,#15352,#15353,#15354,#15355,#15356,#15357,
#15358,#15359,#15360,#15361,#15362,#15363,#15364,#15365,#15366,#15367,#15368,
#15369,#15370,#15371,#15372,#15373,#15374,#15375,#15376,#15377,#15378,#15379,
#15380,#15381,#15382,#15383,#15384,#15385,#15386,#15387,#15388,#15389,#15390));
#16125=CLOSED_SHELL('',(#15391,#15392,#15393));
#16126=CLOSED_SHELL('',(#15394,#15395,#15396));
#16127=CLOSED_SHELL('',(#15397,#15398,#15399));
#16128=CLOSED_SHELL('',(#15400,#15401,#15402));
#16129=CLOSED_SHELL('',(#15403,#15404,#15405,#15406,#15407,#15408,#15409,
#15410,#15411,#15412,#15413,#15414,#15415));
#16130=CLOSED_SHELL('',(#15416,#15417,#15418,#15419,#15420,#15421,#15422,
#15423,#15424,#15425,#15426,#15427,#15428));
#16131=CLOSED_SHELL('',(#15429,#15430,#15431,#15432,#15433,#15434,#15435,
#15436,#15437,#15438));
#16132=CLOSED_SHELL('',(#15439,#15440,#15441,#15442,#15443,#15444,#15445,
#15446,#15447,#15448));
#16133=CLOSED_SHELL('',(#15449,#15450,#15451,#15452,#15453,#15454,#15455,
#15456,#15457,#15458));
#16134=CLOSED_SHELL('',(#15459,#15460,#15461,#15462,#15463,#15464,#15465,
#15466,#15467,#15468));
#16135=CLOSED_SHELL('',(#15469,#15470,#15471,#15472,#15473,#15474,#15475,
#15476,#15477,#15478));
#16136=CLOSED_SHELL('',(#15479,#15480,#15481,#15482,#15483,#15484));
#16137=CLOSED_SHELL('',(#15485,#15486,#15487,#15488,#15489,#15490));
#16138=CLOSED_SHELL('',(#15491,#15492,#15493,#15494,#15495,#15496,#15497,
#15498));
#16139=CLOSED_SHELL('',(#15499,#15500,#15501,#15502,#15503,#15504,#15505,
#15506));
#16140=CLOSED_SHELL('',(#15507,#15508,#15509,#15510,#15511,#15512,#15513,
#15514));
#16141=CLOSED_SHELL('',(#15515,#15516,#15517,#15518,#15519,#15520,#15521,
#15522));
#16142=CLOSED_SHELL('',(#15523));
#16143=CLOSED_SHELL('',(#15524));
#16144=CLOSED_SHELL('',(#15525));
#16145=CLOSED_SHELL('',(#15526));
#16146=CLOSED_SHELL('',(#15527));
#16147=CLOSED_SHELL('',(#15528));
#16148=CLOSED_SHELL('',(#15529));
#16149=CLOSED_SHELL('',(#15530,#15531,#15532,#15533,#15534,#15535,#15536,
#15537,#15538,#15539,#15540,#15541,#15542,#15543,#15544,#15545,#15546));
#16150=CLOSED_SHELL('',(#15547,#15548,#15549,#15550));
#16151=CLOSED_SHELL('',(#15551,#15552,#15553,#15554));
#16152=CLOSED_SHELL('',(#15555,#15556,#15557,#15558,#15559,#15560,#15561,
#15562));
#16153=CLOSED_SHELL('',(#15563,#15564,#15565,#15566,#15567,#15568,#15569,
#15570));
#16154=CLOSED_SHELL('',(#15571));
#16155=CLOSED_SHELL('',(#15572));
#16156=CLOSED_SHELL('',(#15573));
#16157=CLOSED_SHELL('',(#15574));
#16158=CLOSED_SHELL('',(#15575));
#16159=CLOSED_SHELL('',(#15576));
#16160=CLOSED_SHELL('',(#15577));
#16161=CLOSED_SHELL('',(#15578));
#16162=CLOSED_SHELL('',(#15579,#15580,#15581,#15582,#15583,#15584,#15585,
#15586,#15587,#15588,#15589,#15590,#15591,#15592,#15593,#15594,#15595,#15596,
#15597));
#16163=CLOSED_SHELL('',(#15598,#15599,#15600,#15601));
#16164=CLOSED_SHELL('',(#15602,#15603,#15604,#15605));
#16165=CLOSED_SHELL('',(#15606,#15607,#15608,#15609,#15610,#15611,#15612,
#15613,#15614));
#16166=CLOSED_SHELL('',(#15615,#15616,#15617,#15618,#15619,#15620,#15621,
#15622));
#16167=CLOSED_SHELL('',(#15623,#15624,#15625,#15626,#15627,#15628,#15629,
#15630));
#16168=CLOSED_SHELL('',(#15631,#15632,#15633,#15634,#15635,#15636,#15637));
#16169=CLOSED_SHELL('',(#15638,#15639,#15640,#15641,#15642,#15643,#15644));
#16170=CLOSED_SHELL('',(#15645,#15646,#15647,#15648));
#16171=CLOSED_SHELL('',(#15649,#15650,#15651,#15652));
#16172=CLOSED_SHELL('',(#15653,#15654,#15655,#15656));
#16173=CLOSED_SHELL('',(#15657,#15658,#15659,#15660));
#16174=CLOSED_SHELL('',(#15661,#15662,#15663,#15664,#15665,#15666,#15667,
#15668,#15669,#15670,#15671,#15672,#15673,#15674,#15675,#15676,#15677,#15678,
#15679,#15680,#15681,#15682,#15683,#15684,#15685,#15686,#15687,#15688,#15689,
#15690,#15691,#15692,#15693,#15694,#15695,#15696,#15697,#15698,#15699,#15700,
#15701,#15702,#15703,#15704,#15705,#15706,#15707,#15708,#15709,#15710,#15711,
#15712,#15713,#15714,#15715,#15716,#15717,#15718,#15719,#15720,#15721,#15722,
#15723,#15724,#15725,#15726,#15727,#15728,#15729,#15730,#15731,#15732,#15733,
#15734,#15735,#15736,#15737,#15738,#15739,#15740,#15741,#15742,#15743,#15744,
#15745,#15746,#15747,#15748));
#16175=CLOSED_SHELL('',(#15749,#15750,#15751,#15752,#15753,#15754,#15755,
#15756,#15757,#15758));
#16176=CLOSED_SHELL('',(#15759,#15760,#15761,#15762,#15763,#15764,#15765,
#15766,#15767,#15768,#15769,#15770,#15771));
#16177=CLOSED_SHELL('',(#15772,#15773,#15774,#15775,#15776,#15777,#15778));
#16178=CLOSED_SHELL('',(#15779,#15780,#15781,#15782,#15783,#15784,#15785));
#16179=CLOSED_SHELL('',(#15786,#15787,#15788,#15789));
#16180=CLOSED_SHELL('',(#15790,#15791,#15792,#15793));
#16181=CLOSED_SHELL('',(#15794,#15795,#15796,#15797));
#16182=CLOSED_SHELL('',(#15798,#15799,#15800,#15801));
#16183=CLOSED_SHELL('',(#15802,#15803,#15804,#15805));
#16184=CLOSED_SHELL('',(#15806,#15807,#15808,#15809,#15810,#15811,#15812,
#15813,#15814,#15815,#15816,#15817,#15818,#15819,#15820,#15821,#15822,#15823,
#15824,#15825,#15826,#15827,#15828,#15829,#15830,#15831,#15832,#15833,#15834,
#15835,#15836,#15837,#15838,#15839,#15840,#15841,#15842,#15843,#15844,#15845,
#15846,#15847,#15848,#15849,#15850,#15851,#15852,#15853,#15854,#15855,#15856,
#15857,#15858,#15859,#15860,#15861,#15862,#15863,#15864,#15865,#15866,#15867,
#15868,#15869,#15870,#15871,#15872,#15873,#15874,#15875,#15876,#15877,#15878,
#15879,#15880,#15881,#15882,#15883,#15884,#15885,#15886,#15887,#15888,#15889,
#15890,#15891,#15892,#15893));
#16185=CLOSED_SHELL('',(#15894,#15895,#15896,#15897,#15898,#15899,#15900,
#15901));
#16186=CLOSED_SHELL('',(#15902,#15903,#15904,#15905,#15906,#15907,#15908));
#16187=CLOSED_SHELL('',(#15909,#15910,#15911,#15912,#15913,#15914,#15915));
#16188=CLOSED_SHELL('',(#15916,#15917,#15918,#15919));
#16189=CLOSED_SHELL('',(#15920,#15921,#15922,#15923));
#16190=CLOSED_SHELL('',(#15924,#15925,#15926,#15927));
#16191=CLOSED_SHELL('',(#15928,#15929,#15930,#15931));
#16192=CLOSED_SHELL('',(#15932,#15933,#15934,#15935,#15936,#15937,#15938,
#15939,#15940,#15941,#15942,#15943));
#16193=CLOSED_SHELL('',(#15944,#15945,#15946,#15947,#15948,#15949,#15950,
#15951,#15952,#15953,#15954,#15955,#15956,#15957,#15958,#15959,#15960,#15961,
#15962,#15963,#15964,#15965,#15966,#15967,#15968,#15969,#15970,#15971,#15972,
#15973,#15974,#15975,#15976,#15977,#15978,#15979,#15980,#15981,#15982,#15983,
#15984,#15985,#15986,#15987,#15988,#15989,#15990,#15991,#15992,#15993,#15994,
#15995,#15996,#15997,#15998,#15999,#16000,#16001,#16002,#16003,#16004,#16005,
#16006,#16007,#16008,#16009,#16010,#16011,#16012,#16013,#16014,#16015,#16016,
#16017,#16018,#16019,#16020,#16021,#16022,#16023,#16024,#16025,#16026,#16027,
#16028,#16029,#16030,#16031,#16032,#16033,#16034,#16035,#16036,#16037,#16038,
#16039,#16040,#16041,#16042,#16043,#16044,#16045,#16046,#16047,#16048,#16049,
#16050,#16051,#16052,#16053,#16054,#16055,#16056,#16057,#16058,#16059,#16060,
#16061,#16062,#16063,#16064,#16065,#16066,#16067,#16068,#16069,#16070,#16071,
#16072,#16073,#16074,#16075,#16076,#16077,#16078,#16079,#16080,#16081,#16082,
#16083,#16084,#16085,#16086,#16087,#16088,#16089,#16090,#16091,#16092,#16093,
#16094,#16095,#16096,#16097,#16098,#16099,#16100,#16101,#16102,#16103,#16104,
#16105,#16106,#16107,#16108,#16109,#16110,#16111));
#16194=CLOSED_SHELL('',(#16112,#16113,#16114,#16115,#16116,#16117,#16118,
#16119,#16120,#16121));
#16195=DERIVED_UNIT_ELEMENT(#16307,1.);
#16196=DERIVED_UNIT_ELEMENT(#73368,-3.);
#16197=DERIVED_UNIT_ELEMENT(#16307,1.);
#16198=DERIVED_UNIT_ELEMENT(#73368,-3.);
#16199=DERIVED_UNIT_ELEMENT(#16307,1.);
#16200=DERIVED_UNIT_ELEMENT(#73368,-3.);
#16201=DERIVED_UNIT_ELEMENT(#16307,1.);
#16202=DERIVED_UNIT_ELEMENT(#73368,-3.);
#16203=DERIVED_UNIT_ELEMENT(#16307,1.);
#16204=DERIVED_UNIT_ELEMENT(#73368,-3.);
#16205=DERIVED_UNIT_ELEMENT(#16307,1.);
#16206=DERIVED_UNIT_ELEMENT(#73368,-3.);
#16207=DERIVED_UNIT_ELEMENT(#16307,1.);
#16208=DERIVED_UNIT_ELEMENT(#73368,-3.);
#16209=DERIVED_UNIT_ELEMENT(#16307,1.);
#16210=DERIVED_UNIT_ELEMENT(#73368,-3.);
#16211=DERIVED_UNIT_ELEMENT(#16307,1.);
#16212=DERIVED_UNIT_ELEMENT(#73368,-3.);
#16213=DERIVED_UNIT_ELEMENT(#16307,1.);
#16214=DERIVED_UNIT_ELEMENT(#73368,-3.);
#16215=DERIVED_UNIT_ELEMENT(#16307,1.);
#16216=DERIVED_UNIT_ELEMENT(#73368,-3.);
#16217=DERIVED_UNIT_ELEMENT(#16307,1.);
#16218=DERIVED_UNIT_ELEMENT(#73368,-3.);
#16219=DERIVED_UNIT_ELEMENT(#16307,1.);
#16220=DERIVED_UNIT_ELEMENT(#73368,-3.);
#16221=DERIVED_UNIT_ELEMENT(#16307,1.);
#16222=DERIVED_UNIT_ELEMENT(#73368,-3.);
#16223=DERIVED_UNIT_ELEMENT(#16307,1.);
#16224=DERIVED_UNIT_ELEMENT(#73368,-3.);
#16225=DERIVED_UNIT_ELEMENT(#16307,1.);
#16226=DERIVED_UNIT_ELEMENT(#73368,-3.);
#16227=DERIVED_UNIT_ELEMENT(#16307,1.);
#16228=DERIVED_UNIT_ELEMENT(#73368,-3.);
#16229=DERIVED_UNIT_ELEMENT(#16307,1.);
#16230=DERIVED_UNIT_ELEMENT(#73368,-3.);
#16231=DERIVED_UNIT_ELEMENT(#16307,1.);
#16232=DERIVED_UNIT_ELEMENT(#73368,-3.);
#16233=DERIVED_UNIT_ELEMENT(#16307,1.);
#16234=DERIVED_UNIT_ELEMENT(#73368,-3.);
#16235=DERIVED_UNIT_ELEMENT(#16307,1.);
#16236=DERIVED_UNIT_ELEMENT(#73368,-3.);
#16237=DERIVED_UNIT_ELEMENT(#16307,1.);
#16238=DERIVED_UNIT_ELEMENT(#73368,-3.);
#16239=DERIVED_UNIT_ELEMENT(#16307,1.);
#16240=DERIVED_UNIT_ELEMENT(#73368,-3.);
#16241=DERIVED_UNIT_ELEMENT(#16307,1.);
#16242=DERIVED_UNIT_ELEMENT(#73368,-3.);
#16243=DERIVED_UNIT_ELEMENT(#16307,1.);
#16244=DERIVED_UNIT_ELEMENT(#73368,-3.);
#16245=DERIVED_UNIT_ELEMENT(#16307,1.);
#16246=DERIVED_UNIT_ELEMENT(#73368,-3.);
#16247=DERIVED_UNIT_ELEMENT(#16307,1.);
#16248=DERIVED_UNIT_ELEMENT(#73368,-3.);
#16249=DERIVED_UNIT_ELEMENT(#16307,1.);
#16250=DERIVED_UNIT_ELEMENT(#73368,-3.);
#16251=DERIVED_UNIT_ELEMENT(#16307,1.);
#16252=DERIVED_UNIT_ELEMENT(#73368,-3.);
#16253=DERIVED_UNIT_ELEMENT(#16307,1.);
#16254=DERIVED_UNIT_ELEMENT(#73368,-3.);
#16255=DERIVED_UNIT_ELEMENT(#16307,1.);
#16256=DERIVED_UNIT_ELEMENT(#73368,-3.);
#16257=DERIVED_UNIT_ELEMENT(#16307,1.);
#16258=DERIVED_UNIT_ELEMENT(#73368,-3.);
#16259=DERIVED_UNIT_ELEMENT(#16307,1.);
#16260=DERIVED_UNIT_ELEMENT(#73368,-3.);
#16261=DERIVED_UNIT_ELEMENT(#16307,1.);
#16262=DERIVED_UNIT_ELEMENT(#73368,-3.);
#16263=DERIVED_UNIT_ELEMENT(#16307,1.);
#16264=DERIVED_UNIT_ELEMENT(#73368,-3.);
#16265=DERIVED_UNIT_ELEMENT(#16307,1.);
#16266=DERIVED_UNIT_ELEMENT(#73368,-3.);
#16267=DERIVED_UNIT_ELEMENT(#16307,1.);
#16268=DERIVED_UNIT_ELEMENT(#73368,-3.);
#16269=DERIVED_UNIT_ELEMENT(#16307,1.);
#16270=DERIVED_UNIT_ELEMENT(#73368,-3.);
#16271=DERIVED_UNIT_ELEMENT(#16307,1.);
#16272=DERIVED_UNIT_ELEMENT(#73368,-3.);
#16273=DERIVED_UNIT_ELEMENT(#16307,1.);
#16274=DERIVED_UNIT_ELEMENT(#73368,-3.);
#16275=DERIVED_UNIT_ELEMENT(#16307,1.);
#16276=DERIVED_UNIT_ELEMENT(#73368,-3.);
#16277=DERIVED_UNIT_ELEMENT(#16307,1.);
#16278=DERIVED_UNIT_ELEMENT(#73368,-3.);
#16279=DERIVED_UNIT_ELEMENT(#16307,1.);
#16280=DERIVED_UNIT_ELEMENT(#73368,-3.);
#16281=DERIVED_UNIT_ELEMENT(#16307,1.);
#16282=DERIVED_UNIT_ELEMENT(#73368,-3.);
#16283=DERIVED_UNIT_ELEMENT(#16307,1.);
#16284=DERIVED_UNIT_ELEMENT(#73368,-3.);
#16285=DERIVED_UNIT_ELEMENT(#16307,1.);
#16286=DERIVED_UNIT_ELEMENT(#73368,-3.);
#16287=DERIVED_UNIT_ELEMENT(#16307,1.);
#16288=DERIVED_UNIT_ELEMENT(#73368,-3.);
#16289=DERIVED_UNIT_ELEMENT(#16307,1.);
#16290=DERIVED_UNIT_ELEMENT(#73368,-3.);
#16291=DERIVED_UNIT_ELEMENT(#16307,1.);
#16292=DERIVED_UNIT_ELEMENT(#73368,-3.);
#16293=DERIVED_UNIT_ELEMENT(#16307,1.);
#16294=DERIVED_UNIT_ELEMENT(#73368,-3.);
#16295=DERIVED_UNIT_ELEMENT(#16307,1.);
#16296=DERIVED_UNIT_ELEMENT(#73368,-3.);
#16297=DERIVED_UNIT_ELEMENT(#16307,1.);
#16298=DERIVED_UNIT_ELEMENT(#73368,-3.);
#16299=DERIVED_UNIT_ELEMENT(#16307,1.);
#16300=DERIVED_UNIT_ELEMENT(#73368,-3.);
#16301=DERIVED_UNIT_ELEMENT(#16307,1.);
#16302=DERIVED_UNIT_ELEMENT(#73368,-3.);
#16303=DERIVED_UNIT_ELEMENT(#16307,1.);
#16304=DERIVED_UNIT_ELEMENT(#73368,-3.);
#16305=DERIVED_UNIT_ELEMENT(#16307,1.);
#16306=DERIVED_UNIT_ELEMENT(#73368,-3.);
#16307=(
MASS_UNIT()
NAMED_UNIT(*)
SI_UNIT(.KILO.,.GRAM.)
);
#16308=DERIVED_UNIT((#16195,#16196));
#16309=DERIVED_UNIT((#16197,#16198));
#16310=DERIVED_UNIT((#16199,#16200));
#16311=DERIVED_UNIT((#16201,#16202));
#16312=DERIVED_UNIT((#16203,#16204));
#16313=DERIVED_UNIT((#16205,#16206));
#16314=DERIVED_UNIT((#16207,#16208));
#16315=DERIVED_UNIT((#16209,#16210));
#16316=DERIVED_UNIT((#16211,#16212));
#16317=DERIVED_UNIT((#16213,#16214));
#16318=DERIVED_UNIT((#16215,#16216));
#16319=DERIVED_UNIT((#16217,#16218));
#16320=DERIVED_UNIT((#16219,#16220));
#16321=DERIVED_UNIT((#16221,#16222));
#16322=DERIVED_UNIT((#16223,#16224));
#16323=DERIVED_UNIT((#16225,#16226));
#16324=DERIVED_UNIT((#16227,#16228));
#16325=DERIVED_UNIT((#16229,#16230));
#16326=DERIVED_UNIT((#16231,#16232));
#16327=DERIVED_UNIT((#16233,#16234));
#16328=DERIVED_UNIT((#16235,#16236));
#16329=DERIVED_UNIT((#16237,#16238));
#16330=DERIVED_UNIT((#16239,#16240));
#16331=DERIVED_UNIT((#16241,#16242));
#16332=DERIVED_UNIT((#16243,#16244));
#16333=DERIVED_UNIT((#16245,#16246));
#16334=DERIVED_UNIT((#16247,#16248));
#16335=DERIVED_UNIT((#16249,#16250));
#16336=DERIVED_UNIT((#16251,#16252));
#16337=DERIVED_UNIT((#16253,#16254));
#16338=DERIVED_UNIT((#16255,#16256));
#16339=DERIVED_UNIT((#16257,#16258));
#16340=DERIVED_UNIT((#16259,#16260));
#16341=DERIVED_UNIT((#16261,#16262));
#16342=DERIVED_UNIT((#16263,#16264));
#16343=DERIVED_UNIT((#16265,#16266));
#16344=DERIVED_UNIT((#16267,#16268));
#16345=DERIVED_UNIT((#16269,#16270));
#16346=DERIVED_UNIT((#16271,#16272));
#16347=DERIVED_UNIT((#16273,#16274));
#16348=DERIVED_UNIT((#16275,#16276));
#16349=DERIVED_UNIT((#16277,#16278));
#16350=DERIVED_UNIT((#16279,#16280));
#16351=DERIVED_UNIT((#16281,#16282));
#16352=DERIVED_UNIT((#16283,#16284));
#16353=DERIVED_UNIT((#16285,#16286));
#16354=DERIVED_UNIT((#16287,#16288));
#16355=DERIVED_UNIT((#16289,#16290));
#16356=DERIVED_UNIT((#16291,#16292));
#16357=DERIVED_UNIT((#16293,#16294));
#16358=DERIVED_UNIT((#16295,#16296));
#16359=DERIVED_UNIT((#16297,#16298));
#16360=DERIVED_UNIT((#16299,#16300));
#16361=DERIVED_UNIT((#16301,#16302));
#16362=DERIVED_UNIT((#16303,#16304));
#16363=DERIVED_UNIT((#16305,#16306));
#16364=MEASURE_REPRESENTATION_ITEM('density measure',
POSITIVE_RATIO_MEASURE(7850.),#16308);
#16365=MEASURE_REPRESENTATION_ITEM('density measure',
POSITIVE_RATIO_MEASURE(7850.),#16309);
#16366=MEASURE_REPRESENTATION_ITEM('density measure',
POSITIVE_RATIO_MEASURE(7850.),#16310);
#16367=MEASURE_REPRESENTATION_ITEM('density measure',
POSITIVE_RATIO_MEASURE(7850.),#16311);
#16368=MEASURE_REPRESENTATION_ITEM('density measure',
POSITIVE_RATIO_MEASURE(7850.),#16312);
#16369=MEASURE_REPRESENTATION_ITEM('density measure',
POSITIVE_RATIO_MEASURE(7850.),#16313);
#16370=MEASURE_REPRESENTATION_ITEM('density measure',
POSITIVE_RATIO_MEASURE(7850.),#16314);
#16371=MEASURE_REPRESENTATION_ITEM('density measure',
POSITIVE_RATIO_MEASURE(7850.),#16315);
#16372=MEASURE_REPRESENTATION_ITEM('density measure',
POSITIVE_RATIO_MEASURE(7850.),#16316);
#16373=MEASURE_REPRESENTATION_ITEM('density measure',
POSITIVE_RATIO_MEASURE(7850.),#16317);
#16374=MEASURE_REPRESENTATION_ITEM('density measure',
POSITIVE_RATIO_MEASURE(7850.),#16318);
#16375=MEASURE_REPRESENTATION_ITEM('density measure',
POSITIVE_RATIO_MEASURE(7850.),#16319);
#16376=MEASURE_REPRESENTATION_ITEM('density measure',
POSITIVE_RATIO_MEASURE(7850.),#16320);
#16377=MEASURE_REPRESENTATION_ITEM('density measure',
POSITIVE_RATIO_MEASURE(7850.),#16321);
#16378=MEASURE_REPRESENTATION_ITEM('density measure',
POSITIVE_RATIO_MEASURE(7850.),#16322);
#16379=MEASURE_REPRESENTATION_ITEM('density measure',
POSITIVE_RATIO_MEASURE(7850.),#16323);
#16380=MEASURE_REPRESENTATION_ITEM('density measure',
POSITIVE_RATIO_MEASURE(7850.),#16324);
#16381=MEASURE_REPRESENTATION_ITEM('density measure',
POSITIVE_RATIO_MEASURE(7850.),#16325);
#16382=MEASURE_REPRESENTATION_ITEM('density measure',
POSITIVE_RATIO_MEASURE(7850.),#16326);
#16383=MEASURE_REPRESENTATION_ITEM('density measure',
POSITIVE_RATIO_MEASURE(7850.),#16327);
#16384=MEASURE_REPRESENTATION_ITEM('density measure',
POSITIVE_RATIO_MEASURE(7850.),#16328);
#16385=MEASURE_REPRESENTATION_ITEM('density measure',
POSITIVE_RATIO_MEASURE(7850.),#16329);
#16386=MEASURE_REPRESENTATION_ITEM('density measure',
POSITIVE_RATIO_MEASURE(7850.),#16330);
#16387=MEASURE_REPRESENTATION_ITEM('density measure',
POSITIVE_RATIO_MEASURE(7850.),#16331);
#16388=MEASURE_REPRESENTATION_ITEM('density measure',
POSITIVE_RATIO_MEASURE(7850.),#16332);
#16389=MEASURE_REPRESENTATION_ITEM('density measure',
POSITIVE_RATIO_MEASURE(7850.),#16333);
#16390=MEASURE_REPRESENTATION_ITEM('density measure',
POSITIVE_RATIO_MEASURE(7850.),#16334);
#16391=MEASURE_REPRESENTATION_ITEM('density measure',
POSITIVE_RATIO_MEASURE(7850.),#16335);
#16392=MEASURE_REPRESENTATION_ITEM('density measure',
POSITIVE_RATIO_MEASURE(7850.),#16336);
#16393=MEASURE_REPRESENTATION_ITEM('density measure',
POSITIVE_RATIO_MEASURE(7850.),#16337);
#16394=MEASURE_REPRESENTATION_ITEM('density measure',
POSITIVE_RATIO_MEASURE(7850.),#16338);
#16395=MEASURE_REPRESENTATION_ITEM('density measure',
POSITIVE_RATIO_MEASURE(7850.),#16339);
#16396=MEASURE_REPRESENTATION_ITEM('density measure',
POSITIVE_RATIO_MEASURE(7850.),#16340);
#16397=MEASURE_REPRESENTATION_ITEM('density measure',
POSITIVE_RATIO_MEASURE(7850.),#16341);
#16398=MEASURE_REPRESENTATION_ITEM('density measure',
POSITIVE_RATIO_MEASURE(7850.),#16342);
#16399=MEASURE_REPRESENTATION_ITEM('density measure',
POSITIVE_RATIO_MEASURE(7850.),#16343);
#16400=MEASURE_REPRESENTATION_ITEM('density measure',
POSITIVE_RATIO_MEASURE(7850.),#16344);
#16401=MEASURE_REPRESENTATION_ITEM('density measure',
POSITIVE_RATIO_MEASURE(7850.),#16345);
#16402=MEASURE_REPRESENTATION_ITEM('density measure',
POSITIVE_RATIO_MEASURE(7850.),#16346);
#16403=MEASURE_REPRESENTATION_ITEM('density measure',
POSITIVE_RATIO_MEASURE(7850.),#16347);
#16404=MEASURE_REPRESENTATION_ITEM('density measure',
POSITIVE_RATIO_MEASURE(7850.),#16348);
#16405=MEASURE_REPRESENTATION_ITEM('density measure',
POSITIVE_RATIO_MEASURE(7850.),#16349);
#16406=MEASURE_REPRESENTATION_ITEM('density measure',
POSITIVE_RATIO_MEASURE(7850.),#16350);
#16407=MEASURE_REPRESENTATION_ITEM('density measure',
POSITIVE_RATIO_MEASURE(7850.),#16351);
#16408=MEASURE_REPRESENTATION_ITEM('density measure',
POSITIVE_RATIO_MEASURE(7850.),#16352);
#16409=MEASURE_REPRESENTATION_ITEM('density measure',
POSITIVE_RATIO_MEASURE(7850.),#16353);
#16410=MEASURE_REPRESENTATION_ITEM('density measure',
POSITIVE_RATIO_MEASURE(7850.),#16354);
#16411=MEASURE_REPRESENTATION_ITEM('density measure',
POSITIVE_RATIO_MEASURE(7850.),#16355);
#16412=MEASURE_REPRESENTATION_ITEM('density measure',
POSITIVE_RATIO_MEASURE(7850.),#16356);
#16413=MEASURE_REPRESENTATION_ITEM('density measure',
POSITIVE_RATIO_MEASURE(7850.),#16357);
#16414=MEASURE_REPRESENTATION_ITEM('density measure',
POSITIVE_RATIO_MEASURE(7850.),#16358);
#16415=MEASURE_REPRESENTATION_ITEM('density measure',
POSITIVE_RATIO_MEASURE(7850.),#16359);
#16416=MEASURE_REPRESENTATION_ITEM('density measure',
POSITIVE_RATIO_MEASURE(7850.),#16360);
#16417=MEASURE_REPRESENTATION_ITEM('density measure',
POSITIVE_RATIO_MEASURE(7850.),#16361);
#16418=MEASURE_REPRESENTATION_ITEM('density measure',
POSITIVE_RATIO_MEASURE(7850.),#16362);
#16419=MEASURE_REPRESENTATION_ITEM('density measure',
POSITIVE_RATIO_MEASURE(7850.),#16363);
#16420=PROPERTY_DEFINITION_REPRESENTATION(#16700,#16532);
#16421=PROPERTY_DEFINITION_REPRESENTATION(#16701,#16533);
#16422=PROPERTY_DEFINITION_REPRESENTATION(#16702,#16534);
#16423=PROPERTY_DEFINITION_REPRESENTATION(#16703,#16535);
#16424=PROPERTY_DEFINITION_REPRESENTATION(#16704,#16536);
#16425=PROPERTY_DEFINITION_REPRESENTATION(#16705,#16537);
#16426=PROPERTY_DEFINITION_REPRESENTATION(#16706,#16538);
#16427=PROPERTY_DEFINITION_REPRESENTATION(#16707,#16539);
#16428=PROPERTY_DEFINITION_REPRESENTATION(#16708,#16540);
#16429=PROPERTY_DEFINITION_REPRESENTATION(#16709,#16541);
#16430=PROPERTY_DEFINITION_REPRESENTATION(#16710,#16542);
#16431=PROPERTY_DEFINITION_REPRESENTATION(#16711,#16543);
#16432=PROPERTY_DEFINITION_REPRESENTATION(#16712,#16544);
#16433=PROPERTY_DEFINITION_REPRESENTATION(#16713,#16545);
#16434=PROPERTY_DEFINITION_REPRESENTATION(#16714,#16546);
#16435=PROPERTY_DEFINITION_REPRESENTATION(#16715,#16547);
#16436=PROPERTY_DEFINITION_REPRESENTATION(#16716,#16548);
#16437=PROPERTY_DEFINITION_REPRESENTATION(#16717,#16549);
#16438=PROPERTY_DEFINITION_REPRESENTATION(#16718,#16550);
#16439=PROPERTY_DEFINITION_REPRESENTATION(#16719,#16551);
#16440=PROPERTY_DEFINITION_REPRESENTATION(#16720,#16552);
#16441=PROPERTY_DEFINITION_REPRESENTATION(#16721,#16553);
#16442=PROPERTY_DEFINITION_REPRESENTATION(#16722,#16554);
#16443=PROPERTY_DEFINITION_REPRESENTATION(#16723,#16555);
#16444=PROPERTY_DEFINITION_REPRESENTATION(#16724,#16556);
#16445=PROPERTY_DEFINITION_REPRESENTATION(#16725,#16557);
#16446=PROPERTY_DEFINITION_REPRESENTATION(#16726,#16558);
#16447=PROPERTY_DEFINITION_REPRESENTATION(#16727,#16559);
#16448=PROPERTY_DEFINITION_REPRESENTATION(#16728,#16560);
#16449=PROPERTY_DEFINITION_REPRESENTATION(#16729,#16561);
#16450=PROPERTY_DEFINITION_REPRESENTATION(#16730,#16562);
#16451=PROPERTY_DEFINITION_REPRESENTATION(#16731,#16563);
#16452=PROPERTY_DEFINITION_REPRESENTATION(#16732,#16564);
#16453=PROPERTY_DEFINITION_REPRESENTATION(#16733,#16565);
#16454=PROPERTY_DEFINITION_REPRESENTATION(#16734,#16566);
#16455=PROPERTY_DEFINITION_REPRESENTATION(#16735,#16567);
#16456=PROPERTY_DEFINITION_REPRESENTATION(#16736,#16568);
#16457=PROPERTY_DEFINITION_REPRESENTATION(#16737,#16569);
#16458=PROPERTY_DEFINITION_REPRESENTATION(#16738,#16570);
#16459=PROPERTY_DEFINITION_REPRESENTATION(#16739,#16571);
#16460=PROPERTY_DEFINITION_REPRESENTATION(#16740,#16572);
#16461=PROPERTY_DEFINITION_REPRESENTATION(#16741,#16573);
#16462=PROPERTY_DEFINITION_REPRESENTATION(#16742,#16574);
#16463=PROPERTY_DEFINITION_REPRESENTATION(#16743,#16575);
#16464=PROPERTY_DEFINITION_REPRESENTATION(#16744,#16576);
#16465=PROPERTY_DEFINITION_REPRESENTATION(#16745,#16577);
#16466=PROPERTY_DEFINITION_REPRESENTATION(#16746,#16578);
#16467=PROPERTY_DEFINITION_REPRESENTATION(#16747,#16579);
#16468=PROPERTY_DEFINITION_REPRESENTATION(#16748,#16580);
#16469=PROPERTY_DEFINITION_REPRESENTATION(#16749,#16581);
#16470=PROPERTY_DEFINITION_REPRESENTATION(#16750,#16582);
#16471=PROPERTY_DEFINITION_REPRESENTATION(#16751,#16583);
#16472=PROPERTY_DEFINITION_REPRESENTATION(#16752,#16584);
#16473=PROPERTY_DEFINITION_REPRESENTATION(#16753,#16585);
#16474=PROPERTY_DEFINITION_REPRESENTATION(#16754,#16586);
#16475=PROPERTY_DEFINITION_REPRESENTATION(#16755,#16587);
#16476=PROPERTY_DEFINITION_REPRESENTATION(#16756,#16588);
#16477=PROPERTY_DEFINITION_REPRESENTATION(#16757,#16589);
#16478=PROPERTY_DEFINITION_REPRESENTATION(#16758,#16590);
#16479=PROPERTY_DEFINITION_REPRESENTATION(#16759,#16591);
#16480=PROPERTY_DEFINITION_REPRESENTATION(#16760,#16592);
#16481=PROPERTY_DEFINITION_REPRESENTATION(#16761,#16593);
#16482=PROPERTY_DEFINITION_REPRESENTATION(#16762,#16594);
#16483=PROPERTY_DEFINITION_REPRESENTATION(#16763,#16595);
#16484=PROPERTY_DEFINITION_REPRESENTATION(#16764,#16596);
#16485=PROPERTY_DEFINITION_REPRESENTATION(#16765,#16597);
#16486=PROPERTY_DEFINITION_REPRESENTATION(#16766,#16598);
#16487=PROPERTY_DEFINITION_REPRESENTATION(#16767,#16599);
#16488=PROPERTY_DEFINITION_REPRESENTATION(#16768,#16600);
#16489=PROPERTY_DEFINITION_REPRESENTATION(#16769,#16601);
#16490=PROPERTY_DEFINITION_REPRESENTATION(#16770,#16602);
#16491=PROPERTY_DEFINITION_REPRESENTATION(#16771,#16603);
#16492=PROPERTY_DEFINITION_REPRESENTATION(#16772,#16604);
#16493=PROPERTY_DEFINITION_REPRESENTATION(#16773,#16605);
#16494=PROPERTY_DEFINITION_REPRESENTATION(#16774,#16606);
#16495=PROPERTY_DEFINITION_REPRESENTATION(#16775,#16607);
#16496=PROPERTY_DEFINITION_REPRESENTATION(#16776,#16608);
#16497=PROPERTY_DEFINITION_REPRESENTATION(#16777,#16609);
#16498=PROPERTY_DEFINITION_REPRESENTATION(#16778,#16610);
#16499=PROPERTY_DEFINITION_REPRESENTATION(#16779,#16611);
#16500=PROPERTY_DEFINITION_REPRESENTATION(#16780,#16612);
#16501=PROPERTY_DEFINITION_REPRESENTATION(#16781,#16613);
#16502=PROPERTY_DEFINITION_REPRESENTATION(#16782,#16614);
#16503=PROPERTY_DEFINITION_REPRESENTATION(#16783,#16615);
#16504=PROPERTY_DEFINITION_REPRESENTATION(#16784,#16616);
#16505=PROPERTY_DEFINITION_REPRESENTATION(#16785,#16617);
#16506=PROPERTY_DEFINITION_REPRESENTATION(#16786,#16618);
#16507=PROPERTY_DEFINITION_REPRESENTATION(#16787,#16619);
#16508=PROPERTY_DEFINITION_REPRESENTATION(#16788,#16620);
#16509=PROPERTY_DEFINITION_REPRESENTATION(#16789,#16621);
#16510=PROPERTY_DEFINITION_REPRESENTATION(#16790,#16622);
#16511=PROPERTY_DEFINITION_REPRESENTATION(#16791,#16623);
#16512=PROPERTY_DEFINITION_REPRESENTATION(#16792,#16624);
#16513=PROPERTY_DEFINITION_REPRESENTATION(#16793,#16625);
#16514=PROPERTY_DEFINITION_REPRESENTATION(#16794,#16626);
#16515=PROPERTY_DEFINITION_REPRESENTATION(#16795,#16627);
#16516=PROPERTY_DEFINITION_REPRESENTATION(#16796,#16628);
#16517=PROPERTY_DEFINITION_REPRESENTATION(#16797,#16629);
#16518=PROPERTY_DEFINITION_REPRESENTATION(#16798,#16630);
#16519=PROPERTY_DEFINITION_REPRESENTATION(#16799,#16631);
#16520=PROPERTY_DEFINITION_REPRESENTATION(#16800,#16632);
#16521=PROPERTY_DEFINITION_REPRESENTATION(#16801,#16633);
#16522=PROPERTY_DEFINITION_REPRESENTATION(#16802,#16634);
#16523=PROPERTY_DEFINITION_REPRESENTATION(#16803,#16635);
#16524=PROPERTY_DEFINITION_REPRESENTATION(#16804,#16636);
#16525=PROPERTY_DEFINITION_REPRESENTATION(#16805,#16637);
#16526=PROPERTY_DEFINITION_REPRESENTATION(#16806,#16638);
#16527=PROPERTY_DEFINITION_REPRESENTATION(#16807,#16639);
#16528=PROPERTY_DEFINITION_REPRESENTATION(#16808,#16640);
#16529=PROPERTY_DEFINITION_REPRESENTATION(#16809,#16641);
#16530=PROPERTY_DEFINITION_REPRESENTATION(#16810,#16642);
#16531=PROPERTY_DEFINITION_REPRESENTATION(#16811,#16643);
#16532=REPRESENTATION('material name',(#16644),#73305);
#16533=REPRESENTATION('density',(#16364),#73305);
#16534=REPRESENTATION('material name',(#16645),#73306);
#16535=REPRESENTATION('density',(#16365),#73306);
#16536=REPRESENTATION('material name',(#16646),#73307);
#16537=REPRESENTATION('density',(#16366),#73307);
#16538=REPRESENTATION('material name',(#16647),#73308);
#16539=REPRESENTATION('density',(#16367),#73308);
#16540=REPRESENTATION('material name',(#16648),#73309);
#16541=REPRESENTATION('density',(#16368),#73309);
#16542=REPRESENTATION('material name',(#16649),#73310);
#16543=REPRESENTATION('density',(#16369),#73310);
#16544=REPRESENTATION('material name',(#16650),#73311);
#16545=REPRESENTATION('density',(#16370),#73311);
#16546=REPRESENTATION('material name',(#16651),#73312);
#16547=REPRESENTATION('density',(#16371),#73312);
#16548=REPRESENTATION('material name',(#16652),#73313);
#16549=REPRESENTATION('density',(#16372),#73313);
#16550=REPRESENTATION('material name',(#16653),#73314);
#16551=REPRESENTATION('density',(#16373),#73314);
#16552=REPRESENTATION('material name',(#16654),#73315);
#16553=REPRESENTATION('density',(#16374),#73315);
#16554=REPRESENTATION('material name',(#16655),#73316);
#16555=REPRESENTATION('density',(#16375),#73316);
#16556=REPRESENTATION('material name',(#16656),#73317);
#16557=REPRESENTATION('density',(#16376),#73317);
#16558=REPRESENTATION('material name',(#16657),#73318);
#16559=REPRESENTATION('density',(#16377),#73318);
#16560=REPRESENTATION('material name',(#16658),#73319);
#16561=REPRESENTATION('density',(#16378),#73319);
#16562=REPRESENTATION('material name',(#16659),#73320);
#16563=REPRESENTATION('density',(#16379),#73320);
#16564=REPRESENTATION('material name',(#16660),#73321);
#16565=REPRESENTATION('density',(#16380),#73321);
#16566=REPRESENTATION('material name',(#16661),#73323);
#16567=REPRESENTATION('density',(#16381),#73323);
#16568=REPRESENTATION('material name',(#16662),#73324);
#16569=REPRESENTATION('density',(#16382),#73324);
#16570=REPRESENTATION('material name',(#16663),#73325);
#16571=REPRESENTATION('density',(#16383),#73325);
#16572=REPRESENTATION('material name',(#16664),#73326);
#16573=REPRESENTATION('density',(#16384),#73326);
#16574=REPRESENTATION('material name',(#16665),#73327);
#16575=REPRESENTATION('density',(#16385),#73327);
#16576=REPRESENTATION('material name',(#16666),#73329);
#16577=REPRESENTATION('density',(#16386),#73329);
#16578=REPRESENTATION('material name',(#16667),#73330);
#16579=REPRESENTATION('density',(#16387),#73330);
#16580=REPRESENTATION('material name',(#16668),#73331);
#16581=REPRESENTATION('density',(#16388),#73331);
#16582=REPRESENTATION('material name',(#16669),#73332);
#16583=REPRESENTATION('density',(#16389),#73332);
#16584=REPRESENTATION('material name',(#16670),#73333);
#16585=REPRESENTATION('density',(#16390),#73333);
#16586=REPRESENTATION('material name',(#16671),#73334);
#16587=REPRESENTATION('density',(#16391),#73334);
#16588=REPRESENTATION('material name',(#16672),#73336);
#16589=REPRESENTATION('density',(#16392),#73336);
#16590=REPRESENTATION('material name',(#16673),#73337);
#16591=REPRESENTATION('density',(#16393),#73337);
#16592=REPRESENTATION('material name',(#16674),#73338);
#16593=REPRESENTATION('density',(#16394),#73338);
#16594=REPRESENTATION('material name',(#16675),#73339);
#16595=REPRESENTATION('density',(#16395),#73339);
#16596=REPRESENTATION('material name',(#16676),#73340);
#16597=REPRESENTATION('density',(#16396),#73340);
#16598=REPRESENTATION('material name',(#16677),#73341);
#16599=REPRESENTATION('density',(#16397),#73341);
#16600=REPRESENTATION('material name',(#16678),#73342);
#16601=REPRESENTATION('density',(#16398),#73342);
#16602=REPRESENTATION('material name',(#16679),#73343);
#16603=REPRESENTATION('density',(#16399),#73343);
#16604=REPRESENTATION('material name',(#16680),#73344);
#16605=REPRESENTATION('density',(#16400),#73344);
#16606=REPRESENTATION('material name',(#16681),#73346);
#16607=REPRESENTATION('density',(#16401),#73346);
#16608=REPRESENTATION('material name',(#16682),#73347);
#16609=REPRESENTATION('density',(#16402),#73347);
#16610=REPRESENTATION('material name',(#16683),#73348);
#16611=REPRESENTATION('density',(#16403),#73348);
#16612=REPRESENTATION('material name',(#16684),#73349);
#16613=REPRESENTATION('density',(#16404),#73349);
#16614=REPRESENTATION('material name',(#16685),#73350);
#16615=REPRESENTATION('density',(#16405),#73350);
#16616=REPRESENTATION('material name',(#16686),#73351);
#16617=REPRESENTATION('density',(#16406),#73351);
#16618=REPRESENTATION('material name',(#16687),#73352);
#16619=REPRESENTATION('density',(#16407),#73352);
#16620=REPRESENTATION('material name',(#16688),#73353);
#16621=REPRESENTATION('density',(#16408),#73353);
#16622=REPRESENTATION('material name',(#16689),#73354);
#16623=REPRESENTATION('density',(#16409),#73354);
#16624=REPRESENTATION('material name',(#16690),#73356);
#16625=REPRESENTATION('density',(#16410),#73356);
#16626=REPRESENTATION('material name',(#16691),#73357);
#16627=REPRESENTATION('density',(#16411),#73357);
#16628=REPRESENTATION('material name',(#16692),#73358);
#16629=REPRESENTATION('density',(#16412),#73358);
#16630=REPRESENTATION('material name',(#16693),#73359);
#16631=REPRESENTATION('density',(#16413),#73359);
#16632=REPRESENTATION('material name',(#16694),#73360);
#16633=REPRESENTATION('density',(#16414),#73360);
#16634=REPRESENTATION('material name',(#16695),#73361);
#16635=REPRESENTATION('density',(#16415),#73361);
#16636=REPRESENTATION('material name',(#16696),#73362);
#16637=REPRESENTATION('density',(#16416),#73362);
#16638=REPRESENTATION('material name',(#16697),#73363);
#16639=REPRESENTATION('density',(#16417),#73363);
#16640=REPRESENTATION('material name',(#16698),#73364);
#16641=REPRESENTATION('density',(#16418),#73364);
#16642=REPRESENTATION('material name',(#16699),#73365);
#16643=REPRESENTATION('density',(#16419),#73365);
#16644=DESCRIPTIVE_REPRESENTATION_ITEM('Steel','Steel');
#16645=DESCRIPTIVE_REPRESENTATION_ITEM('Steel','Steel');
#16646=DESCRIPTIVE_REPRESENTATION_ITEM('Steel','Steel');
#16647=DESCRIPTIVE_REPRESENTATION_ITEM('Steel','Steel');
#16648=DESCRIPTIVE_REPRESENTATION_ITEM('Steel','Steel');
#16649=DESCRIPTIVE_REPRESENTATION_ITEM('Steel','Steel');
#16650=DESCRIPTIVE_REPRESENTATION_ITEM('Steel','Steel');
#16651=DESCRIPTIVE_REPRESENTATION_ITEM('Steel','Steel');
#16652=DESCRIPTIVE_REPRESENTATION_ITEM('Steel','Steel');
#16653=DESCRIPTIVE_REPRESENTATION_ITEM('Steel','Steel');
#16654=DESCRIPTIVE_REPRESENTATION_ITEM('Steel','Steel');
#16655=DESCRIPTIVE_REPRESENTATION_ITEM('Steel','Steel');
#16656=DESCRIPTIVE_REPRESENTATION_ITEM('Steel','Steel');
#16657=DESCRIPTIVE_REPRESENTATION_ITEM('Steel','Steel');
#16658=DESCRIPTIVE_REPRESENTATION_ITEM('Steel','Steel');
#16659=DESCRIPTIVE_REPRESENTATION_ITEM('Steel','Steel');
#16660=DESCRIPTIVE_REPRESENTATION_ITEM('Steel','Steel');
#16661=DESCRIPTIVE_REPRESENTATION_ITEM('Steel','Steel');
#16662=DESCRIPTIVE_REPRESENTATION_ITEM('Steel','Steel');
#16663=DESCRIPTIVE_REPRESENTATION_ITEM('Steel','Steel');
#16664=DESCRIPTIVE_REPRESENTATION_ITEM('Steel','Steel');
#16665=DESCRIPTIVE_REPRESENTATION_ITEM('Steel','Steel');
#16666=DESCRIPTIVE_REPRESENTATION_ITEM('Steel','Steel');
#16667=DESCRIPTIVE_REPRESENTATION_ITEM('Steel','Steel');
#16668=DESCRIPTIVE_REPRESENTATION_ITEM('Steel','Steel');
#16669=DESCRIPTIVE_REPRESENTATION_ITEM('Steel','Steel');
#16670=DESCRIPTIVE_REPRESENTATION_ITEM('Steel','Steel');
#16671=DESCRIPTIVE_REPRESENTATION_ITEM('Steel','Steel');
#16672=DESCRIPTIVE_REPRESENTATION_ITEM('Steel','Steel');
#16673=DESCRIPTIVE_REPRESENTATION_ITEM('Steel','Steel');
#16674=DESCRIPTIVE_REPRESENTATION_ITEM('Steel','Steel');
#16675=DESCRIPTIVE_REPRESENTATION_ITEM('Steel','Steel');
#16676=DESCRIPTIVE_REPRESENTATION_ITEM('Steel','Steel');
#16677=DESCRIPTIVE_REPRESENTATION_ITEM('Steel','Steel');
#16678=DESCRIPTIVE_REPRESENTATION_ITEM('Steel','Steel');
#16679=DESCRIPTIVE_REPRESENTATION_ITEM('Steel','Steel');
#16680=DESCRIPTIVE_REPRESENTATION_ITEM('Steel','Steel');
#16681=DESCRIPTIVE_REPRESENTATION_ITEM('Steel','Steel');
#16682=DESCRIPTIVE_REPRESENTATION_ITEM('Steel','Steel');
#16683=DESCRIPTIVE_REPRESENTATION_ITEM('Steel','Steel');
#16684=DESCRIPTIVE_REPRESENTATION_ITEM('Steel','Steel');
#16685=DESCRIPTIVE_REPRESENTATION_ITEM('Steel','Steel');
#16686=DESCRIPTIVE_REPRESENTATION_ITEM('Steel','Steel');
#16687=DESCRIPTIVE_REPRESENTATION_ITEM('Steel','Steel');
#16688=DESCRIPTIVE_REPRESENTATION_ITEM('Steel','Steel');
#16689=DESCRIPTIVE_REPRESENTATION_ITEM('Steel','Steel');
#16690=DESCRIPTIVE_REPRESENTATION_ITEM('Steel','Steel');
#16691=DESCRIPTIVE_REPRESENTATION_ITEM('Steel','Steel');
#16692=DESCRIPTIVE_REPRESENTATION_ITEM('Steel','Steel');
#16693=DESCRIPTIVE_REPRESENTATION_ITEM('Steel','Steel');
#16694=DESCRIPTIVE_REPRESENTATION_ITEM('Steel','Steel');
#16695=DESCRIPTIVE_REPRESENTATION_ITEM('Steel','Steel');
#16696=DESCRIPTIVE_REPRESENTATION_ITEM('Steel','Steel');
#16697=DESCRIPTIVE_REPRESENTATION_ITEM('Steel','Steel');
#16698=DESCRIPTIVE_REPRESENTATION_ITEM('Steel','Steel');
#16699=DESCRIPTIVE_REPRESENTATION_ITEM('Steel','Steel');
#16700=PROPERTY_DEFINITION('material property','material name',#73673);
#16701=PROPERTY_DEFINITION('material property','density of part',#73673);
#16702=PROPERTY_DEFINITION('material property','material name',#73674);
#16703=PROPERTY_DEFINITION('material property','density of part',#73674);
#16704=PROPERTY_DEFINITION('material property','material name',#73675);
#16705=PROPERTY_DEFINITION('material property','density of part',#73675);
#16706=PROPERTY_DEFINITION('material property','material name',#73676);
#16707=PROPERTY_DEFINITION('material property','density of part',#73676);
#16708=PROPERTY_DEFINITION('material property','material name',#73677);
#16709=PROPERTY_DEFINITION('material property','density of part',#73677);
#16710=PROPERTY_DEFINITION('material property','material name',#73678);
#16711=PROPERTY_DEFINITION('material property','density of part',#73678);
#16712=PROPERTY_DEFINITION('material property','material name',#73679);
#16713=PROPERTY_DEFINITION('material property','density of part',#73679);
#16714=PROPERTY_DEFINITION('material property','material name',#73680);
#16715=PROPERTY_DEFINITION('material property','density of part',#73680);
#16716=PROPERTY_DEFINITION('material property','material name',#73681);
#16717=PROPERTY_DEFINITION('material property','density of part',#73681);
#16718=PROPERTY_DEFINITION('material property','material name',#73682);
#16719=PROPERTY_DEFINITION('material property','density of part',#73682);
#16720=PROPERTY_DEFINITION('material property','material name',#73683);
#16721=PROPERTY_DEFINITION('material property','density of part',#73683);
#16722=PROPERTY_DEFINITION('material property','material name',#73684);
#16723=PROPERTY_DEFINITION('material property','density of part',#73684);
#16724=PROPERTY_DEFINITION('material property','material name',#73685);
#16725=PROPERTY_DEFINITION('material property','density of part',#73685);
#16726=PROPERTY_DEFINITION('material property','material name',#73686);
#16727=PROPERTY_DEFINITION('material property','density of part',#73686);
#16728=PROPERTY_DEFINITION('material property','material name',#73687);
#16729=PROPERTY_DEFINITION('material property','density of part',#73687);
#16730=PROPERTY_DEFINITION('material property','material name',#73688);
#16731=PROPERTY_DEFINITION('material property','density of part',#73688);
#16732=PROPERTY_DEFINITION('material property','material name',#73689);
#16733=PROPERTY_DEFINITION('material property','density of part',#73689);
#16734=PROPERTY_DEFINITION('material property','material name',#73691);
#16735=PROPERTY_DEFINITION('material property','density of part',#73691);
#16736=PROPERTY_DEFINITION('material property','material name',#73692);
#16737=PROPERTY_DEFINITION('material property','density of part',#73692);
#16738=PROPERTY_DEFINITION('material property','material name',#73693);
#16739=PROPERTY_DEFINITION('material property','density of part',#73693);
#16740=PROPERTY_DEFINITION('material property','material name',#73694);
#16741=PROPERTY_DEFINITION('material property','density of part',#73694);
#16742=PROPERTY_DEFINITION('material property','material name',#73695);
#16743=PROPERTY_DEFINITION('material property','density of part',#73695);
#16744=PROPERTY_DEFINITION('material property','material name',#73697);
#16745=PROPERTY_DEFINITION('material property','density of part',#73697);
#16746=PROPERTY_DEFINITION('material property','material name',#73698);
#16747=PROPERTY_DEFINITION('material property','density of part',#73698);
#16748=PROPERTY_DEFINITION('material property','material name',#73699);
#16749=PROPERTY_DEFINITION('material property','density of part',#73699);
#16750=PROPERTY_DEFINITION('material property','material name',#73700);
#16751=PROPERTY_DEFINITION('material property','density of part',#73700);
#16752=PROPERTY_DEFINITION('material property','material name',#73701);
#16753=PROPERTY_DEFINITION('material property','density of part',#73701);
#16754=PROPERTY_DEFINITION('material property','material name',#73702);
#16755=PROPERTY_DEFINITION('material property','density of part',#73702);
#16756=PROPERTY_DEFINITION('material property','material name',#73704);
#16757=PROPERTY_DEFINITION('material property','density of part',#73704);
#16758=PROPERTY_DEFINITION('material property','material name',#73705);
#16759=PROPERTY_DEFINITION('material property','density of part',#73705);
#16760=PROPERTY_DEFINITION('material property','material name',#73706);
#16761=PROPERTY_DEFINITION('material property','density of part',#73706);
#16762=PROPERTY_DEFINITION('material property','material name',#73707);
#16763=PROPERTY_DEFINITION('material property','density of part',#73707);
#16764=PROPERTY_DEFINITION('material property','material name',#73708);
#16765=PROPERTY_DEFINITION('material property','density of part',#73708);
#16766=PROPERTY_DEFINITION('material property','material name',#73709);
#16767=PROPERTY_DEFINITION('material property','density of part',#73709);
#16768=PROPERTY_DEFINITION('material property','material name',#73710);
#16769=PROPERTY_DEFINITION('material property','density of part',#73710);
#16770=PROPERTY_DEFINITION('material property','material name',#73711);
#16771=PROPERTY_DEFINITION('material property','density of part',#73711);
#16772=PROPERTY_DEFINITION('material property','material name',#73712);
#16773=PROPERTY_DEFINITION('material property','density of part',#73712);
#16774=PROPERTY_DEFINITION('material property','material name',#73714);
#16775=PROPERTY_DEFINITION('material property','density of part',#73714);
#16776=PROPERTY_DEFINITION('material property','material name',#73715);
#16777=PROPERTY_DEFINITION('material property','density of part',#73715);
#16778=PROPERTY_DEFINITION('material property','material name',#73716);
#16779=PROPERTY_DEFINITION('material property','density of part',#73716);
#16780=PROPERTY_DEFINITION('material property','material name',#73717);
#16781=PROPERTY_DEFINITION('material property','density of part',#73717);
#16782=PROPERTY_DEFINITION('material property','material name',#73718);
#16783=PROPERTY_DEFINITION('material property','density of part',#73718);
#16784=PROPERTY_DEFINITION('material property','material name',#73719);
#16785=PROPERTY_DEFINITION('material property','density of part',#73719);
#16786=PROPERTY_DEFINITION('material property','material name',#73720);
#16787=PROPERTY_DEFINITION('material property','density of part',#73720);
#16788=PROPERTY_DEFINITION('material property','material name',#73721);
#16789=PROPERTY_DEFINITION('material property','density of part',#73721);
#16790=PROPERTY_DEFINITION('material property','material name',#73722);
#16791=PROPERTY_DEFINITION('material property','density of part',#73722);
#16792=PROPERTY_DEFINITION('material property','material name',#73724);
#16793=PROPERTY_DEFINITION('material property','density of part',#73724);
#16794=PROPERTY_DEFINITION('material property','material name',#73725);
#16795=PROPERTY_DEFINITION('material property','density of part',#73725);
#16796=PROPERTY_DEFINITION('material property','material name',#73726);
#16797=PROPERTY_DEFINITION('material property','density of part',#73726);
#16798=PROPERTY_DEFINITION('material property','material name',#73727);
#16799=PROPERTY_DEFINITION('material property','density of part',#73727);
#16800=PROPERTY_DEFINITION('material property','material name',#73728);
#16801=PROPERTY_DEFINITION('material property','density of part',#73728);
#16802=PROPERTY_DEFINITION('material property','material name',#73729);
#16803=PROPERTY_DEFINITION('material property','density of part',#73729);
#16804=PROPERTY_DEFINITION('material property','material name',#73730);
#16805=PROPERTY_DEFINITION('material property','density of part',#73730);
#16806=PROPERTY_DEFINITION('material property','material name',#73731);
#16807=PROPERTY_DEFINITION('material property','density of part',#73731);
#16808=PROPERTY_DEFINITION('material property','material name',#73732);
#16809=PROPERTY_DEFINITION('material property','density of part',#73732);
#16810=PROPERTY_DEFINITION('material property','material name',#73733);
#16811=PROPERTY_DEFINITION('material property','density of part',#73733);
#16812=AXIS2_PLACEMENT_3D('',#22774,#18458,#18459);
#16813=AXIS2_PLACEMENT_3D('',#22775,#18460,#18461);
#16814=AXIS2_PLACEMENT_3D('',#22776,#18462,#18463);
#16815=AXIS2_PLACEMENT_3D('',#22777,#18464,#18465);
#16816=AXIS2_PLACEMENT_3D('',#22779,#18466,#18467);
#16817=AXIS2_PLACEMENT_3D('',#22782,#18469,#18470);
#16818=AXIS2_PLACEMENT_3D('',#22783,#18471,#18472);
#16819=AXIS2_PLACEMENT_3D('',#22785,#18473,#18474);
#16820=AXIS2_PLACEMENT_3D('',#22788,#18476,#18477);
#16821=AXIS2_PLACEMENT_3D('',#22789,#18478,#18479);
#16822=AXIS2_PLACEMENT_3D('',#22791,#18480,#18481);
#16823=AXIS2_PLACEMENT_3D('',#22794,#18483,#18484);
#16824=AXIS2_PLACEMENT_3D('',#22795,#18485,#18486);
#16825=AXIS2_PLACEMENT_3D('',#22797,#18487,#18488);
#16826=AXIS2_PLACEMENT_3D('',#22800,#18490,#18491);
#16827=AXIS2_PLACEMENT_3D('',#22801,#18492,#18493);
#16828=AXIS2_PLACEMENT_3D('',#22810,#18498,#18499);
#16829=AXIS2_PLACEMENT_3D('',#22816,#18503,#18504);
#16830=AXIS2_PLACEMENT_3D('',#22822,#18508,#18509);
#16831=AXIS2_PLACEMENT_3D('',#22825,#18512,#18513);
#16832=AXIS2_PLACEMENT_3D('',#22826,#18514,#18515);
#16833=AXIS2_PLACEMENT_3D('',#22827,#18516,#18517);
#16834=AXIS2_PLACEMENT_3D('',#22828,#18518,#18519);
#16835=AXIS2_PLACEMENT_3D('',#22830,#18520,#18521);
#16836=AXIS2_PLACEMENT_3D('',#22833,#18523,#18524);
#16837=AXIS2_PLACEMENT_3D('',#22834,#18525,#18526);
#16838=AXIS2_PLACEMENT_3D('',#22835,#18527,#18528);
#16839=AXIS2_PLACEMENT_3D('',#22837,#18529,#18530);
#16840=AXIS2_PLACEMENT_3D('',#22840,#18532,#18533);
#16841=AXIS2_PLACEMENT_3D('',#22841,#18534,#18535);
#16842=AXIS2_PLACEMENT_3D('',#22842,#18536,#18537);
#16843=AXIS2_PLACEMENT_3D('',#22844,#18538,#18539);
#16844=AXIS2_PLACEMENT_3D('',#22847,#18541,#18542);
#16845=AXIS2_PLACEMENT_3D('',#22848,#18543,#18544);
#16846=AXIS2_PLACEMENT_3D('',#22849,#18545,#18546);
#16847=AXIS2_PLACEMENT_3D('',#22851,#18547,#18548);
#16848=AXIS2_PLACEMENT_3D('',#22854,#18550,#18551);
#16849=AXIS2_PLACEMENT_3D('',#22855,#18552,#18553);
#16850=AXIS2_PLACEMENT_3D('',#22856,#18554,#18555);
#16851=AXIS2_PLACEMENT_3D('',#22861,#18557,#18558);
#16852=AXIS2_PLACEMENT_3D('',#22864,#18560,#18561);
#16853=AXIS2_PLACEMENT_3D('',#22865,#18562,#18563);
#16854=AXIS2_PLACEMENT_3D('',#22869,#18565,#18566);
#16855=AXIS2_PLACEMENT_3D('',#22871,#18568,#18569);
#16856=AXIS2_PLACEMENT_3D('',#22891,#18579,#18580);
#16857=AXIS2_PLACEMENT_3D('',#22895,#18582,#18583);
#16858=AXIS2_PLACEMENT_3D('',#22898,#18585,#18586);
#16859=AXIS2_PLACEMENT_3D('',#22900,#18587,#18588);
#16860=AXIS2_PLACEMENT_3D('',#22902,#18589,#18590);
#16861=AXIS2_PLACEMENT_3D('',#22904,#18591,#18592);
#16862=AXIS2_PLACEMENT_3D('',#22905,#18593,#18594);
#16863=AXIS2_PLACEMENT_3D('',#22924,#18604,#18605);
#16864=AXIS2_PLACEMENT_3D('',#22926,#18606,#18607);
#16865=AXIS2_PLACEMENT_3D('',#22928,#18608,#18609);
#16866=AXIS2_PLACEMENT_3D('',#22930,#18610,#18611);
#16867=AXIS2_PLACEMENT_3D('',#22932,#18612,#18613);
#16868=AXIS2_PLACEMENT_3D('',#22933,#18614,#18615);
#16869=AXIS2_PLACEMENT_3D('',#22935,#18616,#18617);
#16870=AXIS2_PLACEMENT_3D('',#22938,#18619,#18620);
#16871=AXIS2_PLACEMENT_3D('',#22939,#18621,#18622);
#16872=AXIS2_PLACEMENT_3D('',#22941,#18623,#18624);
#16873=AXIS2_PLACEMENT_3D('',#22943,#18626,#18627);
#16874=AXIS2_PLACEMENT_3D('',#22947,#18629,#18630);
#16875=AXIS2_PLACEMENT_3D('',#22951,#18632,#18633);
#16876=AXIS2_PLACEMENT_3D('',#22968,#18642,#18643);
#16877=AXIS2_PLACEMENT_3D('',#22970,#18644,#18645);
#16878=AXIS2_PLACEMENT_3D('',#22972,#18646,#18647);
#16879=AXIS2_PLACEMENT_3D('',#22974,#18648,#18649);
#16880=AXIS2_PLACEMENT_3D('',#22975,#18650,#18651);
#16881=AXIS2_PLACEMENT_3D('',#22985,#18657,#18658);
#16882=AXIS2_PLACEMENT_3D('',#22986,#18659,#18660);
#16883=AXIS2_PLACEMENT_3D('',#22987,#18661,#18662);
#16884=AXIS2_PLACEMENT_3D('',#22990,#18664,#18665);
#16885=AXIS2_PLACEMENT_3D('',#22991,#18666,#18667);
#16886=AXIS2_PLACEMENT_3D('',#22995,#18669,#18670);
#16887=AXIS2_PLACEMENT_3D('',#22999,#18672,#18673);
#16888=AXIS2_PLACEMENT_3D('',#23007,#18678,#18679);
#16889=AXIS2_PLACEMENT_3D('',#23013,#18683,#18684);
#16890=AXIS2_PLACEMENT_3D('',#23015,#18685,#18686);
#16891=AXIS2_PLACEMENT_3D('',#23017,#18688,#18689);
#16892=AXIS2_PLACEMENT_3D('',#23018,#18690,#18691);
#16893=AXIS2_PLACEMENT_3D('',#23020,#18692,#18693);
#16894=AXIS2_PLACEMENT_3D('',#23022,#18695,#18696);
#16895=AXIS2_PLACEMENT_3D('',#23023,#18697,#18698);
#16896=AXIS2_PLACEMENT_3D('',#23026,#18700,#18701);
#16897=AXIS2_PLACEMENT_3D('',#23027,#18702,#18703);
#16898=AXIS2_PLACEMENT_3D('',#23028,#18704,#18705);
#16899=AXIS2_PLACEMENT_3D('',#23031,#18707,#18708);
#16900=AXIS2_PLACEMENT_3D('',#23032,#18709,#18710);
#16901=AXIS2_PLACEMENT_3D('',#23033,#18711,#18712);
#16902=AXIS2_PLACEMENT_3D('',#23036,#18714,#18715);
#16903=AXIS2_PLACEMENT_3D('',#23037,#18716,#18717);
#16904=AXIS2_PLACEMENT_3D('',#23040,#18719,#18720);
#16905=AXIS2_PLACEMENT_3D('',#23041,#18721,#18722);
#16906=AXIS2_PLACEMENT_3D('',#23043,#18723,#18724);
#16907=AXIS2_PLACEMENT_3D('',#23045,#18726,#18727);
#16908=AXIS2_PLACEMENT_3D('',#23047,#18728,#18729);
#16909=AXIS2_PLACEMENT_3D('',#23049,#18731,#18732);
#16910=AXIS2_PLACEMENT_3D('',#23059,#18738,#18739);
#16911=AXIS2_PLACEMENT_3D('',#23061,#18741,#18742);
#16912=AXIS2_PLACEMENT_3D('',#23062,#18743,#18744);
#16913=AXIS2_PLACEMENT_3D('',#23063,#18745,#18746);
#16914=AXIS2_PLACEMENT_3D('',#23072,#18751,#18752);
#16915=AXIS2_PLACEMENT_3D('',#23073,#18753,#18754);
#16916=AXIS2_PLACEMENT_3D('',#23079,#18758,#18759);
#16917=AXIS2_PLACEMENT_3D('',#23081,#18760,#18761);
#16918=AXIS2_PLACEMENT_3D('',#23083,#18763,#18764);
#16919=AXIS2_PLACEMENT_3D('',#23084,#18765,#18766);
#16920=AXIS2_PLACEMENT_3D('',#23086,#18767,#18768);
#16921=AXIS2_PLACEMENT_3D('',#23088,#18770,#18771);
#16922=AXIS2_PLACEMENT_3D('',#23089,#18772,#18773);
#16923=AXIS2_PLACEMENT_3D('',#23092,#18775,#18776);
#16924=AXIS2_PLACEMENT_3D('',#23093,#18777,#18778);
#16925=AXIS2_PLACEMENT_3D('',#23094,#18779,#18780);
#16926=AXIS2_PLACEMENT_3D('',#23097,#18782,#18783);
#16927=AXIS2_PLACEMENT_3D('',#23098,#18784,#18785);
#16928=AXIS2_PLACEMENT_3D('',#23099,#18786,#18787);
#16929=AXIS2_PLACEMENT_3D('',#23102,#18789,#18790);
#16930=AXIS2_PLACEMENT_3D('',#23103,#18791,#18792);
#16931=AXIS2_PLACEMENT_3D('',#23106,#18794,#18795);
#16932=AXIS2_PLACEMENT_3D('',#23107,#18796,#18797);
#16933=AXIS2_PLACEMENT_3D('',#23117,#18804,#18805);
#16934=AXIS2_PLACEMENT_3D('',#23119,#18806,#18807);
#16935=AXIS2_PLACEMENT_3D('',#23121,#18808,#18809);
#16936=AXIS2_PLACEMENT_3D('',#23123,#18810,#18811);
#16937=AXIS2_PLACEMENT_3D('',#23125,#18812,#18813);
#16938=AXIS2_PLACEMENT_3D('',#23126,#18814,#18815);
#16939=AXIS2_PLACEMENT_3D('',#23127,#18816,#18817);
#16940=AXIS2_PLACEMENT_3D('',#23128,#18818,#18819);
#16941=AXIS2_PLACEMENT_3D('',#23129,#18820,#18821);
#16942=AXIS2_PLACEMENT_3D('',#23130,#18822,#18823);
#16943=AXIS2_PLACEMENT_3D('',#23131,#18824,#18825);
#16944=AXIS2_PLACEMENT_3D('',#23132,#18826,#18827);
#16945=AXIS2_PLACEMENT_3D('',#23134,#18828,#18829);
#16946=AXIS2_PLACEMENT_3D('',#23137,#18831,#18832);
#16947=AXIS2_PLACEMENT_3D('',#23138,#18833,#18834);
#16948=AXIS2_PLACEMENT_3D('',#23140,#18835,#18836);
#16949=AXIS2_PLACEMENT_3D('',#23141,#18837,#18838);
#16950=AXIS2_PLACEMENT_3D('',#23143,#18839,#18840);
#16951=AXIS2_PLACEMENT_3D('',#23146,#18842,#18843);
#16952=AXIS2_PLACEMENT_3D('',#23147,#18844,#18845);
#16953=AXIS2_PLACEMENT_3D('',#23149,#18846,#18847);
#16954=AXIS2_PLACEMENT_3D('',#23150,#18848,#18849);
#16955=AXIS2_PLACEMENT_3D('',#23152,#18850,#18851);
#16956=AXIS2_PLACEMENT_3D('',#23155,#18853,#18854);
#16957=AXIS2_PLACEMENT_3D('',#23156,#18855,#18856);
#16958=AXIS2_PLACEMENT_3D('',#23158,#18857,#18858);
#16959=AXIS2_PLACEMENT_3D('',#23159,#18859,#18860);
#16960=AXIS2_PLACEMENT_3D('',#23161,#18861,#18862);
#16961=AXIS2_PLACEMENT_3D('',#23164,#18864,#18865);
#16962=AXIS2_PLACEMENT_3D('',#23165,#18866,#18867);
#16963=AXIS2_PLACEMENT_3D('',#23167,#18868,#18869);
#16964=AXIS2_PLACEMENT_3D('',#23168,#18870,#18871);
#16965=AXIS2_PLACEMENT_3D('',#23170,#18872,#18873);
#16966=AXIS2_PLACEMENT_3D('',#23172,#18875,#18876);
#16967=AXIS2_PLACEMENT_3D('',#23174,#18877,#18878);
#16968=AXIS2_PLACEMENT_3D('',#23176,#18880,#18881);
#16969=AXIS2_PLACEMENT_3D('',#23178,#18882,#18883);
#16970=AXIS2_PLACEMENT_3D('',#23180,#18885,#18886);
#16971=AXIS2_PLACEMENT_3D('',#23182,#18887,#18888);
#16972=AXIS2_PLACEMENT_3D('',#23184,#18890,#18891);
#16973=AXIS2_PLACEMENT_3D('',#23186,#18892,#18893);
#16974=AXIS2_PLACEMENT_3D('',#23188,#18895,#18896);
#16975=AXIS2_PLACEMENT_3D('',#23189,#18897,#18898);
#16976=AXIS2_PLACEMENT_3D('',#23191,#18899,#18900);
#16977=AXIS2_PLACEMENT_3D('',#23193,#18902,#18903);
#16978=AXIS2_PLACEMENT_3D('',#23194,#18904,#18905);
#16979=AXIS2_PLACEMENT_3D('',#23196,#18906,#18907);
#16980=AXIS2_PLACEMENT_3D('',#23198,#18909,#18910);
#16981=AXIS2_PLACEMENT_3D('',#23199,#18911,#18912);
#16982=AXIS2_PLACEMENT_3D('',#23201,#18913,#18914);
#16983=AXIS2_PLACEMENT_3D('',#23203,#18916,#18917);
#16984=AXIS2_PLACEMENT_3D('',#23204,#18918,#18919);
#16985=AXIS2_PLACEMENT_3D('',#23206,#18920,#18921);
#16986=AXIS2_PLACEMENT_3D('',#23208,#18923,#18924);
#16987=AXIS2_PLACEMENT_3D('',#23210,#18925,#18926);
#16988=AXIS2_PLACEMENT_3D('',#23212,#18928,#18929);
#16989=AXIS2_PLACEMENT_3D('',#23214,#18930,#18931);
#16990=AXIS2_PLACEMENT_3D('',#23216,#18933,#18934);
#16991=AXIS2_PLACEMENT_3D('',#23218,#18935,#18936);
#16992=AXIS2_PLACEMENT_3D('',#23220,#18938,#18939);
#16993=AXIS2_PLACEMENT_3D('',#23222,#18940,#18941);
#16994=AXIS2_PLACEMENT_3D('',#23224,#18943,#18944);
#16995=AXIS2_PLACEMENT_3D('',#23226,#18945,#18946);
#16996=AXIS2_PLACEMENT_3D('',#23228,#18948,#18949);
#16997=AXIS2_PLACEMENT_3D('',#23230,#18951,#18952);
#16998=AXIS2_PLACEMENT_3D('',#23232,#18954,#18955);
#16999=AXIS2_PLACEMENT_3D('',#23234,#18957,#18958);
#17000=AXIS2_PLACEMENT_3D('',#23236,#18960,#18961);
#17001=AXIS2_PLACEMENT_3D('',#23238,#18963,#18964);
#17002=AXIS2_PLACEMENT_3D('',#23240,#18966,#18967);
#17003=AXIS2_PLACEMENT_3D('',#23242,#18969,#18970);
#17004=AXIS2_PLACEMENT_3D('',#23243,#18971,#18972);
#17005=AXIS2_PLACEMENT_3D('',#23245,#18974,#18975);
#17006=AXIS2_PLACEMENT_3D('',#23246,#18976,#18977);
#17007=AXIS2_PLACEMENT_3D('',#23247,#18978,#18979);
#17008=AXIS2_PLACEMENT_3D('',#23249,#18980,#18981);
#17009=AXIS2_PLACEMENT_3D('',#23252,#18983,#18984);
#17010=AXIS2_PLACEMENT_3D('',#23253,#18985,#18986);
#17011=AXIS2_PLACEMENT_3D('',#23255,#18987,#18988);
#17012=AXIS2_PLACEMENT_3D('',#23258,#18990,#18991);
#17013=AXIS2_PLACEMENT_3D('',#23259,#18992,#18993);
#17014=AXIS2_PLACEMENT_3D('',#23261,#18994,#18995);
#17015=AXIS2_PLACEMENT_3D('',#23264,#18997,#18998);
#17016=AXIS2_PLACEMENT_3D('',#23265,#18999,#19000);
#17017=AXIS2_PLACEMENT_3D('',#23267,#19001,#19002);
#17018=AXIS2_PLACEMENT_3D('',#23270,#19004,#19005);
#17019=AXIS2_PLACEMENT_3D('',#23271,#19006,#19007);
#17020=AXIS2_PLACEMENT_3D('',#23280,#19012,#19013);
#17021=AXIS2_PLACEMENT_3D('',#23286,#19017,#19018);
#17022=AXIS2_PLACEMENT_3D('',#23292,#19022,#19023);
#17023=AXIS2_PLACEMENT_3D('',#23295,#19026,#19027);
#17024=AXIS2_PLACEMENT_3D('',#23297,#19028,#19029);
#17025=AXIS2_PLACEMENT_3D('',#23300,#19031,#19032);
#17026=AXIS2_PLACEMENT_3D('',#23301,#19033,#19034);
#17027=AXIS2_PLACEMENT_3D('',#23302,#19035,#19036);
#17028=AXIS2_PLACEMENT_3D('',#23304,#19037,#19038);
#17029=AXIS2_PLACEMENT_3D('',#23307,#19040,#19041);
#17030=AXIS2_PLACEMENT_3D('',#23308,#19042,#19043);
#17031=AXIS2_PLACEMENT_3D('',#23309,#19044,#19045);
#17032=AXIS2_PLACEMENT_3D('',#23311,#19046,#19047);
#17033=AXIS2_PLACEMENT_3D('',#23314,#19049,#19050);
#17034=AXIS2_PLACEMENT_3D('',#23315,#19051,#19052);
#17035=AXIS2_PLACEMENT_3D('',#23316,#19053,#19054);
#17036=AXIS2_PLACEMENT_3D('',#23318,#19055,#19056);
#17037=AXIS2_PLACEMENT_3D('',#23321,#19058,#19059);
#17038=AXIS2_PLACEMENT_3D('',#23322,#19060,#19061);
#17039=AXIS2_PLACEMENT_3D('',#23323,#19062,#19063);
#17040=AXIS2_PLACEMENT_3D('',#23328,#19065,#19066);
#17041=AXIS2_PLACEMENT_3D('',#23331,#19068,#19069);
#17042=AXIS2_PLACEMENT_3D('',#23332,#19070,#19071);
#17043=AXIS2_PLACEMENT_3D('',#23336,#19073,#19074);
#17044=AXIS2_PLACEMENT_3D('',#23338,#19076,#19077);
#17045=AXIS2_PLACEMENT_3D('',#23342,#19079,#19080);
#17046=AXIS2_PLACEMENT_3D('',#23344,#19082,#19083);
#17047=AXIS2_PLACEMENT_3D('',#23363,#19093,#19094);
#17048=AXIS2_PLACEMENT_3D('',#23365,#19095,#19096);
#17049=AXIS2_PLACEMENT_3D('',#23367,#19097,#19098);
#17050=AXIS2_PLACEMENT_3D('',#23369,#19099,#19100);
#17051=AXIS2_PLACEMENT_3D('',#23371,#19101,#19102);
#17052=AXIS2_PLACEMENT_3D('',#23372,#19103,#19104);
#17053=AXIS2_PLACEMENT_3D('',#23376,#19106,#19107);
#17054=AXIS2_PLACEMENT_3D('',#23377,#19108,#19109);
#17055=AXIS2_PLACEMENT_3D('',#23378,#19110,#19111);
#17056=AXIS2_PLACEMENT_3D('',#23381,#19113,#19114);
#17057=AXIS2_PLACEMENT_3D('',#23382,#19115,#19116);
#17058=AXIS2_PLACEMENT_3D('',#23400,#19125,#19126);
#17059=AXIS2_PLACEMENT_3D('',#23404,#19128,#19129);
#17060=AXIS2_PLACEMENT_3D('',#23407,#19131,#19132);
#17061=AXIS2_PLACEMENT_3D('',#23409,#19133,#19134);
#17062=AXIS2_PLACEMENT_3D('',#23411,#19135,#19136);
#17063=AXIS2_PLACEMENT_3D('',#23413,#19137,#19138);
#17064=AXIS2_PLACEMENT_3D('',#23414,#19139,#19140);
#17065=AXIS2_PLACEMENT_3D('',#23417,#19142,#19143);
#17066=AXIS2_PLACEMENT_3D('',#23418,#19144,#19145);
#17067=AXIS2_PLACEMENT_3D('',#23422,#19147,#19148);
#17068=AXIS2_PLACEMENT_3D('',#23426,#19150,#19151);
#17069=AXIS2_PLACEMENT_3D('',#23443,#19160,#19161);
#17070=AXIS2_PLACEMENT_3D('',#23445,#19162,#19163);
#17071=AXIS2_PLACEMENT_3D('',#23447,#19164,#19165);
#17072=AXIS2_PLACEMENT_3D('',#23449,#19166,#19167);
#17073=AXIS2_PLACEMENT_3D('',#23450,#19168,#19169);
#17074=AXIS2_PLACEMENT_3D('',#23454,#19171,#19172);
#17075=AXIS2_PLACEMENT_3D('',#23458,#19174,#19175);
#17076=AXIS2_PLACEMENT_3D('',#23466,#19180,#19181);
#17077=AXIS2_PLACEMENT_3D('',#23472,#19185,#19186);
#17078=AXIS2_PLACEMENT_3D('',#23480,#19191,#19192);
#17079=AXIS2_PLACEMENT_3D('',#23482,#19193,#19194);
#17080=AXIS2_PLACEMENT_3D('',#23484,#19196,#19197);
#17081=AXIS2_PLACEMENT_3D('',#23485,#19198,#19199);
#17082=AXIS2_PLACEMENT_3D('',#23487,#19200,#19201);
#17083=AXIS2_PLACEMENT_3D('',#23489,#19203,#19204);
#17084=AXIS2_PLACEMENT_3D('',#23490,#19205,#19206);
#17085=AXIS2_PLACEMENT_3D('',#23493,#19208,#19209);
#17086=AXIS2_PLACEMENT_3D('',#23494,#19210,#19211);
#17087=AXIS2_PLACEMENT_3D('',#23495,#19212,#19213);
#17088=AXIS2_PLACEMENT_3D('',#23498,#19215,#19216);
#17089=AXIS2_PLACEMENT_3D('',#23499,#19217,#19218);
#17090=AXIS2_PLACEMENT_3D('',#23500,#19219,#19220);
#17091=AXIS2_PLACEMENT_3D('',#23504,#19222,#19223);
#17092=AXIS2_PLACEMENT_3D('',#23505,#19224,#19225);
#17093=AXIS2_PLACEMENT_3D('',#23506,#19226,#19227);
#17094=AXIS2_PLACEMENT_3D('',#23508,#19229,#19230);
#17095=AXIS2_PLACEMENT_3D('',#23510,#19231,#19232);
#17096=AXIS2_PLACEMENT_3D('',#23512,#19234,#19235);
#17097=AXIS2_PLACEMENT_3D('',#23515,#19237,#19238);
#17098=AXIS2_PLACEMENT_3D('',#23516,#19239,#19240);
#17099=AXIS2_PLACEMENT_3D('',#23519,#19242,#19243);
#17100=AXIS2_PLACEMENT_3D('',#23520,#19244,#19245);
#17101=AXIS2_PLACEMENT_3D('',#23522,#19247,#19248);
#17102=AXIS2_PLACEMENT_3D('',#23528,#19252,#19253);
#17103=AXIS2_PLACEMENT_3D('',#23536,#19258,#19259);
#17104=AXIS2_PLACEMENT_3D('',#23538,#19260,#19261);
#17105=AXIS2_PLACEMENT_3D('',#23540,#19263,#19264);
#17106=AXIS2_PLACEMENT_3D('',#23541,#19265,#19266);
#17107=AXIS2_PLACEMENT_3D('',#23543,#19267,#19268);
#17108=AXIS2_PLACEMENT_3D('',#23545,#19270,#19271);
#17109=AXIS2_PLACEMENT_3D('',#23546,#19272,#19273);
#17110=AXIS2_PLACEMENT_3D('',#23549,#19275,#19276);
#17111=AXIS2_PLACEMENT_3D('',#23550,#19277,#19278);
#17112=AXIS2_PLACEMENT_3D('',#23551,#19279,#19280);
#17113=AXIS2_PLACEMENT_3D('',#23554,#19282,#19283);
#17114=AXIS2_PLACEMENT_3D('',#23555,#19284,#19285);
#17115=AXIS2_PLACEMENT_3D('',#23556,#19286,#19287);
#17116=AXIS2_PLACEMENT_3D('',#23558,#19288,#19289);
#17117=AXIS2_PLACEMENT_3D('',#23560,#19291,#19292);
#17118=AXIS2_PLACEMENT_3D('',#23562,#19293,#19294);
#17119=AXIS2_PLACEMENT_3D('',#23564,#19296,#19297);
#17120=AXIS2_PLACEMENT_3D('',#23567,#19299,#19300);
#17121=AXIS2_PLACEMENT_3D('',#23568,#19301,#19302);
#17122=AXIS2_PLACEMENT_3D('',#23571,#19304,#19305);
#17123=AXIS2_PLACEMENT_3D('',#23572,#19306,#19307);
#17124=AXIS2_PLACEMENT_3D('',#23574,#19309,#19310);
#17125=AXIS2_PLACEMENT_3D('',#23576,#19311,#19312);
#17126=AXIS2_PLACEMENT_3D('',#23578,#19314,#19315);
#17127=AXIS2_PLACEMENT_3D('',#23586,#19320,#19321);
#17128=AXIS2_PLACEMENT_3D('',#23590,#19324,#19325);
#17129=AXIS2_PLACEMENT_3D('',#23592,#19326,#19327);
#17130=AXIS2_PLACEMENT_3D('',#23594,#19328,#19329);
#17131=AXIS2_PLACEMENT_3D('',#23596,#19330,#19331);
#17132=AXIS2_PLACEMENT_3D('',#23598,#19332,#19333);
#17133=AXIS2_PLACEMENT_3D('',#23599,#19334,#19335);
#17134=AXIS2_PLACEMENT_3D('',#23602,#19337,#19338);
#17135=AXIS2_PLACEMENT_3D('',#23603,#19339,#19340);
#17136=AXIS2_PLACEMENT_3D('',#23604,#19341,#19342);
#17137=AXIS2_PLACEMENT_3D('',#23607,#19344,#19345);
#17138=AXIS2_PLACEMENT_3D('',#23608,#19346,#19347);
#17139=AXIS2_PLACEMENT_3D('',#23609,#19348,#19349);
#17140=AXIS2_PLACEMENT_3D('',#23612,#19351,#19352);
#17141=AXIS2_PLACEMENT_3D('',#23613,#19353,#19354);
#17142=AXIS2_PLACEMENT_3D('',#23614,#19355,#19356);
#17143=AXIS2_PLACEMENT_3D('',#23617,#19358,#19359);
#17144=AXIS2_PLACEMENT_3D('',#23618,#19360,#19361);
#17145=AXIS2_PLACEMENT_3D('',#23619,#19362,#19363);
#17146=AXIS2_PLACEMENT_3D('',#23622,#19365,#19366);
#17147=AXIS2_PLACEMENT_3D('',#23623,#19367,#19368);
#17148=AXIS2_PLACEMENT_3D('',#23626,#19370,#19371);
#17149=AXIS2_PLACEMENT_3D('',#23627,#19372,#19373);
#17150=AXIS2_PLACEMENT_3D('',#23630,#19375,#19376);
#17151=AXIS2_PLACEMENT_3D('',#23631,#19377,#19378);
#17152=AXIS2_PLACEMENT_3D('',#23634,#19380,#19381);
#17153=AXIS2_PLACEMENT_3D('',#23635,#19382,#19383);
#17154=AXIS2_PLACEMENT_3D('',#23638,#19385,#19386);
#17155=AXIS2_PLACEMENT_3D('',#23639,#19387,#19388);
#17156=AXIS2_PLACEMENT_3D('',#23642,#19390,#19391);
#17157=AXIS2_PLACEMENT_3D('',#23643,#19392,#19393);
#17158=AXIS2_PLACEMENT_3D('',#23645,#19395,#19396);
#17159=AXIS2_PLACEMENT_3D('',#23647,#19398,#19399);
#17160=AXIS2_PLACEMENT_3D('',#23649,#19401,#19402);
#17161=AXIS2_PLACEMENT_3D('',#23651,#19404,#19405);
#17162=AXIS2_PLACEMENT_3D('',#23653,#19407,#19408);
#17163=AXIS2_PLACEMENT_3D('',#23655,#19410,#19411);
#17164=AXIS2_PLACEMENT_3D('',#23657,#19413,#19414);
#17165=AXIS2_PLACEMENT_3D('',#23658,#19415,#19416);
#17166=AXIS2_PLACEMENT_3D('',#23660,#19418,#19419);
#17167=AXIS2_PLACEMENT_3D('',#23661,#19420,#19421);
#17168=AXIS2_PLACEMENT_3D('',#23662,#19422,#19423);
#17169=AXIS2_PLACEMENT_3D('',#23664,#19424,#19425);
#17170=AXIS2_PLACEMENT_3D('',#23667,#19427,#19428);
#17171=AXIS2_PLACEMENT_3D('',#23668,#19429,#19430);
#17172=AXIS2_PLACEMENT_3D('',#23669,#19431,#19432);
#17173=AXIS2_PLACEMENT_3D('',#23670,#19433,#19434);
#17174=AXIS2_PLACEMENT_3D('',#23671,#19435,#19436);
#17175=AXIS2_PLACEMENT_3D('',#23673,#19437,#19438);
#17176=AXIS2_PLACEMENT_3D('',#23676,#19440,#19441);
#17177=AXIS2_PLACEMENT_3D('',#23677,#19442,#19443);
#17178=AXIS2_PLACEMENT_3D('',#23678,#19444,#19445);
#17179=AXIS2_PLACEMENT_3D('',#23679,#19446,#19447);
#17180=AXIS2_PLACEMENT_3D('',#23680,#19448,#19449);
#17181=AXIS2_PLACEMENT_3D('',#23682,#19450,#19451);
#17182=AXIS2_PLACEMENT_3D('',#23685,#19453,#19454);
#17183=AXIS2_PLACEMENT_3D('',#23686,#19455,#19456);
#17184=AXIS2_PLACEMENT_3D('',#23687,#19457,#19458);
#17185=AXIS2_PLACEMENT_3D('',#23688,#19459,#19460);
#17186=AXIS2_PLACEMENT_3D('',#23689,#19461,#19462);
#17187=AXIS2_PLACEMENT_3D('',#23691,#19463,#19464);
#17188=AXIS2_PLACEMENT_3D('',#23694,#19466,#19467);
#17189=AXIS2_PLACEMENT_3D('',#23695,#19468,#19469);
#17190=AXIS2_PLACEMENT_3D('',#23696,#19470,#19471);
#17191=AXIS2_PLACEMENT_3D('',#23697,#19472,#19473);
#17192=AXIS2_PLACEMENT_3D('',#23698,#19474,#19475);
#17193=AXIS2_PLACEMENT_3D('',#23703,#19477,#19478);
#17194=AXIS2_PLACEMENT_3D('',#23706,#19480,#19481);
#17195=AXIS2_PLACEMENT_3D('',#23707,#19482,#19483);
#17196=AXIS2_PLACEMENT_3D('',#23712,#19485,#19486);
#17197=AXIS2_PLACEMENT_3D('',#23715,#19488,#19489);
#17198=AXIS2_PLACEMENT_3D('',#23716,#19490,#19491);
#17199=AXIS2_PLACEMENT_3D('',#23721,#19493,#19494);
#17200=AXIS2_PLACEMENT_3D('',#23724,#19496,#19497);
#17201=AXIS2_PLACEMENT_3D('',#23725,#19498,#19499);
#17202=AXIS2_PLACEMENT_3D('',#23730,#19501,#19502);
#17203=AXIS2_PLACEMENT_3D('',#23733,#19504,#19505);
#17204=AXIS2_PLACEMENT_3D('',#23734,#19506,#19507);
#17205=AXIS2_PLACEMENT_3D('',#23735,#19508,#19509);
#17206=AXIS2_PLACEMENT_3D('',#23736,#19510,#19511);
#17207=AXIS2_PLACEMENT_3D('',#23737,#19512,#19513);
#17208=AXIS2_PLACEMENT_3D('',#23738,#19514,#19515);
#17209=AXIS2_PLACEMENT_3D('',#23740,#19516,#19517);
#17210=AXIS2_PLACEMENT_3D('',#23741,#19518,#19519);
#17211=AXIS2_PLACEMENT_3D('',#23742,#19520,#19521);
#17212=AXIS2_PLACEMENT_3D('',#23743,#19522,#19523);
#17213=AXIS2_PLACEMENT_3D('',#23744,#19524,#19525);
#17214=AXIS2_PLACEMENT_3D('',#23745,#19526,#19527);
#17215=AXIS2_PLACEMENT_3D('',#23746,#19528,#19529);
#17216=AXIS2_PLACEMENT_3D('',#23747,#19530,#19531);
#17217=AXIS2_PLACEMENT_3D('',#23748,#19532,#19533);
#17218=AXIS2_PLACEMENT_3D('',#23749,#19534,#19535);
#17219=AXIS2_PLACEMENT_3D('',#23751,#19536,#19537);
#17220=AXIS2_PLACEMENT_3D('',#23754,#19539,#19540);
#17221=AXIS2_PLACEMENT_3D('',#23755,#19541,#19542);
#17222=AXIS2_PLACEMENT_3D('',#23757,#19543,#19544);
#17223=AXIS2_PLACEMENT_3D('',#23758,#19545,#19546);
#17224=AXIS2_PLACEMENT_3D('',#23760,#19548,#19549);
#17225=AXIS2_PLACEMENT_3D('',#23761,#19550,#19551);
#17226=AXIS2_PLACEMENT_3D('',#23762,#19552,#19553);
#17227=AXIS2_PLACEMENT_3D('',#23767,#19555,#19556);
#17228=AXIS2_PLACEMENT_3D('',#23770,#19558,#19559);
#17229=AXIS2_PLACEMENT_3D('',#23771,#19560,#19561);
#17230=AXIS2_PLACEMENT_3D('',#23776,#19563,#19564);
#17231=AXIS2_PLACEMENT_3D('',#23779,#19566,#19567);
#17232=AXIS2_PLACEMENT_3D('',#23780,#19568,#19569);
#17233=AXIS2_PLACEMENT_3D('',#23785,#19571,#19572);
#17234=AXIS2_PLACEMENT_3D('',#23788,#19574,#19575);
#17235=AXIS2_PLACEMENT_3D('',#23789,#19576,#19577);
#17236=AXIS2_PLACEMENT_3D('',#23794,#19579,#19580);
#17237=AXIS2_PLACEMENT_3D('',#23797,#19582,#19583);
#17238=AXIS2_PLACEMENT_3D('',#23798,#19584,#19585);
#17239=AXIS2_PLACEMENT_3D('',#23799,#19586,#19587);
#17240=AXIS2_PLACEMENT_3D('',#23800,#19588,#19589);
#17241=AXIS2_PLACEMENT_3D('',#23801,#19590,#19591);
#17242=AXIS2_PLACEMENT_3D('',#23802,#19592,#19593);
#17243=AXIS2_PLACEMENT_3D('',#23804,#19594,#19595);
#17244=AXIS2_PLACEMENT_3D('',#23805,#19596,#19597);
#17245=AXIS2_PLACEMENT_3D('',#23806,#19598,#19599);
#17246=AXIS2_PLACEMENT_3D('',#23807,#19600,#19601);
#17247=AXIS2_PLACEMENT_3D('',#23808,#19602,#19603);
#17248=AXIS2_PLACEMENT_3D('',#23809,#19604,#19605);
#17249=AXIS2_PLACEMENT_3D('',#23810,#19606,#19607);
#17250=AXIS2_PLACEMENT_3D('',#23811,#19608,#19609);
#17251=AXIS2_PLACEMENT_3D('',#23812,#19610,#19611);
#17252=AXIS2_PLACEMENT_3D('',#23813,#19612,#19613);
#17253=AXIS2_PLACEMENT_3D('',#23816,#19615,#19616);
#17254=AXIS2_PLACEMENT_3D('',#23817,#19617,#19618);
#17255=AXIS2_PLACEMENT_3D('',#23819,#19619,#19620);
#17256=AXIS2_PLACEMENT_3D('',#23820,#19621,#19622);
#17257=AXIS2_PLACEMENT_3D('',#23822,#19623,#19624);
#17258=AXIS2_PLACEMENT_3D('',#23824,#19626,#19627);
#17259=AXIS2_PLACEMENT_3D('',#23825,#19628,#19629);
#17260=AXIS2_PLACEMENT_3D('',#23826,#19630,#19631);
#17261=AXIS2_PLACEMENT_3D('',#23828,#19632,#19633);
#17262=AXIS2_PLACEMENT_3D('',#23831,#19635,#19636);
#17263=AXIS2_PLACEMENT_3D('',#23832,#19637,#19638);
#17264=AXIS2_PLACEMENT_3D('',#23834,#19639,#19640);
#17265=AXIS2_PLACEMENT_3D('',#23837,#19642,#19643);
#17266=AXIS2_PLACEMENT_3D('',#23838,#19644,#19645);
#17267=AXIS2_PLACEMENT_3D('',#23840,#19646,#19647);
#17268=AXIS2_PLACEMENT_3D('',#23843,#19649,#19650);
#17269=AXIS2_PLACEMENT_3D('',#23844,#19651,#19652);
#17270=AXIS2_PLACEMENT_3D('',#23846,#19653,#19654);
#17271=AXIS2_PLACEMENT_3D('',#23849,#19656,#19657);
#17272=AXIS2_PLACEMENT_3D('',#23850,#19658,#19659);
#17273=AXIS2_PLACEMENT_3D('',#23852,#19660,#19661);
#17274=AXIS2_PLACEMENT_3D('',#23855,#19663,#19664);
#17275=AXIS2_PLACEMENT_3D('',#23856,#19665,#19666);
#17276=AXIS2_PLACEMENT_3D('',#23858,#19667,#19668);
#17277=AXIS2_PLACEMENT_3D('',#23859,#19669,#19670);
#17278=AXIS2_PLACEMENT_3D('',#23862,#19672,#19673);
#17279=AXIS2_PLACEMENT_3D('',#23863,#19674,#19675);
#17280=AXIS2_PLACEMENT_3D('',#23865,#19676,#19677);
#17281=AXIS2_PLACEMENT_3D('',#23868,#19679,#19680);
#17282=AXIS2_PLACEMENT_3D('',#23869,#19681,#19682);
#17283=AXIS2_PLACEMENT_3D('',#23870,#19683,#19684);
#17284=AXIS2_PLACEMENT_3D('',#23871,#19685,#19686);
#17285=AXIS2_PLACEMENT_3D('',#23872,#19687,#19688);
#17286=AXIS2_PLACEMENT_3D('',#23874,#19689,#19690);
#17287=AXIS2_PLACEMENT_3D('',#23877,#19692,#19693);
#17288=AXIS2_PLACEMENT_3D('',#23878,#19694,#19695);
#17289=AXIS2_PLACEMENT_3D('',#23880,#19696,#19697);
#17290=AXIS2_PLACEMENT_3D('',#23883,#19699,#19700);
#17291=AXIS2_PLACEMENT_3D('',#23884,#19701,#19702);
#17292=AXIS2_PLACEMENT_3D('',#23886,#19703,#19704);
#17293=AXIS2_PLACEMENT_3D('',#23889,#19706,#19707);
#17294=AXIS2_PLACEMENT_3D('',#23890,#19708,#19709);
#17295=AXIS2_PLACEMENT_3D('',#23892,#19710,#19711);
#17296=AXIS2_PLACEMENT_3D('',#23895,#19713,#19714);
#17297=AXIS2_PLACEMENT_3D('',#23896,#19715,#19716);
#17298=AXIS2_PLACEMENT_3D('',#23898,#19717,#19718);
#17299=AXIS2_PLACEMENT_3D('',#23901,#19720,#19721);
#17300=AXIS2_PLACEMENT_3D('',#23902,#19722,#19723);
#17301=AXIS2_PLACEMENT_3D('',#23904,#19724,#19725);
#17302=AXIS2_PLACEMENT_3D('',#23905,#19726,#19727);
#17303=AXIS2_PLACEMENT_3D('',#23907,#19728,#19729);
#17304=AXIS2_PLACEMENT_3D('',#23909,#19731,#19732);
#17305=AXIS2_PLACEMENT_3D('',#23911,#19733,#19734);
#17306=AXIS2_PLACEMENT_3D('',#23914,#19736,#19737);
#17307=AXIS2_PLACEMENT_3D('',#23915,#19738,#19739);
#17308=AXIS2_PLACEMENT_3D('',#23916,#19740,#19741);
#17309=AXIS2_PLACEMENT_3D('',#23917,#19742,#19743);
#17310=AXIS2_PLACEMENT_3D('',#23918,#19744,#19745);
#17311=AXIS2_PLACEMENT_3D('',#23920,#19746,#19747);
#17312=AXIS2_PLACEMENT_3D('',#23923,#19749,#19750);
#17313=AXIS2_PLACEMENT_3D('',#23924,#19751,#19752);
#17314=AXIS2_PLACEMENT_3D('',#23926,#19753,#19754);
#17315=AXIS2_PLACEMENT_3D('',#23929,#19756,#19757);
#17316=AXIS2_PLACEMENT_3D('',#23930,#19758,#19759);
#17317=AXIS2_PLACEMENT_3D('',#23932,#19760,#19761);
#17318=AXIS2_PLACEMENT_3D('',#23935,#19763,#19764);
#17319=AXIS2_PLACEMENT_3D('',#23936,#19765,#19766);
#17320=AXIS2_PLACEMENT_3D('',#23938,#19767,#19768);
#17321=AXIS2_PLACEMENT_3D('',#23941,#19770,#19771);
#17322=AXIS2_PLACEMENT_3D('',#23942,#19772,#19773);
#17323=AXIS2_PLACEMENT_3D('',#23944,#19774,#19775);
#17324=AXIS2_PLACEMENT_3D('',#23947,#19777,#19778);
#17325=AXIS2_PLACEMENT_3D('',#23948,#19779,#19780);
#17326=AXIS2_PLACEMENT_3D('',#23950,#19781,#19782);
#17327=AXIS2_PLACEMENT_3D('',#23951,#19783,#19784);
#17328=AXIS2_PLACEMENT_3D('',#23954,#19786,#19787);
#17329=AXIS2_PLACEMENT_3D('',#23955,#19788,#19789);
#17330=AXIS2_PLACEMENT_3D('',#23957,#19790,#19791);
#17331=AXIS2_PLACEMENT_3D('',#23960,#19793,#19794);
#17332=AXIS2_PLACEMENT_3D('',#23961,#19795,#19796);
#17333=AXIS2_PLACEMENT_3D('',#23962,#19797,#19798);
#17334=AXIS2_PLACEMENT_3D('',#23963,#19799,#19800);
#17335=AXIS2_PLACEMENT_3D('',#23964,#19801,#19802);
#17336=AXIS2_PLACEMENT_3D('',#23966,#19803,#19804);
#17337=AXIS2_PLACEMENT_3D('',#23969,#19806,#19807);
#17338=AXIS2_PLACEMENT_3D('',#23970,#19808,#19809);
#17339=AXIS2_PLACEMENT_3D('',#23972,#19810,#19811);
#17340=AXIS2_PLACEMENT_3D('',#23975,#19813,#19814);
#17341=AXIS2_PLACEMENT_3D('',#23976,#19815,#19816);
#17342=AXIS2_PLACEMENT_3D('',#23978,#19817,#19818);
#17343=AXIS2_PLACEMENT_3D('',#23981,#19820,#19821);
#17344=AXIS2_PLACEMENT_3D('',#23982,#19822,#19823);
#17345=AXIS2_PLACEMENT_3D('',#23984,#19824,#19825);
#17346=AXIS2_PLACEMENT_3D('',#23987,#19827,#19828);
#17347=AXIS2_PLACEMENT_3D('',#23988,#19829,#19830);
#17348=AXIS2_PLACEMENT_3D('',#23990,#19831,#19832);
#17349=AXIS2_PLACEMENT_3D('',#23993,#19834,#19835);
#17350=AXIS2_PLACEMENT_3D('',#23994,#19836,#19837);
#17351=AXIS2_PLACEMENT_3D('',#23996,#19838,#19839);
#17352=AXIS2_PLACEMENT_3D('',#23997,#19840,#19841);
#17353=AXIS2_PLACEMENT_3D('',#23999,#19842,#19843);
#17354=AXIS2_PLACEMENT_3D('',#24001,#19845,#19846);
#17355=AXIS2_PLACEMENT_3D('',#24003,#19847,#19848);
#17356=AXIS2_PLACEMENT_3D('',#24006,#19850,#19851);
#17357=AXIS2_PLACEMENT_3D('',#24007,#19852,#19853);
#17358=AXIS2_PLACEMENT_3D('',#24008,#19854,#19855);
#17359=AXIS2_PLACEMENT_3D('',#24009,#19856,#19857);
#17360=AXIS2_PLACEMENT_3D('',#24010,#19858,#19859);
#17361=AXIS2_PLACEMENT_3D('',#24012,#19860,#19861);
#17362=AXIS2_PLACEMENT_3D('',#24015,#19863,#19864);
#17363=AXIS2_PLACEMENT_3D('',#24016,#19865,#19866);
#17364=AXIS2_PLACEMENT_3D('',#24018,#19867,#19868);
#17365=AXIS2_PLACEMENT_3D('',#24021,#19870,#19871);
#17366=AXIS2_PLACEMENT_3D('',#24022,#19872,#19873);
#17367=AXIS2_PLACEMENT_3D('',#24024,#19874,#19875);
#17368=AXIS2_PLACEMENT_3D('',#24027,#19877,#19878);
#17369=AXIS2_PLACEMENT_3D('',#24028,#19879,#19880);
#17370=AXIS2_PLACEMENT_3D('',#24030,#19881,#19882);
#17371=AXIS2_PLACEMENT_3D('',#24033,#19884,#19885);
#17372=AXIS2_PLACEMENT_3D('',#24034,#19886,#19887);
#17373=AXIS2_PLACEMENT_3D('',#24043,#19892,#19893);
#17374=AXIS2_PLACEMENT_3D('',#24049,#19897,#19898);
#17375=AXIS2_PLACEMENT_3D('',#24055,#19902,#19903);
#17376=AXIS2_PLACEMENT_3D('',#24058,#19906,#19907);
#17377=AXIS2_PLACEMENT_3D('',#24059,#19908,#19909);
#17378=AXIS2_PLACEMENT_3D('',#24060,#19910,#19911);
#17379=AXIS2_PLACEMENT_3D('',#24061,#19912,#19913);
#17380=AXIS2_PLACEMENT_3D('',#24070,#19918,#19919);
#17381=AXIS2_PLACEMENT_3D('',#24076,#19923,#19924);
#17382=AXIS2_PLACEMENT_3D('',#24082,#19928,#19929);
#17383=AXIS2_PLACEMENT_3D('',#24085,#19932,#19933);
#17384=AXIS2_PLACEMENT_3D('',#24086,#19934,#19935);
#17385=AXIS2_PLACEMENT_3D('',#24087,#19936,#19937);
#17386=AXIS2_PLACEMENT_3D('',#24088,#19938,#19939);
#17387=AXIS2_PLACEMENT_3D('',#24097,#19944,#19945);
#17388=AXIS2_PLACEMENT_3D('',#24103,#19949,#19950);
#17389=AXIS2_PLACEMENT_3D('',#24109,#19954,#19955);
#17390=AXIS2_PLACEMENT_3D('',#24112,#19958,#19959);
#17391=AXIS2_PLACEMENT_3D('',#24113,#19960,#19961);
#17392=AXIS2_PLACEMENT_3D('',#24114,#19962,#19963);
#17393=AXIS2_PLACEMENT_3D('',#24115,#19964,#19965);
#17394=AXIS2_PLACEMENT_3D('',#24124,#19970,#19971);
#17395=AXIS2_PLACEMENT_3D('',#24130,#19975,#19976);
#17396=AXIS2_PLACEMENT_3D('',#24136,#19980,#19981);
#17397=AXIS2_PLACEMENT_3D('',#24142,#19985,#19986);
#17398=AXIS2_PLACEMENT_3D('',#24148,#19990,#19991);
#17399=AXIS2_PLACEMENT_3D('',#24151,#19994,#19995);
#17400=AXIS2_PLACEMENT_3D('',#24152,#19996,#19997);
#17401=AXIS2_PLACEMENT_3D('',#24153,#19998,#19999);
#17402=AXIS2_PLACEMENT_3D('',#24155,#20000,#20001);
#17403=AXIS2_PLACEMENT_3D('',#24156,#20002,#20003);
#17404=AXIS2_PLACEMENT_3D('',#24158,#20004,#20005);
#17405=AXIS2_PLACEMENT_3D('',#24159,#20006,#20007);
#17406=AXIS2_PLACEMENT_3D('',#24161,#20008,#20009);
#17407=AXIS2_PLACEMENT_3D('',#24163,#20011,#20012);
#17408=AXIS2_PLACEMENT_3D('',#24165,#20013,#20014);
#17409=AXIS2_PLACEMENT_3D('',#24167,#20016,#20017);
#17410=AXIS2_PLACEMENT_3D('',#24169,#20018,#20019);
#17411=AXIS2_PLACEMENT_3D('',#24171,#20021,#20022);
#17412=AXIS2_PLACEMENT_3D('',#24173,#20023,#20024);
#17413=AXIS2_PLACEMENT_3D('',#24174,#20025,#20026);
#17414=AXIS2_PLACEMENT_3D('',#24176,#20027,#20028);
#17415=AXIS2_PLACEMENT_3D('',#24178,#20030,#20031);
#17416=AXIS2_PLACEMENT_3D('',#24180,#20033,#20034);
#17417=AXIS2_PLACEMENT_3D('',#24181,#20035,#20036);
#17418=AXIS2_PLACEMENT_3D('',#24182,#20037,#20038);
#17419=AXIS2_PLACEMENT_3D('',#24185,#20039,#20040);
#17420=AXIS2_PLACEMENT_3D('',#24186,#20041,#20042);
#17421=AXIS2_PLACEMENT_3D('',#24188,#20043,#20044);
#17422=AXIS2_PLACEMENT_3D('',#24190,#20045,#20046);
#17423=AXIS2_PLACEMENT_3D('',#24191,#20047,#20048);
#17424=AXIS2_PLACEMENT_3D('',#24192,#20049,#20050);
#17425=AXIS2_PLACEMENT_3D('',#24195,#20052,#20053);
#17426=AXIS2_PLACEMENT_3D('',#24196,#20054,#20055);
#17427=AXIS2_PLACEMENT_3D('',#24198,#20056,#20057);
#17428=AXIS2_PLACEMENT_3D('',#24201,#20059,#20060);
#17429=AXIS2_PLACEMENT_3D('',#24202,#20061,#20062);
#17430=AXIS2_PLACEMENT_3D('',#24205,#20064,#20065);
#17431=AXIS2_PLACEMENT_3D('',#24206,#20066,#20067);
#17432=AXIS2_PLACEMENT_3D('',#24207,#20068,#20069);
#17433=AXIS2_PLACEMENT_3D('',#24209,#20070,#20071);
#17434=AXIS2_PLACEMENT_3D('',#24211,#20073,#20074);
#17435=AXIS2_PLACEMENT_3D('',#24213,#20075,#20076);
#17436=AXIS2_PLACEMENT_3D('',#24214,#20077,#20078);
#17437=AXIS2_PLACEMENT_3D('',#24216,#20080,#20081);
#17438=AXIS2_PLACEMENT_3D('',#24217,#20082,#20083);
#17439=AXIS2_PLACEMENT_3D('',#24220,#20084,#20085);
#17440=AXIS2_PLACEMENT_3D('',#24221,#20086,#20087);
#17441=AXIS2_PLACEMENT_3D('',#24223,#20088,#20089);
#17442=AXIS2_PLACEMENT_3D('',#24225,#20090,#20091);
#17443=AXIS2_PLACEMENT_3D('',#24226,#20092,#20093);
#17444=AXIS2_PLACEMENT_3D('',#24227,#20094,#20095);
#17445=AXIS2_PLACEMENT_3D('',#24229,#20096,#20097);
#17446=AXIS2_PLACEMENT_3D('',#24231,#20099,#20100);
#17447=AXIS2_PLACEMENT_3D('',#24233,#20101,#20102);
#17448=AXIS2_PLACEMENT_3D('',#24235,#20103,#20104);
#17449=AXIS2_PLACEMENT_3D('',#24236,#20105,#20106);
#17450=AXIS2_PLACEMENT_3D('',#24238,#20107,#20108);
#17451=AXIS2_PLACEMENT_3D('',#24240,#20110,#20111);
#17452=AXIS2_PLACEMENT_3D('',#24242,#20112,#20113);
#17453=AXIS2_PLACEMENT_3D('',#24244,#20115,#20116);
#17454=AXIS2_PLACEMENT_3D('',#24246,#20117,#20118);
#17455=AXIS2_PLACEMENT_3D('',#24248,#20120,#20121);
#17456=AXIS2_PLACEMENT_3D('',#24249,#20122,#20123);
#17457=AXIS2_PLACEMENT_3D('',#24251,#20125,#20126);
#17458=AXIS2_PLACEMENT_3D('',#24252,#20127,#20128);
#17459=AXIS2_PLACEMENT_3D('',#24255,#20129,#20130);
#17460=AXIS2_PLACEMENT_3D('',#24256,#20131,#20132);
#17461=AXIS2_PLACEMENT_3D('',#24259,#20133,#20134);
#17462=AXIS2_PLACEMENT_3D('',#24260,#20135,#20136);
#17463=AXIS2_PLACEMENT_3D('',#24263,#20137,#20138);
#17464=AXIS2_PLACEMENT_3D('',#24264,#20139,#20140);
#17465=AXIS2_PLACEMENT_3D('',#24267,#20141,#20142);
#17466=AXIS2_PLACEMENT_3D('',#24268,#20143,#20144);
#17467=AXIS2_PLACEMENT_3D('',#24271,#20145,#20146);
#17468=AXIS2_PLACEMENT_3D('',#24272,#20147,#20148);
#17469=AXIS2_PLACEMENT_3D('',#24275,#20149,#20150);
#17470=AXIS2_PLACEMENT_3D('',#24276,#20151,#20152);
#17471=AXIS2_PLACEMENT_3D('',#24279,#20153,#20154);
#17472=AXIS2_PLACEMENT_3D('',#24280,#20155,#20156);
#17473=AXIS2_PLACEMENT_3D('',#24281,#20157,#20158);
#17474=AXIS2_PLACEMENT_3D('',#24307,#20159,#20160);
#17475=AXIS2_PLACEMENT_3D('',#24331,#20161,#20162);
#17476=AXIS2_PLACEMENT_3D('',#24332,#20163,#20164);
#17477=AXIS2_PLACEMENT_3D('',#24334,#20165,#20166);
#17478=AXIS2_PLACEMENT_3D('',#24359,#20167,#20168);
#17479=AXIS2_PLACEMENT_3D('',#24384,#20169,#20170);
#17480=AXIS2_PLACEMENT_3D('',#24387,#20172,#20173);
#17481=AXIS2_PLACEMENT_3D('',#24389,#20174,#20175);
#17482=AXIS2_PLACEMENT_3D('',#24414,#20176,#20177);
#17483=AXIS2_PLACEMENT_3D('',#24439,#20178,#20179);
#17484=AXIS2_PLACEMENT_3D('',#24464,#20180,#20181);
#17485=AXIS2_PLACEMENT_3D('',#24488,#20182,#20183);
#17486=AXIS2_PLACEMENT_3D('',#24489,#20184,#20185);
#17487=AXIS2_PLACEMENT_3D('',#24491,#20186,#20187);
#17488=AXIS2_PLACEMENT_3D('',#24492,#20188,#20189);
#17489=AXIS2_PLACEMENT_3D('',#24493,#20190,#20191);
#17490=AXIS2_PLACEMENT_3D('',#24517,#20192,#20193);
#17491=AXIS2_PLACEMENT_3D('',#24518,#20194,#20195);
#17492=AXIS2_PLACEMENT_3D('',#24520,#20196,#20197);
#17493=AXIS2_PLACEMENT_3D('',#24521,#20198,#20199);
#17494=AXIS2_PLACEMENT_3D('',#24522,#20200,#20201);
#17495=AXIS2_PLACEMENT_3D('',#24546,#20202,#20203);
#17496=AXIS2_PLACEMENT_3D('',#24547,#20204,#20205);
#17497=AXIS2_PLACEMENT_3D('',#24549,#20206,#20207);
#17498=AXIS2_PLACEMENT_3D('',#24551,#20208,#20209);
#17499=AXIS2_PLACEMENT_3D('',#24552,#20210,#20211);
#17500=AXIS2_PLACEMENT_3D('',#24553,#20212,#20213);
#17501=AXIS2_PLACEMENT_3D('',#24577,#20214,#20215);
#17502=AXIS2_PLACEMENT_3D('',#24578,#20216,#20217);
#17503=AXIS2_PLACEMENT_3D('',#24580,#20218,#20219);
#17504=AXIS2_PLACEMENT_3D('',#24581,#20220,#20221);
#17505=AXIS2_PLACEMENT_3D('',#24582,#20222,#20223);
#17506=AXIS2_PLACEMENT_3D('',#24606,#20224,#20225);
#17507=AXIS2_PLACEMENT_3D('',#24607,#20226,#20227);
#17508=AXIS2_PLACEMENT_3D('',#24609,#20228,#20229);
#17509=AXIS2_PLACEMENT_3D('',#24610,#20230,#20231);
#17510=AXIS2_PLACEMENT_3D('',#24611,#20232,#20233);
#17511=AXIS2_PLACEMENT_3D('',#24635,#20234,#20235);
#17512=AXIS2_PLACEMENT_3D('',#24636,#20236,#20237);
#17513=AXIS2_PLACEMENT_3D('',#24638,#20238,#20239);
#17514=AXIS2_PLACEMENT_3D('',#24641,#20241,#20242);
#17515=AXIS2_PLACEMENT_3D('',#24665,#20243,#20244);
#17516=AXIS2_PLACEMENT_3D('',#24666,#20245,#20246);
#17517=AXIS2_PLACEMENT_3D('',#24667,#20247,#20248);
#17518=AXIS2_PLACEMENT_3D('',#24668,#20249,#20250);
#17519=AXIS2_PLACEMENT_3D('',#24669,#20251,#20252);
#17520=AXIS2_PLACEMENT_3D('',#24670,#20253,#20254);
#17521=AXIS2_PLACEMENT_3D('',#24671,#20255,#20256);
#17522=AXIS2_PLACEMENT_3D('',#24672,#20257,#20258);
#17523=AXIS2_PLACEMENT_3D('',#24673,#20259,#20260);
#17524=AXIS2_PLACEMENT_3D('',#24675,#20261,#20262);
#17525=AXIS2_PLACEMENT_3D('',#24677,#20263,#20264);
#17526=AXIS2_PLACEMENT_3D('',#24678,#20265,#20266);
#17527=AXIS2_PLACEMENT_3D('',#24680,#20267,#20268);
#17528=AXIS2_PLACEMENT_3D('',#24682,#20270,#20271);
#17529=AXIS2_PLACEMENT_3D('',#24684,#20272,#20273);
#17530=AXIS2_PLACEMENT_3D('',#24685,#20274,#20275);
#17531=AXIS2_PLACEMENT_3D('',#24687,#20277,#20278);
#17532=AXIS2_PLACEMENT_3D('',#24689,#20279,#20280);
#17533=AXIS2_PLACEMENT_3D('',#24691,#20281,#20282);
#17534=AXIS2_PLACEMENT_3D('',#24692,#20283,#20284);
#17535=AXIS2_PLACEMENT_3D('',#24694,#20285,#20286);
#17536=AXIS2_PLACEMENT_3D('',#24696,#20288,#20289);
#17537=AXIS2_PLACEMENT_3D('',#24698,#20290,#20291);
#17538=AXIS2_PLACEMENT_3D('',#24699,#20292,#20293);
#17539=AXIS2_PLACEMENT_3D('',#24701,#20295,#20296);
#17540=AXIS2_PLACEMENT_3D('',#24702,#20297,#20298);
#17541=AXIS2_PLACEMENT_3D('',#24703,#20299,#20300);
#17542=AXIS2_PLACEMENT_3D('',#24704,#20301,#20302);
#17543=AXIS2_PLACEMENT_3D('',#24705,#20303,#20304);
#17544=AXIS2_PLACEMENT_3D('',#24706,#20305,#20306);
#17545=AXIS2_PLACEMENT_3D('',#24707,#20307,#20308);
#17546=AXIS2_PLACEMENT_3D('',#24708,#20309,#20310);
#17547=AXIS2_PLACEMENT_3D('',#24711,#20311,#20312);
#17548=AXIS2_PLACEMENT_3D('',#24712,#20313,#20314);
#17549=AXIS2_PLACEMENT_3D('',#24714,#20315,#20316);
#17550=AXIS2_PLACEMENT_3D('',#24716,#20317,#20318);
#17551=AXIS2_PLACEMENT_3D('',#24717,#20319,#20320);
#17552=AXIS2_PLACEMENT_3D('',#24718,#20321,#20322);
#17553=AXIS2_PLACEMENT_3D('',#24721,#20324,#20325);
#17554=AXIS2_PLACEMENT_3D('',#24722,#20326,#20327);
#17555=AXIS2_PLACEMENT_3D('',#24724,#20328,#20329);
#17556=AXIS2_PLACEMENT_3D('',#24727,#20331,#20332);
#17557=AXIS2_PLACEMENT_3D('',#24728,#20333,#20334);
#17558=AXIS2_PLACEMENT_3D('',#24731,#20336,#20337);
#17559=AXIS2_PLACEMENT_3D('',#24732,#20338,#20339);
#17560=AXIS2_PLACEMENT_3D('',#24733,#20340,#20341);
#17561=AXIS2_PLACEMENT_3D('',#24735,#20342,#20343);
#17562=AXIS2_PLACEMENT_3D('',#24737,#20345,#20346);
#17563=AXIS2_PLACEMENT_3D('',#24739,#20347,#20348);
#17564=AXIS2_PLACEMENT_3D('',#24740,#20349,#20350);
#17565=AXIS2_PLACEMENT_3D('',#24742,#20352,#20353);
#17566=AXIS2_PLACEMENT_3D('',#24743,#20354,#20355);
#17567=AXIS2_PLACEMENT_3D('',#24746,#20356,#20357);
#17568=AXIS2_PLACEMENT_3D('',#24747,#20358,#20359);
#17569=AXIS2_PLACEMENT_3D('',#24749,#20360,#20361);
#17570=AXIS2_PLACEMENT_3D('',#24751,#20362,#20363);
#17571=AXIS2_PLACEMENT_3D('',#24752,#20364,#20365);
#17572=AXIS2_PLACEMENT_3D('',#24753,#20366,#20367);
#17573=AXIS2_PLACEMENT_3D('',#24755,#20368,#20369);
#17574=AXIS2_PLACEMENT_3D('',#24757,#20371,#20372);
#17575=AXIS2_PLACEMENT_3D('',#24759,#20373,#20374);
#17576=AXIS2_PLACEMENT_3D('',#24761,#20375,#20376);
#17577=AXIS2_PLACEMENT_3D('',#24762,#20377,#20378);
#17578=AXIS2_PLACEMENT_3D('',#24764,#20379,#20380);
#17579=AXIS2_PLACEMENT_3D('',#24766,#20382,#20383);
#17580=AXIS2_PLACEMENT_3D('',#24768,#20384,#20385);
#17581=AXIS2_PLACEMENT_3D('',#24770,#20387,#20388);
#17582=AXIS2_PLACEMENT_3D('',#24772,#20389,#20390);
#17583=AXIS2_PLACEMENT_3D('',#24774,#20392,#20393);
#17584=AXIS2_PLACEMENT_3D('',#24775,#20394,#20395);
#17585=AXIS2_PLACEMENT_3D('',#24777,#20397,#20398);
#17586=AXIS2_PLACEMENT_3D('',#24778,#20399,#20400);
#17587=AXIS2_PLACEMENT_3D('',#24781,#20401,#20402);
#17588=AXIS2_PLACEMENT_3D('',#24782,#20403,#20404);
#17589=AXIS2_PLACEMENT_3D('',#24785,#20405,#20406);
#17590=AXIS2_PLACEMENT_3D('',#24786,#20407,#20408);
#17591=AXIS2_PLACEMENT_3D('',#24789,#20409,#20410);
#17592=AXIS2_PLACEMENT_3D('',#24790,#20411,#20412);
#17593=AXIS2_PLACEMENT_3D('',#24793,#20413,#20414);
#17594=AXIS2_PLACEMENT_3D('',#24794,#20415,#20416);
#17595=AXIS2_PLACEMENT_3D('',#24797,#20417,#20418);
#17596=AXIS2_PLACEMENT_3D('',#24798,#20419,#20420);
#17597=AXIS2_PLACEMENT_3D('',#24801,#20421,#20422);
#17598=AXIS2_PLACEMENT_3D('',#24802,#20423,#20424);
#17599=AXIS2_PLACEMENT_3D('',#24805,#20425,#20426);
#17600=AXIS2_PLACEMENT_3D('',#24806,#20427,#20428);
#17601=AXIS2_PLACEMENT_3D('',#24809,#20429,#20430);
#17602=AXIS2_PLACEMENT_3D('',#24810,#20431,#20432);
#17603=AXIS2_PLACEMENT_3D('',#24811,#20433,#20434);
#17604=AXIS2_PLACEMENT_3D('',#24837,#20435,#20436);
#17605=AXIS2_PLACEMENT_3D('',#24861,#20437,#20438);
#17606=AXIS2_PLACEMENT_3D('',#24862,#20439,#20440);
#17607=AXIS2_PLACEMENT_3D('',#24864,#20441,#20442);
#17608=AXIS2_PLACEMENT_3D('',#24889,#20443,#20444);
#17609=AXIS2_PLACEMENT_3D('',#24914,#20445,#20446);
#17610=AXIS2_PLACEMENT_3D('',#24930,#20448,#20449);
#17611=AXIS2_PLACEMENT_3D('',#24945,#20450,#20451);
#17612=AXIS2_PLACEMENT_3D('',#24970,#20452,#20453);
#17613=AXIS2_PLACEMENT_3D('',#24995,#20454,#20455);
#17614=AXIS2_PLACEMENT_3D('',#25020,#20456,#20457);
#17615=AXIS2_PLACEMENT_3D('',#25044,#20458,#20459);
#17616=AXIS2_PLACEMENT_3D('',#25045,#20460,#20461);
#17617=AXIS2_PLACEMENT_3D('',#25047,#20462,#20463);
#17618=AXIS2_PLACEMENT_3D('',#25048,#20464,#20465);
#17619=AXIS2_PLACEMENT_3D('',#25049,#20466,#20467);
#17620=AXIS2_PLACEMENT_3D('',#25073,#20468,#20469);
#17621=AXIS2_PLACEMENT_3D('',#25074,#20470,#20471);
#17622=AXIS2_PLACEMENT_3D('',#25076,#20472,#20473);
#17623=AXIS2_PLACEMENT_3D('',#25077,#20474,#20475);
#17624=AXIS2_PLACEMENT_3D('',#25078,#20476,#20477);
#17625=AXIS2_PLACEMENT_3D('',#25102,#20478,#20479);
#17626=AXIS2_PLACEMENT_3D('',#25103,#20480,#20481);
#17627=AXIS2_PLACEMENT_3D('',#25105,#20482,#20483);
#17628=AXIS2_PLACEMENT_3D('',#25106,#20484,#20485);
#17629=AXIS2_PLACEMENT_3D('',#25107,#20486,#20487);
#17630=AXIS2_PLACEMENT_3D('',#25122,#20488,#20489);
#17631=AXIS2_PLACEMENT_3D('',#25135,#20490,#20491);
#17632=AXIS2_PLACEMENT_3D('',#25137,#20492,#20493);
#17633=AXIS2_PLACEMENT_3D('',#25138,#20494,#20495);
#17634=AXIS2_PLACEMENT_3D('',#25139,#20496,#20497);
#17635=AXIS2_PLACEMENT_3D('',#25163,#20498,#20499);
#17636=AXIS2_PLACEMENT_3D('',#25164,#20500,#20501);
#17637=AXIS2_PLACEMENT_3D('',#25166,#20502,#20503);
#17638=AXIS2_PLACEMENT_3D('',#25167,#20504,#20505);
#17639=AXIS2_PLACEMENT_3D('',#25168,#20506,#20507);
#17640=AXIS2_PLACEMENT_3D('',#25192,#20508,#20509);
#17641=AXIS2_PLACEMENT_3D('',#25193,#20510,#20511);
#17642=AXIS2_PLACEMENT_3D('',#25195,#20512,#20513);
#17643=AXIS2_PLACEMENT_3D('',#25196,#20514,#20515);
#17644=AXIS2_PLACEMENT_3D('',#25197,#20516,#20517);
#17645=AXIS2_PLACEMENT_3D('',#25221,#20518,#20519);
#17646=AXIS2_PLACEMENT_3D('',#25222,#20520,#20521);
#17647=AXIS2_PLACEMENT_3D('',#25224,#20522,#20523);
#17648=AXIS2_PLACEMENT_3D('',#25227,#20525,#20526);
#17649=AXIS2_PLACEMENT_3D('',#25251,#20527,#20528);
#17650=AXIS2_PLACEMENT_3D('',#25252,#20529,#20530);
#17651=AXIS2_PLACEMENT_3D('',#25253,#20531,#20532);
#17652=AXIS2_PLACEMENT_3D('',#25254,#20533,#20534);
#17653=AXIS2_PLACEMENT_3D('',#25255,#20535,#20536);
#17654=AXIS2_PLACEMENT_3D('',#25256,#20537,#20538);
#17655=AXIS2_PLACEMENT_3D('',#25257,#20539,#20540);
#17656=AXIS2_PLACEMENT_3D('',#25258,#20541,#20542);
#17657=AXIS2_PLACEMENT_3D('',#25259,#20543,#20544);
#17658=AXIS2_PLACEMENT_3D('',#25261,#20545,#20546);
#17659=AXIS2_PLACEMENT_3D('',#25263,#20547,#20548);
#17660=AXIS2_PLACEMENT_3D('',#25264,#20549,#20550);
#17661=AXIS2_PLACEMENT_3D('',#25266,#20551,#20552);
#17662=AXIS2_PLACEMENT_3D('',#25268,#20554,#20555);
#17663=AXIS2_PLACEMENT_3D('',#25270,#20556,#20557);
#17664=AXIS2_PLACEMENT_3D('',#25271,#20558,#20559);
#17665=AXIS2_PLACEMENT_3D('',#25273,#20561,#20562);
#17666=AXIS2_PLACEMENT_3D('',#25275,#20563,#20564);
#17667=AXIS2_PLACEMENT_3D('',#25277,#20565,#20566);
#17668=AXIS2_PLACEMENT_3D('',#25278,#20567,#20568);
#17669=AXIS2_PLACEMENT_3D('',#25280,#20569,#20570);
#17670=AXIS2_PLACEMENT_3D('',#25282,#20572,#20573);
#17671=AXIS2_PLACEMENT_3D('',#25284,#20574,#20575);
#17672=AXIS2_PLACEMENT_3D('',#25285,#20576,#20577);
#17673=AXIS2_PLACEMENT_3D('',#25287,#20579,#20580);
#17674=AXIS2_PLACEMENT_3D('',#25288,#20581,#20582);
#17675=AXIS2_PLACEMENT_3D('',#25289,#20583,#20584);
#17676=AXIS2_PLACEMENT_3D('',#25290,#20585,#20586);
#17677=AXIS2_PLACEMENT_3D('',#25291,#20587,#20588);
#17678=AXIS2_PLACEMENT_3D('',#25292,#20589,#20590);
#17679=AXIS2_PLACEMENT_3D('',#25293,#20591,#20592);
#17680=AXIS2_PLACEMENT_3D('',#25295,#20593,#20594);
#17681=AXIS2_PLACEMENT_3D('',#25296,#20595,#20596);
#17682=AXIS2_PLACEMENT_3D('',#25298,#20597,#20598);
#17683=AXIS2_PLACEMENT_3D('',#25300,#20600,#20601);
#17684=AXIS2_PLACEMENT_3D('',#25302,#20602,#20603);
#17685=AXIS2_PLACEMENT_3D('',#25304,#20605,#20606);
#17686=AXIS2_PLACEMENT_3D('',#25306,#20607,#20608);
#17687=AXIS2_PLACEMENT_3D('',#25308,#20610,#20611);
#17688=AXIS2_PLACEMENT_3D('',#25310,#20612,#20613);
#17689=AXIS2_PLACEMENT_3D('',#25311,#20614,#20615);
#17690=AXIS2_PLACEMENT_3D('',#25313,#20616,#20617);
#17691=AXIS2_PLACEMENT_3D('',#25315,#20619,#20620);
#17692=AXIS2_PLACEMENT_3D('',#25317,#20621,#20622);
#17693=AXIS2_PLACEMENT_3D('',#25319,#20624,#20625);
#17694=AXIS2_PLACEMENT_3D('',#25321,#20626,#20627);
#17695=AXIS2_PLACEMENT_3D('',#25323,#20629,#20630);
#17696=AXIS2_PLACEMENT_3D('',#25324,#20631,#20632);
#17697=AXIS2_PLACEMENT_3D('',#25333,#20637,#20638);
#17698=AXIS2_PLACEMENT_3D('',#25339,#20642,#20643);
#17699=AXIS2_PLACEMENT_3D('',#25345,#20647,#20648);
#17700=AXIS2_PLACEMENT_3D('',#25351,#20652,#20653);
#17701=AXIS2_PLACEMENT_3D('',#25357,#20657,#20658);
#17702=AXIS2_PLACEMENT_3D('',#25360,#20661,#20662);
#17703=AXIS2_PLACEMENT_3D('',#25361,#20663,#20664);
#17704=AXIS2_PLACEMENT_3D('',#25362,#20665,#20666);
#17705=AXIS2_PLACEMENT_3D('',#25363,#20667,#20668);
#17706=AXIS2_PLACEMENT_3D('',#25364,#20669,#20670);
#17707=AXIS2_PLACEMENT_3D('',#25365,#20671,#20672);
#17708=AXIS2_PLACEMENT_3D('',#25366,#20673,#20674);
#17709=AXIS2_PLACEMENT_3D('',#25367,#20675,#20676);
#17710=AXIS2_PLACEMENT_3D('',#25368,#20677,#20678);
#17711=AXIS2_PLACEMENT_3D('',#25369,#20679,#20680);
#17712=AXIS2_PLACEMENT_3D('',#25370,#20681,#20682);
#17713=AXIS2_PLACEMENT_3D('',#25371,#20683,#20684);
#17714=AXIS2_PLACEMENT_3D('',#25372,#20685,#20686);
#17715=AXIS2_PLACEMENT_3D('',#25373,#20687,#20688);
#17716=AXIS2_PLACEMENT_3D('',#25374,#20689,#20690);
#17717=AXIS2_PLACEMENT_3D('',#25375,#20691,#20692);
#17718=AXIS2_PLACEMENT_3D('',#25376,#20693,#20694);
#17719=AXIS2_PLACEMENT_3D('',#25377,#20695,#20696);
#17720=AXIS2_PLACEMENT_3D('',#25378,#20697,#20698);
#17721=AXIS2_PLACEMENT_3D('',#25379,#20699,#20700);
#17722=AXIS2_PLACEMENT_3D('',#25380,#20701,#20702);
#17723=AXIS2_PLACEMENT_3D('',#25381,#20703,#20704);
#17724=AXIS2_PLACEMENT_3D('',#25382,#20705,#20706);
#17725=AXIS2_PLACEMENT_3D('',#25383,#20707,#20708);
#17726=AXIS2_PLACEMENT_3D('',#25384,#20709,#20710);
#17727=AXIS2_PLACEMENT_3D('',#25385,#20711,#20712);
#17728=AXIS2_PLACEMENT_3D('',#25386,#20713,#20714);
#17729=AXIS2_PLACEMENT_3D('',#25387,#20715,#20716);
#17730=AXIS2_PLACEMENT_3D('',#25388,#20717,#20718);
#17731=AXIS2_PLACEMENT_3D('',#25389,#20719,#20720);
#17732=AXIS2_PLACEMENT_3D('',#25390,#20721,#20722);
#17733=AXIS2_PLACEMENT_3D('',#25391,#20723,#20724);
#17734=AXIS2_PLACEMENT_3D('',#25392,#20725,#20726);
#17735=AXIS2_PLACEMENT_3D('',#25393,#20727,#20728);
#17736=AXIS2_PLACEMENT_3D('',#25394,#20729,#20730);
#17737=AXIS2_PLACEMENT_3D('',#25395,#20731,#20732);
#17738=AXIS2_PLACEMENT_3D('',#25396,#20733,#20734);
#17739=AXIS2_PLACEMENT_3D('',#25397,#20735,#20736);
#17740=AXIS2_PLACEMENT_3D('',#25398,#20737,#20738);
#17741=AXIS2_PLACEMENT_3D('',#25399,#20739,#20740);
#17742=AXIS2_PLACEMENT_3D('',#25400,#20741,#20742);
#17743=AXIS2_PLACEMENT_3D('',#25401,#20743,#20744);
#17744=AXIS2_PLACEMENT_3D('',#25402,#20745,#20746);
#17745=AXIS2_PLACEMENT_3D('',#25403,#20747,#20748);
#17746=AXIS2_PLACEMENT_3D('',#25404,#20749,#20750);
#17747=AXIS2_PLACEMENT_3D('',#25405,#20751,#20752);
#17748=AXIS2_PLACEMENT_3D('',#25406,#20753,#20754);
#17749=AXIS2_PLACEMENT_3D('',#25407,#20755,#20756);
#17750=AXIS2_PLACEMENT_3D('',#25408,#20757,#20758);
#17751=AXIS2_PLACEMENT_3D('',#25409,#20759,#20760);
#17752=AXIS2_PLACEMENT_3D('',#25410,#20761,#20762);
#17753=AXIS2_PLACEMENT_3D('',#25411,#20763,#20764);
#17754=AXIS2_PLACEMENT_3D('',#25412,#20765,#20766);
#17755=AXIS2_PLACEMENT_3D('',#25413,#20767,#20768);
#17756=AXIS2_PLACEMENT_3D('',#25414,#20769,#20770);
#17757=AXIS2_PLACEMENT_3D('',#25415,#20771,#20772);
#17758=AXIS2_PLACEMENT_3D('',#25416,#20773,#20774);
#17759=AXIS2_PLACEMENT_3D('',#25417,#20775,#20776);
#17760=AXIS2_PLACEMENT_3D('',#25418,#20777,#20778);
#17761=AXIS2_PLACEMENT_3D('',#25419,#20779,#20780);
#17762=AXIS2_PLACEMENT_3D('',#25420,#20781,#20782);
#17763=AXIS2_PLACEMENT_3D('',#25421,#20783,#20784);
#17764=AXIS2_PLACEMENT_3D('',#25422,#20785,#20786);
#17765=AXIS2_PLACEMENT_3D('',#25423,#20787,#20788);
#17766=AXIS2_PLACEMENT_3D('',#25424,#20789,#20790);
#17767=AXIS2_PLACEMENT_3D('',#25433,#20795,#20796);
#17768=AXIS2_PLACEMENT_3D('',#25435,#20797,#20798);
#17769=AXIS2_PLACEMENT_3D('',#25439,#20801,#20802);
#17770=AXIS2_PLACEMENT_3D('',#25445,#20806,#20807);
#17771=AXIS2_PLACEMENT_3D('',#25447,#20809,#20810);
#17772=AXIS2_PLACEMENT_3D('',#25448,#20811,#20812);
#17773=AXIS2_PLACEMENT_3D('',#25449,#20813,#20814);
#17774=AXIS2_PLACEMENT_3D('',#25451,#20815,#20816);
#17775=AXIS2_PLACEMENT_3D('',#25454,#20818,#20819);
#17776=AXIS2_PLACEMENT_3D('',#25455,#20820,#20821);
#17777=AXIS2_PLACEMENT_3D('',#25456,#20822,#20823);
#17778=AXIS2_PLACEMENT_3D('',#25457,#20824,#20825);
#17779=AXIS2_PLACEMENT_3D('',#25458,#20826,#20827);
#17780=AXIS2_PLACEMENT_3D('',#25462,#20829,#20830);
#17781=AXIS2_PLACEMENT_3D('',#25463,#20831,#20832);
#17782=AXIS2_PLACEMENT_3D('',#25476,#20833,#20834);
#17783=AXIS2_PLACEMENT_3D('',#25517,#20836,#20837);
#17784=AXIS2_PLACEMENT_3D('',#25528,#20838,#20839);
#17785=AXIS2_PLACEMENT_3D('',#25530,#20841,#20842);
#17786=AXIS2_PLACEMENT_3D('',#25532,#20843,#20844);
#17787=AXIS2_PLACEMENT_3D('',#25535,#20846,#20847);
#17788=AXIS2_PLACEMENT_3D('',#25536,#20848,#20849);
#17789=AXIS2_PLACEMENT_3D('',#25538,#20850,#20851);
#17790=AXIS2_PLACEMENT_3D('',#25541,#20853,#20854);
#17791=AXIS2_PLACEMENT_3D('',#25542,#20855,#20856);
#17792=AXIS2_PLACEMENT_3D('',#25543,#20857,#20858);
#17793=AXIS2_PLACEMENT_3D('',#25544,#20859,#20860);
#17794=AXIS2_PLACEMENT_3D('',#25545,#20861,#20862);
#17795=AXIS2_PLACEMENT_3D('',#25549,#20864,#20865);
#17796=AXIS2_PLACEMENT_3D('',#25550,#20866,#20867);
#17797=AXIS2_PLACEMENT_3D('',#25563,#20868,#20869);
#17798=AXIS2_PLACEMENT_3D('',#25604,#20871,#20872);
#17799=AXIS2_PLACEMENT_3D('',#25615,#20873,#20874);
#17800=AXIS2_PLACEMENT_3D('',#25617,#20876,#20877);
#17801=AXIS2_PLACEMENT_3D('',#25619,#20878,#20879);
#17802=AXIS2_PLACEMENT_3D('',#25622,#20881,#20882);
#17803=AXIS2_PLACEMENT_3D('',#25623,#20883,#20884);
#17804=AXIS2_PLACEMENT_3D('',#25625,#20885,#20886);
#17805=AXIS2_PLACEMENT_3D('',#25628,#20888,#20889);
#17806=AXIS2_PLACEMENT_3D('',#25629,#20890,#20891);
#17807=AXIS2_PLACEMENT_3D('',#25630,#20892,#20893);
#17808=AXIS2_PLACEMENT_3D('',#25631,#20894,#20895);
#17809=AXIS2_PLACEMENT_3D('',#25632,#20896,#20897);
#17810=AXIS2_PLACEMENT_3D('',#25634,#20898,#20899);
#17811=AXIS2_PLACEMENT_3D('',#25637,#20901,#20902);
#17812=AXIS2_PLACEMENT_3D('',#25638,#20903,#20904);
#17813=AXIS2_PLACEMENT_3D('',#25640,#20905,#20906);
#17814=AXIS2_PLACEMENT_3D('',#25643,#20908,#20909);
#17815=AXIS2_PLACEMENT_3D('',#25644,#20910,#20911);
#17816=AXIS2_PLACEMENT_3D('',#25645,#20912,#20913);
#17817=AXIS2_PLACEMENT_3D('',#25646,#20914,#20915);
#17818=AXIS2_PLACEMENT_3D('',#25647,#20916,#20917);
#17819=AXIS2_PLACEMENT_3D('',#25649,#20918,#20919);
#17820=AXIS2_PLACEMENT_3D('',#25652,#20921,#20922);
#17821=AXIS2_PLACEMENT_3D('',#25653,#20923,#20924);
#17822=AXIS2_PLACEMENT_3D('',#25655,#20925,#20926);
#17823=AXIS2_PLACEMENT_3D('',#25658,#20928,#20929);
#17824=AXIS2_PLACEMENT_3D('',#25659,#20930,#20931);
#17825=AXIS2_PLACEMENT_3D('',#25660,#20932,#20933);
#17826=AXIS2_PLACEMENT_3D('',#25661,#20934,#20935);
#17827=AXIS2_PLACEMENT_3D('',#25662,#20936,#20937);
#17828=AXIS2_PLACEMENT_3D('',#25664,#20938,#20939);
#17829=AXIS2_PLACEMENT_3D('',#25667,#20941,#20942);
#17830=AXIS2_PLACEMENT_3D('',#25668,#20943,#20944);
#17831=AXIS2_PLACEMENT_3D('',#25670,#20945,#20946);
#17832=AXIS2_PLACEMENT_3D('',#25673,#20948,#20949);
#17833=AXIS2_PLACEMENT_3D('',#25674,#20950,#20951);
#17834=AXIS2_PLACEMENT_3D('',#25675,#20952,#20953);
#17835=AXIS2_PLACEMENT_3D('',#25676,#20954,#20955);
#17836=AXIS2_PLACEMENT_3D('',#25677,#20956,#20957);
#17837=AXIS2_PLACEMENT_3D('',#25679,#20958,#20959);
#17838=AXIS2_PLACEMENT_3D('',#25682,#20961,#20962);
#17839=AXIS2_PLACEMENT_3D('',#25683,#20963,#20964);
#17840=AXIS2_PLACEMENT_3D('',#25685,#20965,#20966);
#17841=AXIS2_PLACEMENT_3D('',#25688,#20968,#20969);
#17842=AXIS2_PLACEMENT_3D('',#25689,#20970,#20971);
#17843=AXIS2_PLACEMENT_3D('',#25690,#20972,#20973);
#17844=AXIS2_PLACEMENT_3D('',#25691,#20974,#20975);
#17845=AXIS2_PLACEMENT_3D('',#25692,#20976,#20977);
#17846=AXIS2_PLACEMENT_3D('',#25701,#20982,#20983);
#17847=AXIS2_PLACEMENT_3D('',#25707,#20987,#20988);
#17848=AXIS2_PLACEMENT_3D('',#25713,#20992,#20993);
#17849=AXIS2_PLACEMENT_3D('',#25716,#20994,#20995);
#17850=AXIS2_PLACEMENT_3D('',#25862,#20997,#20998);
#17851=AXIS2_PLACEMENT_3D('',#26008,#21000,#21001);
#17852=AXIS2_PLACEMENT_3D('',#26154,#21003,#21004);
#17853=AXIS2_PLACEMENT_3D('',#26300,#21006,#21007);
#17854=AXIS2_PLACEMENT_3D('',#26446,#21009,#21010);
#17855=AXIS2_PLACEMENT_3D('',#26592,#21012,#21013);
#17856=AXIS2_PLACEMENT_3D('',#26738,#21015,#21016);
#17857=AXIS2_PLACEMENT_3D('',#26884,#21018,#21019);
#17858=AXIS2_PLACEMENT_3D('',#27030,#21021,#21022);
#17859=AXIS2_PLACEMENT_3D('',#27176,#21024,#21025);
#17860=AXIS2_PLACEMENT_3D('',#27322,#21027,#21028);
#17861=AXIS2_PLACEMENT_3D('',#27468,#21030,#21031);
#17862=AXIS2_PLACEMENT_3D('',#27614,#21033,#21034);
#17863=AXIS2_PLACEMENT_3D('',#27760,#21036,#21037);
#17864=AXIS2_PLACEMENT_3D('',#27906,#21039,#21040);
#17865=AXIS2_PLACEMENT_3D('',#28052,#21042,#21043);
#17866=AXIS2_PLACEMENT_3D('',#28198,#21045,#21046);
#17867=AXIS2_PLACEMENT_3D('',#28344,#21048,#21049);
#17868=AXIS2_PLACEMENT_3D('',#28490,#21051,#21052);
#17869=AXIS2_PLACEMENT_3D('',#28634,#21054,#21055);
#17870=AXIS2_PLACEMENT_3D('',#28635,#21056,#21057);
#17871=AXIS2_PLACEMENT_3D('',#28636,#21058,#21059);
#17872=AXIS2_PLACEMENT_3D('',#28637,#21060,#21061);
#17873=AXIS2_PLACEMENT_3D('',#28639,#21062,#21063);
#17874=AXIS2_PLACEMENT_3D('',#28642,#21065,#21066);
#17875=AXIS2_PLACEMENT_3D('',#28643,#21067,#21068);
#17876=AXIS2_PLACEMENT_3D('',#28858,#21071,#21072);
#17877=AXIS2_PLACEMENT_3D('',#29074,#21076,#21077);
#17878=AXIS2_PLACEMENT_3D('',#29076,#21078,#21079);
#17879=AXIS2_PLACEMENT_3D('',#29290,#21082,#21083);
#17880=AXIS2_PLACEMENT_3D('',#29506,#21087,#21088);
#17881=AXIS2_PLACEMENT_3D('',#29508,#21089,#21090);
#17882=AXIS2_PLACEMENT_3D('',#29722,#21093,#21094);
#17883=AXIS2_PLACEMENT_3D('',#29938,#21098,#21099);
#17884=AXIS2_PLACEMENT_3D('',#29940,#21100,#21101);
#17885=AXIS2_PLACEMENT_3D('',#30154,#21104,#21105);
#17886=AXIS2_PLACEMENT_3D('',#30370,#21109,#21110);
#17887=AXIS2_PLACEMENT_3D('',#30372,#21111,#21112);
#17888=AXIS2_PLACEMENT_3D('',#30586,#21115,#21116);
#17889=AXIS2_PLACEMENT_3D('',#30802,#21120,#21121);
#17890=AXIS2_PLACEMENT_3D('',#30804,#21122,#21123);
#17891=AXIS2_PLACEMENT_3D('',#31018,#21126,#21127);
#17892=AXIS2_PLACEMENT_3D('',#31234,#21131,#21132);
#17893=AXIS2_PLACEMENT_3D('',#31236,#21133,#21134);
#17894=AXIS2_PLACEMENT_3D('',#31450,#21137,#21138);
#17895=AXIS2_PLACEMENT_3D('',#31666,#21142,#21143);
#17896=AXIS2_PLACEMENT_3D('',#31668,#21144,#21145);
#17897=AXIS2_PLACEMENT_3D('',#31882,#21148,#21149);
#17898=AXIS2_PLACEMENT_3D('',#32098,#21153,#21154);
#17899=AXIS2_PLACEMENT_3D('',#32100,#21155,#21156);
#17900=AXIS2_PLACEMENT_3D('',#32314,#21159,#21160);
#17901=AXIS2_PLACEMENT_3D('',#32530,#21164,#21165);
#17902=AXIS2_PLACEMENT_3D('',#32532,#21166,#21167);
#17903=AXIS2_PLACEMENT_3D('',#32746,#21170,#21171);
#17904=AXIS2_PLACEMENT_3D('',#32962,#21175,#21176);
#17905=AXIS2_PLACEMENT_3D('',#32964,#21177,#21178);
#17906=AXIS2_PLACEMENT_3D('',#33178,#21181,#21182);
#17907=AXIS2_PLACEMENT_3D('',#33394,#21186,#21187);
#17908=AXIS2_PLACEMENT_3D('',#33396,#21188,#21189);
#17909=AXIS2_PLACEMENT_3D('',#33610,#21192,#21193);
#17910=AXIS2_PLACEMENT_3D('',#33826,#21197,#21198);
#17911=AXIS2_PLACEMENT_3D('',#33828,#21199,#21200);
#17912=AXIS2_PLACEMENT_3D('',#34042,#21203,#21204);
#17913=AXIS2_PLACEMENT_3D('',#34258,#21208,#21209);
#17914=AXIS2_PLACEMENT_3D('',#34260,#21210,#21211);
#17915=AXIS2_PLACEMENT_3D('',#34474,#21214,#21215);
#17916=AXIS2_PLACEMENT_3D('',#34690,#21219,#21220);
#17917=AXIS2_PLACEMENT_3D('',#34692,#21221,#21222);
#17918=AXIS2_PLACEMENT_3D('',#34906,#21225,#21226);
#17919=AXIS2_PLACEMENT_3D('',#35122,#21230,#21231);
#17920=AXIS2_PLACEMENT_3D('',#35124,#21232,#21233);
#17921=AXIS2_PLACEMENT_3D('',#35338,#21236,#21237);
#17922=AXIS2_PLACEMENT_3D('',#35554,#21241,#21242);
#17923=AXIS2_PLACEMENT_3D('',#35556,#21243,#21244);
#17924=AXIS2_PLACEMENT_3D('',#35770,#21247,#21248);
#17925=AXIS2_PLACEMENT_3D('',#35986,#21252,#21253);
#17926=AXIS2_PLACEMENT_3D('',#35988,#21254,#21255);
#17927=AXIS2_PLACEMENT_3D('',#36202,#21258,#21259);
#17928=AXIS2_PLACEMENT_3D('',#36418,#21263,#21264);
#17929=AXIS2_PLACEMENT_3D('',#36420,#21265,#21266);
#17930=AXIS2_PLACEMENT_3D('',#36634,#21269,#21270);
#17931=AXIS2_PLACEMENT_3D('',#36850,#21274,#21275);
#17932=AXIS2_PLACEMENT_3D('',#36852,#21276,#21277);
#17933=AXIS2_PLACEMENT_3D('',#37066,#21280,#21281);
#17934=AXIS2_PLACEMENT_3D('',#37282,#21285,#21286);
#17935=AXIS2_PLACEMENT_3D('',#37283,#21287,#21288);
#17936=AXIS2_PLACEMENT_3D('',#37284,#21289,#21290);
#17937=AXIS2_PLACEMENT_3D('',#37285,#21291,#21292);
#17938=AXIS2_PLACEMENT_3D('',#37286,#21293,#21294);
#17939=AXIS2_PLACEMENT_3D('',#37303,#21303,#21304);
#17940=AXIS2_PLACEMENT_3D('',#37309,#21308,#21309);
#17941=AXIS2_PLACEMENT_3D('',#37313,#21312,#21313);
#17942=AXIS2_PLACEMENT_3D('',#37317,#21316,#21317);
#17943=AXIS2_PLACEMENT_3D('',#37321,#21320,#21321);
#17944=AXIS2_PLACEMENT_3D('',#37329,#21326,#21327);
#17945=AXIS2_PLACEMENT_3D('',#37331,#21329,#21330);
#17946=AXIS2_PLACEMENT_3D('',#37333,#21332,#21333);
#17947=AXIS2_PLACEMENT_3D('',#37335,#21335,#21336);
#17948=AXIS2_PLACEMENT_3D('',#37336,#21337,#21338);
#17949=AXIS2_PLACEMENT_3D('',#37337,#21339,#21340);
#17950=AXIS2_PLACEMENT_3D('',#37338,#21341,#21342);
#17951=AXIS2_PLACEMENT_3D('',#37347,#21347,#21348);
#17952=AXIS2_PLACEMENT_3D('',#37349,#21349,#21350);
#17953=AXIS2_PLACEMENT_3D('',#37353,#21353,#21354);
#17954=AXIS2_PLACEMENT_3D('',#37359,#21358,#21359);
#17955=AXIS2_PLACEMENT_3D('',#37361,#21361,#21362);
#17956=AXIS2_PLACEMENT_3D('',#37362,#21363,#21364);
#17957=AXIS2_PLACEMENT_3D('',#37363,#21365,#21366);
#17958=AXIS2_PLACEMENT_3D('',#37372,#21371,#21372);
#17959=AXIS2_PLACEMENT_3D('',#37374,#21373,#21374);
#17960=AXIS2_PLACEMENT_3D('',#37378,#21377,#21378);
#17961=AXIS2_PLACEMENT_3D('',#37384,#21382,#21383);
#17962=AXIS2_PLACEMENT_3D('',#37386,#21385,#21386);
#17963=AXIS2_PLACEMENT_3D('',#37387,#21387,#21388);
#17964=AXIS2_PLACEMENT_3D('',#37388,#21389,#21390);
#17965=AXIS2_PLACEMENT_3D('',#37390,#21391,#21392);
#17966=AXIS2_PLACEMENT_3D('',#37393,#21394,#21395);
#17967=AXIS2_PLACEMENT_3D('',#37394,#21396,#21397);
#17968=AXIS2_PLACEMENT_3D('',#37395,#21398,#21399);
#17969=AXIS2_PLACEMENT_3D('',#37396,#21400,#21401);
#17970=AXIS2_PLACEMENT_3D('',#37397,#21402,#21403);
#17971=AXIS2_PLACEMENT_3D('',#37401,#21405,#21406);
#17972=AXIS2_PLACEMENT_3D('',#37402,#21407,#21408);
#17973=AXIS2_PLACEMENT_3D('',#37419,#21409,#21410);
#17974=AXIS2_PLACEMENT_3D('',#37460,#21412,#21413);
#17975=AXIS2_PLACEMENT_3D('',#37475,#21414,#21415);
#17976=AXIS2_PLACEMENT_3D('',#37477,#21417,#21418);
#17977=AXIS2_PLACEMENT_3D('',#37479,#21419,#21420);
#17978=AXIS2_PLACEMENT_3D('',#37482,#21422,#21423);
#17979=AXIS2_PLACEMENT_3D('',#37483,#21424,#21425);
#17980=AXIS2_PLACEMENT_3D('',#37485,#21426,#21427);
#17981=AXIS2_PLACEMENT_3D('',#37488,#21429,#21430);
#17982=AXIS2_PLACEMENT_3D('',#37489,#21431,#21432);
#17983=AXIS2_PLACEMENT_3D('',#37490,#21433,#21434);
#17984=AXIS2_PLACEMENT_3D('',#37491,#21435,#21436);
#17985=AXIS2_PLACEMENT_3D('',#37492,#21437,#21438);
#17986=AXIS2_PLACEMENT_3D('',#37496,#21440,#21441);
#17987=AXIS2_PLACEMENT_3D('',#37497,#21442,#21443);
#17988=AXIS2_PLACEMENT_3D('',#37514,#21444,#21445);
#17989=AXIS2_PLACEMENT_3D('',#37555,#21447,#21448);
#17990=AXIS2_PLACEMENT_3D('',#37570,#21449,#21450);
#17991=AXIS2_PLACEMENT_3D('',#37572,#21452,#21453);
#17992=AXIS2_PLACEMENT_3D('',#37574,#21454,#21455);
#17993=AXIS2_PLACEMENT_3D('',#37577,#21457,#21458);
#17994=AXIS2_PLACEMENT_3D('',#37578,#21459,#21460);
#17995=AXIS2_PLACEMENT_3D('',#37580,#21461,#21462);
#17996=AXIS2_PLACEMENT_3D('',#37583,#21464,#21465);
#17997=AXIS2_PLACEMENT_3D('',#37584,#21466,#21467);
#17998=AXIS2_PLACEMENT_3D('',#37585,#21468,#21469);
#17999=AXIS2_PLACEMENT_3D('',#37586,#21470,#21471);
#18000=AXIS2_PLACEMENT_3D('',#37587,#21472,#21473);
#18001=AXIS2_PLACEMENT_3D('',#37589,#21474,#21475);
#18002=AXIS2_PLACEMENT_3D('',#37592,#21477,#21478);
#18003=AXIS2_PLACEMENT_3D('',#37593,#21479,#21480);
#18004=AXIS2_PLACEMENT_3D('',#37595,#21481,#21482);
#18005=AXIS2_PLACEMENT_3D('',#37598,#21484,#21485);
#18006=AXIS2_PLACEMENT_3D('',#37599,#21486,#21487);
#18007=AXIS2_PLACEMENT_3D('',#37600,#21488,#21489);
#18008=AXIS2_PLACEMENT_3D('',#37601,#21490,#21491);
#18009=AXIS2_PLACEMENT_3D('',#37602,#21492,#21493);
#18010=AXIS2_PLACEMENT_3D('',#37604,#21494,#21495);
#18011=AXIS2_PLACEMENT_3D('',#37607,#21497,#21498);
#18012=AXIS2_PLACEMENT_3D('',#37608,#21499,#21500);
#18013=AXIS2_PLACEMENT_3D('',#37610,#21501,#21502);
#18014=AXIS2_PLACEMENT_3D('',#37613,#21504,#21505);
#18015=AXIS2_PLACEMENT_3D('',#37614,#21506,#21507);
#18016=AXIS2_PLACEMENT_3D('',#37615,#21508,#21509);
#18017=AXIS2_PLACEMENT_3D('',#37616,#21510,#21511);
#18018=AXIS2_PLACEMENT_3D('',#37617,#21512,#21513);
#18019=AXIS2_PLACEMENT_3D('',#37619,#21514,#21515);
#18020=AXIS2_PLACEMENT_3D('',#37622,#21517,#21518);
#18021=AXIS2_PLACEMENT_3D('',#37623,#21519,#21520);
#18022=AXIS2_PLACEMENT_3D('',#37625,#21521,#21522);
#18023=AXIS2_PLACEMENT_3D('',#37628,#21524,#21525);
#18024=AXIS2_PLACEMENT_3D('',#37629,#21526,#21527);
#18025=AXIS2_PLACEMENT_3D('',#37630,#21528,#21529);
#18026=AXIS2_PLACEMENT_3D('',#37631,#21530,#21531);
#18027=AXIS2_PLACEMENT_3D('',#37632,#21532,#21533);
#18028=AXIS2_PLACEMENT_3D('',#37634,#21534,#21535);
#18029=AXIS2_PLACEMENT_3D('',#37637,#21537,#21538);
#18030=AXIS2_PLACEMENT_3D('',#37638,#21539,#21540);
#18031=AXIS2_PLACEMENT_3D('',#37640,#21541,#21542);
#18032=AXIS2_PLACEMENT_3D('',#37643,#21544,#21545);
#18033=AXIS2_PLACEMENT_3D('',#37644,#21546,#21547);
#18034=AXIS2_PLACEMENT_3D('',#37645,#21548,#21549);
#18035=AXIS2_PLACEMENT_3D('',#37646,#21550,#21551);
#18036=AXIS2_PLACEMENT_3D('',#37647,#21552,#21553);
#18037=AXIS2_PLACEMENT_3D('',#37649,#21554,#21555);
#18038=AXIS2_PLACEMENT_3D('',#37652,#21557,#21558);
#18039=AXIS2_PLACEMENT_3D('',#37653,#21559,#21560);
#18040=AXIS2_PLACEMENT_3D('',#37655,#21561,#21562);
#18041=AXIS2_PLACEMENT_3D('',#37658,#21564,#21565);
#18042=AXIS2_PLACEMENT_3D('',#37659,#21566,#21567);
#18043=AXIS2_PLACEMENT_3D('',#37660,#21568,#21569);
#18044=AXIS2_PLACEMENT_3D('',#37661,#21570,#21571);
#18045=AXIS2_PLACEMENT_3D('',#37662,#21572,#21573);
#18046=AXIS2_PLACEMENT_3D('',#37671,#21578,#21579);
#18047=AXIS2_PLACEMENT_3D('',#37677,#21583,#21584);
#18048=AXIS2_PLACEMENT_3D('',#37683,#21588,#21589);
#18049=AXIS2_PLACEMENT_3D('',#37685,#21590,#21591);
#18050=AXIS2_PLACEMENT_3D('',#37686,#21592,#21593);
#18051=AXIS2_PLACEMENT_3D('',#37687,#21594,#21595);
#18052=AXIS2_PLACEMENT_3D('',#37688,#21596,#21597);
#18053=AXIS2_PLACEMENT_3D('',#37689,#21598,#21599);
#18054=AXIS2_PLACEMENT_3D('',#37692,#21600,#21601);
#18055=AXIS2_PLACEMENT_3D('',#37838,#21603,#21604);
#18056=AXIS2_PLACEMENT_3D('',#37984,#21606,#21607);
#18057=AXIS2_PLACEMENT_3D('',#38130,#21609,#21610);
#18058=AXIS2_PLACEMENT_3D('',#38276,#21612,#21613);
#18059=AXIS2_PLACEMENT_3D('',#38422,#21615,#21616);
#18060=AXIS2_PLACEMENT_3D('',#38568,#21618,#21619);
#18061=AXIS2_PLACEMENT_3D('',#38714,#21621,#21622);
#18062=AXIS2_PLACEMENT_3D('',#38860,#21624,#21625);
#18063=AXIS2_PLACEMENT_3D('',#39006,#21627,#21628);
#18064=AXIS2_PLACEMENT_3D('',#39152,#21630,#21631);
#18065=AXIS2_PLACEMENT_3D('',#39298,#21633,#21634);
#18066=AXIS2_PLACEMENT_3D('',#39444,#21636,#21637);
#18067=AXIS2_PLACEMENT_3D('',#39590,#21639,#21640);
#18068=AXIS2_PLACEMENT_3D('',#39736,#21642,#21643);
#18069=AXIS2_PLACEMENT_3D('',#39882,#21645,#21646);
#18070=AXIS2_PLACEMENT_3D('',#40028,#21648,#21649);
#18071=AXIS2_PLACEMENT_3D('',#40174,#21651,#21652);
#18072=AXIS2_PLACEMENT_3D('',#40320,#21654,#21655);
#18073=AXIS2_PLACEMENT_3D('',#40466,#21657,#21658);
#18074=AXIS2_PLACEMENT_3D('',#40610,#21660,#21661);
#18075=AXIS2_PLACEMENT_3D('',#40613,#21663,#21664);
#18076=AXIS2_PLACEMENT_3D('',#40828,#21667,#21668);
#18077=AXIS2_PLACEMENT_3D('',#41044,#21672,#21673);
#18078=AXIS2_PLACEMENT_3D('',#41046,#21674,#21675);
#18079=AXIS2_PLACEMENT_3D('',#41260,#21678,#21679);
#18080=AXIS2_PLACEMENT_3D('',#41476,#21683,#21684);
#18081=AXIS2_PLACEMENT_3D('',#41478,#21685,#21686);
#18082=AXIS2_PLACEMENT_3D('',#41692,#21689,#21690);
#18083=AXIS2_PLACEMENT_3D('',#41908,#21694,#21695);
#18084=AXIS2_PLACEMENT_3D('',#41910,#21696,#21697);
#18085=AXIS2_PLACEMENT_3D('',#42124,#21700,#21701);
#18086=AXIS2_PLACEMENT_3D('',#42340,#21705,#21706);
#18087=AXIS2_PLACEMENT_3D('',#42342,#21707,#21708);
#18088=AXIS2_PLACEMENT_3D('',#42556,#21711,#21712);
#18089=AXIS2_PLACEMENT_3D('',#42772,#21716,#21717);
#18090=AXIS2_PLACEMENT_3D('',#42774,#21718,#21719);
#18091=AXIS2_PLACEMENT_3D('',#42988,#21722,#21723);
#18092=AXIS2_PLACEMENT_3D('',#43204,#21727,#21728);
#18093=AXIS2_PLACEMENT_3D('',#43206,#21729,#21730);
#18094=AXIS2_PLACEMENT_3D('',#43420,#21733,#21734);
#18095=AXIS2_PLACEMENT_3D('',#43636,#21738,#21739);
#18096=AXIS2_PLACEMENT_3D('',#43638,#21740,#21741);
#18097=AXIS2_PLACEMENT_3D('',#43852,#21744,#21745);
#18098=AXIS2_PLACEMENT_3D('',#44068,#21749,#21750);
#18099=AXIS2_PLACEMENT_3D('',#44070,#21751,#21752);
#18100=AXIS2_PLACEMENT_3D('',#44284,#21755,#21756);
#18101=AXIS2_PLACEMENT_3D('',#44500,#21760,#21761);
#18102=AXIS2_PLACEMENT_3D('',#44502,#21762,#21763);
#18103=AXIS2_PLACEMENT_3D('',#44716,#21766,#21767);
#18104=AXIS2_PLACEMENT_3D('',#44932,#21771,#21772);
#18105=AXIS2_PLACEMENT_3D('',#44934,#21773,#21774);
#18106=AXIS2_PLACEMENT_3D('',#45148,#21777,#21778);
#18107=AXIS2_PLACEMENT_3D('',#45364,#21782,#21783);
#18108=AXIS2_PLACEMENT_3D('',#45366,#21784,#21785);
#18109=AXIS2_PLACEMENT_3D('',#45580,#21788,#21789);
#18110=AXIS2_PLACEMENT_3D('',#45796,#21793,#21794);
#18111=AXIS2_PLACEMENT_3D('',#45798,#21795,#21796);
#18112=AXIS2_PLACEMENT_3D('',#46012,#21799,#21800);
#18113=AXIS2_PLACEMENT_3D('',#46228,#21804,#21805);
#18114=AXIS2_PLACEMENT_3D('',#46230,#21806,#21807);
#18115=AXIS2_PLACEMENT_3D('',#46444,#21810,#21811);
#18116=AXIS2_PLACEMENT_3D('',#46660,#21815,#21816);
#18117=AXIS2_PLACEMENT_3D('',#46662,#21817,#21818);
#18118=AXIS2_PLACEMENT_3D('',#46876,#21821,#21822);
#18119=AXIS2_PLACEMENT_3D('',#47092,#21826,#21827);
#18120=AXIS2_PLACEMENT_3D('',#47094,#21828,#21829);
#18121=AXIS2_PLACEMENT_3D('',#47308,#21832,#21833);
#18122=AXIS2_PLACEMENT_3D('',#47524,#21837,#21838);
#18123=AXIS2_PLACEMENT_3D('',#47526,#21839,#21840);
#18124=AXIS2_PLACEMENT_3D('',#47740,#21843,#21844);
#18125=AXIS2_PLACEMENT_3D('',#47956,#21848,#21849);
#18126=AXIS2_PLACEMENT_3D('',#47958,#21850,#21851);
#18127=AXIS2_PLACEMENT_3D('',#48172,#21854,#21855);
#18128=AXIS2_PLACEMENT_3D('',#48388,#21859,#21860);
#18129=AXIS2_PLACEMENT_3D('',#48390,#21861,#21862);
#18130=AXIS2_PLACEMENT_3D('',#48604,#21865,#21866);
#18131=AXIS2_PLACEMENT_3D('',#48820,#21870,#21871);
#18132=AXIS2_PLACEMENT_3D('',#48822,#21872,#21873);
#18133=AXIS2_PLACEMENT_3D('',#49036,#21876,#21877);
#18134=AXIS2_PLACEMENT_3D('',#49252,#21881,#21882);
#18135=AXIS2_PLACEMENT_3D('',#49253,#21883,#21884);
#18136=AXIS2_PLACEMENT_3D('',#49254,#21885,#21886);
#18137=AXIS2_PLACEMENT_3D('',#49255,#21887,#21888);
#18138=AXIS2_PLACEMENT_3D('',#49256,#21889,#21890);
#18139=AXIS2_PLACEMENT_3D('',#49257,#21891,#21892);
#18140=AXIS2_PLACEMENT_3D('',#49266,#21897,#21898);
#18141=AXIS2_PLACEMENT_3D('',#49268,#21899,#21900);
#18142=AXIS2_PLACEMENT_3D('',#49272,#21903,#21904);
#18143=AXIS2_PLACEMENT_3D('',#49278,#21908,#21909);
#18144=AXIS2_PLACEMENT_3D('',#49280,#21911,#21912);
#18145=AXIS2_PLACEMENT_3D('',#49281,#21913,#21914);
#18146=AXIS2_PLACEMENT_3D('',#49282,#21915,#21916);
#18147=AXIS2_PLACEMENT_3D('',#49284,#21917,#21918);
#18148=AXIS2_PLACEMENT_3D('',#49287,#21920,#21921);
#18149=AXIS2_PLACEMENT_3D('',#49288,#21922,#21923);
#18150=AXIS2_PLACEMENT_3D('',#49289,#21924,#21925);
#18151=AXIS2_PLACEMENT_3D('',#49290,#21926,#21927);
#18152=AXIS2_PLACEMENT_3D('',#49291,#21928,#21929);
#18153=AXIS2_PLACEMENT_3D('',#49295,#21931,#21932);
#18154=AXIS2_PLACEMENT_3D('',#49296,#21933,#21934);
#18155=AXIS2_PLACEMENT_3D('',#49313,#21935,#21936);
#18156=AXIS2_PLACEMENT_3D('',#49354,#21938,#21939);
#18157=AXIS2_PLACEMENT_3D('',#49369,#21940,#21941);
#18158=AXIS2_PLACEMENT_3D('',#49371,#21943,#21944);
#18159=AXIS2_PLACEMENT_3D('',#49373,#21945,#21946);
#18160=AXIS2_PLACEMENT_3D('',#49376,#21948,#21949);
#18161=AXIS2_PLACEMENT_3D('',#49377,#21950,#21951);
#18162=AXIS2_PLACEMENT_3D('',#49379,#21952,#21953);
#18163=AXIS2_PLACEMENT_3D('',#49382,#21955,#21956);
#18164=AXIS2_PLACEMENT_3D('',#49383,#21957,#21958);
#18165=AXIS2_PLACEMENT_3D('',#49384,#21959,#21960);
#18166=AXIS2_PLACEMENT_3D('',#49385,#21961,#21962);
#18167=AXIS2_PLACEMENT_3D('',#49386,#21963,#21964);
#18168=AXIS2_PLACEMENT_3D('',#49390,#21966,#21967);
#18169=AXIS2_PLACEMENT_3D('',#49391,#21968,#21969);
#18170=AXIS2_PLACEMENT_3D('',#49408,#21970,#21971);
#18171=AXIS2_PLACEMENT_3D('',#49449,#21973,#21974);
#18172=AXIS2_PLACEMENT_3D('',#49464,#21975,#21976);
#18173=AXIS2_PLACEMENT_3D('',#49466,#21978,#21979);
#18174=AXIS2_PLACEMENT_3D('',#49468,#21980,#21981);
#18175=AXIS2_PLACEMENT_3D('',#49471,#21983,#21984);
#18176=AXIS2_PLACEMENT_3D('',#49472,#21985,#21986);
#18177=AXIS2_PLACEMENT_3D('',#49474,#21987,#21988);
#18178=AXIS2_PLACEMENT_3D('',#49477,#21990,#21991);
#18179=AXIS2_PLACEMENT_3D('',#49478,#21992,#21993);
#18180=AXIS2_PLACEMENT_3D('',#49479,#21994,#21995);
#18181=AXIS2_PLACEMENT_3D('',#49480,#21996,#21997);
#18182=AXIS2_PLACEMENT_3D('',#49481,#21998,#21999);
#18183=AXIS2_PLACEMENT_3D('',#49483,#22000,#22001);
#18184=AXIS2_PLACEMENT_3D('',#49486,#22003,#22004);
#18185=AXIS2_PLACEMENT_3D('',#49487,#22005,#22006);
#18186=AXIS2_PLACEMENT_3D('',#49489,#22007,#22008);
#18187=AXIS2_PLACEMENT_3D('',#49492,#22010,#22011);
#18188=AXIS2_PLACEMENT_3D('',#49493,#22012,#22013);
#18189=AXIS2_PLACEMENT_3D('',#49494,#22014,#22015);
#18190=AXIS2_PLACEMENT_3D('',#49495,#22016,#22017);
#18191=AXIS2_PLACEMENT_3D('',#49496,#22018,#22019);
#18192=AXIS2_PLACEMENT_3D('',#49498,#22020,#22021);
#18193=AXIS2_PLACEMENT_3D('',#49501,#22023,#22024);
#18194=AXIS2_PLACEMENT_3D('',#49502,#22025,#22026);
#18195=AXIS2_PLACEMENT_3D('',#49504,#22027,#22028);
#18196=AXIS2_PLACEMENT_3D('',#49507,#22030,#22031);
#18197=AXIS2_PLACEMENT_3D('',#49508,#22032,#22033);
#18198=AXIS2_PLACEMENT_3D('',#49509,#22034,#22035);
#18199=AXIS2_PLACEMENT_3D('',#49510,#22036,#22037);
#18200=AXIS2_PLACEMENT_3D('',#49511,#22038,#22039);
#18201=AXIS2_PLACEMENT_3D('',#49513,#22040,#22041);
#18202=AXIS2_PLACEMENT_3D('',#49516,#22043,#22044);
#18203=AXIS2_PLACEMENT_3D('',#49517,#22045,#22046);
#18204=AXIS2_PLACEMENT_3D('',#49519,#22047,#22048);
#18205=AXIS2_PLACEMENT_3D('',#49522,#22050,#22051);
#18206=AXIS2_PLACEMENT_3D('',#49523,#22052,#22053);
#18207=AXIS2_PLACEMENT_3D('',#49524,#22054,#22055);
#18208=AXIS2_PLACEMENT_3D('',#49525,#22056,#22057);
#18209=AXIS2_PLACEMENT_3D('',#49526,#22058,#22059);
#18210=AXIS2_PLACEMENT_3D('',#49528,#22060,#22061);
#18211=AXIS2_PLACEMENT_3D('',#49531,#22063,#22064);
#18212=AXIS2_PLACEMENT_3D('',#49532,#22065,#22066);
#18213=AXIS2_PLACEMENT_3D('',#49534,#22067,#22068);
#18214=AXIS2_PLACEMENT_3D('',#49537,#22070,#22071);
#18215=AXIS2_PLACEMENT_3D('',#49538,#22072,#22073);
#18216=AXIS2_PLACEMENT_3D('',#49539,#22074,#22075);
#18217=AXIS2_PLACEMENT_3D('',#49540,#22076,#22077);
#18218=AXIS2_PLACEMENT_3D('',#49541,#22078,#22079);
#18219=AXIS2_PLACEMENT_3D('',#49550,#22084,#22085);
#18220=AXIS2_PLACEMENT_3D('',#49556,#22089,#22090);
#18221=AXIS2_PLACEMENT_3D('',#49562,#22094,#22095);
#18222=AXIS2_PLACEMENT_3D('',#49568,#22099,#22100);
#18223=AXIS2_PLACEMENT_3D('',#49574,#22104,#22105);
#18224=AXIS2_PLACEMENT_3D('',#49577,#22108,#22109);
#18225=AXIS2_PLACEMENT_3D('',#49578,#22110,#22111);
#18226=AXIS2_PLACEMENT_3D('',#49580,#22112,#22113);
#18227=AXIS2_PLACEMENT_3D('',#49581,#22114,#22115);
#18228=AXIS2_PLACEMENT_3D('',#49583,#22116,#22117);
#18229=AXIS2_PLACEMENT_3D('',#49585,#22119,#22120);
#18230=AXIS2_PLACEMENT_3D('',#49587,#22121,#22122);
#18231=AXIS2_PLACEMENT_3D('',#49589,#22124,#22125);
#18232=AXIS2_PLACEMENT_3D('',#49591,#22126,#22127);
#18233=AXIS2_PLACEMENT_3D('',#49593,#22129,#22130);
#18234=AXIS2_PLACEMENT_3D('',#49594,#22131,#22132);
#18235=AXIS2_PLACEMENT_3D('',#49595,#22133,#22134);
#18236=AXIS2_PLACEMENT_3D('',#49596,#22135,#22136);
#18237=AXIS2_PLACEMENT_3D('',#49597,#22137,#22138);
#18238=AXIS2_PLACEMENT_3D('',#49598,#22139,#22140);
#18239=AXIS2_PLACEMENT_3D('',#49599,#22141,#22142);
#18240=AXIS2_PLACEMENT_3D('',#49600,#22143,#22144);
#18241=AXIS2_PLACEMENT_3D('',#49601,#22145,#22146);
#18242=AXIS2_PLACEMENT_3D('',#49602,#22147,#22148);
#18243=AXIS2_PLACEMENT_3D('',#49603,#22149,#22150);
#18244=AXIS2_PLACEMENT_3D('',#49604,#22151,#22152);
#18245=AXIS2_PLACEMENT_3D('',#49605,#22153,#22154);
#18246=AXIS2_PLACEMENT_3D('',#49606,#22155,#22156);
#18247=AXIS2_PLACEMENT_3D('',#49615,#22161,#22162);
#18248=AXIS2_PLACEMENT_3D('',#49621,#22166,#22167);
#18249=AXIS2_PLACEMENT_3D('',#49627,#22171,#22172);
#18250=AXIS2_PLACEMENT_3D('',#49630,#22173,#22174);
#18251=AXIS2_PLACEMENT_3D('',#49776,#22176,#22177);
#18252=AXIS2_PLACEMENT_3D('',#49922,#22179,#22180);
#18253=AXIS2_PLACEMENT_3D('',#50068,#22182,#22183);
#18254=AXIS2_PLACEMENT_3D('',#50214,#22185,#22186);
#18255=AXIS2_PLACEMENT_3D('',#50360,#22188,#22189);
#18256=AXIS2_PLACEMENT_3D('',#50506,#22191,#22192);
#18257=AXIS2_PLACEMENT_3D('',#50652,#22194,#22195);
#18258=AXIS2_PLACEMENT_3D('',#50798,#22197,#22198);
#18259=AXIS2_PLACEMENT_3D('',#50944,#22200,#22201);
#18260=AXIS2_PLACEMENT_3D('',#51090,#22203,#22204);
#18261=AXIS2_PLACEMENT_3D('',#51236,#22206,#22207);
#18262=AXIS2_PLACEMENT_3D('',#51382,#22209,#22210);
#18263=AXIS2_PLACEMENT_3D('',#51528,#22212,#22213);
#18264=AXIS2_PLACEMENT_3D('',#51674,#22215,#22216);
#18265=AXIS2_PLACEMENT_3D('',#51820,#22218,#22219);
#18266=AXIS2_PLACEMENT_3D('',#51966,#22221,#22222);
#18267=AXIS2_PLACEMENT_3D('',#52112,#22224,#22225);
#18268=AXIS2_PLACEMENT_3D('',#52258,#22227,#22228);
#18269=AXIS2_PLACEMENT_3D('',#52404,#22230,#22231);
#18270=AXIS2_PLACEMENT_3D('',#52550,#22233,#22234);
#18271=AXIS2_PLACEMENT_3D('',#52696,#22236,#22237);
#18272=AXIS2_PLACEMENT_3D('',#52842,#22239,#22240);
#18273=AXIS2_PLACEMENT_3D('',#52988,#22242,#22243);
#18274=AXIS2_PLACEMENT_3D('',#53134,#22245,#22246);
#18275=AXIS2_PLACEMENT_3D('',#53280,#22248,#22249);
#18276=AXIS2_PLACEMENT_3D('',#53426,#22251,#22252);
#18277=AXIS2_PLACEMENT_3D('',#53572,#22254,#22255);
#18278=AXIS2_PLACEMENT_3D('',#53718,#22257,#22258);
#18279=AXIS2_PLACEMENT_3D('',#53864,#22260,#22261);
#18280=AXIS2_PLACEMENT_3D('',#54010,#22263,#22264);
#18281=AXIS2_PLACEMENT_3D('',#54156,#22266,#22267);
#18282=AXIS2_PLACEMENT_3D('',#54302,#22269,#22270);
#18283=AXIS2_PLACEMENT_3D('',#54448,#22272,#22273);
#18284=AXIS2_PLACEMENT_3D('',#54594,#22275,#22276);
#18285=AXIS2_PLACEMENT_3D('',#54740,#22278,#22279);
#18286=AXIS2_PLACEMENT_3D('',#54886,#22281,#22282);
#18287=AXIS2_PLACEMENT_3D('',#55032,#22284,#22285);
#18288=AXIS2_PLACEMENT_3D('',#55178,#22287,#22288);
#18289=AXIS2_PLACEMENT_3D('',#55324,#22290,#22291);
#18290=AXIS2_PLACEMENT_3D('',#55468,#22293,#22294);
#18291=AXIS2_PLACEMENT_3D('',#55469,#22295,#22296);
#18292=AXIS2_PLACEMENT_3D('',#55470,#22297,#22298);
#18293=AXIS2_PLACEMENT_3D('',#55471,#22299,#22300);
#18294=AXIS2_PLACEMENT_3D('',#55473,#22301,#22302);
#18295=AXIS2_PLACEMENT_3D('',#55476,#22304,#22305);
#18296=AXIS2_PLACEMENT_3D('',#55477,#22306,#22307);
#18297=AXIS2_PLACEMENT_3D('',#55916,#22310,#22311);
#18298=AXIS2_PLACEMENT_3D('',#55918,#22313,#22314);
#18299=AXIS2_PLACEMENT_3D('',#55920,#22315,#22316);
#18300=AXIS2_PLACEMENT_3D('',#56358,#22319,#22320);
#18301=AXIS2_PLACEMENT_3D('',#56360,#22322,#22323);
#18302=AXIS2_PLACEMENT_3D('',#56362,#22324,#22325);
#18303=AXIS2_PLACEMENT_3D('',#56800,#22328,#22329);
#18304=AXIS2_PLACEMENT_3D('',#56802,#22331,#22332);
#18305=AXIS2_PLACEMENT_3D('',#56804,#22333,#22334);
#18306=AXIS2_PLACEMENT_3D('',#57242,#22337,#22338);
#18307=AXIS2_PLACEMENT_3D('',#57244,#22340,#22341);
#18308=AXIS2_PLACEMENT_3D('',#57246,#22342,#22343);
#18309=AXIS2_PLACEMENT_3D('',#57684,#22346,#22347);
#18310=AXIS2_PLACEMENT_3D('',#57686,#22349,#22350);
#18311=AXIS2_PLACEMENT_3D('',#57688,#22351,#22352);
#18312=AXIS2_PLACEMENT_3D('',#58126,#22355,#22356);
#18313=AXIS2_PLACEMENT_3D('',#58128,#22358,#22359);
#18314=AXIS2_PLACEMENT_3D('',#58130,#22360,#22361);
#18315=AXIS2_PLACEMENT_3D('',#58568,#22364,#22365);
#18316=AXIS2_PLACEMENT_3D('',#58570,#22367,#22368);
#18317=AXIS2_PLACEMENT_3D('',#58572,#22369,#22370);
#18318=AXIS2_PLACEMENT_3D('',#59010,#22373,#22374);
#18319=AXIS2_PLACEMENT_3D('',#59012,#22376,#22377);
#18320=AXIS2_PLACEMENT_3D('',#59014,#22378,#22379);
#18321=AXIS2_PLACEMENT_3D('',#59452,#22382,#22383);
#18322=AXIS2_PLACEMENT_3D('',#59454,#22385,#22386);
#18323=AXIS2_PLACEMENT_3D('',#59456,#22387,#22388);
#18324=AXIS2_PLACEMENT_3D('',#59894,#22391,#22392);
#18325=AXIS2_PLACEMENT_3D('',#59896,#22394,#22395);
#18326=AXIS2_PLACEMENT_3D('',#59898,#22396,#22397);
#18327=AXIS2_PLACEMENT_3D('',#60336,#22400,#22401);
#18328=AXIS2_PLACEMENT_3D('',#60338,#22403,#22404);
#18329=AXIS2_PLACEMENT_3D('',#60340,#22405,#22406);
#18330=AXIS2_PLACEMENT_3D('',#60778,#22409,#22410);
#18331=AXIS2_PLACEMENT_3D('',#60780,#22412,#22413);
#18332=AXIS2_PLACEMENT_3D('',#60782,#22414,#22415);
#18333=AXIS2_PLACEMENT_3D('',#61220,#22418,#22419);
#18334=AXIS2_PLACEMENT_3D('',#61222,#22421,#22422);
#18335=AXIS2_PLACEMENT_3D('',#61224,#22423,#22424);
#18336=AXIS2_PLACEMENT_3D('',#61662,#22427,#22428);
#18337=AXIS2_PLACEMENT_3D('',#61664,#22430,#22431);
#18338=AXIS2_PLACEMENT_3D('',#61666,#22432,#22433);
#18339=AXIS2_PLACEMENT_3D('',#62104,#22436,#22437);
#18340=AXIS2_PLACEMENT_3D('',#62106,#22439,#22440);
#18341=AXIS2_PLACEMENT_3D('',#62108,#22441,#22442);
#18342=AXIS2_PLACEMENT_3D('',#62546,#22445,#22446);
#18343=AXIS2_PLACEMENT_3D('',#62548,#22448,#22449);
#18344=AXIS2_PLACEMENT_3D('',#62550,#22450,#22451);
#18345=AXIS2_PLACEMENT_3D('',#62988,#22454,#22455);
#18346=AXIS2_PLACEMENT_3D('',#62990,#22457,#22458);
#18347=AXIS2_PLACEMENT_3D('',#62992,#22459,#22460);
#18348=AXIS2_PLACEMENT_3D('',#63430,#22463,#22464);
#18349=AXIS2_PLACEMENT_3D('',#63432,#22466,#22467);
#18350=AXIS2_PLACEMENT_3D('',#63434,#22468,#22469);
#18351=AXIS2_PLACEMENT_3D('',#63872,#22472,#22473);
#18352=AXIS2_PLACEMENT_3D('',#63874,#22475,#22476);
#18353=AXIS2_PLACEMENT_3D('',#63876,#22477,#22478);
#18354=AXIS2_PLACEMENT_3D('',#64314,#22481,#22482);
#18355=AXIS2_PLACEMENT_3D('',#64316,#22484,#22485);
#18356=AXIS2_PLACEMENT_3D('',#64318,#22486,#22487);
#18357=AXIS2_PLACEMENT_3D('',#64756,#22490,#22491);
#18358=AXIS2_PLACEMENT_3D('',#64758,#22493,#22494);
#18359=AXIS2_PLACEMENT_3D('',#64760,#22495,#22496);
#18360=AXIS2_PLACEMENT_3D('',#65198,#22499,#22500);
#18361=AXIS2_PLACEMENT_3D('',#65200,#22502,#22503);
#18362=AXIS2_PLACEMENT_3D('',#65202,#22504,#22505);
#18363=AXIS2_PLACEMENT_3D('',#65640,#22508,#22509);
#18364=AXIS2_PLACEMENT_3D('',#65642,#22511,#22512);
#18365=AXIS2_PLACEMENT_3D('',#65644,#22513,#22514);
#18366=AXIS2_PLACEMENT_3D('',#66082,#22517,#22518);
#18367=AXIS2_PLACEMENT_3D('',#66084,#22520,#22521);
#18368=AXIS2_PLACEMENT_3D('',#66086,#22522,#22523);
#18369=AXIS2_PLACEMENT_3D('',#66524,#22526,#22527);
#18370=AXIS2_PLACEMENT_3D('',#66526,#22529,#22530);
#18371=AXIS2_PLACEMENT_3D('',#66528,#22531,#22532);
#18372=AXIS2_PLACEMENT_3D('',#66966,#22535,#22536);
#18373=AXIS2_PLACEMENT_3D('',#66968,#22538,#22539);
#18374=AXIS2_PLACEMENT_3D('',#66970,#22540,#22541);
#18375=AXIS2_PLACEMENT_3D('',#67408,#22544,#22545);
#18376=AXIS2_PLACEMENT_3D('',#67410,#22547,#22548);
#18377=AXIS2_PLACEMENT_3D('',#67412,#22549,#22550);
#18378=AXIS2_PLACEMENT_3D('',#67850,#22553,#22554);
#18379=AXIS2_PLACEMENT_3D('',#67852,#22556,#22557);
#18380=AXIS2_PLACEMENT_3D('',#67854,#22558,#22559);
#18381=AXIS2_PLACEMENT_3D('',#68292,#22562,#22563);
#18382=AXIS2_PLACEMENT_3D('',#68294,#22565,#22566);
#18383=AXIS2_PLACEMENT_3D('',#68296,#22567,#22568);
#18384=AXIS2_PLACEMENT_3D('',#68734,#22571,#22572);
#18385=AXIS2_PLACEMENT_3D('',#68736,#22574,#22575);
#18386=AXIS2_PLACEMENT_3D('',#68738,#22576,#22577);
#18387=AXIS2_PLACEMENT_3D('',#69176,#22580,#22581);
#18388=AXIS2_PLACEMENT_3D('',#69178,#22583,#22584);
#18389=AXIS2_PLACEMENT_3D('',#69180,#22585,#22586);
#18390=AXIS2_PLACEMENT_3D('',#69618,#22589,#22590);
#18391=AXIS2_PLACEMENT_3D('',#69620,#22592,#22593);
#18392=AXIS2_PLACEMENT_3D('',#69622,#22594,#22595);
#18393=AXIS2_PLACEMENT_3D('',#70060,#22598,#22599);
#18394=AXIS2_PLACEMENT_3D('',#70062,#22601,#22602);
#18395=AXIS2_PLACEMENT_3D('',#70064,#22603,#22604);
#18396=AXIS2_PLACEMENT_3D('',#70502,#22607,#22608);
#18397=AXIS2_PLACEMENT_3D('',#70504,#22610,#22611);
#18398=AXIS2_PLACEMENT_3D('',#70506,#22612,#22613);
#18399=AXIS2_PLACEMENT_3D('',#70944,#22616,#22617);
#18400=AXIS2_PLACEMENT_3D('',#70946,#22619,#22620);
#18401=AXIS2_PLACEMENT_3D('',#70948,#22621,#22622);
#18402=AXIS2_PLACEMENT_3D('',#71386,#22625,#22626);
#18403=AXIS2_PLACEMENT_3D('',#71388,#22628,#22629);
#18404=AXIS2_PLACEMENT_3D('',#71390,#22630,#22631);
#18405=AXIS2_PLACEMENT_3D('',#71828,#22634,#22635);
#18406=AXIS2_PLACEMENT_3D('',#71830,#22637,#22638);
#18407=AXIS2_PLACEMENT_3D('',#71832,#22639,#22640);
#18408=AXIS2_PLACEMENT_3D('',#72270,#22643,#22644);
#18409=AXIS2_PLACEMENT_3D('',#72272,#22646,#22647);
#18410=AXIS2_PLACEMENT_3D('',#72274,#22648,#22649);
#18411=AXIS2_PLACEMENT_3D('',#72493,#22651,#22652);
#18412=AXIS2_PLACEMENT_3D('',#72714,#22655,#22656);
#18413=AXIS2_PLACEMENT_3D('',#72716,#22657,#22658);
#18414=AXIS2_PLACEMENT_3D('',#73154,#22661,#22662);
#18415=AXIS2_PLACEMENT_3D('',#73156,#22664,#22665);
#18416=AXIS2_PLACEMENT_3D('',#73157,#22666,#22667);
#18417=AXIS2_PLACEMENT_3D('',#73158,#22668,#22669);
#18418=AXIS2_PLACEMENT_3D('',#73159,#22670,#22671);
#18419=AXIS2_PLACEMENT_3D('',#73160,#22672,#22673);
#18420=AXIS2_PLACEMENT_3D('',#73177,#22682,#22683);
#18421=AXIS2_PLACEMENT_3D('',#73183,#22687,#22688);
#18422=AXIS2_PLACEMENT_3D('',#73187,#22691,#22692);
#18423=AXIS2_PLACEMENT_3D('',#73191,#22695,#22696);
#18424=AXIS2_PLACEMENT_3D('',#73195,#22699,#22700);
#18425=AXIS2_PLACEMENT_3D('',#73203,#22705,#22706);
#18426=AXIS2_PLACEMENT_3D('',#73205,#22708,#22709);
#18427=AXIS2_PLACEMENT_3D('',#73207,#22711,#22712);
#18428=AXIS2_PLACEMENT_3D('',#73209,#22714,#22715);
#18429=AXIS2_PLACEMENT_3D('',#73210,#22716,#22717);
#18430=AXIS2_PLACEMENT_3D('',#73211,#22718,#22719);
#18431=AXIS2_PLACEMENT_3D('',#73212,#22720,#22721);
#18432=AXIS2_PLACEMENT_3D('',#73213,#22722,#22723);
#18433=AXIS2_PLACEMENT_3D('',#73214,#22724,#22725);
#18434=AXIS2_PLACEMENT_3D('',#73215,#22726,#22727);
#18435=AXIS2_PLACEMENT_3D('',#73216,#22728,#22729);
#18436=AXIS2_PLACEMENT_3D('',#73217,#22730,#22731);
#18437=AXIS2_PLACEMENT_3D('',#73218,#22732,#22733);
#18438=AXIS2_PLACEMENT_3D('',#73219,#22734,#22735);
#18439=AXIS2_PLACEMENT_3D('',#73220,#22736,#22737);
#18440=AXIS2_PLACEMENT_3D('',#73221,#22738,#22739);
#18441=AXIS2_PLACEMENT_3D('',#73222,#22740,#22741);
#18442=AXIS2_PLACEMENT_3D('',#73223,#22742,#22743);
#18443=AXIS2_PLACEMENT_3D('',#73224,#22744,#22745);
#18444=AXIS2_PLACEMENT_3D('',#73225,#22746,#22747);
#18445=AXIS2_PLACEMENT_3D('',#73226,#22748,#22749);
#18446=AXIS2_PLACEMENT_3D('',#73227,#22750,#22751);
#18447=AXIS2_PLACEMENT_3D('',#73228,#22752,#22753);
#18448=AXIS2_PLACEMENT_3D('',#73229,#22754,#22755);
#18449=AXIS2_PLACEMENT_3D('',#73230,#22756,#22757);
#18450=AXIS2_PLACEMENT_3D('',#73231,#22758,#22759);
#18451=AXIS2_PLACEMENT_3D('',#73232,#22760,#22761);
#18452=AXIS2_PLACEMENT_3D('',#73233,#22762,#22763);
#18453=AXIS2_PLACEMENT_3D('',#73234,#22764,#22765);
#18454=AXIS2_PLACEMENT_3D('',#73235,#22766,#22767);
#18455=AXIS2_PLACEMENT_3D('',#73236,#22768,#22769);
#18456=AXIS2_PLACEMENT_3D('',#73237,#22770,#22771);
#18457=AXIS2_PLACEMENT_3D('',#73238,#22772,#22773);
#18458=DIRECTION('axis',(0.,0.,1.));
#18459=DIRECTION('refdir',(1.,0.,0.));
#18460=DIRECTION('axis',(0.,0.,1.));
#18461=DIRECTION('refdir',(1.,0.,0.));
#18462=DIRECTION('axis',(0.,0.,1.));
#18463=DIRECTION('refdir',(1.,0.,0.));
#18464=DIRECTION('center_axis',(0.,0.,1.));
#18465=DIRECTION('ref_axis',(1.,0.,0.));
#18466=DIRECTION('center_axis',(0.,0.,1.));
#18467=DIRECTION('ref_axis',(1.,0.,0.));
#18468=DIRECTION('',(0.,0.,1.));
#18469=DIRECTION('center_axis',(0.,0.,-1.));
#18470=DIRECTION('ref_axis',(1.,0.,0.));
#18471=DIRECTION('center_axis',(0.,0.,1.));
#18472=DIRECTION('ref_axis',(1.,0.,0.));
#18473=DIRECTION('center_axis',(0.,0.,1.));
#18474=DIRECTION('ref_axis',(1.,0.,0.));
#18475=DIRECTION('',(0.,0.,1.));
#18476=DIRECTION('center_axis',(0.,0.,-1.));
#18477=DIRECTION('ref_axis',(1.,0.,0.));
#18478=DIRECTION('center_axis',(0.,0.,1.));
#18479=DIRECTION('ref_axis',(1.,0.,0.));
#18480=DIRECTION('center_axis',(0.,0.,1.));
#18481=DIRECTION('ref_axis',(1.,0.,0.));
#18482=DIRECTION('',(0.,0.,1.));
#18483=DIRECTION('center_axis',(0.,0.,-1.));
#18484=DIRECTION('ref_axis',(1.,0.,0.));
#18485=DIRECTION('center_axis',(0.,0.,1.));
#18486=DIRECTION('ref_axis',(1.,0.,0.));
#18487=DIRECTION('center_axis',(0.,0.,1.));
#18488=DIRECTION('ref_axis',(1.,0.,0.));
#18489=DIRECTION('',(0.,0.,1.));
#18490=DIRECTION('center_axis',(0.,0.,-1.));
#18491=DIRECTION('ref_axis',(1.,0.,0.));
#18492=DIRECTION('center_axis',(0.,1.,0.));
#18493=DIRECTION('ref_axis',(-1.,0.,0.));
#18494=DIRECTION('',(-1.,0.,0.));
#18495=DIRECTION('',(0.,0.,1.));
#18496=DIRECTION('',(-1.,0.,0.));
#18497=DIRECTION('',(0.,0.,1.));
#18498=DIRECTION('center_axis',(1.,0.,0.));
#18499=DIRECTION('ref_axis',(0.,1.,0.));
#18500=DIRECTION('',(0.,1.,0.));
#18501=DIRECTION('',(0.,1.,0.));
#18502=DIRECTION('',(0.,0.,1.));
#18503=DIRECTION('center_axis',(0.,-1.,0.));
#18504=DIRECTION('ref_axis',(1.,0.,0.));
#18505=DIRECTION('',(1.,0.,0.));
#18506=DIRECTION('',(1.,0.,0.));
#18507=DIRECTION('',(0.,0.,1.));
#18508=DIRECTION('center_axis',(-1.,0.,0.));
#18509=DIRECTION('ref_axis',(0.,-1.,0.));
#18510=DIRECTION('',(0.,-1.,0.));
#18511=DIRECTION('',(0.,-1.,0.));
#18512=DIRECTION('center_axis',(0.,0.,1.));
#18513=DIRECTION('ref_axis',(1.,0.,0.));
#18514=DIRECTION('center_axis',(0.,0.,1.));
#18515=DIRECTION('ref_axis',(1.,0.,0.));
#18516=DIRECTION('axis',(0.,0.,1.));
#18517=DIRECTION('refdir',(1.,0.,0.));
#18518=DIRECTION('center_axis',(0.,1.,0.));
#18519=DIRECTION('ref_axis',(1.,0.,0.));
#18520=DIRECTION('center_axis',(0.,1.,0.));
#18521=DIRECTION('ref_axis',(1.,0.,0.));
#18522=DIRECTION('',(0.,1.,0.));
#18523=DIRECTION('center_axis',(0.,-1.,0.));
#18524=DIRECTION('ref_axis',(1.,0.,0.));
#18525=DIRECTION('center_axis',(0.,1.,0.));
#18526=DIRECTION('ref_axis',(1.,0.,0.));
#18527=DIRECTION('center_axis',(0.,1.,0.));
#18528=DIRECTION('ref_axis',(1.,0.,0.));
#18529=DIRECTION('center_axis',(0.,1.,0.));
#18530=DIRECTION('ref_axis',(1.,0.,0.));
#18531=DIRECTION('',(0.,1.,0.));
#18532=DIRECTION('center_axis',(0.,-1.,0.));
#18533=DIRECTION('ref_axis',(1.,0.,0.));
#18534=DIRECTION('center_axis',(0.,1.,0.));
#18535=DIRECTION('ref_axis',(1.,0.,0.));
#18536=DIRECTION('center_axis',(0.,1.,0.));
#18537=DIRECTION('ref_axis',(1.,0.,0.));
#18538=DIRECTION('center_axis',(0.,1.,0.));
#18539=DIRECTION('ref_axis',(1.,0.,0.));
#18540=DIRECTION('',(0.,1.,0.));
#18541=DIRECTION('center_axis',(0.,1.,0.));
#18542=DIRECTION('ref_axis',(1.,0.,0.));
#18543=DIRECTION('center_axis',(0.,1.,0.));
#18544=DIRECTION('ref_axis',(1.,0.,0.));
#18545=DIRECTION('center_axis',(0.,1.,0.));
#18546=DIRECTION('ref_axis',(1.,0.,0.));
#18547=DIRECTION('center_axis',(0.,1.,0.));
#18548=DIRECTION('ref_axis',(1.,0.,0.));
#18549=DIRECTION('',(0.,1.,0.));
#18550=DIRECTION('center_axis',(0.,1.,0.));
#18551=DIRECTION('ref_axis',(1.,0.,0.));
#18552=DIRECTION('center_axis',(0.,1.,0.));
#18553=DIRECTION('ref_axis',(1.,0.,0.));
#18554=DIRECTION('center_axis',(0.,1.,0.));
#18555=DIRECTION('ref_axis',(1.,0.,0.));
#18556=DIRECTION('',(0.,1.,0.));
#18557=DIRECTION('center_axis',(0.,1.,0.));
#18558=DIRECTION('ref_axis',(1.,0.,0.));
#18559=DIRECTION('',(0.,-1.,0.));
#18560=DIRECTION('center_axis',(0.,-1.,0.));
#18561=DIRECTION('ref_axis',(1.,0.,0.));
#18562=DIRECTION('center_axis',(0.,1.,0.));
#18563=DIRECTION('ref_axis',(1.,0.,0.));
#18564=DIRECTION('',(-1.,0.,0.));
#18565=DIRECTION('center_axis',(0.,1.,0.));
#18566=DIRECTION('ref_axis',(1.,0.,0.));
#18567=DIRECTION('',(-1.,0.,0.));
#18568=DIRECTION('center_axis',(0.,1.,0.));
#18569=DIRECTION('ref_axis',(-1.,0.,0.));
#18570=DIRECTION('',(-1.,0.,0.));
#18571=DIRECTION('',(0.,0.,1.));
#18572=DIRECTION('',(-1.,0.,0.));
#18573=DIRECTION('',(0.,0.,1.));
#18574=DIRECTION('',(-1.,0.,0.));
#18575=DIRECTION('',(0.,0.,1.));
#18576=DIRECTION('',(-1.,0.,0.));
#18577=DIRECTION('',(0.,0.,1.));
#18578=DIRECTION('',(-1.,0.,0.));
#18579=DIRECTION('center_axis',(0.,-1.,0.));
#18580=DIRECTION('ref_axis',(1.,0.,0.));
#18581=DIRECTION('',(-1.,0.,0.));
#18582=DIRECTION('center_axis',(0.,-1.,0.));
#18583=DIRECTION('ref_axis',(1.,0.,0.));
#18584=DIRECTION('',(-1.,0.,0.));
#18585=DIRECTION('center_axis',(0.,-1.,0.));
#18586=DIRECTION('ref_axis',(1.,0.,0.));
#18587=DIRECTION('center_axis',(0.,-1.,0.));
#18588=DIRECTION('ref_axis',(1.,0.,0.));
#18589=DIRECTION('center_axis',(0.,-1.,0.));
#18590=DIRECTION('ref_axis',(1.,0.,0.));
#18591=DIRECTION('center_axis',(0.,-1.,0.));
#18592=DIRECTION('ref_axis',(1.,0.,0.));
#18593=DIRECTION('center_axis',(0.,0.,1.));
#18594=DIRECTION('ref_axis',(1.,0.,0.));
#18595=DIRECTION('',(0.,-1.,0.));
#18596=DIRECTION('',(1.,0.,0.));
#18597=DIRECTION('',(0.,-1.,0.));
#18598=DIRECTION('',(-1.,0.,0.));
#18599=DIRECTION('',(0.,-1.,0.));
#18600=DIRECTION('',(1.,0.,0.));
#18601=DIRECTION('',(0.,-1.,0.));
#18602=DIRECTION('',(1.,0.,0.));
#18603=DIRECTION('',(0.,1.,0.));
#18604=DIRECTION('center_axis',(0.,0.,-1.));
#18605=DIRECTION('ref_axis',(1.,0.,0.));
#18606=DIRECTION('center_axis',(0.,0.,-1.));
#18607=DIRECTION('ref_axis',(1.,0.,0.));
#18608=DIRECTION('center_axis',(0.,0.,-1.));
#18609=DIRECTION('ref_axis',(1.,0.,0.));
#18610=DIRECTION('center_axis',(0.,0.,-1.));
#18611=DIRECTION('ref_axis',(1.,0.,0.));
#18612=DIRECTION('center_axis',(0.,0.,-1.));
#18613=DIRECTION('ref_axis',(1.,0.,0.));
#18614=DIRECTION('center_axis',(0.,1.,0.));
#18615=DIRECTION('ref_axis',(1.,0.,0.));
#18616=DIRECTION('center_axis',(0.,1.,0.));
#18617=DIRECTION('ref_axis',(1.,0.,0.));
#18618=DIRECTION('',(0.,1.,0.));
#18619=DIRECTION('center_axis',(0.,1.,0.));
#18620=DIRECTION('ref_axis',(1.,0.,0.));
#18621=DIRECTION('center_axis',(0.,1.,0.));
#18622=DIRECTION('ref_axis',(1.,0.,0.));
#18623=DIRECTION('center_axis',(0.,-1.,0.));
#18624=DIRECTION('ref_axis',(1.,0.,0.));
#18625=DIRECTION('',(1.,0.,0.));
#18626=DIRECTION('center_axis',(0.,-1.,0.));
#18627=DIRECTION('ref_axis',(1.,0.,0.));
#18628=DIRECTION('',(1.,0.,0.));
#18629=DIRECTION('center_axis',(0.,1.,0.));
#18630=DIRECTION('ref_axis',(1.,0.,0.));
#18631=DIRECTION('',(1.,0.,0.));
#18632=DIRECTION('center_axis',(0.,1.,0.));
#18633=DIRECTION('ref_axis',(1.,0.,0.));
#18634=DIRECTION('',(1.,0.,0.));
#18635=DIRECTION('',(0.,0.,1.));
#18636=DIRECTION('',(1.,0.,0.));
#18637=DIRECTION('',(0.,0.,1.));
#18638=DIRECTION('',(1.,0.,0.));
#18639=DIRECTION('',(0.,0.,1.));
#18640=DIRECTION('',(1.,0.,0.));
#18641=DIRECTION('',(0.,0.,1.));
#18642=DIRECTION('center_axis',(0.,1.,0.));
#18643=DIRECTION('ref_axis',(1.,0.,0.));
#18644=DIRECTION('center_axis',(0.,1.,0.));
#18645=DIRECTION('ref_axis',(1.,0.,0.));
#18646=DIRECTION('center_axis',(0.,1.,0.));
#18647=DIRECTION('ref_axis',(1.,0.,0.));
#18648=DIRECTION('center_axis',(0.,1.,0.));
#18649=DIRECTION('ref_axis',(1.,0.,0.));
#18650=DIRECTION('center_axis',(0.,0.,1.));
#18651=DIRECTION('ref_axis',(1.,0.,0.));
#18652=DIRECTION('',(0.,1.,0.));
#18653=DIRECTION('',(-1.,0.,0.));
#18654=DIRECTION('',(0.,-1.,0.));
#18655=DIRECTION('',(1.,0.,0.));
#18656=DIRECTION('',(0.,-1.,0.));
#18657=DIRECTION('center_axis',(0.,1.,0.));
#18658=DIRECTION('ref_axis',(1.,0.,0.));
#18659=DIRECTION('center_axis',(0.,-1.,0.));
#18660=DIRECTION('ref_axis',(1.,0.,0.));
#18661=DIRECTION('center_axis',(0.,1.,0.));
#18662=DIRECTION('ref_axis',(1.,0.,0.));
#18663=DIRECTION('',(0.,1.,0.));
#18664=DIRECTION('center_axis',(0.,1.,0.));
#18665=DIRECTION('ref_axis',(1.,0.,0.));
#18666=DIRECTION('center_axis',(0.,1.,0.));
#18667=DIRECTION('ref_axis',(-1.,0.,0.));
#18668=DIRECTION('',(1.,0.,0.));
#18669=DIRECTION('center_axis',(0.,1.,0.));
#18670=DIRECTION('ref_axis',(1.,0.,0.));
#18671=DIRECTION('',(1.,0.,0.));
#18672=DIRECTION('center_axis',(0.,1.,0.));
#18673=DIRECTION('ref_axis',(1.,0.,0.));
#18674=DIRECTION('',(1.,0.,0.));
#18675=DIRECTION('',(0.,0.,1.));
#18676=DIRECTION('',(-1.,0.,0.));
#18677=DIRECTION('',(0.,0.,1.));
#18678=DIRECTION('center_axis',(0.,0.,1.));
#18679=DIRECTION('ref_axis',(1.,0.,0.));
#18680=DIRECTION('',(0.,-1.,0.));
#18681=DIRECTION('',(-1.,0.,0.));
#18682=DIRECTION('',(0.,-1.,0.));
#18683=DIRECTION('center_axis',(0.,1.,0.));
#18684=DIRECTION('ref_axis',(1.,0.,0.));
#18685=DIRECTION('center_axis',(0.,1.,0.));
#18686=DIRECTION('ref_axis',(1.,0.,0.));
#18687=DIRECTION('',(0.,1.,0.));
#18688=DIRECTION('center_axis',(0.,1.,0.));
#18689=DIRECTION('ref_axis',(1.,0.,0.));
#18690=DIRECTION('center_axis',(0.,1.,0.));
#18691=DIRECTION('ref_axis',(1.,0.,0.));
#18692=DIRECTION('center_axis',(0.,1.,0.));
#18693=DIRECTION('ref_axis',(1.,0.,0.));
#18694=DIRECTION('',(0.,1.,0.));
#18695=DIRECTION('center_axis',(0.,1.,0.));
#18696=DIRECTION('ref_axis',(1.,0.,0.));
#18697=DIRECTION('center_axis',(0.,1.,0.));
#18698=DIRECTION('ref_axis',(1.,0.,0.));
#18699=DIRECTION('',(0.,1.,0.));
#18700=DIRECTION('center_axis',(0.,1.,0.));
#18701=DIRECTION('ref_axis',(1.,0.,0.));
#18702=DIRECTION('center_axis',(0.,1.,0.));
#18703=DIRECTION('ref_axis',(1.,0.,0.));
#18704=DIRECTION('center_axis',(0.,1.,0.));
#18705=DIRECTION('ref_axis',(1.,0.,0.));
#18706=DIRECTION('',(0.,1.,0.));
#18707=DIRECTION('center_axis',(0.,1.,0.));
#18708=DIRECTION('ref_axis',(1.,0.,0.));
#18709=DIRECTION('center_axis',(0.,1.,0.));
#18710=DIRECTION('ref_axis',(1.,0.,0.));
#18711=DIRECTION('center_axis',(0.,1.,0.));
#18712=DIRECTION('ref_axis',(1.,0.,0.));
#18713=DIRECTION('',(0.,1.,0.));
#18714=DIRECTION('center_axis',(0.,1.,0.));
#18715=DIRECTION('ref_axis',(1.,0.,0.));
#18716=DIRECTION('center_axis',(0.,1.,0.));
#18717=DIRECTION('ref_axis',(1.,0.,0.));
#18718=DIRECTION('',(-1.,0.,0.));
#18719=DIRECTION('center_axis',(0.,1.,0.));
#18720=DIRECTION('ref_axis',(1.,0.,0.));
#18721=DIRECTION('center_axis',(0.,1.,0.));
#18722=DIRECTION('ref_axis',(1.,0.,0.));
#18723=DIRECTION('center_axis',(0.,1.,0.));
#18724=DIRECTION('ref_axis',(1.,0.,0.));
#18725=DIRECTION('',(0.,1.,0.));
#18726=DIRECTION('center_axis',(0.,1.,0.));
#18727=DIRECTION('ref_axis',(1.,0.,0.));
#18728=DIRECTION('center_axis',(0.,-1.,0.));
#18729=DIRECTION('ref_axis',(1.,0.,0.));
#18730=DIRECTION('',(1.,0.,0.));
#18731=DIRECTION('center_axis',(0.,0.,1.));
#18732=DIRECTION('ref_axis',(1.,0.,0.));
#18733=DIRECTION('',(0.,1.,0.));
#18734=DIRECTION('',(-1.,0.,0.));
#18735=DIRECTION('',(0.,-1.,0.));
#18736=DIRECTION('',(1.,0.,0.));
#18737=DIRECTION('',(0.,-1.,0.));
#18738=DIRECTION('center_axis',(0.,1.,0.));
#18739=DIRECTION('ref_axis',(1.,0.,0.));
#18740=DIRECTION('',(0.,1.,0.));
#18741=DIRECTION('center_axis',(0.,1.,0.));
#18742=DIRECTION('ref_axis',(1.,0.,0.));
#18743=DIRECTION('center_axis',(0.,-1.,0.));
#18744=DIRECTION('ref_axis',(1.,0.,0.));
#18745=DIRECTION('center_axis',(0.,-1.,0.));
#18746=DIRECTION('ref_axis',(1.,0.,0.));
#18747=DIRECTION('',(0.,0.,1.));
#18748=DIRECTION('',(1.,0.,0.));
#18749=DIRECTION('',(0.,0.,1.));
#18750=DIRECTION('',(-1.,0.,0.));
#18751=DIRECTION('center_axis',(0.,-1.,0.));
#18752=DIRECTION('ref_axis',(1.,0.,0.));
#18753=DIRECTION('center_axis',(0.,0.,1.));
#18754=DIRECTION('ref_axis',(1.,0.,0.));
#18755=DIRECTION('',(0.,-1.,0.));
#18756=DIRECTION('',(-1.,0.,0.));
#18757=DIRECTION('',(0.,-1.,0.));
#18758=DIRECTION('center_axis',(0.,1.,0.));
#18759=DIRECTION('ref_axis',(1.,0.,0.));
#18760=DIRECTION('center_axis',(0.,1.,0.));
#18761=DIRECTION('ref_axis',(1.,0.,0.));
#18762=DIRECTION('',(0.,1.,0.));
#18763=DIRECTION('center_axis',(0.,1.,0.));
#18764=DIRECTION('ref_axis',(1.,0.,0.));
#18765=DIRECTION('center_axis',(0.,1.,0.));
#18766=DIRECTION('ref_axis',(1.,0.,0.));
#18767=DIRECTION('center_axis',(0.,1.,0.));
#18768=DIRECTION('ref_axis',(1.,0.,0.));
#18769=DIRECTION('',(0.,1.,0.));
#18770=DIRECTION('center_axis',(0.,1.,0.));
#18771=DIRECTION('ref_axis',(1.,0.,0.));
#18772=DIRECTION('center_axis',(0.,1.,0.));
#18773=DIRECTION('ref_axis',(1.,0.,0.));
#18774=DIRECTION('',(0.,1.,0.));
#18775=DIRECTION('center_axis',(0.,1.,0.));
#18776=DIRECTION('ref_axis',(1.,0.,0.));
#18777=DIRECTION('center_axis',(0.,1.,0.));
#18778=DIRECTION('ref_axis',(1.,0.,0.));
#18779=DIRECTION('center_axis',(0.,1.,0.));
#18780=DIRECTION('ref_axis',(1.,0.,0.));
#18781=DIRECTION('',(0.,1.,0.));
#18782=DIRECTION('center_axis',(0.,1.,0.));
#18783=DIRECTION('ref_axis',(1.,0.,0.));
#18784=DIRECTION('center_axis',(0.,1.,0.));
#18785=DIRECTION('ref_axis',(1.,0.,0.));
#18786=DIRECTION('center_axis',(0.,1.,0.));
#18787=DIRECTION('ref_axis',(1.,0.,0.));
#18788=DIRECTION('',(0.,1.,0.));
#18789=DIRECTION('center_axis',(0.,1.,0.));
#18790=DIRECTION('ref_axis',(1.,0.,0.));
#18791=DIRECTION('center_axis',(0.,1.,0.));
#18792=DIRECTION('ref_axis',(1.,0.,0.));
#18793=DIRECTION('',(-1.,0.,0.));
#18794=DIRECTION('center_axis',(0.,1.,0.));
#18795=DIRECTION('ref_axis',(1.,0.,0.));
#18796=DIRECTION('center_axis',(0.,0.,1.));
#18797=DIRECTION('ref_axis',(1.,0.,0.));
#18798=DIRECTION('',(0.,-1.,0.));
#18799=DIRECTION('',(0.,1.,0.));
#18800=DIRECTION('',(1.,0.,0.));
#18801=DIRECTION('',(0.,1.,0.));
#18802=DIRECTION('',(0.,1.,0.));
#18803=DIRECTION('',(0.,1.,0.));
#18804=DIRECTION('center_axis',(0.,0.,-1.));
#18805=DIRECTION('ref_axis',(1.,0.,0.));
#18806=DIRECTION('center_axis',(0.,0.,-1.));
#18807=DIRECTION('ref_axis',(1.,0.,0.));
#18808=DIRECTION('center_axis',(0.,0.,-1.));
#18809=DIRECTION('ref_axis',(1.,0.,0.));
#18810=DIRECTION('center_axis',(0.,0.,-1.));
#18811=DIRECTION('ref_axis',(1.,0.,0.));
#18812=DIRECTION('center_axis',(0.,0.,-1.));
#18813=DIRECTION('ref_axis',(1.,0.,0.));
#18814=DIRECTION('center_axis',(0.,1.,0.));
#18815=DIRECTION('ref_axis',(1.,0.,0.));
#18816=DIRECTION('center_axis',(0.,1.,0.));
#18817=DIRECTION('ref_axis',(1.,0.,0.));
#18818=DIRECTION('center_axis',(0.,1.,0.));
#18819=DIRECTION('ref_axis',(1.,0.,0.));
#18820=DIRECTION('center_axis',(0.,-1.,0.));
#18821=DIRECTION('ref_axis',(1.,0.,0.));
#18822=DIRECTION('center_axis',(0.,1.,0.));
#18823=DIRECTION('ref_axis',(1.,0.,0.));
#18824=DIRECTION('center_axis',(0.,1.,0.));
#18825=DIRECTION('ref_axis',(1.,0.,0.));
#18826=DIRECTION('center_axis',(0.,0.,1.));
#18827=DIRECTION('ref_axis',(1.,0.,0.));
#18828=DIRECTION('center_axis',(0.,0.,1.));
#18829=DIRECTION('ref_axis',(1.,0.,0.));
#18830=DIRECTION('',(0.,0.,1.));
#18831=DIRECTION('center_axis',(0.,0.,-1.));
#18832=DIRECTION('ref_axis',(1.,0.,0.));
#18833=DIRECTION('center_axis',(0.,0.,1.));
#18834=DIRECTION('ref_axis',(1.,0.,0.));
#18835=DIRECTION('center_axis',(0.,0.,1.));
#18836=DIRECTION('ref_axis',(1.,0.,0.));
#18837=DIRECTION('center_axis',(0.,0.,1.));
#18838=DIRECTION('ref_axis',(1.,0.,0.));
#18839=DIRECTION('center_axis',(0.,0.,1.));
#18840=DIRECTION('ref_axis',(1.,0.,0.));
#18841=DIRECTION('',(0.,0.,1.));
#18842=DIRECTION('center_axis',(0.,0.,-1.));
#18843=DIRECTION('ref_axis',(1.,0.,0.));
#18844=DIRECTION('center_axis',(0.,0.,1.));
#18845=DIRECTION('ref_axis',(1.,0.,0.));
#18846=DIRECTION('center_axis',(0.,0.,1.));
#18847=DIRECTION('ref_axis',(1.,0.,0.));
#18848=DIRECTION('center_axis',(0.,0.,1.));
#18849=DIRECTION('ref_axis',(1.,0.,0.));
#18850=DIRECTION('center_axis',(0.,0.,1.));
#18851=DIRECTION('ref_axis',(1.,0.,0.));
#18852=DIRECTION('',(0.,0.,1.));
#18853=DIRECTION('center_axis',(0.,0.,-1.));
#18854=DIRECTION('ref_axis',(1.,0.,0.));
#18855=DIRECTION('center_axis',(0.,0.,1.));
#18856=DIRECTION('ref_axis',(1.,0.,0.));
#18857=DIRECTION('center_axis',(0.,0.,1.));
#18858=DIRECTION('ref_axis',(1.,0.,0.));
#18859=DIRECTION('center_axis',(0.,0.,1.));
#18860=DIRECTION('ref_axis',(1.,0.,0.));
#18861=DIRECTION('center_axis',(0.,0.,1.));
#18862=DIRECTION('ref_axis',(1.,0.,0.));
#18863=DIRECTION('',(0.,0.,1.));
#18864=DIRECTION('center_axis',(0.,0.,-1.));
#18865=DIRECTION('ref_axis',(1.,0.,0.));
#18866=DIRECTION('center_axis',(0.,0.,1.));
#18867=DIRECTION('ref_axis',(1.,0.,0.));
#18868=DIRECTION('center_axis',(0.,0.,1.));
#18869=DIRECTION('ref_axis',(1.,0.,0.));
#18870=DIRECTION('center_axis',(0.,0.,1.));
#18871=DIRECTION('ref_axis',(1.,0.,0.));
#18872=DIRECTION('center_axis',(0.,0.,1.));
#18873=DIRECTION('ref_axis',(1.,0.,0.));
#18874=DIRECTION('',(0.,0.,1.));
#18875=DIRECTION('center_axis',(0.,0.,1.));
#18876=DIRECTION('ref_axis',(1.,0.,0.));
#18877=DIRECTION('center_axis',(0.,0.,1.));
#18878=DIRECTION('ref_axis',(1.,0.,0.));
#18879=DIRECTION('',(0.,0.,1.));
#18880=DIRECTION('center_axis',(0.,0.,1.));
#18881=DIRECTION('ref_axis',(1.,0.,0.));
#18882=DIRECTION('center_axis',(0.,0.,1.));
#18883=DIRECTION('ref_axis',(1.,0.,0.));
#18884=DIRECTION('',(0.,0.,1.));
#18885=DIRECTION('center_axis',(0.,0.,1.));
#18886=DIRECTION('ref_axis',(1.,0.,0.));
#18887=DIRECTION('center_axis',(0.,0.,1.));
#18888=DIRECTION('ref_axis',(1.,0.,0.));
#18889=DIRECTION('',(0.,0.,1.));
#18890=DIRECTION('center_axis',(0.,0.,1.));
#18891=DIRECTION('ref_axis',(1.,0.,0.));
#18892=DIRECTION('center_axis',(0.,0.,1.));
#18893=DIRECTION('ref_axis',(1.,0.,0.));
#18894=DIRECTION('',(0.,0.,1.));
#18895=DIRECTION('center_axis',(0.,0.,1.));
#18896=DIRECTION('ref_axis',(1.,0.,0.));
#18897=DIRECTION('center_axis',(0.,0.,1.));
#18898=DIRECTION('ref_axis',(1.,0.,0.));
#18899=DIRECTION('center_axis',(0.,0.,1.));
#18900=DIRECTION('ref_axis',(1.,0.,0.));
#18901=DIRECTION('',(0.,0.,1.));
#18902=DIRECTION('center_axis',(0.,0.,1.));
#18903=DIRECTION('ref_axis',(1.,0.,0.));
#18904=DIRECTION('center_axis',(0.,0.,1.));
#18905=DIRECTION('ref_axis',(1.,0.,0.));
#18906=DIRECTION('center_axis',(0.,0.,1.));
#18907=DIRECTION('ref_axis',(1.,0.,0.));
#18908=DIRECTION('',(0.,0.,1.));
#18909=DIRECTION('center_axis',(0.,0.,1.));
#18910=DIRECTION('ref_axis',(1.,0.,0.));
#18911=DIRECTION('center_axis',(0.,0.,1.));
#18912=DIRECTION('ref_axis',(1.,0.,0.));
#18913=DIRECTION('center_axis',(0.,0.,1.));
#18914=DIRECTION('ref_axis',(1.,0.,0.));
#18915=DIRECTION('',(0.,0.,1.));
#18916=DIRECTION('center_axis',(0.,0.,1.));
#18917=DIRECTION('ref_axis',(1.,0.,0.));
#18918=DIRECTION('center_axis',(0.,0.,1.));
#18919=DIRECTION('ref_axis',(1.,0.,0.));
#18920=DIRECTION('center_axis',(0.,0.,1.));
#18921=DIRECTION('ref_axis',(1.,0.,0.));
#18922=DIRECTION('',(0.,0.,1.));
#18923=DIRECTION('center_axis',(0.,0.,1.));
#18924=DIRECTION('ref_axis',(1.,0.,0.));
#18925=DIRECTION('center_axis',(0.,0.,1.));
#18926=DIRECTION('ref_axis',(1.,0.,0.));
#18927=DIRECTION('',(0.,0.,1.));
#18928=DIRECTION('center_axis',(0.,0.,1.));
#18929=DIRECTION('ref_axis',(1.,0.,0.));
#18930=DIRECTION('center_axis',(0.,0.,1.));
#18931=DIRECTION('ref_axis',(1.,0.,0.));
#18932=DIRECTION('',(0.,0.,1.));
#18933=DIRECTION('center_axis',(0.,0.,1.));
#18934=DIRECTION('ref_axis',(1.,0.,0.));
#18935=DIRECTION('center_axis',(0.,0.,1.));
#18936=DIRECTION('ref_axis',(1.,0.,0.));
#18937=DIRECTION('',(0.,0.,1.));
#18938=DIRECTION('center_axis',(0.,0.,1.));
#18939=DIRECTION('ref_axis',(1.,0.,0.));
#18940=DIRECTION('center_axis',(0.,0.,1.));
#18941=DIRECTION('ref_axis',(1.,0.,0.));
#18942=DIRECTION('',(0.,0.,1.));
#18943=DIRECTION('center_axis',(0.,0.,1.));
#18944=DIRECTION('ref_axis',(1.,0.,0.));
#18945=DIRECTION('center_axis',(0.,0.,1.));
#18946=DIRECTION('ref_axis',(1.,0.,0.));
#18947=DIRECTION('',(0.,0.,1.));
#18948=DIRECTION('center_axis',(1.,0.,0.));
#18949=DIRECTION('ref_axis',(0.,1.,0.));
#18950=DIRECTION('',(0.,1.,0.));
#18951=DIRECTION('center_axis',(0.,0.,1.));
#18952=DIRECTION('ref_axis',(1.,0.,0.));
#18953=DIRECTION('',(0.,-1.,0.));
#18954=DIRECTION('center_axis',(1.,0.,0.));
#18955=DIRECTION('ref_axis',(0.,1.,0.));
#18956=DIRECTION('',(0.,1.,0.));
#18957=DIRECTION('center_axis',(-1.,0.,0.));
#18958=DIRECTION('ref_axis',(0.,-1.,0.));
#18959=DIRECTION('',(0.,-1.,0.));
#18960=DIRECTION('center_axis',(0.,0.,1.));
#18961=DIRECTION('ref_axis',(1.,0.,0.));
#18962=DIRECTION('',(0.,1.,0.));
#18963=DIRECTION('center_axis',(-1.,0.,0.));
#18964=DIRECTION('ref_axis',(0.,-1.,0.));
#18965=DIRECTION('',(0.,-1.,0.));
#18966=DIRECTION('center_axis',(1.,0.,0.));
#18967=DIRECTION('ref_axis',(0.,1.,0.));
#18968=DIRECTION('',(0.,1.,0.));
#18969=DIRECTION('center_axis',(0.,0.,1.));
#18970=DIRECTION('ref_axis',(1.,0.,0.));
#18971=DIRECTION('center_axis',(-1.,0.,0.));
#18972=DIRECTION('ref_axis',(0.,-1.,0.));
#18973=DIRECTION('',(0.,-1.,0.));
#18974=DIRECTION('center_axis',(0.,0.,1.));
#18975=DIRECTION('ref_axis',(1.,0.,0.));
#18976=DIRECTION('axis',(0.,0.,1.));
#18977=DIRECTION('refdir',(1.,0.,0.));
#18978=DIRECTION('center_axis',(0.,0.,1.));
#18979=DIRECTION('ref_axis',(1.,0.,0.));
#18980=DIRECTION('center_axis',(0.,0.,1.));
#18981=DIRECTION('ref_axis',(1.,0.,0.));
#18982=DIRECTION('',(0.,0.,1.));
#18983=DIRECTION('center_axis',(0.,0.,-1.));
#18984=DIRECTION('ref_axis',(1.,0.,0.));
#18985=DIRECTION('center_axis',(0.,0.,1.));
#18986=DIRECTION('ref_axis',(1.,0.,0.));
#18987=DIRECTION('center_axis',(0.,0.,1.));
#18988=DIRECTION('ref_axis',(1.,0.,0.));
#18989=DIRECTION('',(0.,0.,1.));
#18990=DIRECTION('center_axis',(0.,0.,-1.));
#18991=DIRECTION('ref_axis',(1.,0.,0.));
#18992=DIRECTION('center_axis',(0.,0.,1.));
#18993=DIRECTION('ref_axis',(1.,0.,0.));
#18994=DIRECTION('center_axis',(0.,0.,1.));
#18995=DIRECTION('ref_axis',(1.,0.,0.));
#18996=DIRECTION('',(0.,0.,1.));
#18997=DIRECTION('center_axis',(0.,0.,-1.));
#18998=DIRECTION('ref_axis',(1.,0.,0.));
#18999=DIRECTION('center_axis',(0.,0.,1.));
#19000=DIRECTION('ref_axis',(1.,0.,0.));
#19001=DIRECTION('center_axis',(0.,0.,1.));
#19002=DIRECTION('ref_axis',(1.,0.,0.));
#19003=DIRECTION('',(0.,0.,1.));
#19004=DIRECTION('center_axis',(0.,0.,-1.));
#19005=DIRECTION('ref_axis',(1.,0.,0.));
#19006=DIRECTION('center_axis',(0.,-1.,0.));
#19007=DIRECTION('ref_axis',(1.,0.,0.));
#19008=DIRECTION('',(1.,0.,0.));
#19009=DIRECTION('',(0.,0.,1.));
#19010=DIRECTION('',(-1.,0.,0.));
#19011=DIRECTION('',(0.,0.,1.));
#19012=DIRECTION('center_axis',(1.,0.,0.));
#19013=DIRECTION('ref_axis',(0.,1.,0.));
#19014=DIRECTION('',(0.,1.,0.));
#19015=DIRECTION('',(0.,-1.,0.));
#19016=DIRECTION('',(0.,0.,1.));
#19017=DIRECTION('center_axis',(0.,1.,0.));
#19018=DIRECTION('ref_axis',(-1.,0.,0.));
#19019=DIRECTION('',(-1.,0.,0.));
#19020=DIRECTION('',(1.,0.,0.));
#19021=DIRECTION('',(0.,0.,1.));
#19022=DIRECTION('center_axis',(-1.,0.,0.));
#19023=DIRECTION('ref_axis',(0.,-1.,0.));
#19024=DIRECTION('',(0.,-1.,0.));
#19025=DIRECTION('',(0.,1.,0.));
#19026=DIRECTION('center_axis',(0.,1.,0.));
#19027=DIRECTION('ref_axis',(1.,0.,0.));
#19028=DIRECTION('center_axis',(0.,1.,0.));
#19029=DIRECTION('ref_axis',(1.,0.,0.));
#19030=DIRECTION('',(0.,1.,0.));
#19031=DIRECTION('center_axis',(0.,-1.,0.));
#19032=DIRECTION('ref_axis',(1.,0.,0.));
#19033=DIRECTION('center_axis',(0.,1.,0.));
#19034=DIRECTION('ref_axis',(1.,0.,0.));
#19035=DIRECTION('center_axis',(0.,1.,0.));
#19036=DIRECTION('ref_axis',(1.,0.,0.));
#19037=DIRECTION('center_axis',(0.,1.,0.));
#19038=DIRECTION('ref_axis',(1.,0.,0.));
#19039=DIRECTION('',(0.,1.,0.));
#19040=DIRECTION('center_axis',(0.,-1.,0.));
#19041=DIRECTION('ref_axis',(1.,0.,0.));
#19042=DIRECTION('center_axis',(0.,1.,0.));
#19043=DIRECTION('ref_axis',(1.,0.,0.));
#19044=DIRECTION('center_axis',(0.,1.,0.));
#19045=DIRECTION('ref_axis',(1.,0.,0.));
#19046=DIRECTION('center_axis',(0.,1.,0.));
#19047=DIRECTION('ref_axis',(1.,0.,0.));
#19048=DIRECTION('',(0.,1.,0.));
#19049=DIRECTION('center_axis',(0.,1.,0.));
#19050=DIRECTION('ref_axis',(1.,0.,0.));
#19051=DIRECTION('center_axis',(0.,1.,0.));
#19052=DIRECTION('ref_axis',(1.,0.,0.));
#19053=DIRECTION('center_axis',(0.,1.,0.));
#19054=DIRECTION('ref_axis',(1.,0.,0.));
#19055=DIRECTION('center_axis',(0.,1.,0.));
#19056=DIRECTION('ref_axis',(1.,0.,0.));
#19057=DIRECTION('',(0.,1.,0.));
#19058=DIRECTION('center_axis',(0.,1.,0.));
#19059=DIRECTION('ref_axis',(1.,0.,0.));
#19060=DIRECTION('center_axis',(0.,1.,0.));
#19061=DIRECTION('ref_axis',(1.,0.,0.));
#19062=DIRECTION('center_axis',(0.,1.,0.));
#19063=DIRECTION('ref_axis',(1.,0.,0.));
#19064=DIRECTION('',(1.,0.,0.));
#19065=DIRECTION('center_axis',(0.,1.,0.));
#19066=DIRECTION('ref_axis',(1.,0.,0.));
#19067=DIRECTION('',(1.,0.,0.));
#19068=DIRECTION('center_axis',(0.,1.,0.));
#19069=DIRECTION('ref_axis',(1.,0.,0.));
#19070=DIRECTION('center_axis',(0.,1.,0.));
#19071=DIRECTION('ref_axis',(1.,0.,0.));
#19072=DIRECTION('',(0.,-1.,0.));
#19073=DIRECTION('center_axis',(0.,-1.,0.));
#19074=DIRECTION('ref_axis',(1.,0.,0.));
#19075=DIRECTION('',(0.,1.,0.));
#19076=DIRECTION('center_axis',(0.,1.,0.));
#19077=DIRECTION('ref_axis',(1.,0.,0.));
#19078=DIRECTION('',(0.,1.,0.));
#19079=DIRECTION('center_axis',(0.,1.,0.));
#19080=DIRECTION('ref_axis',(1.,0.,0.));
#19081=DIRECTION('',(0.,-1.,0.));
#19082=DIRECTION('center_axis',(0.,0.,1.));
#19083=DIRECTION('ref_axis',(1.,0.,0.));
#19084=DIRECTION('',(-1.,0.,0.));
#19085=DIRECTION('',(0.,1.,0.));
#19086=DIRECTION('',(1.,0.,0.));
#19087=DIRECTION('',(0.,1.,0.));
#19088=DIRECTION('',(-1.,0.,0.));
#19089=DIRECTION('',(0.,1.,0.));
#19090=DIRECTION('',(1.,0.,0.));
#19091=DIRECTION('',(0.,1.,0.));
#19092=DIRECTION('',(-1.,0.,0.));
#19093=DIRECTION('center_axis',(0.,0.,1.));
#19094=DIRECTION('ref_axis',(1.,0.,0.));
#19095=DIRECTION('center_axis',(0.,0.,1.));
#19096=DIRECTION('ref_axis',(1.,0.,0.));
#19097=DIRECTION('center_axis',(0.,0.,1.));
#19098=DIRECTION('ref_axis',(1.,0.,0.));
#19099=DIRECTION('center_axis',(0.,0.,1.));
#19100=DIRECTION('ref_axis',(1.,0.,0.));
#19101=DIRECTION('center_axis',(0.,0.,1.));
#19102=DIRECTION('ref_axis',(1.,0.,0.));
#19103=DIRECTION('center_axis',(0.,1.,0.));
#19104=DIRECTION('ref_axis',(1.,0.,0.));
#19105=DIRECTION('',(0.,-1.,0.));
#19106=DIRECTION('center_axis',(0.,1.,0.));
#19107=DIRECTION('ref_axis',(1.,0.,0.));
#19108=DIRECTION('center_axis',(0.,1.,0.));
#19109=DIRECTION('ref_axis',(1.,0.,0.));
#19110=DIRECTION('center_axis',(0.,1.,0.));
#19111=DIRECTION('ref_axis',(1.,0.,0.));
#19112=DIRECTION('',(-1.,0.,0.));
#19113=DIRECTION('center_axis',(0.,-1.,0.));
#19114=DIRECTION('ref_axis',(1.,0.,0.));
#19115=DIRECTION('center_axis',(0.,-1.,0.));
#19116=DIRECTION('ref_axis',(1.,0.,0.));
#19117=DIRECTION('',(0.,0.,1.));
#19118=DIRECTION('',(1.,0.,0.));
#19119=DIRECTION('',(0.,0.,1.));
#19120=DIRECTION('',(1.,0.,0.));
#19121=DIRECTION('',(0.,0.,1.));
#19122=DIRECTION('',(1.,0.,0.));
#19123=DIRECTION('',(0.,0.,1.));
#19124=DIRECTION('',(1.,0.,0.));
#19125=DIRECTION('center_axis',(0.,1.,0.));
#19126=DIRECTION('ref_axis',(1.,0.,0.));
#19127=DIRECTION('',(1.,0.,0.));
#19128=DIRECTION('center_axis',(0.,1.,0.));
#19129=DIRECTION('ref_axis',(1.,0.,0.));
#19130=DIRECTION('',(1.,0.,0.));
#19131=DIRECTION('center_axis',(0.,1.,0.));
#19132=DIRECTION('ref_axis',(1.,0.,0.));
#19133=DIRECTION('center_axis',(0.,1.,0.));
#19134=DIRECTION('ref_axis',(1.,0.,0.));
#19135=DIRECTION('center_axis',(0.,1.,0.));
#19136=DIRECTION('ref_axis',(1.,0.,0.));
#19137=DIRECTION('center_axis',(0.,1.,0.));
#19138=DIRECTION('ref_axis',(1.,0.,0.));
#19139=DIRECTION('center_axis',(0.,1.,0.));
#19140=DIRECTION('ref_axis',(1.,0.,0.));
#19141=DIRECTION('',(0.,-1.,0.));
#19142=DIRECTION('center_axis',(0.,-1.,0.));
#19143=DIRECTION('ref_axis',(1.,0.,0.));
#19144=DIRECTION('center_axis',(0.,1.,0.));
#19145=DIRECTION('ref_axis',(-1.,0.,0.));
#19146=DIRECTION('',(-1.,0.,0.));
#19147=DIRECTION('center_axis',(0.,-1.,0.));
#19148=DIRECTION('ref_axis',(1.,0.,0.));
#19149=DIRECTION('',(-1.,0.,0.));
#19150=DIRECTION('center_axis',(0.,-1.,0.));
#19151=DIRECTION('ref_axis',(1.,0.,0.));
#19152=DIRECTION('',(-1.,0.,0.));
#19153=DIRECTION('',(0.,0.,1.));
#19154=DIRECTION('',(-1.,0.,0.));
#19155=DIRECTION('',(0.,0.,1.));
#19156=DIRECTION('',(-1.,0.,0.));
#19157=DIRECTION('',(0.,0.,1.));
#19158=DIRECTION('',(-1.,0.,0.));
#19159=DIRECTION('',(0.,0.,1.));
#19160=DIRECTION('center_axis',(0.,-1.,0.));
#19161=DIRECTION('ref_axis',(1.,0.,0.));
#19162=DIRECTION('center_axis',(0.,-1.,0.));
#19163=DIRECTION('ref_axis',(1.,0.,0.));
#19164=DIRECTION('center_axis',(0.,-1.,0.));
#19165=DIRECTION('ref_axis',(1.,0.,0.));
#19166=DIRECTION('center_axis',(0.,-1.,0.));
#19167=DIRECTION('ref_axis',(1.,0.,0.));
#19168=DIRECTION('center_axis',(0.,-1.,0.));
#19169=DIRECTION('ref_axis',(1.,0.,0.));
#19170=DIRECTION('',(1.,0.,0.));
#19171=DIRECTION('center_axis',(0.,-1.,0.));
#19172=DIRECTION('ref_axis',(1.,0.,0.));
#19173=DIRECTION('',(1.,0.,0.));
#19174=DIRECTION('center_axis',(0.,-1.,0.));
#19175=DIRECTION('ref_axis',(1.,0.,0.));
#19176=DIRECTION('',(1.,0.,0.));
#19177=DIRECTION('',(0.,0.,1.));
#19178=DIRECTION('',(1.,0.,0.));
#19179=DIRECTION('',(0.,0.,1.));
#19180=DIRECTION('center_axis',(0.,0.,1.));
#19181=DIRECTION('ref_axis',(1.,0.,0.));
#19182=DIRECTION('',(0.,1.,0.));
#19183=DIRECTION('',(-1.,0.,0.));
#19184=DIRECTION('',(0.,1.,0.));
#19185=DIRECTION('center_axis',(0.,0.,1.));
#19186=DIRECTION('ref_axis',(1.,0.,0.));
#19187=DIRECTION('',(-1.,0.,0.));
#19188=DIRECTION('',(0.,1.,0.));
#19189=DIRECTION('',(1.,0.,0.));
#19190=DIRECTION('',(0.,1.,0.));
#19191=DIRECTION('center_axis',(0.,1.,0.));
#19192=DIRECTION('ref_axis',(1.,0.,0.));
#19193=DIRECTION('center_axis',(0.,1.,0.));
#19194=DIRECTION('ref_axis',(1.,0.,0.));
#19195=DIRECTION('',(0.,1.,0.));
#19196=DIRECTION('center_axis',(0.,1.,0.));
#19197=DIRECTION('ref_axis',(1.,0.,0.));
#19198=DIRECTION('center_axis',(0.,1.,0.));
#19199=DIRECTION('ref_axis',(1.,0.,0.));
#19200=DIRECTION('center_axis',(0.,1.,0.));
#19201=DIRECTION('ref_axis',(1.,0.,0.));
#19202=DIRECTION('',(0.,1.,0.));
#19203=DIRECTION('center_axis',(0.,1.,0.));
#19204=DIRECTION('ref_axis',(1.,0.,0.));
#19205=DIRECTION('center_axis',(0.,1.,0.));
#19206=DIRECTION('ref_axis',(1.,0.,0.));
#19207=DIRECTION('',(0.,1.,0.));
#19208=DIRECTION('center_axis',(0.,1.,0.));
#19209=DIRECTION('ref_axis',(1.,0.,0.));
#19210=DIRECTION('center_axis',(0.,1.,0.));
#19211=DIRECTION('ref_axis',(1.,0.,0.));
#19212=DIRECTION('center_axis',(0.,1.,0.));
#19213=DIRECTION('ref_axis',(1.,0.,0.));
#19214=DIRECTION('',(0.,1.,0.));
#19215=DIRECTION('center_axis',(0.,1.,0.));
#19216=DIRECTION('ref_axis',(1.,0.,0.));
#19217=DIRECTION('center_axis',(0.,1.,0.));
#19218=DIRECTION('ref_axis',(1.,0.,0.));
#19219=DIRECTION('center_axis',(0.,1.,0.));
#19220=DIRECTION('ref_axis',(1.,0.,0.));
#19221=DIRECTION('',(1.,0.,0.));
#19222=DIRECTION('center_axis',(0.,1.,0.));
#19223=DIRECTION('ref_axis',(1.,0.,0.));
#19224=DIRECTION('center_axis',(0.,1.,0.));
#19225=DIRECTION('ref_axis',(1.,0.,0.));
#19226=DIRECTION('center_axis',(0.,1.,0.));
#19227=DIRECTION('ref_axis',(1.,0.,0.));
#19228=DIRECTION('',(0.,-1.,0.));
#19229=DIRECTION('center_axis',(0.,1.,0.));
#19230=DIRECTION('ref_axis',(1.,0.,0.));
#19231=DIRECTION('center_axis',(0.,1.,0.));
#19232=DIRECTION('ref_axis',(1.,0.,0.));
#19233=DIRECTION('',(0.,-1.,0.));
#19234=DIRECTION('center_axis',(0.,1.,0.));
#19235=DIRECTION('ref_axis',(1.,0.,0.));
#19236=DIRECTION('',(0.,-1.,0.));
#19237=DIRECTION('center_axis',(0.,1.,0.));
#19238=DIRECTION('ref_axis',(1.,0.,0.));
#19239=DIRECTION('center_axis',(0.,1.,0.));
#19240=DIRECTION('ref_axis',(1.,0.,0.));
#19241=DIRECTION('',(-1.,0.,0.));
#19242=DIRECTION('center_axis',(0.,-1.,0.));
#19243=DIRECTION('ref_axis',(1.,0.,0.));
#19244=DIRECTION('center_axis',(0.,1.,0.));
#19245=DIRECTION('ref_axis',(1.,0.,0.));
#19246=DIRECTION('',(0.,-1.,0.));
#19247=DIRECTION('center_axis',(0.,0.,1.));
#19248=DIRECTION('ref_axis',(1.,0.,0.));
#19249=DIRECTION('',(0.,1.,0.));
#19250=DIRECTION('',(-1.,0.,0.));
#19251=DIRECTION('',(0.,1.,0.));
#19252=DIRECTION('center_axis',(0.,0.,1.));
#19253=DIRECTION('ref_axis',(1.,0.,0.));
#19254=DIRECTION('',(-1.,0.,0.));
#19255=DIRECTION('',(0.,1.,0.));
#19256=DIRECTION('',(1.,0.,0.));
#19257=DIRECTION('',(0.,1.,0.));
#19258=DIRECTION('center_axis',(0.,1.,0.));
#19259=DIRECTION('ref_axis',(1.,0.,0.));
#19260=DIRECTION('center_axis',(0.,1.,0.));
#19261=DIRECTION('ref_axis',(1.,0.,0.));
#19262=DIRECTION('',(0.,1.,0.));
#19263=DIRECTION('center_axis',(0.,1.,0.));
#19264=DIRECTION('ref_axis',(1.,0.,0.));
#19265=DIRECTION('center_axis',(0.,1.,0.));
#19266=DIRECTION('ref_axis',(1.,0.,0.));
#19267=DIRECTION('center_axis',(0.,1.,0.));
#19268=DIRECTION('ref_axis',(1.,0.,0.));
#19269=DIRECTION('',(0.,1.,0.));
#19270=DIRECTION('center_axis',(0.,1.,0.));
#19271=DIRECTION('ref_axis',(1.,0.,0.));
#19272=DIRECTION('center_axis',(0.,1.,0.));
#19273=DIRECTION('ref_axis',(1.,0.,0.));
#19274=DIRECTION('',(0.,1.,0.));
#19275=DIRECTION('center_axis',(0.,1.,0.));
#19276=DIRECTION('ref_axis',(1.,0.,0.));
#19277=DIRECTION('center_axis',(0.,1.,0.));
#19278=DIRECTION('ref_axis',(1.,0.,0.));
#19279=DIRECTION('center_axis',(0.,1.,0.));
#19280=DIRECTION('ref_axis',(1.,0.,0.));
#19281=DIRECTION('',(0.,1.,0.));
#19282=DIRECTION('center_axis',(0.,1.,0.));
#19283=DIRECTION('ref_axis',(1.,0.,0.));
#19284=DIRECTION('center_axis',(0.,1.,0.));
#19285=DIRECTION('ref_axis',(1.,0.,0.));
#19286=DIRECTION('center_axis',(0.,1.,0.));
#19287=DIRECTION('ref_axis',(1.,0.,0.));
#19288=DIRECTION('center_axis',(0.,1.,0.));
#19289=DIRECTION('ref_axis',(1.,0.,0.));
#19290=DIRECTION('',(0.,-1.,0.));
#19291=DIRECTION('center_axis',(0.,1.,0.));
#19292=DIRECTION('ref_axis',(1.,0.,0.));
#19293=DIRECTION('center_axis',(0.,1.,0.));
#19294=DIRECTION('ref_axis',(1.,0.,0.));
#19295=DIRECTION('',(1.,0.,0.));
#19296=DIRECTION('center_axis',(0.,1.,0.));
#19297=DIRECTION('ref_axis',(1.,0.,0.));
#19298=DIRECTION('',(0.,-1.,0.));
#19299=DIRECTION('center_axis',(0.,1.,0.));
#19300=DIRECTION('ref_axis',(1.,0.,0.));
#19301=DIRECTION('center_axis',(0.,1.,0.));
#19302=DIRECTION('ref_axis',(1.,0.,0.));
#19303=DIRECTION('',(-1.,0.,0.));
#19304=DIRECTION('center_axis',(0.,-1.,0.));
#19305=DIRECTION('ref_axis',(1.,0.,0.));
#19306=DIRECTION('center_axis',(0.,1.,0.));
#19307=DIRECTION('ref_axis',(1.,0.,0.));
#19308=DIRECTION('',(0.,-1.,0.));
#19309=DIRECTION('center_axis',(0.,1.,0.));
#19310=DIRECTION('ref_axis',(1.,0.,0.));
#19311=DIRECTION('center_axis',(0.,1.,0.));
#19312=DIRECTION('ref_axis',(1.,0.,0.));
#19313=DIRECTION('',(0.,-1.,0.));
#19314=DIRECTION('center_axis',(0.,1.,0.));
#19315=DIRECTION('ref_axis',(-1.,0.,0.));
#19316=DIRECTION('',(0.,0.,1.));
#19317=DIRECTION('',(-1.,0.,0.));
#19318=DIRECTION('',(0.,0.,1.));
#19319=DIRECTION('',(-1.,0.,0.));
#19320=DIRECTION('center_axis',(0.,0.,1.));
#19321=DIRECTION('ref_axis',(1.,0.,0.));
#19322=DIRECTION('',(0.,-1.,0.));
#19323=DIRECTION('',(0.,-1.,0.));
#19324=DIRECTION('center_axis',(0.,0.,1.));
#19325=DIRECTION('ref_axis',(1.,0.,0.));
#19326=DIRECTION('center_axis',(0.,0.,1.));
#19327=DIRECTION('ref_axis',(1.,0.,0.));
#19328=DIRECTION('center_axis',(0.,0.,1.));
#19329=DIRECTION('ref_axis',(1.,0.,0.));
#19330=DIRECTION('center_axis',(0.,0.,1.));
#19331=DIRECTION('ref_axis',(1.,0.,0.));
#19332=DIRECTION('center_axis',(0.,0.,1.));
#19333=DIRECTION('ref_axis',(1.,0.,0.));
#19334=DIRECTION('center_axis',(0.,0.,1.));
#19335=DIRECTION('ref_axis',(1.,0.,0.));
#19336=DIRECTION('',(0.,0.,1.));
#19337=DIRECTION('center_axis',(0.,0.,1.));
#19338=DIRECTION('ref_axis',(1.,0.,0.));
#19339=DIRECTION('center_axis',(0.,0.,1.));
#19340=DIRECTION('ref_axis',(1.,0.,0.));
#19341=DIRECTION('center_axis',(0.,0.,1.));
#19342=DIRECTION('ref_axis',(1.,0.,0.));
#19343=DIRECTION('',(0.,0.,1.));
#19344=DIRECTION('center_axis',(0.,0.,1.));
#19345=DIRECTION('ref_axis',(1.,0.,0.));
#19346=DIRECTION('center_axis',(0.,0.,1.));
#19347=DIRECTION('ref_axis',(1.,0.,0.));
#19348=DIRECTION('center_axis',(0.,0.,1.));
#19349=DIRECTION('ref_axis',(1.,0.,0.));
#19350=DIRECTION('',(0.,0.,1.));
#19351=DIRECTION('center_axis',(0.,0.,1.));
#19352=DIRECTION('ref_axis',(1.,0.,0.));
#19353=DIRECTION('center_axis',(0.,0.,1.));
#19354=DIRECTION('ref_axis',(1.,0.,0.));
#19355=DIRECTION('center_axis',(0.,0.,1.));
#19356=DIRECTION('ref_axis',(1.,0.,0.));
#19357=DIRECTION('',(0.,0.,1.));
#19358=DIRECTION('center_axis',(0.,0.,1.));
#19359=DIRECTION('ref_axis',(1.,0.,0.));
#19360=DIRECTION('center_axis',(0.,0.,1.));
#19361=DIRECTION('ref_axis',(1.,0.,0.));
#19362=DIRECTION('center_axis',(0.,0.,1.));
#19363=DIRECTION('ref_axis',(1.,0.,0.));
#19364=DIRECTION('',(0.,0.,1.));
#19365=DIRECTION('center_axis',(0.,0.,-1.));
#19366=DIRECTION('ref_axis',(1.,0.,0.));
#19367=DIRECTION('center_axis',(0.,0.,1.));
#19368=DIRECTION('ref_axis',(1.,0.,0.));
#19369=DIRECTION('',(0.,0.,1.));
#19370=DIRECTION('center_axis',(0.,0.,-1.));
#19371=DIRECTION('ref_axis',(1.,0.,0.));
#19372=DIRECTION('center_axis',(0.,0.,1.));
#19373=DIRECTION('ref_axis',(1.,0.,0.));
#19374=DIRECTION('',(0.,0.,1.));
#19375=DIRECTION('center_axis',(0.,0.,-1.));
#19376=DIRECTION('ref_axis',(1.,0.,0.));
#19377=DIRECTION('center_axis',(0.,0.,1.));
#19378=DIRECTION('ref_axis',(1.,0.,0.));
#19379=DIRECTION('',(0.,0.,1.));
#19380=DIRECTION('center_axis',(0.,0.,-1.));
#19381=DIRECTION('ref_axis',(1.,0.,0.));
#19382=DIRECTION('center_axis',(0.,0.,1.));
#19383=DIRECTION('ref_axis',(1.,0.,0.));
#19384=DIRECTION('',(0.,0.,1.));
#19385=DIRECTION('center_axis',(0.,0.,-1.));
#19386=DIRECTION('ref_axis',(1.,0.,0.));
#19387=DIRECTION('center_axis',(0.,0.,1.));
#19388=DIRECTION('ref_axis',(1.,0.,0.));
#19389=DIRECTION('',(0.,0.,1.));
#19390=DIRECTION('center_axis',(0.,0.,-1.));
#19391=DIRECTION('ref_axis',(1.,0.,0.));
#19392=DIRECTION('center_axis',(1.,0.,0.));
#19393=DIRECTION('ref_axis',(0.,1.,0.));
#19394=DIRECTION('',(0.,1.,0.));
#19395=DIRECTION('center_axis',(0.,0.,1.));
#19396=DIRECTION('ref_axis',(1.,0.,0.));
#19397=DIRECTION('',(0.,1.,0.));
#19398=DIRECTION('center_axis',(-1.,0.,0.));
#19399=DIRECTION('ref_axis',(0.,-1.,0.));
#19400=DIRECTION('',(0.,-1.,0.));
#19401=DIRECTION('center_axis',(0.,0.,1.));
#19402=DIRECTION('ref_axis',(1.,0.,0.));
#19403=DIRECTION('',(0.,-1.,0.));
#19404=DIRECTION('center_axis',(-1.,0.,0.));
#19405=DIRECTION('ref_axis',(0.,-1.,0.));
#19406=DIRECTION('',(0.,-1.,0.));
#19407=DIRECTION('center_axis',(1.,0.,0.));
#19408=DIRECTION('ref_axis',(0.,1.,0.));
#19409=DIRECTION('',(0.,1.,0.));
#19410=DIRECTION('center_axis',(-1.,0.,0.));
#19411=DIRECTION('ref_axis',(0.,-1.,0.));
#19412=DIRECTION('',(0.,-1.,0.));
#19413=DIRECTION('center_axis',(0.,0.,1.));
#19414=DIRECTION('ref_axis',(1.,0.,0.));
#19415=DIRECTION('center_axis',(1.,0.,0.));
#19416=DIRECTION('ref_axis',(0.,1.,0.));
#19417=DIRECTION('',(0.,1.,0.));
#19418=DIRECTION('center_axis',(0.,0.,1.));
#19419=DIRECTION('ref_axis',(1.,0.,0.));
#19420=DIRECTION('axis',(0.,0.,1.));
#19421=DIRECTION('refdir',(1.,0.,0.));
#19422=DIRECTION('center_axis',(0.,0.,1.));
#19423=DIRECTION('ref_axis',(1.,0.,0.));
#19424=DIRECTION('center_axis',(0.,0.,1.));
#19425=DIRECTION('ref_axis',(1.,0.,0.));
#19426=DIRECTION('',(0.,0.,-1.));
#19427=DIRECTION('center_axis',(0.,0.,1.));
#19428=DIRECTION('ref_axis',(1.,0.,0.));
#19429=DIRECTION('center_axis',(0.,0.,1.));
#19430=DIRECTION('ref_axis',(1.,0.,0.));
#19431=DIRECTION('center_axis',(0.,0.,1.));
#19432=DIRECTION('ref_axis',(1.,0.,0.));
#19433=DIRECTION('axis',(0.,0.,1.));
#19434=DIRECTION('refdir',(1.,0.,0.));
#19435=DIRECTION('center_axis',(0.,0.,1.));
#19436=DIRECTION('ref_axis',(1.,0.,0.));
#19437=DIRECTION('center_axis',(0.,0.,1.));
#19438=DIRECTION('ref_axis',(1.,0.,0.));
#19439=DIRECTION('',(0.,0.,-1.));
#19440=DIRECTION('center_axis',(0.,0.,1.));
#19441=DIRECTION('ref_axis',(1.,0.,0.));
#19442=DIRECTION('center_axis',(0.,0.,1.));
#19443=DIRECTION('ref_axis',(1.,0.,0.));
#19444=DIRECTION('center_axis',(0.,0.,1.));
#19445=DIRECTION('ref_axis',(1.,0.,0.));
#19446=DIRECTION('axis',(0.,0.,1.));
#19447=DIRECTION('refdir',(1.,0.,0.));
#19448=DIRECTION('center_axis',(0.,0.,1.));
#19449=DIRECTION('ref_axis',(1.,0.,0.));
#19450=DIRECTION('center_axis',(0.,0.,1.));
#19451=DIRECTION('ref_axis',(1.,0.,0.));
#19452=DIRECTION('',(0.,0.,-1.));
#19453=DIRECTION('center_axis',(0.,0.,1.));
#19454=DIRECTION('ref_axis',(1.,0.,0.));
#19455=DIRECTION('center_axis',(0.,0.,1.));
#19456=DIRECTION('ref_axis',(1.,0.,0.));
#19457=DIRECTION('center_axis',(0.,0.,1.));
#19458=DIRECTION('ref_axis',(1.,0.,0.));
#19459=DIRECTION('axis',(0.,0.,1.));
#19460=DIRECTION('refdir',(1.,0.,0.));
#19461=DIRECTION('center_axis',(0.,0.,1.));
#19462=DIRECTION('ref_axis',(1.,0.,0.));
#19463=DIRECTION('center_axis',(0.,0.,1.));
#19464=DIRECTION('ref_axis',(1.,0.,0.));
#19465=DIRECTION('',(0.,0.,-1.));
#19466=DIRECTION('center_axis',(0.,0.,1.));
#19467=DIRECTION('ref_axis',(1.,0.,0.));
#19468=DIRECTION('center_axis',(0.,0.,1.));
#19469=DIRECTION('ref_axis',(1.,0.,0.));
#19470=DIRECTION('center_axis',(0.,0.,1.));
#19471=DIRECTION('ref_axis',(1.,0.,0.));
#19472=DIRECTION('axis',(0.,0.,1.));
#19473=DIRECTION('refdir',(1.,0.,0.));
#19474=DIRECTION('center_axis',(0.,1.,0.));
#19475=DIRECTION('ref_axis',(0.707106781186543,0.,0.707106781186552));
#19476=DIRECTION('',(0.,1.,0.));
#19477=DIRECTION('center_axis',(0.,1.,0.));
#19478=DIRECTION('ref_axis',(1.,0.,0.));
#19479=DIRECTION('',(0.,-1.,0.));
#19480=DIRECTION('center_axis',(0.,-1.,0.));
#19481=DIRECTION('ref_axis',(1.,0.,0.));
#19482=DIRECTION('center_axis',(0.,1.,0.));
#19483=DIRECTION('ref_axis',(0.707106781186542,0.,-0.707106781186553));
#19484=DIRECTION('',(0.,1.,0.));
#19485=DIRECTION('center_axis',(0.,1.,0.));
#19486=DIRECTION('ref_axis',(1.,0.,0.));
#19487=DIRECTION('',(0.,-1.,0.));
#19488=DIRECTION('center_axis',(0.,-1.,0.));
#19489=DIRECTION('ref_axis',(1.,0.,0.));
#19490=DIRECTION('center_axis',(0.,1.,0.));
#19491=DIRECTION('ref_axis',(-0.707106781186542,0.,-0.707106781186553));
#19492=DIRECTION('',(0.,1.,0.));
#19493=DIRECTION('center_axis',(0.,1.,0.));
#19494=DIRECTION('ref_axis',(1.,0.,0.));
#19495=DIRECTION('',(0.,-1.,0.));
#19496=DIRECTION('center_axis',(0.,-1.,0.));
#19497=DIRECTION('ref_axis',(1.,0.,0.));
#19498=DIRECTION('center_axis',(0.,1.,0.));
#19499=DIRECTION('ref_axis',(-0.707106781186549,0.,0.707106781186546));
#19500=DIRECTION('',(0.,1.,0.));
#19501=DIRECTION('center_axis',(0.,1.,0.));
#19502=DIRECTION('ref_axis',(1.,0.,0.));
#19503=DIRECTION('',(0.,-1.,0.));
#19504=DIRECTION('center_axis',(0.,-1.,0.));
#19505=DIRECTION('ref_axis',(1.,0.,0.));
#19506=DIRECTION('center_axis',(0.,1.,0.));
#19507=DIRECTION('ref_axis',(1.,0.,0.));
#19508=DIRECTION('center_axis',(0.,1.,0.));
#19509=DIRECTION('ref_axis',(1.,0.,0.));
#19510=DIRECTION('center_axis',(0.,1.,0.));
#19511=DIRECTION('ref_axis',(1.,0.,0.));
#19512=DIRECTION('center_axis',(0.,1.,0.));
#19513=DIRECTION('ref_axis',(1.,0.,0.));
#19514=DIRECTION('center_axis',(0.,1.,0.));
#19515=DIRECTION('ref_axis',(1.,0.,0.));
#19516=DIRECTION('center_axis',(0.,-1.,0.));
#19517=DIRECTION('ref_axis',(1.,0.,0.));
#19518=DIRECTION('center_axis',(0.,1.,0.));
#19519=DIRECTION('ref_axis',(1.,0.,0.));
#19520=DIRECTION('center_axis',(0.,1.,0.));
#19521=DIRECTION('ref_axis',(1.,0.,0.));
#19522=DIRECTION('center_axis',(0.,1.,0.));
#19523=DIRECTION('ref_axis',(1.,0.,0.));
#19524=DIRECTION('center_axis',(0.,1.,0.));
#19525=DIRECTION('ref_axis',(1.,0.,0.));
#19526=DIRECTION('center_axis',(0.,1.,0.));
#19527=DIRECTION('ref_axis',(1.,0.,0.));
#19528=DIRECTION('center_axis',(0.,1.,0.));
#19529=DIRECTION('ref_axis',(1.,0.,0.));
#19530=DIRECTION('center_axis',(0.,1.,0.));
#19531=DIRECTION('ref_axis',(-1.,0.,3.21624529935327E-16));
#19532=DIRECTION('center_axis',(0.,1.,0.));
#19533=DIRECTION('ref_axis',(1.,0.,0.));
#19534=DIRECTION('center_axis',(0.,1.,0.));
#19535=DIRECTION('ref_axis',(1.,0.,0.));
#19536=DIRECTION('center_axis',(0.,1.,0.));
#19537=DIRECTION('ref_axis',(1.,0.,0.));
#19538=DIRECTION('',(0.,-1.,0.));
#19539=DIRECTION('center_axis',(0.,-1.,0.));
#19540=DIRECTION('ref_axis',(1.,0.,0.));
#19541=DIRECTION('center_axis',(0.,1.,0.));
#19542=DIRECTION('ref_axis',(1.,0.,0.));
#19543=DIRECTION('center_axis',(0.,-1.,0.));
#19544=DIRECTION('ref_axis',(1.,0.,0.));
#19545=DIRECTION('center_axis',(0.,1.,0.));
#19546=DIRECTION('ref_axis',(1.,0.,0.));
#19547=DIRECTION('',(0.,-1.,0.));
#19548=DIRECTION('center_axis',(0.,1.,0.));
#19549=DIRECTION('ref_axis',(1.,0.,0.));
#19550=DIRECTION('axis',(0.,0.,1.));
#19551=DIRECTION('refdir',(1.,0.,0.));
#19552=DIRECTION('center_axis',(0.,1.,0.));
#19553=DIRECTION('ref_axis',(0.707106781186543,0.,0.707106781186552));
#19554=DIRECTION('',(0.,1.,0.));
#19555=DIRECTION('center_axis',(0.,1.,0.));
#19556=DIRECTION('ref_axis',(1.,0.,0.));
#19557=DIRECTION('',(0.,-1.,0.));
#19558=DIRECTION('center_axis',(0.,-1.,0.));
#19559=DIRECTION('ref_axis',(1.,0.,0.));
#19560=DIRECTION('center_axis',(0.,1.,0.));
#19561=DIRECTION('ref_axis',(0.707106781186542,0.,-0.707106781186553));
#19562=DIRECTION('',(0.,1.,0.));
#19563=DIRECTION('center_axis',(0.,1.,0.));
#19564=DIRECTION('ref_axis',(1.,0.,0.));
#19565=DIRECTION('',(0.,-1.,0.));
#19566=DIRECTION('center_axis',(0.,-1.,0.));
#19567=DIRECTION('ref_axis',(1.,0.,0.));
#19568=DIRECTION('center_axis',(0.,1.,0.));
#19569=DIRECTION('ref_axis',(-0.707106781186542,0.,-0.707106781186553));
#19570=DIRECTION('',(0.,1.,0.));
#19571=DIRECTION('center_axis',(0.,1.,0.));
#19572=DIRECTION('ref_axis',(1.,0.,0.));
#19573=DIRECTION('',(0.,-1.,0.));
#19574=DIRECTION('center_axis',(0.,-1.,0.));
#19575=DIRECTION('ref_axis',(1.,0.,0.));
#19576=DIRECTION('center_axis',(0.,1.,0.));
#19577=DIRECTION('ref_axis',(-0.707106781186549,0.,0.707106781186546));
#19578=DIRECTION('',(0.,1.,0.));
#19579=DIRECTION('center_axis',(0.,1.,0.));
#19580=DIRECTION('ref_axis',(1.,0.,0.));
#19581=DIRECTION('',(0.,-1.,0.));
#19582=DIRECTION('center_axis',(0.,-1.,0.));
#19583=DIRECTION('ref_axis',(1.,0.,0.));
#19584=DIRECTION('center_axis',(0.,1.,0.));
#19585=DIRECTION('ref_axis',(1.,0.,0.));
#19586=DIRECTION('center_axis',(0.,1.,0.));
#19587=DIRECTION('ref_axis',(1.,0.,0.));
#19588=DIRECTION('center_axis',(0.,1.,0.));
#19589=DIRECTION('ref_axis',(1.,0.,0.));
#19590=DIRECTION('center_axis',(0.,1.,0.));
#19591=DIRECTION('ref_axis',(1.,0.,0.));
#19592=DIRECTION('center_axis',(0.,1.,0.));
#19593=DIRECTION('ref_axis',(1.,0.,0.));
#19594=DIRECTION('center_axis',(0.,1.,0.));
#19595=DIRECTION('ref_axis',(1.,0.,0.));
#19596=DIRECTION('center_axis',(0.,1.,0.));
#19597=DIRECTION('ref_axis',(1.,0.,0.));
#19598=DIRECTION('center_axis',(0.,1.,0.));
#19599=DIRECTION('ref_axis',(1.,0.,0.));
#19600=DIRECTION('center_axis',(0.,1.,0.));
#19601=DIRECTION('ref_axis',(1.,0.,0.));
#19602=DIRECTION('center_axis',(0.,1.,0.));
#19603=DIRECTION('ref_axis',(1.,0.,0.));
#19604=DIRECTION('center_axis',(0.,1.,0.));
#19605=DIRECTION('ref_axis',(1.,0.,0.));
#19606=DIRECTION('center_axis',(0.,1.,0.));
#19607=DIRECTION('ref_axis',(1.,0.,0.));
#19608=DIRECTION('center_axis',(0.,1.,0.));
#19609=DIRECTION('ref_axis',(-1.,0.,3.21624529935327E-16));
#19610=DIRECTION('center_axis',(0.,1.,0.));
#19611=DIRECTION('ref_axis',(1.,0.,0.));
#19612=DIRECTION('center_axis',(0.,1.,0.));
#19613=DIRECTION('ref_axis',(1.,0.,0.));
#19614=DIRECTION('',(0.,-1.,0.));
#19615=DIRECTION('center_axis',(0.,1.,0.));
#19616=DIRECTION('ref_axis',(1.,0.,0.));
#19617=DIRECTION('center_axis',(0.,1.,0.));
#19618=DIRECTION('ref_axis',(1.,0.,0.));
#19619=DIRECTION('center_axis',(0.,-1.,0.));
#19620=DIRECTION('ref_axis',(1.,0.,0.));
#19621=DIRECTION('center_axis',(0.,1.,0.));
#19622=DIRECTION('ref_axis',(1.,0.,0.));
#19623=DIRECTION('center_axis',(0.,-1.,0.));
#19624=DIRECTION('ref_axis',(1.,0.,0.));
#19625=DIRECTION('',(0.,-1.,0.));
#19626=DIRECTION('center_axis',(0.,1.,0.));
#19627=DIRECTION('ref_axis',(1.,0.,0.));
#19628=DIRECTION('axis',(0.,0.,1.));
#19629=DIRECTION('refdir',(1.,0.,0.));
#19630=DIRECTION('center_axis',(0.,1.,0.));
#19631=DIRECTION('ref_axis',(1.,0.,0.));
#19632=DIRECTION('center_axis',(0.,1.,0.));
#19633=DIRECTION('ref_axis',(1.,0.,0.));
#19634=DIRECTION('',(0.,1.,0.));
#19635=DIRECTION('center_axis',(0.,-1.,0.));
#19636=DIRECTION('ref_axis',(1.,0.,0.));
#19637=DIRECTION('center_axis',(0.,1.,0.));
#19638=DIRECTION('ref_axis',(1.,0.,0.));
#19639=DIRECTION('center_axis',(0.,1.,0.));
#19640=DIRECTION('ref_axis',(1.,0.,0.));
#19641=DIRECTION('',(0.,1.,0.));
#19642=DIRECTION('center_axis',(0.,-1.,0.));
#19643=DIRECTION('ref_axis',(1.,0.,0.));
#19644=DIRECTION('center_axis',(0.,1.,0.));
#19645=DIRECTION('ref_axis',(1.,0.,0.));
#19646=DIRECTION('center_axis',(0.,1.,0.));
#19647=DIRECTION('ref_axis',(1.,0.,0.));
#19648=DIRECTION('',(0.,1.,0.));
#19649=DIRECTION('center_axis',(0.,-1.,0.));
#19650=DIRECTION('ref_axis',(1.,0.,0.));
#19651=DIRECTION('center_axis',(0.,1.,0.));
#19652=DIRECTION('ref_axis',(1.,0.,0.));
#19653=DIRECTION('center_axis',(0.,1.,0.));
#19654=DIRECTION('ref_axis',(1.,0.,0.));
#19655=DIRECTION('',(0.,1.,0.));
#19656=DIRECTION('center_axis',(0.,-1.,0.));
#19657=DIRECTION('ref_axis',(1.,0.,0.));
#19658=DIRECTION('center_axis',(0.,1.,0.));
#19659=DIRECTION('ref_axis',(1.,0.,0.));
#19660=DIRECTION('center_axis',(0.,1.,0.));
#19661=DIRECTION('ref_axis',(1.,0.,0.));
#19662=DIRECTION('',(0.,-1.,0.));
#19663=DIRECTION('center_axis',(0.,-1.,0.));
#19664=DIRECTION('ref_axis',(1.,0.,0.));
#19665=DIRECTION('center_axis',(0.,1.,0.));
#19666=DIRECTION('ref_axis',(1.,0.,0.));
#19667=DIRECTION('center_axis',(0.,-1.,0.));
#19668=DIRECTION('ref_axis',(1.,0.,0.));
#19669=DIRECTION('center_axis',(0.,1.,0.));
#19670=DIRECTION('ref_axis',(1.,0.,0.));
#19671=DIRECTION('',(0.,-1.,0.));
#19672=DIRECTION('center_axis',(0.,-1.,0.));
#19673=DIRECTION('ref_axis',(1.,0.,0.));
#19674=DIRECTION('center_axis',(0.,1.,0.));
#19675=DIRECTION('ref_axis',(1.,0.,0.));
#19676=DIRECTION('center_axis',(0.,1.,0.));
#19677=DIRECTION('ref_axis',(1.,0.,0.));
#19678=DIRECTION('',(0.,-1.,0.));
#19679=DIRECTION('center_axis',(0.,1.,0.));
#19680=DIRECTION('ref_axis',(1.,0.,0.));
#19681=DIRECTION('center_axis',(0.,1.,0.));
#19682=DIRECTION('ref_axis',(1.,0.,0.));
#19683=DIRECTION('center_axis',(0.,1.,0.));
#19684=DIRECTION('ref_axis',(1.,0.,0.));
#19685=DIRECTION('axis',(0.,0.,1.));
#19686=DIRECTION('refdir',(1.,0.,0.));
#19687=DIRECTION('center_axis',(0.,1.,0.));
#19688=DIRECTION('ref_axis',(1.,0.,0.));
#19689=DIRECTION('center_axis',(0.,1.,0.));
#19690=DIRECTION('ref_axis',(1.,0.,0.));
#19691=DIRECTION('',(0.,1.,0.));
#19692=DIRECTION('center_axis',(0.,-1.,0.));
#19693=DIRECTION('ref_axis',(1.,0.,0.));
#19694=DIRECTION('center_axis',(0.,1.,0.));
#19695=DIRECTION('ref_axis',(1.,0.,0.));
#19696=DIRECTION('center_axis',(0.,1.,0.));
#19697=DIRECTION('ref_axis',(1.,0.,0.));
#19698=DIRECTION('',(0.,1.,0.));
#19699=DIRECTION('center_axis',(0.,-1.,0.));
#19700=DIRECTION('ref_axis',(1.,0.,0.));
#19701=DIRECTION('center_axis',(0.,1.,0.));
#19702=DIRECTION('ref_axis',(1.,0.,0.));
#19703=DIRECTION('center_axis',(0.,1.,0.));
#19704=DIRECTION('ref_axis',(1.,0.,0.));
#19705=DIRECTION('',(0.,1.,0.));
#19706=DIRECTION('center_axis',(0.,-1.,0.));
#19707=DIRECTION('ref_axis',(1.,0.,0.));
#19708=DIRECTION('center_axis',(0.,1.,0.));
#19709=DIRECTION('ref_axis',(1.,0.,0.));
#19710=DIRECTION('center_axis',(0.,1.,0.));
#19711=DIRECTION('ref_axis',(1.,0.,0.));
#19712=DIRECTION('',(0.,1.,0.));
#19713=DIRECTION('center_axis',(0.,-1.,0.));
#19714=DIRECTION('ref_axis',(1.,0.,0.));
#19715=DIRECTION('center_axis',(0.,1.,0.));
#19716=DIRECTION('ref_axis',(1.,0.,0.));
#19717=DIRECTION('center_axis',(0.,1.,0.));
#19718=DIRECTION('ref_axis',(1.,0.,0.));
#19719=DIRECTION('',(0.,-1.,0.));
#19720=DIRECTION('center_axis',(0.,1.,0.));
#19721=DIRECTION('ref_axis',(1.,0.,0.));
#19722=DIRECTION('center_axis',(0.,1.,0.));
#19723=DIRECTION('ref_axis',(1.,0.,0.));
#19724=DIRECTION('center_axis',(0.,-1.,0.));
#19725=DIRECTION('ref_axis',(1.,0.,0.));
#19726=DIRECTION('center_axis',(0.,1.,0.));
#19727=DIRECTION('ref_axis',(1.,0.,0.));
#19728=DIRECTION('center_axis',(0.,-1.,0.));
#19729=DIRECTION('ref_axis',(1.,0.,0.));
#19730=DIRECTION('',(0.,-1.,0.));
#19731=DIRECTION('center_axis',(0.,1.,0.));
#19732=DIRECTION('ref_axis',(1.,0.,0.));
#19733=DIRECTION('center_axis',(0.,1.,0.));
#19734=DIRECTION('ref_axis',(1.,0.,0.));
#19735=DIRECTION('',(0.,-1.,0.));
#19736=DIRECTION('center_axis',(0.,1.,0.));
#19737=DIRECTION('ref_axis',(1.,0.,0.));
#19738=DIRECTION('center_axis',(0.,1.,0.));
#19739=DIRECTION('ref_axis',(1.,0.,0.));
#19740=DIRECTION('center_axis',(0.,1.,0.));
#19741=DIRECTION('ref_axis',(1.,0.,0.));
#19742=DIRECTION('axis',(0.,0.,1.));
#19743=DIRECTION('refdir',(1.,0.,0.));
#19744=DIRECTION('center_axis',(0.,1.,0.));
#19745=DIRECTION('ref_axis',(1.,0.,0.));
#19746=DIRECTION('center_axis',(0.,1.,0.));
#19747=DIRECTION('ref_axis',(1.,0.,0.));
#19748=DIRECTION('',(0.,1.,0.));
#19749=DIRECTION('center_axis',(0.,-1.,0.));
#19750=DIRECTION('ref_axis',(1.,0.,0.));
#19751=DIRECTION('center_axis',(0.,1.,0.));
#19752=DIRECTION('ref_axis',(1.,0.,0.));
#19753=DIRECTION('center_axis',(0.,1.,0.));
#19754=DIRECTION('ref_axis',(1.,0.,0.));
#19755=DIRECTION('',(0.,1.,0.));
#19756=DIRECTION('center_axis',(0.,-1.,0.));
#19757=DIRECTION('ref_axis',(1.,0.,0.));
#19758=DIRECTION('center_axis',(0.,1.,0.));
#19759=DIRECTION('ref_axis',(1.,0.,0.));
#19760=DIRECTION('center_axis',(0.,1.,0.));
#19761=DIRECTION('ref_axis',(1.,0.,0.));
#19762=DIRECTION('',(0.,1.,0.));
#19763=DIRECTION('center_axis',(0.,-1.,0.));
#19764=DIRECTION('ref_axis',(1.,0.,0.));
#19765=DIRECTION('center_axis',(0.,1.,0.));
#19766=DIRECTION('ref_axis',(1.,0.,0.));
#19767=DIRECTION('center_axis',(0.,1.,0.));
#19768=DIRECTION('ref_axis',(1.,0.,0.));
#19769=DIRECTION('',(0.,1.,0.));
#19770=DIRECTION('center_axis',(0.,-1.,0.));
#19771=DIRECTION('ref_axis',(1.,0.,0.));
#19772=DIRECTION('center_axis',(0.,1.,0.));
#19773=DIRECTION('ref_axis',(1.,0.,0.));
#19774=DIRECTION('center_axis',(0.,1.,0.));
#19775=DIRECTION('ref_axis',(1.,0.,0.));
#19776=DIRECTION('',(0.,-1.,0.));
#19777=DIRECTION('center_axis',(0.,-1.,0.));
#19778=DIRECTION('ref_axis',(1.,0.,0.));
#19779=DIRECTION('center_axis',(0.,1.,0.));
#19780=DIRECTION('ref_axis',(1.,0.,0.));
#19781=DIRECTION('center_axis',(0.,-1.,0.));
#19782=DIRECTION('ref_axis',(1.,0.,0.));
#19783=DIRECTION('center_axis',(0.,1.,0.));
#19784=DIRECTION('ref_axis',(1.,0.,0.));
#19785=DIRECTION('',(0.,-1.,0.));
#19786=DIRECTION('center_axis',(0.,-1.,0.));
#19787=DIRECTION('ref_axis',(1.,0.,0.));
#19788=DIRECTION('center_axis',(0.,1.,0.));
#19789=DIRECTION('ref_axis',(1.,0.,0.));
#19790=DIRECTION('center_axis',(0.,1.,0.));
#19791=DIRECTION('ref_axis',(1.,0.,0.));
#19792=DIRECTION('',(0.,-1.,0.));
#19793=DIRECTION('center_axis',(0.,1.,0.));
#19794=DIRECTION('ref_axis',(1.,0.,0.));
#19795=DIRECTION('center_axis',(0.,1.,0.));
#19796=DIRECTION('ref_axis',(1.,0.,0.));
#19797=DIRECTION('center_axis',(0.,1.,0.));
#19798=DIRECTION('ref_axis',(1.,0.,0.));
#19799=DIRECTION('axis',(0.,0.,1.));
#19800=DIRECTION('refdir',(1.,0.,0.));
#19801=DIRECTION('center_axis',(0.,1.,0.));
#19802=DIRECTION('ref_axis',(1.,0.,0.));
#19803=DIRECTION('center_axis',(0.,1.,0.));
#19804=DIRECTION('ref_axis',(1.,0.,0.));
#19805=DIRECTION('',(0.,1.,0.));
#19806=DIRECTION('center_axis',(0.,-1.,0.));
#19807=DIRECTION('ref_axis',(1.,0.,0.));
#19808=DIRECTION('center_axis',(0.,1.,0.));
#19809=DIRECTION('ref_axis',(1.,0.,0.));
#19810=DIRECTION('center_axis',(0.,1.,0.));
#19811=DIRECTION('ref_axis',(1.,0.,0.));
#19812=DIRECTION('',(0.,1.,0.));
#19813=DIRECTION('center_axis',(0.,-1.,0.));
#19814=DIRECTION('ref_axis',(1.,0.,0.));
#19815=DIRECTION('center_axis',(0.,1.,0.));
#19816=DIRECTION('ref_axis',(1.,0.,0.));
#19817=DIRECTION('center_axis',(0.,1.,0.));
#19818=DIRECTION('ref_axis',(1.,0.,0.));
#19819=DIRECTION('',(0.,1.,0.));
#19820=DIRECTION('center_axis',(0.,-1.,0.));
#19821=DIRECTION('ref_axis',(1.,0.,0.));
#19822=DIRECTION('center_axis',(0.,1.,0.));
#19823=DIRECTION('ref_axis',(1.,0.,0.));
#19824=DIRECTION('center_axis',(0.,1.,0.));
#19825=DIRECTION('ref_axis',(1.,0.,0.));
#19826=DIRECTION('',(0.,1.,0.));
#19827=DIRECTION('center_axis',(0.,-1.,0.));
#19828=DIRECTION('ref_axis',(1.,0.,0.));
#19829=DIRECTION('center_axis',(0.,1.,0.));
#19830=DIRECTION('ref_axis',(1.,0.,0.));
#19831=DIRECTION('center_axis',(0.,1.,0.));
#19832=DIRECTION('ref_axis',(1.,0.,0.));
#19833=DIRECTION('',(0.,-1.,0.));
#19834=DIRECTION('center_axis',(0.,1.,0.));
#19835=DIRECTION('ref_axis',(1.,0.,0.));
#19836=DIRECTION('center_axis',(0.,1.,0.));
#19837=DIRECTION('ref_axis',(1.,0.,0.));
#19838=DIRECTION('center_axis',(0.,-1.,0.));
#19839=DIRECTION('ref_axis',(1.,0.,0.));
#19840=DIRECTION('center_axis',(0.,1.,0.));
#19841=DIRECTION('ref_axis',(1.,0.,0.));
#19842=DIRECTION('center_axis',(0.,-1.,0.));
#19843=DIRECTION('ref_axis',(1.,0.,0.));
#19844=DIRECTION('',(0.,-1.,0.));
#19845=DIRECTION('center_axis',(0.,1.,0.));
#19846=DIRECTION('ref_axis',(1.,0.,0.));
#19847=DIRECTION('center_axis',(0.,1.,0.));
#19848=DIRECTION('ref_axis',(1.,0.,0.));
#19849=DIRECTION('',(0.,-1.,0.));
#19850=DIRECTION('center_axis',(0.,1.,0.));
#19851=DIRECTION('ref_axis',(1.,0.,0.));
#19852=DIRECTION('center_axis',(0.,1.,0.));
#19853=DIRECTION('ref_axis',(1.,0.,0.));
#19854=DIRECTION('center_axis',(0.,1.,0.));
#19855=DIRECTION('ref_axis',(1.,0.,0.));
#19856=DIRECTION('axis',(0.,0.,1.));
#19857=DIRECTION('refdir',(1.,0.,0.));
#19858=DIRECTION('center_axis',(0.,0.,1.));
#19859=DIRECTION('ref_axis',(1.,0.,0.));
#19860=DIRECTION('center_axis',(0.,0.,1.));
#19861=DIRECTION('ref_axis',(1.,0.,0.));
#19862=DIRECTION('',(0.,0.,1.));
#19863=DIRECTION('center_axis',(0.,0.,-1.));
#19864=DIRECTION('ref_axis',(1.,0.,0.));
#19865=DIRECTION('center_axis',(0.,0.,1.));
#19866=DIRECTION('ref_axis',(1.,0.,0.));
#19867=DIRECTION('center_axis',(0.,0.,1.));
#19868=DIRECTION('ref_axis',(1.,0.,0.));
#19869=DIRECTION('',(0.,0.,1.));
#19870=DIRECTION('center_axis',(0.,0.,-1.));
#19871=DIRECTION('ref_axis',(1.,0.,0.));
#19872=DIRECTION('center_axis',(0.,0.,1.));
#19873=DIRECTION('ref_axis',(1.,0.,0.));
#19874=DIRECTION('center_axis',(0.,0.,1.));
#19875=DIRECTION('ref_axis',(1.,0.,0.));
#19876=DIRECTION('',(0.,0.,1.));
#19877=DIRECTION('center_axis',(0.,0.,-1.));
#19878=DIRECTION('ref_axis',(1.,0.,0.));
#19879=DIRECTION('center_axis',(0.,0.,1.));
#19880=DIRECTION('ref_axis',(1.,0.,0.));
#19881=DIRECTION('center_axis',(0.,0.,1.));
#19882=DIRECTION('ref_axis',(1.,0.,0.));
#19883=DIRECTION('',(0.,0.,1.));
#19884=DIRECTION('center_axis',(0.,0.,-1.));
#19885=DIRECTION('ref_axis',(1.,0.,0.));
#19886=DIRECTION('center_axis',(0.,1.,0.));
#19887=DIRECTION('ref_axis',(-1.,0.,0.));
#19888=DIRECTION('',(-1.,0.,0.));
#19889=DIRECTION('',(0.,0.,1.));
#19890=DIRECTION('',(-1.,0.,0.));
#19891=DIRECTION('',(0.,0.,1.));
#19892=DIRECTION('center_axis',(1.,0.,0.));
#19893=DIRECTION('ref_axis',(0.,1.,0.));
#19894=DIRECTION('',(0.,1.,0.));
#19895=DIRECTION('',(0.,1.,0.));
#19896=DIRECTION('',(0.,0.,1.));
#19897=DIRECTION('center_axis',(0.,-1.,0.));
#19898=DIRECTION('ref_axis',(1.,0.,0.));
#19899=DIRECTION('',(1.,0.,0.));
#19900=DIRECTION('',(1.,0.,0.));
#19901=DIRECTION('',(0.,0.,1.));
#19902=DIRECTION('center_axis',(-1.,0.,0.));
#19903=DIRECTION('ref_axis',(0.,-1.,0.));
#19904=DIRECTION('',(0.,-1.,0.));
#19905=DIRECTION('',(0.,-1.,0.));
#19906=DIRECTION('center_axis',(0.,0.,1.));
#19907=DIRECTION('ref_axis',(1.,0.,0.));
#19908=DIRECTION('center_axis',(0.,0.,1.));
#19909=DIRECTION('ref_axis',(1.,0.,0.));
#19910=DIRECTION('axis',(0.,0.,1.));
#19911=DIRECTION('refdir',(1.,0.,0.));
#19912=DIRECTION('center_axis',(0.,1.,0.));
#19913=DIRECTION('ref_axis',(-1.,0.,0.));
#19914=DIRECTION('',(-1.,0.,0.));
#19915=DIRECTION('',(0.,0.,1.));
#19916=DIRECTION('',(-1.,0.,0.));
#19917=DIRECTION('',(0.,0.,1.));
#19918=DIRECTION('center_axis',(1.,0.,0.));
#19919=DIRECTION('ref_axis',(0.,1.,0.));
#19920=DIRECTION('',(0.,1.,0.));
#19921=DIRECTION('',(0.,1.,0.));
#19922=DIRECTION('',(0.,0.,1.));
#19923=DIRECTION('center_axis',(0.,-1.,0.));
#19924=DIRECTION('ref_axis',(1.,0.,0.));
#19925=DIRECTION('',(1.,0.,0.));
#19926=DIRECTION('',(1.,0.,0.));
#19927=DIRECTION('',(0.,0.,1.));
#19928=DIRECTION('center_axis',(-1.,0.,0.));
#19929=DIRECTION('ref_axis',(0.,-1.,0.));
#19930=DIRECTION('',(0.,-1.,0.));
#19931=DIRECTION('',(0.,-1.,0.));
#19932=DIRECTION('center_axis',(0.,0.,1.));
#19933=DIRECTION('ref_axis',(1.,0.,0.));
#19934=DIRECTION('center_axis',(0.,0.,1.));
#19935=DIRECTION('ref_axis',(1.,0.,0.));
#19936=DIRECTION('axis',(0.,0.,1.));
#19937=DIRECTION('refdir',(1.,0.,0.));
#19938=DIRECTION('center_axis',(0.,1.,0.));
#19939=DIRECTION('ref_axis',(-1.,0.,0.));
#19940=DIRECTION('',(-1.,0.,0.));
#19941=DIRECTION('',(0.,0.,1.));
#19942=DIRECTION('',(-1.,0.,0.));
#19943=DIRECTION('',(0.,0.,1.));
#19944=DIRECTION('center_axis',(1.,0.,0.));
#19945=DIRECTION('ref_axis',(0.,1.,0.));
#19946=DIRECTION('',(0.,1.,0.));
#19947=DIRECTION('',(0.,1.,0.));
#19948=DIRECTION('',(0.,0.,1.));
#19949=DIRECTION('center_axis',(0.,-1.,0.));
#19950=DIRECTION('ref_axis',(1.,0.,0.));
#19951=DIRECTION('',(1.,0.,0.));
#19952=DIRECTION('',(1.,0.,0.));
#19953=DIRECTION('',(0.,0.,1.));
#19954=DIRECTION('center_axis',(-1.,0.,0.));
#19955=DIRECTION('ref_axis',(0.,-1.,0.));
#19956=DIRECTION('',(0.,-1.,0.));
#19957=DIRECTION('',(0.,-1.,0.));
#19958=DIRECTION('center_axis',(0.,0.,1.));
#19959=DIRECTION('ref_axis',(1.,0.,0.));
#19960=DIRECTION('center_axis',(0.,0.,1.));
#19961=DIRECTION('ref_axis',(1.,0.,0.));
#19962=DIRECTION('axis',(0.,0.,1.));
#19963=DIRECTION('refdir',(1.,0.,0.));
#19964=DIRECTION('center_axis',(0.866025403784439,0.,-0.5));
#19965=DIRECTION('ref_axis',(0.5,0.,0.866025403784439));
#19966=DIRECTION('',(-0.5,0.,-0.866025403784439));
#19967=DIRECTION('',(0.,-1.,0.));
#19968=DIRECTION('',(0.5,0.,0.866025403784439));
#19969=DIRECTION('',(0.,-1.,0.));
#19970=DIRECTION('center_axis',(1.92296268638356E-16,0.,-1.));
#19971=DIRECTION('ref_axis',(1.,0.,1.92296268638356E-16));
#19972=DIRECTION('',(-1.,0.,-1.92296268638356E-16));
#19973=DIRECTION('',(0.,-1.,0.));
#19974=DIRECTION('',(1.,0.,1.92296268638356E-16));
#19975=DIRECTION('center_axis',(-0.866025403784439,0.,-0.5));
#19976=DIRECTION('ref_axis',(0.5,0.,-0.866025403784439));
#19977=DIRECTION('',(-0.5,0.,0.866025403784438));
#19978=DIRECTION('',(0.,-1.,0.));
#19979=DIRECTION('',(0.5,0.,-0.866025403784438));
#19980=DIRECTION('center_axis',(-0.866025403784439,0.,0.5));
#19981=DIRECTION('ref_axis',(-0.5,0.,-0.866025403784439));
#19982=DIRECTION('',(0.5,0.,0.866025403784439));
#19983=DIRECTION('',(0.,-1.,0.));
#19984=DIRECTION('',(-0.5,0.,-0.866025403784439));
#19985=DIRECTION('center_axis',(-1.92296268638356E-16,0.,1.));
#19986=DIRECTION('ref_axis',(-1.,0.,-1.92296268638356E-16));
#19987=DIRECTION('',(1.,0.,1.92296268638356E-16));
#19988=DIRECTION('',(0.,-1.,0.));
#19989=DIRECTION('',(-1.,0.,-1.92296268638356E-16));
#19990=DIRECTION('center_axis',(0.866025403784439,0.,0.5));
#19991=DIRECTION('ref_axis',(-0.5,0.,0.866025403784439));
#19992=DIRECTION('',(0.5,0.,-0.866025403784439));
#19993=DIRECTION('',(-0.5,0.,0.866025403784439));
#19994=DIRECTION('center_axis',(0.,1.,0.));
#19995=DIRECTION('ref_axis',(1.,0.,0.));
#19996=DIRECTION('center_axis',(0.,-1.,0.));
#19997=DIRECTION('ref_axis',(0.,0.,-1.));
#19998=DIRECTION('center_axis',(0.,1.,0.));
#19999=DIRECTION('ref_axis',(1.,0.,0.));
#20000=DIRECTION('center_axis',(0.,1.,0.));
#20001=DIRECTION('ref_axis',(1.,0.,0.));
#20002=DIRECTION('center_axis',(0.,1.,0.));
#20003=DIRECTION('ref_axis',(0.,0.,1.));
#20004=DIRECTION('center_axis',(0.,-1.,0.));
#20005=DIRECTION('ref_axis',(1.,0.,0.));
#20006=DIRECTION('center_axis',(0.,-1.,0.));
#20007=DIRECTION('ref_axis',(1.,0.,0.));
#20008=DIRECTION('center_axis',(0.,-1.,0.));
#20009=DIRECTION('ref_axis',(1.,0.,0.));
#20010=DIRECTION('',(0.707106781186548,0.707106781186547,8.65956056235494E-17));
#20011=DIRECTION('center_axis',(0.,-1.,0.));
#20012=DIRECTION('ref_axis',(1.,0.,0.));
#20013=DIRECTION('center_axis',(0.,-1.,0.));
#20014=DIRECTION('ref_axis',(1.,0.,0.));
#20015=DIRECTION('',(0.,1.,0.));
#20016=DIRECTION('center_axis',(0.,1.,0.));
#20017=DIRECTION('ref_axis',(1.,0.,0.));
#20018=DIRECTION('center_axis',(0.,-1.,0.));
#20019=DIRECTION('ref_axis',(1.,0.,0.));
#20020=DIRECTION('',(-0.707106781186547,0.707106781186548,-8.65956056235493E-17));
#20021=DIRECTION('center_axis',(0.,-1.,0.));
#20022=DIRECTION('ref_axis',(0.,0.,-1.));
#20023=DIRECTION('center_axis',(0.,-1.,0.));
#20024=DIRECTION('ref_axis',(1.,0.,0.));
#20025=DIRECTION('center_axis',(0.,1.,0.));
#20026=DIRECTION('ref_axis',(1.,0.,0.));
#20027=DIRECTION('center_axis',(0.,1.,0.));
#20028=DIRECTION('ref_axis',(1.,0.,0.));
#20029=DIRECTION('',(-0.447213595499958,0.894427190999916,-5.47678698264203E-17));
#20030=DIRECTION('center_axis',(0.,-1.,0.));
#20031=DIRECTION('ref_axis',(1.,0.,0.));
#20032=DIRECTION('',(0.,1.,0.));
#20033=DIRECTION('axis',(0.,0.,1.));
#20034=DIRECTION('refdir',(1.,0.,0.));
#20035=DIRECTION('axis',(0.,0.,1.));
#20036=DIRECTION('refdir',(1.,0.,0.));
#20037=DIRECTION('center_axis',(0.,-1.,0.));
#20038=DIRECTION('ref_axis',(0.,0.,-1.));
#20039=DIRECTION('center_axis',(0.,-1.,0.));
#20040=DIRECTION('ref_axis',(1.,0.,0.));
#20041=DIRECTION('center_axis',(0.,-1.,0.));
#20042=DIRECTION('ref_axis',(1.,0.,0.));
#20043=DIRECTION('center_axis',(1.,0.,1.22464679914735E-16));
#20044=DIRECTION('ref_axis',(-1.22464679914735E-16,0.,1.));
#20045=DIRECTION('center_axis',(0.,1.,0.));
#20046=DIRECTION('ref_axis',(1.,0.,0.));
#20047=DIRECTION('center_axis',(0.,1.,0.));
#20048=DIRECTION('ref_axis',(1.,0.,0.));
#20049=DIRECTION('center_axis',(0.,-1.,0.));
#20050=DIRECTION('ref_axis',(1.,0.,0.));
#20051=DIRECTION('',(0.,1.,0.));
#20052=DIRECTION('center_axis',(0.,-1.,0.));
#20053=DIRECTION('ref_axis',(1.,0.,0.));
#20054=DIRECTION('center_axis',(0.,-1.,0.));
#20055=DIRECTION('ref_axis',(1.,0.,0.));
#20056=DIRECTION('center_axis',(0.,-1.,0.));
#20057=DIRECTION('ref_axis',(1.,0.,0.));
#20058=DIRECTION('',(0.,1.,0.));
#20059=DIRECTION('center_axis',(0.,-1.,0.));
#20060=DIRECTION('ref_axis',(1.,0.,0.));
#20061=DIRECTION('center_axis',(0.,1.,0.));
#20062=DIRECTION('ref_axis',(1.,0.,0.));
#20063=DIRECTION('',(-0.707106781186548,0.707106781186547,-8.65956056235493E-17));
#20064=DIRECTION('center_axis',(0.,-1.,0.));
#20065=DIRECTION('ref_axis',(1.,0.,0.));
#20066=DIRECTION('center_axis',(0.,1.,0.));
#20067=DIRECTION('ref_axis',(0.,0.,1.));
#20068=DIRECTION('center_axis',(0.,-1.,0.));
#20069=DIRECTION('ref_axis',(1.,0.,0.));
#20070=DIRECTION('center_axis',(0.,-1.,0.));
#20071=DIRECTION('ref_axis',(1.,0.,0.));
#20072=DIRECTION('',(0.,1.,0.));
#20073=DIRECTION('center_axis',(0.,-1.,0.));
#20074=DIRECTION('ref_axis',(0.,0.,-1.));
#20075=DIRECTION('center_axis',(0.,-1.,0.));
#20076=DIRECTION('ref_axis',(1.,0.,0.));
#20077=DIRECTION('center_axis',(0.,-1.,0.));
#20078=DIRECTION('ref_axis',(1.,0.,0.));
#20079=DIRECTION('',(0.707106781186548,0.707106781186547,8.65956056235493E-17));
#20080=DIRECTION('axis',(0.,0.,1.));
#20081=DIRECTION('refdir',(1.,0.,0.));
#20082=DIRECTION('center_axis',(0.,-1.,0.));
#20083=DIRECTION('ref_axis',(0.,0.,-1.));
#20084=DIRECTION('center_axis',(0.,-1.,0.));
#20085=DIRECTION('ref_axis',(1.,0.,0.));
#20086=DIRECTION('center_axis',(0.,-1.,0.));
#20087=DIRECTION('ref_axis',(1.,0.,0.));
#20088=DIRECTION('center_axis',(1.,0.,1.22464679914735E-16));
#20089=DIRECTION('ref_axis',(-1.22464679914735E-16,0.,1.));
#20090=DIRECTION('center_axis',(0.,1.,0.));
#20091=DIRECTION('ref_axis',(1.,0.,0.));
#20092=DIRECTION('center_axis',(0.,1.,0.));
#20093=DIRECTION('ref_axis',(1.,0.,0.));
#20094=DIRECTION('center_axis',(0.,-1.,0.));
#20095=DIRECTION('ref_axis',(1.,0.,0.));
#20096=DIRECTION('center_axis',(0.,-1.,0.));
#20097=DIRECTION('ref_axis',(1.,0.,0.));
#20098=DIRECTION('',(0.,1.,0.));
#20099=DIRECTION('center_axis',(0.,1.,0.));
#20100=DIRECTION('ref_axis',(0.,0.,1.));
#20101=DIRECTION('center_axis',(0.,-1.,0.));
#20102=DIRECTION('ref_axis',(1.,0.,0.));
#20103=DIRECTION('center_axis',(0.,-1.,0.));
#20104=DIRECTION('ref_axis',(1.,0.,0.));
#20105=DIRECTION('center_axis',(0.,-1.,0.));
#20106=DIRECTION('ref_axis',(1.,0.,0.));
#20107=DIRECTION('center_axis',(0.,-1.,0.));
#20108=DIRECTION('ref_axis',(1.,0.,0.));
#20109=DIRECTION('',(0.707106781186548,0.707106781186547,8.65956056235494E-17));
#20110=DIRECTION('center_axis',(0.,-1.,0.));
#20111=DIRECTION('ref_axis',(1.,0.,0.));
#20112=DIRECTION('center_axis',(0.,-1.,0.));
#20113=DIRECTION('ref_axis',(1.,0.,0.));
#20114=DIRECTION('',(0.,1.,0.));
#20115=DIRECTION('center_axis',(0.,1.,0.));
#20116=DIRECTION('ref_axis',(1.,0.,0.));
#20117=DIRECTION('center_axis',(0.,-1.,0.));
#20118=DIRECTION('ref_axis',(1.,0.,0.));
#20119=DIRECTION('',(-0.707106781186548,0.707106781186547,-8.65956056235494E-17));
#20120=DIRECTION('center_axis',(0.,-1.,0.));
#20121=DIRECTION('ref_axis',(0.,0.,-1.));
#20122=DIRECTION('center_axis',(0.,-1.,0.));
#20123=DIRECTION('ref_axis',(1.,0.,0.));
#20124=DIRECTION('',(0.,1.,0.));
#20125=DIRECTION('axis',(0.,0.,1.));
#20126=DIRECTION('refdir',(1.,0.,0.));
#20127=DIRECTION('center_axis',(0.,0.,1.));
#20128=DIRECTION('ref_axis',(1.,0.,0.));
#20129=DIRECTION('center_axis',(1.22464679914735E-16,-1.,0.));
#20130=DIRECTION('ref_axis',(-1.,-1.22464679914735E-16,0.));
#20131=DIRECTION('center_axis',(0.78183148246803,0.,0.623489801858733));
#20132=DIRECTION('ref_axis',(0.623489801858734,0.,-0.78183148246803));
#20133=DIRECTION('center_axis',(7.63554790147315E-17,-1.,-9.57467422477103E-17));
#20134=DIRECTION('ref_axis',(-0.623489801858734,-1.22464679914735E-16,0.78183148246803));
#20135=DIRECTION('center_axis',(0.974927912181824,0.,-0.222520933956314));
#20136=DIRECTION('ref_axis',(-0.222520933956314,0.,-0.974927912181824));
#20137=DIRECTION('center_axis',(-2.7250954951288E-17,-1.,-1.19394234705288E-16));
#20138=DIRECTION('ref_axis',(0.222520933956314,-1.22464679914735E-16,0.974927912181824));
#20139=DIRECTION('center_axis',(0.433883739117558,0.,-0.900968867902419));
#20140=DIRECTION('ref_axis',(-0.900968867902419,0.,-0.433883739117558));
#20141=DIRECTION('center_axis',(-1.10336864020811E-16,-1.,-5.31354332312403E-17));
#20142=DIRECTION('ref_axis',(0.900968867902419,-1.22464679914735E-16,0.433883739117558));
#20143=DIRECTION('center_axis',(-0.433883739117558,0.,-0.900968867902419));
#20144=DIRECTION('ref_axis',(-0.900968867902419,0.,0.433883739117558));
#20145=DIRECTION('center_axis',(-1.10336864020811E-16,-1.,5.31354332312403E-17));
#20146=DIRECTION('ref_axis',(0.900968867902419,-1.22464679914735E-16,-0.433883739117558));
#20147=DIRECTION('center_axis',(-0.974927912181824,0.,-0.222520933956314));
#20148=DIRECTION('ref_axis',(-0.222520933956315,0.,0.974927912181824));
#20149=DIRECTION('center_axis',(-2.7250954951288E-17,-1.,1.19394234705288E-16));
#20150=DIRECTION('ref_axis',(0.222520933956315,-1.22464679914735E-16,-0.974927912181824));
#20151=DIRECTION('center_axis',(-0.78183148246803,0.,0.623489801858734));
#20152=DIRECTION('ref_axis',(0.623489801858733,0.,0.78183148246803));
#20153=DIRECTION('center_axis',(7.63554790147315E-17,-1.,9.57467422477103E-17));
#20154=DIRECTION('ref_axis',(-0.623489801858733,-1.22464679914735E-16,-0.78183148246803));
#20155=DIRECTION('axis',(0.,0.,1.));
#20156=DIRECTION('refdir',(1.,0.,0.));
#20157=DIRECTION('center_axis',(0.,0.,1.));
#20158=DIRECTION('ref_axis',(1.,0.,0.));
#20159=DIRECTION('center_axis',(0.,-1.,0.));
#20160=DIRECTION('ref_axis',(0.,0.,-1.));
#20161=DIRECTION('center_axis',(0.,-1.,0.));
#20162=DIRECTION('ref_axis',(0.,0.,-1.));
#20163=DIRECTION('center_axis',(0.,1.,0.));
#20164=DIRECTION('ref_axis',(1.,0.,0.));
#20165=DIRECTION('center_axis',(0.,1.,0.));
#20166=DIRECTION('ref_axis',(1.,0.,0.));
#20167=DIRECTION('center_axis',(0.,1.,0.));
#20168=DIRECTION('ref_axis',(1.,0.,0.));
#20169=DIRECTION('center_axis',(0.,1.,0.));
#20170=DIRECTION('ref_axis',(1.,0.,0.));
#20171=DIRECTION('',(0.,-1.,0.));
#20172=DIRECTION('center_axis',(0.,-1.,0.));
#20173=DIRECTION('ref_axis',(1.,0.,0.));
#20174=DIRECTION('center_axis',(0.,1.,0.));
#20175=DIRECTION('ref_axis',(1.,0.,0.));
#20176=DIRECTION('center_axis',(0.,1.,0.));
#20177=DIRECTION('ref_axis',(1.,0.,0.));
#20178=DIRECTION('center_axis',(0.,1.,0.));
#20179=DIRECTION('ref_axis',(1.,0.,0.));
#20180=DIRECTION('center_axis',(0.,1.,0.));
#20181=DIRECTION('ref_axis',(1.,0.,0.));
#20182=DIRECTION('center_axis',(0.,1.,0.));
#20183=DIRECTION('ref_axis',(1.,0.,0.));
#20184=DIRECTION('center_axis',(0.,1.,0.));
#20185=DIRECTION('ref_axis',(1.,0.,0.));
#20186=DIRECTION('center_axis',(0.,-1.,0.));
#20187=DIRECTION('ref_axis',(1.,0.,0.));
#20188=DIRECTION('center_axis',(0.,-1.,0.));
#20189=DIRECTION('ref_axis',(0.,0.,-1.));
#20190=DIRECTION('center_axis',(8.96625347776458E-17,0.,1.));
#20191=DIRECTION('ref_axis',(1.,0.,0.));
#20192=DIRECTION('center_axis',(0.,-1.,0.));
#20193=DIRECTION('ref_axis',(0.,0.,-1.));
#20194=DIRECTION('center_axis',(0.,1.,0.));
#20195=DIRECTION('ref_axis',(1.,0.,0.));
#20196=DIRECTION('center_axis',(0.,-1.,0.));
#20197=DIRECTION('ref_axis',(1.,0.,0.));
#20198=DIRECTION('center_axis',(0.,-1.,0.));
#20199=DIRECTION('ref_axis',(0.,0.,-1.));
#20200=DIRECTION('center_axis',(0.,0.,1.));
#20201=DIRECTION('ref_axis',(1.,0.,0.));
#20202=DIRECTION('center_axis',(0.,-1.,0.));
#20203=DIRECTION('ref_axis',(0.,0.,-1.));
#20204=DIRECTION('center_axis',(0.,1.,0.));
#20205=DIRECTION('ref_axis',(1.,0.,0.));
#20206=DIRECTION('center_axis',(0.,-1.,0.));
#20207=DIRECTION('ref_axis',(1.,0.,0.));
#20208=DIRECTION('center_axis',(0.,-1.,0.));
#20209=DIRECTION('ref_axis',(1.,0.,0.));
#20210=DIRECTION('center_axis',(0.,-1.,0.));
#20211=DIRECTION('ref_axis',(0.,0.,-1.));
#20212=DIRECTION('center_axis',(0.,0.,1.));
#20213=DIRECTION('ref_axis',(1.,0.,0.));
#20214=DIRECTION('center_axis',(0.,-1.,0.));
#20215=DIRECTION('ref_axis',(0.,0.,-1.));
#20216=DIRECTION('center_axis',(0.,1.,0.));
#20217=DIRECTION('ref_axis',(1.,0.,0.));
#20218=DIRECTION('center_axis',(0.,-1.,0.));
#20219=DIRECTION('ref_axis',(1.,0.,0.));
#20220=DIRECTION('center_axis',(0.,-1.,0.));
#20221=DIRECTION('ref_axis',(0.,0.,-1.));
#20222=DIRECTION('center_axis',(8.96625347776458E-17,0.,1.));
#20223=DIRECTION('ref_axis',(1.,0.,0.));
#20224=DIRECTION('center_axis',(0.,-1.,0.));
#20225=DIRECTION('ref_axis',(0.,0.,-1.));
#20226=DIRECTION('center_axis',(0.,1.,0.));
#20227=DIRECTION('ref_axis',(1.,0.,0.));
#20228=DIRECTION('center_axis',(0.,-1.,0.));
#20229=DIRECTION('ref_axis',(1.,0.,0.));
#20230=DIRECTION('center_axis',(0.,-1.,0.));
#20231=DIRECTION('ref_axis',(0.,0.,-1.));
#20232=DIRECTION('center_axis',(0.,0.,1.));
#20233=DIRECTION('ref_axis',(1.,0.,0.));
#20234=DIRECTION('center_axis',(0.,-1.,0.));
#20235=DIRECTION('ref_axis',(0.,0.,-1.));
#20236=DIRECTION('center_axis',(0.,1.,0.));
#20237=DIRECTION('ref_axis',(1.,0.,0.));
#20238=DIRECTION('center_axis',(0.,1.,0.));
#20239=DIRECTION('ref_axis',(1.,0.,0.));
#20240=DIRECTION('',(0.,1.,0.));
#20241=DIRECTION('center_axis',(0.,-1.,0.));
#20242=DIRECTION('ref_axis',(1.,0.,0.));
#20243=DIRECTION('center_axis',(0.,-1.,0.));
#20244=DIRECTION('ref_axis',(1.,0.,0.));
#20245=DIRECTION('center_axis',(0.,1.,0.));
#20246=DIRECTION('ref_axis',(1.,0.,0.));
#20247=DIRECTION('center_axis',(0.,-1.,0.));
#20248=DIRECTION('ref_axis',(0.,0.,-1.));
#20249=DIRECTION('center_axis',(0.,0.,1.));
#20250=DIRECTION('ref_axis',(1.,0.,0.));
#20251=DIRECTION('center_axis',(0.,-1.,0.));
#20252=DIRECTION('ref_axis',(0.,0.,-1.));
#20253=DIRECTION('center_axis',(0.,-1.,0.));
#20254=DIRECTION('ref_axis',(-1.,0.,0.));
#20255=DIRECTION('center_axis',(0.,1.,0.));
#20256=DIRECTION('ref_axis',(1.,0.,0.));
#20257=DIRECTION('axis',(0.,0.,1.));
#20258=DIRECTION('refdir',(1.,0.,0.));
#20259=DIRECTION('center_axis',(0.,1.,0.));
#20260=DIRECTION('ref_axis',(0.,0.,1.));
#20261=DIRECTION('center_axis',(0.,-1.,0.));
#20262=DIRECTION('ref_axis',(1.,0.,0.));
#20263=DIRECTION('center_axis',(0.,-1.,0.));
#20264=DIRECTION('ref_axis',(1.,0.,0.));
#20265=DIRECTION('center_axis',(0.,-1.,0.));
#20266=DIRECTION('ref_axis',(1.,0.,0.));
#20267=DIRECTION('center_axis',(0.,-1.,0.));
#20268=DIRECTION('ref_axis',(1.,0.,0.));
#20269=DIRECTION('',(0.,1.,0.));
#20270=DIRECTION('center_axis',(0.,-1.,0.));
#20271=DIRECTION('ref_axis',(0.,0.,-1.));
#20272=DIRECTION('center_axis',(0.,-1.,0.));
#20273=DIRECTION('ref_axis',(1.,0.,0.));
#20274=DIRECTION('center_axis',(0.,-1.,0.));
#20275=DIRECTION('ref_axis',(1.,0.,0.));
#20276=DIRECTION('',(0.,1.,0.));
#20277=DIRECTION('center_axis',(0.,1.,0.));
#20278=DIRECTION('ref_axis',(0.,0.,1.));
#20279=DIRECTION('center_axis',(0.,-1.,0.));
#20280=DIRECTION('ref_axis',(1.,0.,0.));
#20281=DIRECTION('center_axis',(0.,-1.,0.));
#20282=DIRECTION('ref_axis',(1.,0.,0.));
#20283=DIRECTION('center_axis',(0.,-1.,0.));
#20284=DIRECTION('ref_axis',(1.,0.,0.));
#20285=DIRECTION('center_axis',(0.,-1.,0.));
#20286=DIRECTION('ref_axis',(1.,0.,0.));
#20287=DIRECTION('',(0.,1.,0.));
#20288=DIRECTION('center_axis',(0.,-1.,0.));
#20289=DIRECTION('ref_axis',(0.,0.,-1.));
#20290=DIRECTION('center_axis',(0.,-1.,0.));
#20291=DIRECTION('ref_axis',(1.,0.,0.));
#20292=DIRECTION('center_axis',(0.,-1.,0.));
#20293=DIRECTION('ref_axis',(1.,0.,0.));
#20294=DIRECTION('',(0.,1.,0.));
#20295=DIRECTION('',(0.,0.,1.));
#20296=DIRECTION('',(1.,0.,0.));
#20297=DIRECTION('',(0.,0.,1.));
#20298=DIRECTION('',(1.,0.,0.));
#20299=DIRECTION('',(0.,0.,1.));
#20300=DIRECTION('',(1.,0.,0.));
#20301=DIRECTION('',(0.,0.,1.));
#20302=DIRECTION('',(1.,0.,0.));
#20303=DIRECTION('',(0.,0.,1.));
#20304=DIRECTION('',(1.,0.,0.));
#20305=DIRECTION('axis',(0.,0.,1.));
#20306=DIRECTION('refdir',(1.,0.,0.));
#20307=DIRECTION('axis',(0.,0.,1.));
#20308=DIRECTION('refdir',(1.,0.,0.));
#20309=DIRECTION('center_axis',(0.,-1.,0.));
#20310=DIRECTION('ref_axis',(0.,0.,-1.));
#20311=DIRECTION('center_axis',(0.,-1.,0.));
#20312=DIRECTION('ref_axis',(1.,0.,0.));
#20313=DIRECTION('center_axis',(0.,-1.,0.));
#20314=DIRECTION('ref_axis',(1.,0.,0.));
#20315=DIRECTION('center_axis',(1.,0.,1.22464679914735E-16));
#20316=DIRECTION('ref_axis',(-1.22464679914735E-16,0.,1.));
#20317=DIRECTION('center_axis',(0.,1.,0.));
#20318=DIRECTION('ref_axis',(1.,0.,0.));
#20319=DIRECTION('center_axis',(0.,1.,0.));
#20320=DIRECTION('ref_axis',(1.,0.,0.));
#20321=DIRECTION('center_axis',(0.,-1.,0.));
#20322=DIRECTION('ref_axis',(1.,0.,0.));
#20323=DIRECTION('',(0.,1.,0.));
#20324=DIRECTION('center_axis',(0.,-1.,0.));
#20325=DIRECTION('ref_axis',(1.,0.,0.));
#20326=DIRECTION('center_axis',(0.,-1.,0.));
#20327=DIRECTION('ref_axis',(1.,0.,0.));
#20328=DIRECTION('center_axis',(0.,-1.,0.));
#20329=DIRECTION('ref_axis',(1.,0.,0.));
#20330=DIRECTION('',(0.,1.,0.));
#20331=DIRECTION('center_axis',(0.,-1.,0.));
#20332=DIRECTION('ref_axis',(1.,0.,0.));
#20333=DIRECTION('center_axis',(0.,1.,0.));
#20334=DIRECTION('ref_axis',(1.,0.,0.));
#20335=DIRECTION('',(-0.707106781186548,0.707106781186547,-8.65956056235494E-17));
#20336=DIRECTION('center_axis',(0.,-1.,0.));
#20337=DIRECTION('ref_axis',(1.,0.,0.));
#20338=DIRECTION('center_axis',(0.,1.,0.));
#20339=DIRECTION('ref_axis',(0.,0.,1.));
#20340=DIRECTION('center_axis',(0.,-1.,0.));
#20341=DIRECTION('ref_axis',(1.,0.,0.));
#20342=DIRECTION('center_axis',(0.,-1.,0.));
#20343=DIRECTION('ref_axis',(1.,0.,0.));
#20344=DIRECTION('',(0.,1.,0.));
#20345=DIRECTION('center_axis',(0.,-1.,0.));
#20346=DIRECTION('ref_axis',(0.,0.,-1.));
#20347=DIRECTION('center_axis',(0.,-1.,0.));
#20348=DIRECTION('ref_axis',(1.,0.,0.));
#20349=DIRECTION('center_axis',(0.,-1.,0.));
#20350=DIRECTION('ref_axis',(1.,0.,0.));
#20351=DIRECTION('',(0.707106781186548,0.707106781186547,8.65956056235494E-17));
#20352=DIRECTION('axis',(0.,0.,1.));
#20353=DIRECTION('refdir',(1.,0.,0.));
#20354=DIRECTION('center_axis',(0.,-1.,0.));
#20355=DIRECTION('ref_axis',(0.,0.,-1.));
#20356=DIRECTION('center_axis',(0.,-1.,0.));
#20357=DIRECTION('ref_axis',(1.,0.,0.));
#20358=DIRECTION('center_axis',(0.,-1.,0.));
#20359=DIRECTION('ref_axis',(1.,0.,0.));
#20360=DIRECTION('center_axis',(1.,0.,1.22464679914735E-16));
#20361=DIRECTION('ref_axis',(-1.22464679914735E-16,0.,1.));
#20362=DIRECTION('center_axis',(0.,1.,0.));
#20363=DIRECTION('ref_axis',(1.,0.,0.));
#20364=DIRECTION('center_axis',(0.,1.,0.));
#20365=DIRECTION('ref_axis',(1.,0.,0.));
#20366=DIRECTION('center_axis',(0.,-1.,0.));
#20367=DIRECTION('ref_axis',(1.,0.,0.));
#20368=DIRECTION('center_axis',(0.,-1.,0.));
#20369=DIRECTION('ref_axis',(1.,0.,0.));
#20370=DIRECTION('',(0.,1.,0.));
#20371=DIRECTION('center_axis',(0.,1.,0.));
#20372=DIRECTION('ref_axis',(0.,0.,1.));
#20373=DIRECTION('center_axis',(0.,-1.,0.));
#20374=DIRECTION('ref_axis',(1.,0.,0.));
#20375=DIRECTION('center_axis',(0.,-1.,0.));
#20376=DIRECTION('ref_axis',(1.,0.,0.));
#20377=DIRECTION('center_axis',(0.,-1.,0.));
#20378=DIRECTION('ref_axis',(1.,0.,0.));
#20379=DIRECTION('center_axis',(0.,-1.,0.));
#20380=DIRECTION('ref_axis',(1.,0.,0.));
#20381=DIRECTION('',(0.707106781186548,0.707106781186547,8.65956056235494E-17));
#20382=DIRECTION('center_axis',(0.,-1.,0.));
#20383=DIRECTION('ref_axis',(1.,0.,0.));
#20384=DIRECTION('center_axis',(0.,-1.,0.));
#20385=DIRECTION('ref_axis',(1.,0.,0.));
#20386=DIRECTION('',(0.,1.,0.));
#20387=DIRECTION('center_axis',(0.,1.,0.));
#20388=DIRECTION('ref_axis',(1.,0.,0.));
#20389=DIRECTION('center_axis',(0.,-1.,0.));
#20390=DIRECTION('ref_axis',(1.,0.,0.));
#20391=DIRECTION('',(-0.707106781186548,0.707106781186547,-8.65956056235494E-17));
#20392=DIRECTION('center_axis',(0.,-1.,0.));
#20393=DIRECTION('ref_axis',(0.,0.,-1.));
#20394=DIRECTION('center_axis',(0.,-1.,0.));
#20395=DIRECTION('ref_axis',(1.,0.,0.));
#20396=DIRECTION('',(0.,1.,0.));
#20397=DIRECTION('axis',(0.,0.,1.));
#20398=DIRECTION('refdir',(1.,0.,0.));
#20399=DIRECTION('center_axis',(0.,0.,1.));
#20400=DIRECTION('ref_axis',(1.,0.,0.));
#20401=DIRECTION('center_axis',(1.22464679914735E-16,-1.,0.));
#20402=DIRECTION('ref_axis',(-1.,-1.22464679914735E-16,0.));
#20403=DIRECTION('center_axis',(0.707106781186548,0.,0.707106781186548));
#20404=DIRECTION('ref_axis',(0.707106781186548,0.,-0.707106781186548));
#20405=DIRECTION('center_axis',(8.65956056235493E-17,-1.,-8.65956056235493E-17));
#20406=DIRECTION('ref_axis',(-0.707106781186548,-1.22464679914735E-16,0.707106781186548));
#20407=DIRECTION('center_axis',(1.,0.,0.));
#20408=DIRECTION('ref_axis',(6.12323399573677E-17,0.,-1.));
#20409=DIRECTION('center_axis',(7.49879891330929E-33,-1.,-1.22464679914735E-16));
#20410=DIRECTION('ref_axis',(-6.12323399573677E-17,-1.22464679914735E-16,
1.));
#20411=DIRECTION('center_axis',(0.707106781186548,0.,-0.707106781186548));
#20412=DIRECTION('ref_axis',(-0.707106781186548,0.,-0.707106781186548));
#20413=DIRECTION('center_axis',(-8.65956056235493E-17,-1.,-8.65956056235493E-17));
#20414=DIRECTION('ref_axis',(0.707106781186548,-1.22464679914735E-16,0.707106781186548));
#20415=DIRECTION('center_axis',(0.,0.,-1.));
#20416=DIRECTION('ref_axis',(-1.,0.,-1.22464679914735E-16));
#20417=DIRECTION('center_axis',(-1.22464679914735E-16,-1.,-1.49975978266186E-32));
#20418=DIRECTION('ref_axis',(1.,-1.22464679914735E-16,1.22464679914735E-16));
#20419=DIRECTION('center_axis',(-0.707106781186548,0.,-0.707106781186548));
#20420=DIRECTION('ref_axis',(-0.707106781186548,0.,0.707106781186548));
#20421=DIRECTION('center_axis',(-8.65956056235493E-17,-1.,8.65956056235493E-17));
#20422=DIRECTION('ref_axis',(0.707106781186548,-1.22464679914735E-16,-0.707106781186548));
#20423=DIRECTION('center_axis',(-1.,0.,0.));
#20424=DIRECTION('ref_axis',(-1.83697019872103E-16,0.,1.));
#20425=DIRECTION('center_axis',(-2.24963967399279E-32,-1.,1.22464679914735E-16));
#20426=DIRECTION('ref_axis',(1.83697019872103E-16,-1.22464679914735E-16,
-1.));
#20427=DIRECTION('center_axis',(-0.707106781186548,0.,0.707106781186548));
#20428=DIRECTION('ref_axis',(0.707106781186548,0.,0.707106781186548));
#20429=DIRECTION('center_axis',(8.65956056235493E-17,-1.,8.65956056235494E-17));
#20430=DIRECTION('ref_axis',(-0.707106781186548,-1.22464679914735E-16,-0.707106781186548));
#20431=DIRECTION('axis',(0.,0.,1.));
#20432=DIRECTION('refdir',(1.,0.,0.));
#20433=DIRECTION('center_axis',(0.,0.,1.));
#20434=DIRECTION('ref_axis',(1.,0.,0.));
#20435=DIRECTION('center_axis',(0.,-1.,0.));
#20436=DIRECTION('ref_axis',(0.,0.,-1.));
#20437=DIRECTION('center_axis',(0.,-1.,0.));
#20438=DIRECTION('ref_axis',(0.,0.,-1.));
#20439=DIRECTION('center_axis',(0.,1.,0.));
#20440=DIRECTION('ref_axis',(1.,0.,0.));
#20441=DIRECTION('center_axis',(0.,1.,0.));
#20442=DIRECTION('ref_axis',(1.,0.,0.));
#20443=DIRECTION('center_axis',(0.,1.,0.));
#20444=DIRECTION('ref_axis',(1.,0.,0.));
#20445=DIRECTION('center_axis',(0.,1.,0.));
#20446=DIRECTION('ref_axis',(1.,0.,0.));
#20447=DIRECTION('',(0.,-1.,0.));
#20448=DIRECTION('center_axis',(0.,-1.,0.));
#20449=DIRECTION('ref_axis',(1.,0.,0.));
#20450=DIRECTION('center_axis',(0.,1.,0.));
#20451=DIRECTION('ref_axis',(1.,0.,0.));
#20452=DIRECTION('center_axis',(0.,1.,0.));
#20453=DIRECTION('ref_axis',(1.,0.,0.));
#20454=DIRECTION('center_axis',(0.,1.,0.));
#20455=DIRECTION('ref_axis',(1.,0.,0.));
#20456=DIRECTION('center_axis',(0.,1.,0.));
#20457=DIRECTION('ref_axis',(1.,0.,0.));
#20458=DIRECTION('center_axis',(0.,1.,0.));
#20459=DIRECTION('ref_axis',(1.,0.,0.));
#20460=DIRECTION('center_axis',(0.,1.,0.));
#20461=DIRECTION('ref_axis',(1.,0.,0.));
#20462=DIRECTION('center_axis',(0.,-1.,0.));
#20463=DIRECTION('ref_axis',(1.,0.,0.));
#20464=DIRECTION('center_axis',(0.,-1.,0.));
#20465=DIRECTION('ref_axis',(0.,0.,-1.));
#20466=DIRECTION('center_axis',(6.12323399573677E-17,0.,1.));
#20467=DIRECTION('ref_axis',(1.,0.,0.));
#20468=DIRECTION('center_axis',(0.,-1.,0.));
#20469=DIRECTION('ref_axis',(0.,0.,-1.));
#20470=DIRECTION('center_axis',(0.,1.,0.));
#20471=DIRECTION('ref_axis',(1.,0.,0.));
#20472=DIRECTION('center_axis',(0.,-1.,0.));
#20473=DIRECTION('ref_axis',(1.,0.,0.));
#20474=DIRECTION('center_axis',(0.,-1.,0.));
#20475=DIRECTION('ref_axis',(0.,0.,-1.));
#20476=DIRECTION('center_axis',(0.,0.,1.));
#20477=DIRECTION('ref_axis',(1.,0.,0.));
#20478=DIRECTION('center_axis',(0.,-1.,0.));
#20479=DIRECTION('ref_axis',(0.,0.,-1.));
#20480=DIRECTION('center_axis',(0.,1.,0.));
#20481=DIRECTION('ref_axis',(1.,0.,0.));
#20482=DIRECTION('center_axis',(0.,-1.,0.));
#20483=DIRECTION('ref_axis',(1.,0.,0.));
#20484=DIRECTION('center_axis',(0.,-1.,0.));
#20485=DIRECTION('ref_axis',(0.,0.,-1.));
#20486=DIRECTION('center_axis',(0.,0.,1.));
#20487=DIRECTION('ref_axis',(1.,0.,0.));
#20488=DIRECTION('center_axis',(0.,-1.,0.));
#20489=DIRECTION('ref_axis',(0.,0.,-1.));
#20490=DIRECTION('center_axis',(0.,1.,0.));
#20491=DIRECTION('ref_axis',(1.,0.,0.));
#20492=DIRECTION('center_axis',(0.,-1.,0.));
#20493=DIRECTION('ref_axis',(1.,0.,0.));
#20494=DIRECTION('center_axis',(0.,-1.,0.));
#20495=DIRECTION('ref_axis',(0.,0.,-1.));
#20496=DIRECTION('center_axis',(0.,0.,1.));
#20497=DIRECTION('ref_axis',(1.,0.,0.));
#20498=DIRECTION('center_axis',(0.,-1.,0.));
#20499=DIRECTION('ref_axis',(0.,0.,-1.));
#20500=DIRECTION('center_axis',(0.,1.,0.));
#20501=DIRECTION('ref_axis',(1.,0.,0.));
#20502=DIRECTION('center_axis',(0.,-1.,0.));
#20503=DIRECTION('ref_axis',(1.,0.,0.));
#20504=DIRECTION('center_axis',(0.,-1.,0.));
#20505=DIRECTION('ref_axis',(0.,0.,-1.));
#20506=DIRECTION('center_axis',(6.12323399573676E-17,0.,1.));
#20507=DIRECTION('ref_axis',(1.,0.,0.));
#20508=DIRECTION('center_axis',(0.,-1.,0.));
#20509=DIRECTION('ref_axis',(0.,0.,-1.));
#20510=DIRECTION('center_axis',(0.,1.,0.));
#20511=DIRECTION('ref_axis',(1.,0.,0.));
#20512=DIRECTION('center_axis',(0.,-1.,0.));
#20513=DIRECTION('ref_axis',(1.,0.,0.));
#20514=DIRECTION('center_axis',(0.,-1.,0.));
#20515=DIRECTION('ref_axis',(0.,0.,-1.));
#20516=DIRECTION('center_axis',(0.,0.,1.));
#20517=DIRECTION('ref_axis',(1.,0.,0.));
#20518=DIRECTION('center_axis',(0.,-1.,0.));
#20519=DIRECTION('ref_axis',(0.,0.,-1.));
#20520=DIRECTION('center_axis',(0.,1.,0.));
#20521=DIRECTION('ref_axis',(1.,0.,0.));
#20522=DIRECTION('center_axis',(0.,1.,0.));
#20523=DIRECTION('ref_axis',(1.,0.,0.));
#20524=DIRECTION('',(0.,1.,0.));
#20525=DIRECTION('center_axis',(0.,-1.,0.));
#20526=DIRECTION('ref_axis',(1.,0.,0.));
#20527=DIRECTION('center_axis',(0.,-1.,0.));
#20528=DIRECTION('ref_axis',(1.,0.,0.));
#20529=DIRECTION('center_axis',(0.,1.,0.));
#20530=DIRECTION('ref_axis',(1.,0.,0.));
#20531=DIRECTION('center_axis',(0.,-1.,0.));
#20532=DIRECTION('ref_axis',(0.,0.,-1.));
#20533=DIRECTION('center_axis',(0.,0.,1.));
#20534=DIRECTION('ref_axis',(1.,0.,0.));
#20535=DIRECTION('center_axis',(0.,-1.,0.));
#20536=DIRECTION('ref_axis',(0.,0.,-1.));
#20537=DIRECTION('center_axis',(0.,-1.,0.));
#20538=DIRECTION('ref_axis',(-1.,0.,0.));
#20539=DIRECTION('center_axis',(0.,1.,0.));
#20540=DIRECTION('ref_axis',(1.,0.,0.));
#20541=DIRECTION('axis',(0.,0.,1.));
#20542=DIRECTION('refdir',(1.,0.,0.));
#20543=DIRECTION('center_axis',(0.,1.,0.));
#20544=DIRECTION('ref_axis',(0.,0.,1.));
#20545=DIRECTION('center_axis',(0.,-1.,0.));
#20546=DIRECTION('ref_axis',(1.,0.,0.));
#20547=DIRECTION('center_axis',(0.,-1.,0.));
#20548=DIRECTION('ref_axis',(1.,0.,0.));
#20549=DIRECTION('center_axis',(0.,-1.,0.));
#20550=DIRECTION('ref_axis',(1.,0.,0.));
#20551=DIRECTION('center_axis',(0.,-1.,0.));
#20552=DIRECTION('ref_axis',(1.,0.,0.));
#20553=DIRECTION('',(0.,1.,0.));
#20554=DIRECTION('center_axis',(0.,-1.,0.));
#20555=DIRECTION('ref_axis',(0.,0.,-1.));
#20556=DIRECTION('center_axis',(0.,-1.,0.));
#20557=DIRECTION('ref_axis',(1.,0.,0.));
#20558=DIRECTION('center_axis',(0.,-1.,0.));
#20559=DIRECTION('ref_axis',(1.,0.,0.));
#20560=DIRECTION('',(0.,1.,0.));
#20561=DIRECTION('center_axis',(0.,1.,0.));
#20562=DIRECTION('ref_axis',(0.,0.,1.));
#20563=DIRECTION('center_axis',(0.,-1.,0.));
#20564=DIRECTION('ref_axis',(1.,0.,0.));
#20565=DIRECTION('center_axis',(0.,-1.,0.));
#20566=DIRECTION('ref_axis',(1.,0.,0.));
#20567=DIRECTION('center_axis',(0.,-1.,0.));
#20568=DIRECTION('ref_axis',(1.,0.,0.));
#20569=DIRECTION('center_axis',(0.,-1.,0.));
#20570=DIRECTION('ref_axis',(1.,0.,0.));
#20571=DIRECTION('',(0.,1.,0.));
#20572=DIRECTION('center_axis',(0.,-1.,0.));
#20573=DIRECTION('ref_axis',(0.,0.,-1.));
#20574=DIRECTION('center_axis',(0.,-1.,0.));
#20575=DIRECTION('ref_axis',(1.,0.,0.));
#20576=DIRECTION('center_axis',(0.,-1.,0.));
#20577=DIRECTION('ref_axis',(1.,0.,0.));
#20578=DIRECTION('',(0.,1.,0.));
#20579=DIRECTION('',(0.,0.,1.));
#20580=DIRECTION('',(1.,0.,0.));
#20581=DIRECTION('',(0.,0.,1.));
#20582=DIRECTION('',(1.,0.,0.));
#20583=DIRECTION('',(0.,0.,1.));
#20584=DIRECTION('',(1.,0.,0.));
#20585=DIRECTION('',(0.,0.,1.));
#20586=DIRECTION('',(1.,0.,0.));
#20587=DIRECTION('',(0.,0.,1.));
#20588=DIRECTION('',(1.,0.,0.));
#20589=DIRECTION('axis',(0.,0.,1.));
#20590=DIRECTION('refdir',(1.,0.,0.));
#20591=DIRECTION('center_axis',(0.,1.,0.));
#20592=DIRECTION('ref_axis',(0.,0.,1.));
#20593=DIRECTION('center_axis',(0.,-1.,0.));
#20594=DIRECTION('ref_axis',(1.,0.,0.));
#20595=DIRECTION('center_axis',(0.,-1.,0.));
#20596=DIRECTION('ref_axis',(1.,0.,0.));
#20597=DIRECTION('center_axis',(0.,-1.,0.));
#20598=DIRECTION('ref_axis',(1.,0.,0.));
#20599=DIRECTION('',(0.707106781186547,0.707106781186548,8.65956056235493E-17));
#20600=DIRECTION('center_axis',(0.,-1.,0.));
#20601=DIRECTION('ref_axis',(1.,0.,0.));
#20602=DIRECTION('center_axis',(0.,-1.,0.));
#20603=DIRECTION('ref_axis',(1.,0.,0.));
#20604=DIRECTION('',(0.,1.,0.));
#20605=DIRECTION('center_axis',(0.,1.,0.));
#20606=DIRECTION('ref_axis',(1.,0.,0.));
#20607=DIRECTION('center_axis',(0.,-1.,0.));
#20608=DIRECTION('ref_axis',(1.,0.,0.));
#20609=DIRECTION('',(-0.707106781186547,0.707106781186548,-8.65956056235493E-17));
#20610=DIRECTION('center_axis',(0.,-1.,0.));
#20611=DIRECTION('ref_axis',(0.,0.,-1.));
#20612=DIRECTION('center_axis',(0.,-1.,0.));
#20613=DIRECTION('ref_axis',(1.,0.,0.));
#20614=DIRECTION('center_axis',(0.,1.,0.));
#20615=DIRECTION('ref_axis',(1.,0.,0.));
#20616=DIRECTION('center_axis',(0.,1.,0.));
#20617=DIRECTION('ref_axis',(1.,0.,0.));
#20618=DIRECTION('',(-0.447213595499958,0.894427190999916,-5.47678698264203E-17));
#20619=DIRECTION('center_axis',(0.,-1.,0.));
#20620=DIRECTION('ref_axis',(1.,0.,0.));
#20621=DIRECTION('center_axis',(0.,1.,0.));
#20622=DIRECTION('ref_axis',(1.,0.,0.));
#20623=DIRECTION('',(0.,1.,0.));
#20624=DIRECTION('center_axis',(0.,1.,0.));
#20625=DIRECTION('ref_axis',(1.,0.,0.));
#20626=DIRECTION('center_axis',(0.,-1.,0.));
#20627=DIRECTION('ref_axis',(1.,0.,0.));
#20628=DIRECTION('',(-0.707106781186547,0.707106781186548,-8.65956056235493E-17));
#20629=DIRECTION('center_axis',(0.,-1.,0.));
#20630=DIRECTION('ref_axis',(0.,0.,-1.));
#20631=DIRECTION('center_axis',(0.866025403784439,0.,-0.5));
#20632=DIRECTION('ref_axis',(0.5,0.,0.866025403784439));
#20633=DIRECTION('',(-0.5,0.,-0.866025403784439));
#20634=DIRECTION('',(0.,-1.,0.));
#20635=DIRECTION('',(0.5,0.,0.866025403784439));
#20636=DIRECTION('',(0.,-1.,0.));
#20637=DIRECTION('center_axis',(1.60246890531964E-16,0.,-1.));
#20638=DIRECTION('ref_axis',(1.,0.,1.60246890531964E-16));
#20639=DIRECTION('',(-1.,0.,-1.60246890531964E-16));
#20640=DIRECTION('',(0.,-1.,0.));
#20641=DIRECTION('',(1.,0.,1.60246890531964E-16));
#20642=DIRECTION('center_axis',(-0.866025403784439,0.,-0.5));
#20643=DIRECTION('ref_axis',(0.5,0.,-0.866025403784439));
#20644=DIRECTION('',(-0.5,0.,0.866025403784439));
#20645=DIRECTION('',(0.,-1.,0.));
#20646=DIRECTION('',(0.5,0.,-0.866025403784439));
#20647=DIRECTION('center_axis',(-0.866025403784439,0.,0.5));
#20648=DIRECTION('ref_axis',(-0.5,0.,-0.866025403784439));
#20649=DIRECTION('',(0.5,0.,0.866025403784439));
#20650=DIRECTION('',(0.,-1.,0.));
#20651=DIRECTION('',(-0.5,0.,-0.866025403784439));
#20652=DIRECTION('center_axis',(-1.60246890531964E-16,0.,1.));
#20653=DIRECTION('ref_axis',(-1.,0.,-1.60246890531964E-16));
#20654=DIRECTION('',(1.,0.,1.60246890531964E-16));
#20655=DIRECTION('',(0.,-1.,0.));
#20656=DIRECTION('',(-1.,0.,-1.60246890531964E-16));
#20657=DIRECTION('center_axis',(0.866025403784439,0.,0.5));
#20658=DIRECTION('ref_axis',(-0.5,0.,0.866025403784439));
#20659=DIRECTION('',(0.5,0.,-0.866025403784439));
#20660=DIRECTION('',(-0.5,0.,0.866025403784439));
#20661=DIRECTION('center_axis',(0.,1.,0.));
#20662=DIRECTION('ref_axis',(1.,0.,0.));
#20663=DIRECTION('center_axis',(0.,-1.,0.));
#20664=DIRECTION('ref_axis',(0.,0.,-1.));
#20665=DIRECTION('',(0.,0.,1.));
#20666=DIRECTION('',(1.,0.,0.));
#20667=DIRECTION('',(0.,0.,1.));
#20668=DIRECTION('',(1.,0.,0.));
#20669=DIRECTION('',(0.,0.,1.));
#20670=DIRECTION('',(1.,0.,0.));
#20671=DIRECTION('',(0.,0.,1.));
#20672=DIRECTION('',(1.,0.,0.));
#20673=DIRECTION('',(0.,0.,1.));
#20674=DIRECTION('',(1.,0.,0.));
#20675=DIRECTION('',(0.,0.,1.));
#20676=DIRECTION('',(1.,0.,0.));
#20677=DIRECTION('',(0.,0.,1.));
#20678=DIRECTION('',(1.,0.,0.));
#20679=DIRECTION('',(0.,0.,1.));
#20680=DIRECTION('',(1.,0.,0.));
#20681=DIRECTION('',(0.,0.,1.));
#20682=DIRECTION('',(1.,0.,0.));
#20683=DIRECTION('',(0.,0.,1.));
#20684=DIRECTION('',(1.,0.,0.));
#20685=DIRECTION('',(0.,0.,1.));
#20686=DIRECTION('',(1.,0.,0.));
#20687=DIRECTION('',(0.,0.,1.));
#20688=DIRECTION('',(1.,0.,0.));
#20689=DIRECTION('',(0.,0.,1.));
#20690=DIRECTION('',(1.,0.,0.));
#20691=DIRECTION('',(0.,0.,1.));
#20692=DIRECTION('',(1.,0.,0.));
#20693=DIRECTION('',(0.,0.,1.));
#20694=DIRECTION('',(1.,0.,0.));
#20695=DIRECTION('',(0.,0.,1.));
#20696=DIRECTION('',(1.,0.,0.));
#20697=DIRECTION('',(0.,-1.,2.22044604925031E-16));
#20698=DIRECTION('',(1.,0.,0.));
#20699=DIRECTION('',(0.,-1.,2.22044604925031E-16));
#20700=DIRECTION('',(1.,0.,0.));
#20701=DIRECTION('',(0.,-1.,2.22044604925031E-16));
#20702=DIRECTION('',(1.,0.,0.));
#20703=DIRECTION('',(0.,-1.,2.22044604925031E-16));
#20704=DIRECTION('',(1.,0.,0.));
#20705=DIRECTION('',(0.,-1.,2.22044604925031E-16));
#20706=DIRECTION('',(1.,0.,0.));
#20707=DIRECTION('',(0.,-1.,2.22044604925031E-16));
#20708=DIRECTION('',(1.,0.,0.));
#20709=DIRECTION('',(0.,-1.,2.22044604925031E-16));
#20710=DIRECTION('',(1.,0.,0.));
#20711=DIRECTION('',(0.,-1.,2.22044604925031E-16));
#20712=DIRECTION('',(1.,0.,0.));
#20713=DIRECTION('',(0.,-1.,2.22044604925031E-16));
#20714=DIRECTION('',(1.,0.,0.));
#20715=DIRECTION('',(0.,-1.,2.22044604925031E-16));
#20716=DIRECTION('',(1.,0.,0.));
#20717=DIRECTION('',(0.,0.,1.));
#20718=DIRECTION('',(1.,0.,0.));
#20719=DIRECTION('',(0.,0.,1.));
#20720=DIRECTION('',(1.,0.,0.));
#20721=DIRECTION('',(0.,0.,1.));
#20722=DIRECTION('',(-1.,1.22464679914735E-16,0.));
#20723=DIRECTION('',(0.,0.,1.));
#20724=DIRECTION('',(-1.,1.22464679914735E-16,0.));
#20725=DIRECTION('',(0.,0.,1.));
#20726=DIRECTION('',(-1.,1.22464679914735E-16,0.));
#20727=DIRECTION('',(0.,0.,1.));
#20728=DIRECTION('',(-1.,1.22464679914735E-16,0.));
#20729=DIRECTION('',(0.,0.,1.));
#20730=DIRECTION('',(1.,0.,0.));
#20731=DIRECTION('',(0.,0.,1.));
#20732=DIRECTION('',(1.,0.,0.));
#20733=DIRECTION('',(0.,0.,1.));
#20734=DIRECTION('',(1.,0.,0.));
#20735=DIRECTION('',(0.,0.,1.));
#20736=DIRECTION('',(1.,0.,0.));
#20737=DIRECTION('',(0.,0.,1.));
#20738=DIRECTION('',(1.,0.,0.));
#20739=DIRECTION('',(0.,0.,1.));
#20740=DIRECTION('',(1.,0.,0.));
#20741=DIRECTION('',(0.,0.,1.));
#20742=DIRECTION('',(-1.,1.22464679914735E-16,0.));
#20743=DIRECTION('',(0.,0.,1.));
#20744=DIRECTION('',(-1.,1.22464679914735E-16,0.));
#20745=DIRECTION('',(0.,0.,1.));
#20746=DIRECTION('',(-1.,1.22464679914735E-16,0.));
#20747=DIRECTION('',(0.,0.,1.));
#20748=DIRECTION('',(-1.,1.22464679914735E-16,0.));
#20749=DIRECTION('',(0.,0.,1.));
#20750=DIRECTION('',(1.,0.,0.));
#20751=DIRECTION('',(0.,0.,1.));
#20752=DIRECTION('',(1.,0.,0.));
#20753=DIRECTION('',(0.,0.,1.));
#20754=DIRECTION('',(1.,0.,0.));
#20755=DIRECTION('',(0.,0.,1.));
#20756=DIRECTION('',(1.,0.,0.));
#20757=DIRECTION('',(0.,0.,1.));
#20758=DIRECTION('',(1.,0.,0.));
#20759=DIRECTION('',(0.,0.,1.));
#20760=DIRECTION('',(1.,0.,0.));
#20761=DIRECTION('',(0.,0.,1.));
#20762=DIRECTION('',(-1.,1.22464679914735E-16,0.));
#20763=DIRECTION('',(0.,0.,1.));
#20764=DIRECTION('',(-1.,1.22464679914735E-16,0.));
#20765=DIRECTION('',(0.,0.,1.));
#20766=DIRECTION('',(-1.,1.22464679914735E-16,0.));
#20767=DIRECTION('',(0.,0.,1.));
#20768=DIRECTION('',(-1.,1.22464679914735E-16,0.));
#20769=DIRECTION('',(0.,0.,1.));
#20770=DIRECTION('',(1.,0.,0.));
#20771=DIRECTION('',(0.,0.,1.));
#20772=DIRECTION('',(1.,0.,0.));
#20773=DIRECTION('',(0.,0.,1.));
#20774=DIRECTION('',(1.,0.,0.));
#20775=DIRECTION('',(0.,0.,1.));
#20776=DIRECTION('',(1.,0.,0.));
#20777=DIRECTION('',(0.,-1.,2.22044604925031E-16));
#20778=DIRECTION('',(1.,0.,0.));
#20779=DIRECTION('',(0.,-1.,2.22044604925031E-16));
#20780=DIRECTION('',(1.,0.,0.));
#20781=DIRECTION('',(0.,-1.,2.22044604925031E-16));
#20782=DIRECTION('',(1.,0.,0.));
#20783=DIRECTION('',(0.,-1.,2.22044604925031E-16));
#20784=DIRECTION('',(1.,0.,0.));
#20785=DIRECTION('axis',(0.,0.,1.));
#20786=DIRECTION('refdir',(1.,0.,0.));
#20787=DIRECTION('axis',(0.,0.,1.));
#20788=DIRECTION('refdir',(1.,0.,0.));
#20789=DIRECTION('center_axis',(-1.,0.,0.));
#20790=DIRECTION('ref_axis',(0.,0.,1.));
#20791=DIRECTION('',(0.,-1.,0.));
#20792=DIRECTION('',(0.,0.,1.));
#20793=DIRECTION('',(0.,1.,0.));
#20794=DIRECTION('',(0.,0.,-1.));
#20795=DIRECTION('center_axis',(0.,1.,0.));
#20796=DIRECTION('ref_axis',(1.,0.,0.));
#20797=DIRECTION('center_axis',(0.,-1.,0.));
#20798=DIRECTION('ref_axis',(1.,0.,0.));
#20799=DIRECTION('',(-1.,0.,0.));
#20800=DIRECTION('',(0.,0.,1.));
#20801=DIRECTION('center_axis',(1.,0.,0.));
#20802=DIRECTION('ref_axis',(0.,0.,-1.));
#20803=DIRECTION('',(0.,1.,0.));
#20804=DIRECTION('',(0.,1.,0.));
#20805=DIRECTION('',(0.,0.,-1.));
#20806=DIRECTION('center_axis',(0.,0.,1.));
#20807=DIRECTION('ref_axis',(1.,0.,0.));
#20808=DIRECTION('',(1.,0.,0.));
#20809=DIRECTION('center_axis',(0.,1.,0.));
#20810=DIRECTION('ref_axis',(0.,0.,1.));
#20811=DIRECTION('center_axis',(0.,1.,0.));
#20812=DIRECTION('ref_axis',(1.,0.,0.));
#20813=DIRECTION('center_axis',(0.,1.,0.));
#20814=DIRECTION('ref_axis',(1.,0.,0.));
#20815=DIRECTION('center_axis',(0.,1.,0.));
#20816=DIRECTION('ref_axis',(1.,0.,0.));
#20817=DIRECTION('',(0.,-1.,0.));
#20818=DIRECTION('center_axis',(0.,1.,0.));
#20819=DIRECTION('ref_axis',(1.,0.,0.));
#20820=DIRECTION('center_axis',(0.,1.,0.));
#20821=DIRECTION('ref_axis',(1.,0.,0.));
#20822=DIRECTION('center_axis',(0.,1.,0.));
#20823=DIRECTION('ref_axis',(1.,0.,0.));
#20824=DIRECTION('axis',(0.,0.,1.));
#20825=DIRECTION('refdir',(1.,0.,0.));
#20826=DIRECTION('center_axis',(0.,0.,1.));
#20827=DIRECTION('ref_axis',(1.,0.,0.));
#20828=DIRECTION('',(0.,1.,0.));
#20829=DIRECTION('center_axis',(0.,0.,1.));
#20830=DIRECTION('ref_axis',(1.,0.,0.));
#20831=DIRECTION('center_axis',(0.,0.,1.));
#20832=DIRECTION('ref_axis',(1.,0.,0.));
#20833=DIRECTION('center_axis',(0.,0.,1.));
#20834=DIRECTION('ref_axis',(1.,0.,0.));
#20835=DIRECTION('',(0.,0.,1.));
#20836=DIRECTION('center_axis',(0.,0.,1.));
#20837=DIRECTION('ref_axis',(1.,0.,0.));
#20838=DIRECTION('center_axis',(0.,0.,1.));
#20839=DIRECTION('ref_axis',(1.,0.,0.));
#20840=DIRECTION('',(0.,-1.,0.));
#20841=DIRECTION('center_axis',(0.,1.,0.));
#20842=DIRECTION('ref_axis',(1.,0.,0.));
#20843=DIRECTION('center_axis',(0.,-1.,0.));
#20844=DIRECTION('ref_axis',(1.,0.,0.));
#20845=DIRECTION('',(0.,-1.,0.));
#20846=DIRECTION('center_axis',(0.,-1.,0.));
#20847=DIRECTION('ref_axis',(1.,0.,0.));
#20848=DIRECTION('center_axis',(0.,1.,0.));
#20849=DIRECTION('ref_axis',(1.,0.,0.));
#20850=DIRECTION('center_axis',(0.,1.,0.));
#20851=DIRECTION('ref_axis',(1.,0.,0.));
#20852=DIRECTION('',(0.,-1.,0.));
#20853=DIRECTION('center_axis',(0.,1.,0.));
#20854=DIRECTION('ref_axis',(1.,0.,0.));
#20855=DIRECTION('center_axis',(0.,1.,0.));
#20856=DIRECTION('ref_axis',(1.,0.,0.));
#20857=DIRECTION('center_axis',(0.,1.,0.));
#20858=DIRECTION('ref_axis',(1.,0.,0.));
#20859=DIRECTION('axis',(0.,0.,1.));
#20860=DIRECTION('refdir',(1.,0.,0.));
#20861=DIRECTION('center_axis',(0.,0.,1.));
#20862=DIRECTION('ref_axis',(1.,0.,0.));
#20863=DIRECTION('',(0.,1.,0.));
#20864=DIRECTION('center_axis',(0.,0.,1.));
#20865=DIRECTION('ref_axis',(1.,0.,0.));
#20866=DIRECTION('center_axis',(0.,0.,1.));
#20867=DIRECTION('ref_axis',(1.,0.,0.));
#20868=DIRECTION('center_axis',(0.,0.,1.));
#20869=DIRECTION('ref_axis',(1.,0.,0.));
#20870=DIRECTION('',(0.,0.,1.));
#20871=DIRECTION('center_axis',(0.,0.,1.));
#20872=DIRECTION('ref_axis',(1.,0.,0.));
#20873=DIRECTION('center_axis',(0.,0.,1.));
#20874=DIRECTION('ref_axis',(1.,0.,0.));
#20875=DIRECTION('',(0.,-1.,0.));
#20876=DIRECTION('center_axis',(0.,1.,0.));
#20877=DIRECTION('ref_axis',(1.,0.,0.));
#20878=DIRECTION('center_axis',(0.,-1.,0.));
#20879=DIRECTION('ref_axis',(1.,0.,0.));
#20880=DIRECTION('',(0.,-1.,0.));
#20881=DIRECTION('center_axis',(0.,-1.,0.));
#20882=DIRECTION('ref_axis',(1.,0.,0.));
#20883=DIRECTION('center_axis',(0.,1.,0.));
#20884=DIRECTION('ref_axis',(1.,0.,0.));
#20885=DIRECTION('center_axis',(0.,1.,0.));
#20886=DIRECTION('ref_axis',(1.,0.,0.));
#20887=DIRECTION('',(0.,-1.,0.));
#20888=DIRECTION('center_axis',(0.,1.,0.));
#20889=DIRECTION('ref_axis',(1.,0.,0.));
#20890=DIRECTION('center_axis',(0.,1.,0.));
#20891=DIRECTION('ref_axis',(1.,0.,0.));
#20892=DIRECTION('center_axis',(0.,1.,0.));
#20893=DIRECTION('ref_axis',(1.,0.,0.));
#20894=DIRECTION('axis',(0.,0.,1.));
#20895=DIRECTION('refdir',(1.,0.,0.));
#20896=DIRECTION('center_axis',(0.,1.,0.));
#20897=DIRECTION('ref_axis',(1.,0.,0.));
#20898=DIRECTION('center_axis',(0.,-1.,0.));
#20899=DIRECTION('ref_axis',(1.,0.,0.));
#20900=DIRECTION('',(0.,-1.,0.));
#20901=DIRECTION('center_axis',(0.,-1.,0.));
#20902=DIRECTION('ref_axis',(1.,0.,0.));
#20903=DIRECTION('center_axis',(0.,1.,0.));
#20904=DIRECTION('ref_axis',(1.,0.,0.));
#20905=DIRECTION('center_axis',(0.,1.,0.));
#20906=DIRECTION('ref_axis',(1.,0.,0.));
#20907=DIRECTION('',(0.,-1.,0.));
#20908=DIRECTION('center_axis',(0.,1.,0.));
#20909=DIRECTION('ref_axis',(1.,0.,0.));
#20910=DIRECTION('center_axis',(0.,1.,0.));
#20911=DIRECTION('ref_axis',(1.,0.,0.));
#20912=DIRECTION('center_axis',(0.,1.,0.));
#20913=DIRECTION('ref_axis',(1.,0.,0.));
#20914=DIRECTION('axis',(0.,0.,1.));
#20915=DIRECTION('refdir',(1.,0.,0.));
#20916=DIRECTION('center_axis',(0.,1.,0.));
#20917=DIRECTION('ref_axis',(1.,0.,0.));
#20918=DIRECTION('center_axis',(0.,-1.,0.));
#20919=DIRECTION('ref_axis',(1.,0.,0.));
#20920=DIRECTION('',(0.,-1.,0.));
#20921=DIRECTION('center_axis',(0.,-1.,0.));
#20922=DIRECTION('ref_axis',(1.,0.,0.));
#20923=DIRECTION('center_axis',(0.,1.,0.));
#20924=DIRECTION('ref_axis',(1.,0.,0.));
#20925=DIRECTION('center_axis',(0.,1.,0.));
#20926=DIRECTION('ref_axis',(1.,0.,0.));
#20927=DIRECTION('',(0.,-1.,0.));
#20928=DIRECTION('center_axis',(0.,1.,0.));
#20929=DIRECTION('ref_axis',(1.,0.,0.));
#20930=DIRECTION('center_axis',(0.,1.,0.));
#20931=DIRECTION('ref_axis',(1.,0.,0.));
#20932=DIRECTION('center_axis',(0.,1.,0.));
#20933=DIRECTION('ref_axis',(1.,0.,0.));
#20934=DIRECTION('axis',(0.,0.,1.));
#20935=DIRECTION('refdir',(1.,0.,0.));
#20936=DIRECTION('center_axis',(0.,1.,0.));
#20937=DIRECTION('ref_axis',(1.,0.,0.));
#20938=DIRECTION('center_axis',(0.,-1.,0.));
#20939=DIRECTION('ref_axis',(1.,0.,0.));
#20940=DIRECTION('',(0.,-1.,0.));
#20941=DIRECTION('center_axis',(0.,-1.,0.));
#20942=DIRECTION('ref_axis',(1.,0.,0.));
#20943=DIRECTION('center_axis',(0.,1.,0.));
#20944=DIRECTION('ref_axis',(1.,0.,0.));
#20945=DIRECTION('center_axis',(0.,1.,0.));
#20946=DIRECTION('ref_axis',(1.,0.,0.));
#20947=DIRECTION('',(0.,-1.,0.));
#20948=DIRECTION('center_axis',(0.,1.,0.));
#20949=DIRECTION('ref_axis',(1.,0.,0.));
#20950=DIRECTION('center_axis',(0.,1.,0.));
#20951=DIRECTION('ref_axis',(1.,0.,0.));
#20952=DIRECTION('center_axis',(0.,1.,0.));
#20953=DIRECTION('ref_axis',(1.,0.,0.));
#20954=DIRECTION('axis',(0.,0.,1.));
#20955=DIRECTION('refdir',(1.,0.,0.));
#20956=DIRECTION('center_axis',(0.,1.,0.));
#20957=DIRECTION('ref_axis',(1.,0.,0.));
#20958=DIRECTION('center_axis',(0.,-1.,0.));
#20959=DIRECTION('ref_axis',(1.,0.,0.));
#20960=DIRECTION('',(0.,-1.,0.));
#20961=DIRECTION('center_axis',(0.,-1.,0.));
#20962=DIRECTION('ref_axis',(1.,0.,0.));
#20963=DIRECTION('center_axis',(0.,1.,0.));
#20964=DIRECTION('ref_axis',(1.,0.,0.));
#20965=DIRECTION('center_axis',(0.,1.,0.));
#20966=DIRECTION('ref_axis',(1.,0.,0.));
#20967=DIRECTION('',(0.,-1.,0.));
#20968=DIRECTION('center_axis',(0.,1.,0.));
#20969=DIRECTION('ref_axis',(1.,0.,0.));
#20970=DIRECTION('center_axis',(0.,1.,0.));
#20971=DIRECTION('ref_axis',(1.,0.,0.));
#20972=DIRECTION('center_axis',(0.,1.,0.));
#20973=DIRECTION('ref_axis',(1.,0.,0.));
#20974=DIRECTION('axis',(0.,0.,1.));
#20975=DIRECTION('refdir',(1.,0.,0.));
#20976=DIRECTION('center_axis',(1.,0.,0.));
#20977=DIRECTION('ref_axis',(0.,0.,-1.));
#20978=DIRECTION('',(0.,0.,1.));
#20979=DIRECTION('',(0.,1.,0.));
#20980=DIRECTION('',(0.,0.,-1.));
#20981=DIRECTION('',(0.,-1.,0.));
#20982=DIRECTION('center_axis',(0.,0.,-1.));
#20983=DIRECTION('ref_axis',(-1.,0.,0.));
#20984=DIRECTION('',(1.,0.,0.));
#20985=DIRECTION('',(0.,-1.,0.));
#20986=DIRECTION('',(-1.,0.,0.));
#20987=DIRECTION('center_axis',(-1.,0.,0.));
#20988=DIRECTION('ref_axis',(0.,0.,1.));
#20989=DIRECTION('',(0.,0.,-1.));
#20990=DIRECTION('',(0.,1.,0.));
#20991=DIRECTION('',(0.,0.,1.));
#20992=DIRECTION('center_axis',(0.,1.,0.));
#20993=DIRECTION('ref_axis',(1.,0.,0.));
#20994=DIRECTION('center_axis',(0.,-1.,0.));
#20995=DIRECTION('ref_axis',(1.,0.,0.));
#20996=DIRECTION('',(-0.587785252292473,0.,0.809016994374947));
#20997=DIRECTION('center_axis',(0.,-1.,0.));
#20998=DIRECTION('ref_axis',(1.,0.,0.));
#20999=DIRECTION('',(-0.809016994374948,0.,0.587785252292473));
#21000=DIRECTION('center_axis',(0.,-1.,0.));
#21001=DIRECTION('ref_axis',(1.,0.,0.));
#21002=DIRECTION('',(-0.951056516295154,0.,0.309016994374947));
#21003=DIRECTION('center_axis',(0.,-1.,0.));
#21004=DIRECTION('ref_axis',(1.,0.,0.));
#21005=DIRECTION('',(-1.,0.,-1.83697019872103E-16));
#21006=DIRECTION('center_axis',(0.,-1.,0.));
#21007=DIRECTION('ref_axis',(1.,0.,0.));
#21008=DIRECTION('',(-0.951056516295154,0.,-0.309016994374948));
#21009=DIRECTION('center_axis',(0.,-1.,0.));
#21010=DIRECTION('ref_axis',(1.,0.,0.));
#21011=DIRECTION('',(-0.809016994374947,0.,-0.587785252292473));
#21012=DIRECTION('center_axis',(0.,-1.,0.));
#21013=DIRECTION('ref_axis',(1.,0.,0.));
#21014=DIRECTION('',(-0.587785252292473,0.,-0.809016994374948));
#21015=DIRECTION('center_axis',(0.,-1.,0.));
#21016=DIRECTION('ref_axis',(1.,0.,0.));
#21017=DIRECTION('',(-0.309016994374947,0.,-0.951056516295154));
#21018=DIRECTION('center_axis',(0.,-1.,0.));
#21019=DIRECTION('ref_axis',(1.,0.,0.));
#21020=DIRECTION('',(1.22464679914735E-16,0.,-1.));
#21021=DIRECTION('center_axis',(0.,-1.,0.));
#21022=DIRECTION('ref_axis',(1.,0.,0.));
#21023=DIRECTION('',(0.309016994374948,0.,-0.951056516295154));
#21024=DIRECTION('center_axis',(0.,-1.,0.));
#21025=DIRECTION('ref_axis',(1.,0.,0.));
#21026=DIRECTION('',(0.587785252292473,0.,-0.809016994374947));
#21027=DIRECTION('center_axis',(0.,-1.,0.));
#21028=DIRECTION('ref_axis',(1.,0.,0.));
#21029=DIRECTION('',(0.809016994374948,0.,-0.587785252292473));
#21030=DIRECTION('center_axis',(0.,-1.,0.));
#21031=DIRECTION('ref_axis',(1.,0.,0.));
#21032=DIRECTION('',(0.951056516295154,0.,-0.309016994374947));
#21033=DIRECTION('center_axis',(0.,-1.,0.));
#21034=DIRECTION('ref_axis',(1.,0.,0.));
#21035=DIRECTION('',(1.,0.,6.12323399573677E-17));
#21036=DIRECTION('center_axis',(0.,-1.,0.));
#21037=DIRECTION('ref_axis',(1.,0.,0.));
#21038=DIRECTION('',(0.951056516295154,0.,0.309016994374948));
#21039=DIRECTION('center_axis',(0.,-1.,0.));
#21040=DIRECTION('ref_axis',(1.,0.,0.));
#21041=DIRECTION('',(0.809016994374947,0.,0.587785252292473));
#21042=DIRECTION('center_axis',(0.,-1.,0.));
#21043=DIRECTION('ref_axis',(1.,0.,0.));
#21044=DIRECTION('',(0.587785252292473,0.,0.809016994374947));
#21045=DIRECTION('center_axis',(0.,-1.,0.));
#21046=DIRECTION('ref_axis',(1.,0.,0.));
#21047=DIRECTION('',(0.309016994374947,0.,0.951056516295154));
#21048=DIRECTION('center_axis',(0.,-1.,0.));
#21049=DIRECTION('ref_axis',(1.,0.,0.));
#21050=DIRECTION('',(0.,0.,1.));
#21051=DIRECTION('center_axis',(0.,-1.,0.));
#21052=DIRECTION('ref_axis',(1.,0.,0.));
#21053=DIRECTION('',(-0.309016994374948,0.,0.951056516295154));
#21054=DIRECTION('center_axis',(0.,1.,0.));
#21055=DIRECTION('ref_axis',(1.,0.,0.));
#21056=DIRECTION('center_axis',(0.,1.,0.));
#21057=DIRECTION('ref_axis',(6.12323399573677E-17,0.,1.));
#21058=DIRECTION('center_axis',(0.,-1.,0.));
#21059=DIRECTION('ref_axis',(1.,0.,0.));
#21060=DIRECTION('center_axis',(0.,1.,0.));
#21061=DIRECTION('ref_axis',(1.,0.,0.));
#21062=DIRECTION('center_axis',(0.,1.,0.));
#21063=DIRECTION('ref_axis',(1.,0.,0.));
#21064=DIRECTION('',(0.,-1.,0.));
#21065=DIRECTION('center_axis',(0.,-1.,0.));
#21066=DIRECTION('ref_axis',(1.,0.,0.));
#21067=DIRECTION('center_axis',(0.,1.,0.));
#21068=DIRECTION('ref_axis',(1.,0.,0.));
#21069=DIRECTION('',(0.,-1.,0.));
#21070=DIRECTION('',(0.,1.,0.));
#21071=DIRECTION('center_axis',(0.951056516295154,0.,0.309016994374948));
#21072=DIRECTION('ref_axis',(0.309016994374948,0.,-0.951056516295154));
#21073=DIRECTION('',(0.309016994374948,0.,-0.951056516295154));
#21074=DIRECTION('',(0.,1.,0.));
#21075=DIRECTION('',(0.,1.,0.));
#21076=DIRECTION('center_axis',(0.,1.,0.));
#21077=DIRECTION('ref_axis',(1.,0.,0.));
#21078=DIRECTION('center_axis',(0.,1.,0.));
#21079=DIRECTION('ref_axis',(1.,0.,0.));
#21080=DIRECTION('',(0.,-1.,0.));
#21081=DIRECTION('',(0.,1.,0.));
#21082=DIRECTION('center_axis',(0.809016994374947,0.,0.587785252292473));
#21083=DIRECTION('ref_axis',(0.587785252292473,0.,-0.809016994374947));
#21084=DIRECTION('',(0.587785252292473,0.,-0.809016994374947));
#21085=DIRECTION('',(0.,1.,0.));
#21086=DIRECTION('',(0.,1.,0.));
#21087=DIRECTION('center_axis',(0.,1.,0.));
#21088=DIRECTION('ref_axis',(1.,0.,0.));
#21089=DIRECTION('center_axis',(0.,1.,0.));
#21090=DIRECTION('ref_axis',(1.,0.,0.));
#21091=DIRECTION('',(0.,-1.,0.));
#21092=DIRECTION('',(0.,1.,0.));
#21093=DIRECTION('center_axis',(0.587785252292473,0.,0.809016994374948));
#21094=DIRECTION('ref_axis',(0.809016994374948,0.,-0.587785252292473));
#21095=DIRECTION('',(0.809016994374948,0.,-0.587785252292473));
#21096=DIRECTION('',(0.,1.,0.));
#21097=DIRECTION('',(0.,1.,0.));
#21098=DIRECTION('center_axis',(0.,1.,0.));
#21099=DIRECTION('ref_axis',(1.,0.,0.));
#21100=DIRECTION('center_axis',(0.,1.,0.));
#21101=DIRECTION('ref_axis',(1.,0.,0.));
#21102=DIRECTION('',(0.,-1.,0.));
#21103=DIRECTION('',(0.,1.,0.));
#21104=DIRECTION('center_axis',(0.309016994374947,0.,0.951056516295154));
#21105=DIRECTION('ref_axis',(0.951056516295154,0.,-0.309016994374947));
#21106=DIRECTION('',(0.951056516295154,0.,-0.309016994374947));
#21107=DIRECTION('',(0.,1.,0.));
#21108=DIRECTION('',(0.,1.,0.));
#21109=DIRECTION('center_axis',(0.,1.,0.));
#21110=DIRECTION('ref_axis',(1.,0.,0.));
#21111=DIRECTION('center_axis',(0.,1.,0.));
#21112=DIRECTION('ref_axis',(1.,0.,0.));
#21113=DIRECTION('',(0.,-1.,0.));
#21114=DIRECTION('',(0.,1.,0.));
#21115=DIRECTION('center_axis',(-1.83697019872103E-16,0.,1.));
#21116=DIRECTION('ref_axis',(1.,0.,1.83697019872103E-16));
#21117=DIRECTION('',(1.,0.,1.83697019872103E-16));
#21118=DIRECTION('',(0.,1.,0.));
#21119=DIRECTION('',(0.,1.,0.));
#21120=DIRECTION('center_axis',(0.,1.,0.));
#21121=DIRECTION('ref_axis',(1.,0.,0.));
#21122=DIRECTION('center_axis',(0.,1.,0.));
#21123=DIRECTION('ref_axis',(1.,0.,0.));
#21124=DIRECTION('',(0.,-1.,0.));
#21125=DIRECTION('',(0.,1.,0.));
#21126=DIRECTION('center_axis',(-0.309016994374948,0.,0.951056516295154));
#21127=DIRECTION('ref_axis',(0.951056516295154,0.,0.309016994374948));
#21128=DIRECTION('',(0.951056516295154,0.,0.309016994374948));
#21129=DIRECTION('',(0.,1.,0.));
#21130=DIRECTION('',(0.,1.,0.));
#21131=DIRECTION('center_axis',(0.,1.,0.));
#21132=DIRECTION('ref_axis',(1.,0.,0.));
#21133=DIRECTION('center_axis',(0.,1.,0.));
#21134=DIRECTION('ref_axis',(1.,0.,0.));
#21135=DIRECTION('',(0.,-1.,0.));
#21136=DIRECTION('',(0.,1.,0.));
#21137=DIRECTION('center_axis',(-0.587785252292473,0.,0.809016994374947));
#21138=DIRECTION('ref_axis',(0.809016994374947,0.,0.587785252292473));
#21139=DIRECTION('',(0.809016994374947,0.,0.587785252292473));
#21140=DIRECTION('',(0.,1.,0.));
#21141=DIRECTION('',(0.,1.,0.));
#21142=DIRECTION('center_axis',(0.,1.,0.));
#21143=DIRECTION('ref_axis',(1.,0.,0.));
#21144=DIRECTION('center_axis',(0.,1.,0.));
#21145=DIRECTION('ref_axis',(1.,0.,0.));
#21146=DIRECTION('',(0.,-1.,0.));
#21147=DIRECTION('',(0.,1.,0.));
#21148=DIRECTION('center_axis',(-0.809016994374948,0.,0.587785252292473));
#21149=DIRECTION('ref_axis',(0.587785252292473,0.,0.809016994374948));
#21150=DIRECTION('',(0.587785252292473,0.,0.809016994374948));
#21151=DIRECTION('',(0.,1.,0.));
#21152=DIRECTION('',(0.,1.,0.));
#21153=DIRECTION('center_axis',(0.,1.,0.));
#21154=DIRECTION('ref_axis',(1.,0.,0.));
#21155=DIRECTION('center_axis',(0.,1.,0.));
#21156=DIRECTION('ref_axis',(1.,0.,0.));
#21157=DIRECTION('',(0.,-1.,0.));
#21158=DIRECTION('',(0.,1.,0.));
#21159=DIRECTION('center_axis',(-0.951056516295154,0.,0.309016994374947));
#21160=DIRECTION('ref_axis',(0.309016994374947,0.,0.951056516295154));
#21161=DIRECTION('',(0.309016994374947,0.,0.951056516295154));
#21162=DIRECTION('',(0.,1.,0.));
#21163=DIRECTION('',(0.,1.,0.));
#21164=DIRECTION('center_axis',(0.,1.,0.));
#21165=DIRECTION('ref_axis',(1.,0.,0.));
#21166=DIRECTION('center_axis',(0.,1.,0.));
#21167=DIRECTION('ref_axis',(1.,0.,0.));
#21168=DIRECTION('',(0.,-1.,0.));
#21169=DIRECTION('',(0.,1.,0.));
#21170=DIRECTION('center_axis',(-1.,0.,-1.22464679914735E-16));
#21171=DIRECTION('ref_axis',(-1.22464679914735E-16,0.,1.));
#21172=DIRECTION('',(-1.22464679914735E-16,0.,1.));
#21173=DIRECTION('',(0.,1.,0.));
#21174=DIRECTION('',(0.,1.,0.));
#21175=DIRECTION('center_axis',(0.,1.,0.));
#21176=DIRECTION('ref_axis',(1.,0.,0.));
#21177=DIRECTION('center_axis',(0.,1.,0.));
#21178=DIRECTION('ref_axis',(1.,0.,0.));
#21179=DIRECTION('',(0.,-1.,0.));
#21180=DIRECTION('',(0.,1.,0.));
#21181=DIRECTION('center_axis',(-0.951056516295154,0.,-0.309016994374948));
#21182=DIRECTION('ref_axis',(-0.309016994374948,0.,0.951056516295154));
#21183=DIRECTION('',(-0.309016994374948,0.,0.951056516295154));
#21184=DIRECTION('',(0.,1.,0.));
#21185=DIRECTION('',(0.,1.,0.));
#21186=DIRECTION('center_axis',(0.,1.,0.));
#21187=DIRECTION('ref_axis',(1.,0.,0.));
#21188=DIRECTION('center_axis',(0.,1.,0.));
#21189=DIRECTION('ref_axis',(1.,0.,0.));
#21190=DIRECTION('',(0.,-1.,0.));
#21191=DIRECTION('',(0.,1.,0.));
#21192=DIRECTION('center_axis',(-0.809016994374947,0.,-0.587785252292473));
#21193=DIRECTION('ref_axis',(-0.587785252292473,0.,0.809016994374947));
#21194=DIRECTION('',(-0.587785252292473,0.,0.809016994374947));
#21195=DIRECTION('',(0.,1.,0.));
#21196=DIRECTION('',(0.,1.,0.));
#21197=DIRECTION('center_axis',(0.,1.,0.));
#21198=DIRECTION('ref_axis',(1.,0.,0.));
#21199=DIRECTION('center_axis',(0.,1.,0.));
#21200=DIRECTION('ref_axis',(1.,0.,0.));
#21201=DIRECTION('',(0.,-1.,0.));
#21202=DIRECTION('',(0.,1.,0.));
#21203=DIRECTION('center_axis',(-0.587785252292473,0.,-0.809016994374948));
#21204=DIRECTION('ref_axis',(-0.809016994374948,0.,0.587785252292473));
#21205=DIRECTION('',(-0.809016994374948,0.,0.587785252292473));
#21206=DIRECTION('',(0.,1.,0.));
#21207=DIRECTION('',(0.,1.,0.));
#21208=DIRECTION('center_axis',(0.,1.,0.));
#21209=DIRECTION('ref_axis',(1.,0.,0.));
#21210=DIRECTION('center_axis',(0.,1.,0.));
#21211=DIRECTION('ref_axis',(1.,0.,0.));
#21212=DIRECTION('',(0.,-1.,0.));
#21213=DIRECTION('',(0.,1.,0.));
#21214=DIRECTION('center_axis',(-0.309016994374947,0.,-0.951056516295154));
#21215=DIRECTION('ref_axis',(-0.951056516295154,0.,0.309016994374947));
#21216=DIRECTION('',(-0.951056516295154,0.,0.309016994374947));
#21217=DIRECTION('',(0.,1.,0.));
#21218=DIRECTION('',(0.,1.,0.));
#21219=DIRECTION('center_axis',(0.,1.,0.));
#21220=DIRECTION('ref_axis',(1.,0.,0.));
#21221=DIRECTION('center_axis',(0.,1.,0.));
#21222=DIRECTION('ref_axis',(1.,0.,0.));
#21223=DIRECTION('',(0.,-1.,0.));
#21224=DIRECTION('',(0.,1.,0.));
#21225=DIRECTION('center_axis',(6.12323399573677E-17,0.,-1.));
#21226=DIRECTION('ref_axis',(-1.,0.,-6.12323399573677E-17));
#21227=DIRECTION('',(-1.,0.,-6.12323399573677E-17));
#21228=DIRECTION('',(0.,1.,0.));
#21229=DIRECTION('',(0.,1.,0.));
#21230=DIRECTION('center_axis',(0.,1.,0.));
#21231=DIRECTION('ref_axis',(1.,0.,0.));
#21232=DIRECTION('center_axis',(0.,1.,0.));
#21233=DIRECTION('ref_axis',(1.,0.,0.));
#21234=DIRECTION('',(0.,-1.,0.));
#21235=DIRECTION('',(0.,1.,0.));
#21236=DIRECTION('center_axis',(0.309016994374948,0.,-0.951056516295154));
#21237=DIRECTION('ref_axis',(-0.951056516295154,0.,-0.309016994374948));
#21238=DIRECTION('',(-0.951056516295154,0.,-0.309016994374948));
#21239=DIRECTION('',(0.,1.,0.));
#21240=DIRECTION('',(0.,1.,0.));
#21241=DIRECTION('center_axis',(0.,1.,0.));
#21242=DIRECTION('ref_axis',(1.,0.,0.));
#21243=DIRECTION('center_axis',(0.,1.,0.));
#21244=DIRECTION('ref_axis',(1.,0.,0.));
#21245=DIRECTION('',(0.,-1.,0.));
#21246=DIRECTION('',(0.,1.,0.));
#21247=DIRECTION('center_axis',(0.587785252292473,0.,-0.809016994374947));
#21248=DIRECTION('ref_axis',(-0.809016994374947,0.,-0.587785252292473));
#21249=DIRECTION('',(-0.809016994374947,0.,-0.587785252292473));
#21250=DIRECTION('',(0.,1.,0.));
#21251=DIRECTION('',(0.,1.,0.));
#21252=DIRECTION('center_axis',(0.,1.,0.));
#21253=DIRECTION('ref_axis',(1.,0.,0.));
#21254=DIRECTION('center_axis',(0.,1.,0.));
#21255=DIRECTION('ref_axis',(1.,0.,0.));
#21256=DIRECTION('',(0.,-1.,0.));
#21257=DIRECTION('',(0.,1.,0.));
#21258=DIRECTION('center_axis',(0.809016994374947,0.,-0.587785252292473));
#21259=DIRECTION('ref_axis',(-0.587785252292473,0.,-0.809016994374947));
#21260=DIRECTION('',(-0.587785252292473,0.,-0.809016994374947));
#21261=DIRECTION('',(0.,1.,0.));
#21262=DIRECTION('',(0.,1.,0.));
#21263=DIRECTION('center_axis',(0.,1.,0.));
#21264=DIRECTION('ref_axis',(1.,0.,0.));
#21265=DIRECTION('center_axis',(0.,1.,0.));
#21266=DIRECTION('ref_axis',(1.,0.,0.));
#21267=DIRECTION('',(0.,-1.,0.));
#21268=DIRECTION('',(0.,1.,0.));
#21269=DIRECTION('center_axis',(0.951056516295154,0.,-0.309016994374947));
#21270=DIRECTION('ref_axis',(-0.309016994374947,0.,-0.951056516295154));
#21271=DIRECTION('',(-0.309016994374947,0.,-0.951056516295154));
#21272=DIRECTION('',(0.,1.,0.));
#21273=DIRECTION('',(0.,1.,0.));
#21274=DIRECTION('center_axis',(0.,1.,0.));
#21275=DIRECTION('ref_axis',(1.,0.,0.));
#21276=DIRECTION('center_axis',(0.,1.,0.));
#21277=DIRECTION('ref_axis',(1.,0.,0.));
#21278=DIRECTION('',(0.,-1.,0.));
#21279=DIRECTION('',(0.,1.,0.));
#21280=DIRECTION('center_axis',(1.,0.,0.));
#21281=DIRECTION('ref_axis',(0.,0.,-1.));
#21282=DIRECTION('',(0.,0.,-1.));
#21283=DIRECTION('',(0.,1.,0.));
#21284=DIRECTION('',(0.,1.,0.));
#21285=DIRECTION('center_axis',(0.,1.,0.));
#21286=DIRECTION('ref_axis',(1.,0.,0.));
#21287=DIRECTION('center_axis',(0.,1.,0.));
#21288=DIRECTION('ref_axis',(1.,0.,0.));
#21289=DIRECTION('center_axis',(0.,1.,0.));
#21290=DIRECTION('ref_axis',(1.,0.,0.));
#21291=DIRECTION('axis',(0.,0.,1.));
#21292=DIRECTION('refdir',(1.,0.,0.));
#21293=DIRECTION('center_axis',(1.,0.,0.));
#21294=DIRECTION('ref_axis',(0.,0.,-1.));
#21295=DIRECTION('',(0.,0.707106781186547,-0.707106781186548));
#21296=DIRECTION('',(0.,1.,0.));
#21297=DIRECTION('',(0.,0.707106781186547,0.707106781186548));
#21298=DIRECTION('',(0.,0.,1.));
#21299=DIRECTION('',(0.,-0.707106781186548,0.707106781186548));
#21300=DIRECTION('',(0.,-1.,0.));
#21301=DIRECTION('',(0.,-0.707106781186548,-0.707106781186548));
#21302=DIRECTION('',(0.,0.,-1.));
#21303=DIRECTION('center_axis',(0.,-0.707106781186548,-0.707106781186548));
#21304=DIRECTION('ref_axis',(-1.,0.,0.));
#21305=DIRECTION('',(-1.,0.,0.));
#21306=DIRECTION('',(0.,0.707106781186548,-0.707106781186548));
#21307=DIRECTION('',(1.,0.,0.));
#21308=DIRECTION('center_axis',(0.,-1.,0.));
#21309=DIRECTION('ref_axis',(1.,0.,0.));
#21310=DIRECTION('',(1.,0.,0.));
#21311=DIRECTION('',(0.,0.,-1.));
#21312=DIRECTION('center_axis',(0.,-0.707106781186548,0.707106781186547));
#21313=DIRECTION('ref_axis',(1.,0.,0.));
#21314=DIRECTION('',(-1.,0.,0.));
#21315=DIRECTION('',(0.,-0.707106781186547,-0.707106781186548));
#21316=DIRECTION('center_axis',(0.,0.,1.));
#21317=DIRECTION('ref_axis',(1.,0.,0.));
#21318=DIRECTION('',(1.,0.,0.));
#21319=DIRECTION('',(0.,-1.,0.));
#21320=DIRECTION('center_axis',(1.,0.,0.));
#21321=DIRECTION('ref_axis',(0.,0.,-1.));
#21322=DIRECTION('',(0.,-0.707106781186547,0.707106781186548));
#21323=DIRECTION('',(0.,0.,1.));
#21324=DIRECTION('',(0.,0.707106781186548,0.707106781186548));
#21325=DIRECTION('',(0.,1.,0.));
#21326=DIRECTION('center_axis',(0.,0.707106781186548,0.707106781186547));
#21327=DIRECTION('ref_axis',(1.,0.,0.));
#21328=DIRECTION('',(-1.,0.,0.));
#21329=DIRECTION('center_axis',(0.,1.,0.));
#21330=DIRECTION('ref_axis',(-1.,0.,0.));
#21331=DIRECTION('',(1.,0.,0.));
#21332=DIRECTION('center_axis',(0.,0.707106781186548,-0.707106781186548));
#21333=DIRECTION('ref_axis',(-1.,0.,0.));
#21334=DIRECTION('',(-1.,0.,0.));
#21335=DIRECTION('center_axis',(0.,0.,1.));
#21336=DIRECTION('ref_axis',(1.,0.,0.));
#21337=DIRECTION('axis',(0.,0.,1.));
#21338=DIRECTION('refdir',(1.,0.,0.));
#21339=DIRECTION('axis',(0.,0.,1.));
#21340=DIRECTION('refdir',(1.,0.,0.));
#21341=DIRECTION('center_axis',(-1.,0.,0.));
#21342=DIRECTION('ref_axis',(0.,0.,1.));
#21343=DIRECTION('',(0.,-1.,0.));
#21344=DIRECTION('',(0.,0.,1.));
#21345=DIRECTION('',(0.,1.,0.));
#21346=DIRECTION('',(0.,0.,-1.));
#21347=DIRECTION('center_axis',(0.,1.,0.));
#21348=DIRECTION('ref_axis',(1.,0.,0.));
#21349=DIRECTION('center_axis',(0.,-1.,0.));
#21350=DIRECTION('ref_axis',(1.,0.,0.));
#21351=DIRECTION('',(-1.,0.,0.));
#21352=DIRECTION('',(0.,0.,1.));
#21353=DIRECTION('center_axis',(1.,0.,0.));
#21354=DIRECTION('ref_axis',(0.,0.,-1.));
#21355=DIRECTION('',(0.,1.,0.));
#21356=DIRECTION('',(0.,1.,0.));
#21357=DIRECTION('',(0.,0.,-1.));
#21358=DIRECTION('center_axis',(0.,0.,1.));
#21359=DIRECTION('ref_axis',(1.,0.,0.));
#21360=DIRECTION('',(1.,0.,0.));
#21361=DIRECTION('center_axis',(0.,1.,0.));
#21362=DIRECTION('ref_axis',(0.,0.,1.));
#21363=DIRECTION('center_axis',(0.,1.,0.));
#21364=DIRECTION('ref_axis',(1.,0.,0.));
#21365=DIRECTION('center_axis',(-0.996917333733128,0.,0.0784590957278455));
#21366=DIRECTION('ref_axis',(0.0784590957278455,0.,0.996917333733128));
#21367=DIRECTION('',(0.,-1.,0.));
#21368=DIRECTION('',(0.0784590957278455,0.,0.996917333733128));
#21369=DIRECTION('',(0.,1.,0.));
#21370=DIRECTION('',(-0.0784590957278455,0.,-0.996917333733128));
#21371=DIRECTION('center_axis',(0.,1.,0.));
#21372=DIRECTION('ref_axis',(1.,0.,0.));
#21373=DIRECTION('center_axis',(0.,-1.,0.));
#21374=DIRECTION('ref_axis',(1.,0.,0.));
#21375=DIRECTION('',(-0.996917333733128,0.,0.0784590957278475));
#21376=DIRECTION('',(0.0784590957278456,0.,0.996917333733128));
#21377=DIRECTION('center_axis',(0.996917333733128,0.,-0.0784590957278456));
#21378=DIRECTION('ref_axis',(-0.0784590957278456,0.,-0.996917333733128));
#21379=DIRECTION('',(0.,1.,0.));
#21380=DIRECTION('',(0.,1.,0.));
#21381=DIRECTION('',(-0.0784590957278456,0.,-0.996917333733128));
#21382=DIRECTION('center_axis',(0.0784590957278475,0.,0.996917333733128));
#21383=DIRECTION('ref_axis',(0.996917333733128,0.,-0.0784590957278475));
#21384=DIRECTION('',(0.996917333733128,0.,-0.0784590957278475));
#21385=DIRECTION('center_axis',(0.,1.,0.));
#21386=DIRECTION('ref_axis',(0.,0.,1.));
#21387=DIRECTION('center_axis',(0.,1.,0.));
#21388=DIRECTION('ref_axis',(1.,0.,0.));
#21389=DIRECTION('center_axis',(0.,1.,0.));
#21390=DIRECTION('ref_axis',(1.,0.,0.));
#21391=DIRECTION('center_axis',(0.,1.,0.));
#21392=DIRECTION('ref_axis',(1.,0.,0.));
#21393=DIRECTION('',(0.,-1.,0.));
#21394=DIRECTION('center_axis',(0.,1.,0.));
#21395=DIRECTION('ref_axis',(1.,0.,0.));
#21396=DIRECTION('center_axis',(0.,1.,0.));
#21397=DIRECTION('ref_axis',(1.,0.,0.));
#21398=DIRECTION('center_axis',(0.,1.,0.));
#21399=DIRECTION('ref_axis',(1.,0.,0.));
#21400=DIRECTION('axis',(0.,0.,1.));
#21401=DIRECTION('refdir',(1.,0.,0.));
#21402=DIRECTION('center_axis',(0.,0.,1.));
#21403=DIRECTION('ref_axis',(1.,0.,0.));
#21404=DIRECTION('',(0.,1.,0.));
#21405=DIRECTION('center_axis',(0.,0.,1.));
#21406=DIRECTION('ref_axis',(1.,0.,0.));
#21407=DIRECTION('center_axis',(0.,0.,1.));
#21408=DIRECTION('ref_axis',(1.,0.,0.));
#21409=DIRECTION('center_axis',(0.,0.,1.));
#21410=DIRECTION('ref_axis',(1.,0.,0.));
#21411=DIRECTION('',(0.,0.,1.));
#21412=DIRECTION('center_axis',(0.,0.,1.));
#21413=DIRECTION('ref_axis',(1.,0.,0.));
#21414=DIRECTION('center_axis',(0.,0.,1.));
#21415=DIRECTION('ref_axis',(1.,0.,0.));
#21416=DIRECTION('',(0.,-1.,0.));
#21417=DIRECTION('center_axis',(0.,1.,0.));
#21418=DIRECTION('ref_axis',(1.,0.,0.));
#21419=DIRECTION('center_axis',(0.,-1.,0.));
#21420=DIRECTION('ref_axis',(1.,0.,0.));
#21421=DIRECTION('',(0.,-1.,0.));
#21422=DIRECTION('center_axis',(0.,-1.,0.));
#21423=DIRECTION('ref_axis',(1.,0.,0.));
#21424=DIRECTION('center_axis',(0.,1.,0.));
#21425=DIRECTION('ref_axis',(1.,0.,0.));
#21426=DIRECTION('center_axis',(0.,1.,0.));
#21427=DIRECTION('ref_axis',(1.,0.,0.));
#21428=DIRECTION('',(0.,-1.,0.));
#21429=DIRECTION('center_axis',(0.,1.,0.));
#21430=DIRECTION('ref_axis',(1.,0.,0.));
#21431=DIRECTION('center_axis',(0.,1.,0.));
#21432=DIRECTION('ref_axis',(1.,0.,0.));
#21433=DIRECTION('center_axis',(0.,1.,0.));
#21434=DIRECTION('ref_axis',(1.,0.,0.));
#21435=DIRECTION('axis',(0.,0.,1.));
#21436=DIRECTION('refdir',(1.,0.,0.));
#21437=DIRECTION('center_axis',(0.,0.,1.));
#21438=DIRECTION('ref_axis',(1.,0.,0.));
#21439=DIRECTION('',(0.,1.,0.));
#21440=DIRECTION('center_axis',(0.,0.,1.));
#21441=DIRECTION('ref_axis',(1.,0.,0.));
#21442=DIRECTION('center_axis',(0.,0.,1.));
#21443=DIRECTION('ref_axis',(1.,0.,0.));
#21444=DIRECTION('center_axis',(0.,0.,1.));
#21445=DIRECTION('ref_axis',(1.,0.,0.));
#21446=DIRECTION('',(0.,0.,1.));
#21447=DIRECTION('center_axis',(0.,0.,1.));
#21448=DIRECTION('ref_axis',(1.,0.,0.));
#21449=DIRECTION('center_axis',(0.,0.,1.));
#21450=DIRECTION('ref_axis',(1.,0.,0.));
#21451=DIRECTION('',(0.,-1.,0.));
#21452=DIRECTION('center_axis',(0.,1.,0.));
#21453=DIRECTION('ref_axis',(1.,0.,0.));
#21454=DIRECTION('center_axis',(0.,-1.,0.));
#21455=DIRECTION('ref_axis',(1.,0.,0.));
#21456=DIRECTION('',(0.,-1.,0.));
#21457=DIRECTION('center_axis',(0.,-1.,0.));
#21458=DIRECTION('ref_axis',(1.,0.,0.));
#21459=DIRECTION('center_axis',(0.,1.,0.));
#21460=DIRECTION('ref_axis',(1.,0.,0.));
#21461=DIRECTION('center_axis',(0.,1.,0.));
#21462=DIRECTION('ref_axis',(1.,0.,0.));
#21463=DIRECTION('',(0.,-1.,0.));
#21464=DIRECTION('center_axis',(0.,1.,0.));
#21465=DIRECTION('ref_axis',(1.,0.,0.));
#21466=DIRECTION('center_axis',(0.,1.,0.));
#21467=DIRECTION('ref_axis',(1.,0.,0.));
#21468=DIRECTION('center_axis',(0.,1.,0.));
#21469=DIRECTION('ref_axis',(1.,0.,0.));
#21470=DIRECTION('axis',(0.,0.,1.));
#21471=DIRECTION('refdir',(1.,0.,0.));
#21472=DIRECTION('center_axis',(0.,1.,0.));
#21473=DIRECTION('ref_axis',(1.,0.,0.));
#21474=DIRECTION('center_axis',(0.,-1.,0.));
#21475=DIRECTION('ref_axis',(1.,0.,0.));
#21476=DIRECTION('',(0.,-1.,0.));
#21477=DIRECTION('center_axis',(0.,-1.,0.));
#21478=DIRECTION('ref_axis',(1.,0.,0.));
#21479=DIRECTION('center_axis',(0.,1.,0.));
#21480=DIRECTION('ref_axis',(1.,0.,0.));
#21481=DIRECTION('center_axis',(0.,1.,0.));
#21482=DIRECTION('ref_axis',(1.,0.,0.));
#21483=DIRECTION('',(0.,-1.,0.));
#21484=DIRECTION('center_axis',(0.,1.,0.));
#21485=DIRECTION('ref_axis',(1.,0.,0.));
#21486=DIRECTION('center_axis',(0.,1.,0.));
#21487=DIRECTION('ref_axis',(1.,0.,0.));
#21488=DIRECTION('center_axis',(0.,1.,0.));
#21489=DIRECTION('ref_axis',(1.,0.,0.));
#21490=DIRECTION('axis',(0.,0.,1.));
#21491=DIRECTION('refdir',(1.,0.,0.));
#21492=DIRECTION('center_axis',(0.,1.,0.));
#21493=DIRECTION('ref_axis',(1.,0.,0.));
#21494=DIRECTION('center_axis',(0.,-1.,0.));
#21495=DIRECTION('ref_axis',(1.,0.,0.));
#21496=DIRECTION('',(0.,-1.,0.));
#21497=DIRECTION('center_axis',(0.,-1.,0.));
#21498=DIRECTION('ref_axis',(1.,0.,0.));
#21499=DIRECTION('center_axis',(0.,1.,0.));
#21500=DIRECTION('ref_axis',(1.,0.,0.));
#21501=DIRECTION('center_axis',(0.,1.,0.));
#21502=DIRECTION('ref_axis',(1.,0.,0.));
#21503=DIRECTION('',(0.,-1.,0.));
#21504=DIRECTION('center_axis',(0.,1.,0.));
#21505=DIRECTION('ref_axis',(1.,0.,0.));
#21506=DIRECTION('center_axis',(0.,1.,0.));
#21507=DIRECTION('ref_axis',(1.,0.,0.));
#21508=DIRECTION('center_axis',(0.,1.,0.));
#21509=DIRECTION('ref_axis',(1.,0.,0.));
#21510=DIRECTION('axis',(0.,0.,1.));
#21511=DIRECTION('refdir',(1.,0.,0.));
#21512=DIRECTION('center_axis',(0.,1.,0.));
#21513=DIRECTION('ref_axis',(1.,0.,0.));
#21514=DIRECTION('center_axis',(0.,-1.,0.));
#21515=DIRECTION('ref_axis',(1.,0.,0.));
#21516=DIRECTION('',(0.,-1.,0.));
#21517=DIRECTION('center_axis',(0.,-1.,0.));
#21518=DIRECTION('ref_axis',(1.,0.,0.));
#21519=DIRECTION('center_axis',(0.,1.,0.));
#21520=DIRECTION('ref_axis',(1.,0.,0.));
#21521=DIRECTION('center_axis',(0.,1.,0.));
#21522=DIRECTION('ref_axis',(1.,0.,0.));
#21523=DIRECTION('',(0.,-1.,0.));
#21524=DIRECTION('center_axis',(0.,1.,0.));
#21525=DIRECTION('ref_axis',(1.,0.,0.));
#21526=DIRECTION('center_axis',(0.,1.,0.));
#21527=DIRECTION('ref_axis',(1.,0.,0.));
#21528=DIRECTION('center_axis',(0.,1.,0.));
#21529=DIRECTION('ref_axis',(1.,0.,0.));
#21530=DIRECTION('axis',(0.,0.,1.));
#21531=DIRECTION('refdir',(1.,0.,0.));
#21532=DIRECTION('center_axis',(0.,1.,0.));
#21533=DIRECTION('ref_axis',(1.,0.,0.));
#21534=DIRECTION('center_axis',(0.,-1.,0.));
#21535=DIRECTION('ref_axis',(1.,0.,0.));
#21536=DIRECTION('',(0.,-1.,0.));
#21537=DIRECTION('center_axis',(0.,-1.,0.));
#21538=DIRECTION('ref_axis',(1.,0.,0.));
#21539=DIRECTION('center_axis',(0.,1.,0.));
#21540=DIRECTION('ref_axis',(1.,0.,0.));
#21541=DIRECTION('center_axis',(0.,1.,0.));
#21542=DIRECTION('ref_axis',(1.,0.,0.));
#21543=DIRECTION('',(0.,-1.,0.));
#21544=DIRECTION('center_axis',(0.,1.,0.));
#21545=DIRECTION('ref_axis',(1.,0.,0.));
#21546=DIRECTION('center_axis',(0.,1.,0.));
#21547=DIRECTION('ref_axis',(1.,0.,0.));
#21548=DIRECTION('center_axis',(0.,1.,0.));
#21549=DIRECTION('ref_axis',(1.,0.,0.));
#21550=DIRECTION('axis',(0.,0.,1.));
#21551=DIRECTION('refdir',(1.,0.,0.));
#21552=DIRECTION('center_axis',(0.,1.,0.));
#21553=DIRECTION('ref_axis',(1.,0.,0.));
#21554=DIRECTION('center_axis',(0.,-1.,0.));
#21555=DIRECTION('ref_axis',(1.,0.,0.));
#21556=DIRECTION('',(0.,-1.,0.));
#21557=DIRECTION('center_axis',(0.,-1.,0.));
#21558=DIRECTION('ref_axis',(1.,0.,0.));
#21559=DIRECTION('center_axis',(0.,1.,0.));
#21560=DIRECTION('ref_axis',(1.,0.,0.));
#21561=DIRECTION('center_axis',(0.,1.,0.));
#21562=DIRECTION('ref_axis',(1.,0.,0.));
#21563=DIRECTION('',(0.,-1.,0.));
#21564=DIRECTION('center_axis',(0.,1.,0.));
#21565=DIRECTION('ref_axis',(1.,0.,0.));
#21566=DIRECTION('center_axis',(0.,1.,0.));
#21567=DIRECTION('ref_axis',(1.,0.,0.));
#21568=DIRECTION('center_axis',(0.,1.,0.));
#21569=DIRECTION('ref_axis',(1.,0.,0.));
#21570=DIRECTION('axis',(0.,0.,1.));
#21571=DIRECTION('refdir',(1.,0.,0.));
#21572=DIRECTION('center_axis',(-1.,0.,0.));
#21573=DIRECTION('ref_axis',(0.,0.,1.));
#21574=DIRECTION('',(0.,0.,1.));
#21575=DIRECTION('',(0.,1.,0.));
#21576=DIRECTION('',(0.,0.,-1.));
#21577=DIRECTION('',(0.,1.,0.));
#21578=DIRECTION('center_axis',(0.,0.,-1.));
#21579=DIRECTION('ref_axis',(-1.,0.,0.));
#21580=DIRECTION('',(-1.,0.,0.));
#21581=DIRECTION('',(0.,1.,0.));
#21582=DIRECTION('',(1.,0.,0.));
#21583=DIRECTION('center_axis',(1.,0.,0.));
#21584=DIRECTION('ref_axis',(0.,0.,-1.));
#21585=DIRECTION('',(0.,0.,-1.));
#21586=DIRECTION('',(0.,-1.,0.));
#21587=DIRECTION('',(0.,0.,1.));
#21588=DIRECTION('center_axis',(0.,1.,0.));
#21589=DIRECTION('ref_axis',(1.,0.,0.));
#21590=DIRECTION('center_axis',(0.,1.,0.));
#21591=DIRECTION('ref_axis',(1.,0.,0.));
#21592=DIRECTION('center_axis',(0.,-1.,0.));
#21593=DIRECTION('ref_axis',(1.,0.,0.));
#21594=DIRECTION('center_axis',(0.,1.,0.));
#21595=DIRECTION('ref_axis',(-1.83697019872103E-16,0.,1.));
#21596=DIRECTION('center_axis',(0.,1.,0.));
#21597=DIRECTION('ref_axis',(1.,0.,0.));
#21598=DIRECTION('center_axis',(0.,1.,0.));
#21599=DIRECTION('ref_axis',(1.,0.,0.));
#21600=DIRECTION('center_axis',(0.,-1.,0.));
#21601=DIRECTION('ref_axis',(1.,0.,0.));
#21602=DIRECTION('',(-0.587785252292473,0.,0.809016994374947));
#21603=DIRECTION('center_axis',(0.,-1.,0.));
#21604=DIRECTION('ref_axis',(1.,0.,0.));
#21605=DIRECTION('',(-0.809016994374948,0.,0.587785252292473));
#21606=DIRECTION('center_axis',(0.,-1.,0.));
#21607=DIRECTION('ref_axis',(1.,0.,0.));
#21608=DIRECTION('',(-0.951056516295154,0.,0.309016994374947));
#21609=DIRECTION('center_axis',(0.,-1.,0.));
#21610=DIRECTION('ref_axis',(1.,0.,0.));
#21611=DIRECTION('',(-1.,0.,-1.83697019872103E-16));
#21612=DIRECTION('center_axis',(0.,-1.,0.));
#21613=DIRECTION('ref_axis',(1.,0.,0.));
#21614=DIRECTION('',(-0.951056516295154,0.,-0.309016994374948));
#21615=DIRECTION('center_axis',(0.,-1.,0.));
#21616=DIRECTION('ref_axis',(1.,0.,0.));
#21617=DIRECTION('',(-0.809016994374947,0.,-0.587785252292473));
#21618=DIRECTION('center_axis',(0.,-1.,0.));
#21619=DIRECTION('ref_axis',(1.,0.,0.));
#21620=DIRECTION('',(-0.587785252292473,0.,-0.809016994374948));
#21621=DIRECTION('center_axis',(0.,-1.,0.));
#21622=DIRECTION('ref_axis',(1.,0.,0.));
#21623=DIRECTION('',(-0.309016994374947,0.,-0.951056516295154));
#21624=DIRECTION('center_axis',(0.,-1.,0.));
#21625=DIRECTION('ref_axis',(1.,0.,0.));
#21626=DIRECTION('',(1.22464679914735E-16,0.,-1.));
#21627=DIRECTION('center_axis',(0.,-1.,0.));
#21628=DIRECTION('ref_axis',(1.,0.,0.));
#21629=DIRECTION('',(0.309016994374948,0.,-0.951056516295154));
#21630=DIRECTION('center_axis',(0.,-1.,0.));
#21631=DIRECTION('ref_axis',(1.,0.,0.));
#21632=DIRECTION('',(0.587785252292473,0.,-0.809016994374947));
#21633=DIRECTION('center_axis',(0.,-1.,0.));
#21634=DIRECTION('ref_axis',(1.,0.,0.));
#21635=DIRECTION('',(0.809016994374948,0.,-0.587785252292473));
#21636=DIRECTION('center_axis',(0.,-1.,0.));
#21637=DIRECTION('ref_axis',(1.,0.,0.));
#21638=DIRECTION('',(0.951056516295154,0.,-0.309016994374947));
#21639=DIRECTION('center_axis',(0.,-1.,0.));
#21640=DIRECTION('ref_axis',(1.,0.,0.));
#21641=DIRECTION('',(1.,0.,6.12323399573677E-17));
#21642=DIRECTION('center_axis',(0.,-1.,0.));
#21643=DIRECTION('ref_axis',(1.,0.,0.));
#21644=DIRECTION('',(0.951056516295154,0.,0.309016994374948));
#21645=DIRECTION('center_axis',(0.,-1.,0.));
#21646=DIRECTION('ref_axis',(1.,0.,0.));
#21647=DIRECTION('',(0.809016994374947,0.,0.587785252292473));
#21648=DIRECTION('center_axis',(0.,-1.,0.));
#21649=DIRECTION('ref_axis',(1.,0.,0.));
#21650=DIRECTION('',(0.587785252292473,0.,0.809016994374947));
#21651=DIRECTION('center_axis',(0.,-1.,0.));
#21652=DIRECTION('ref_axis',(1.,0.,0.));
#21653=DIRECTION('',(0.309016994374947,0.,0.951056516295154));
#21654=DIRECTION('center_axis',(0.,-1.,0.));
#21655=DIRECTION('ref_axis',(1.,0.,0.));
#21656=DIRECTION('',(0.,0.,1.));
#21657=DIRECTION('center_axis',(0.,-1.,0.));
#21658=DIRECTION('ref_axis',(1.,0.,0.));
#21659=DIRECTION('',(-0.309016994374948,0.,0.951056516295154));
#21660=DIRECTION('center_axis',(0.,1.,0.));
#21661=DIRECTION('ref_axis',(1.,0.,0.));
#21662=DIRECTION('',(0.,-1.,0.));
#21663=DIRECTION('center_axis',(0.,-1.,0.));
#21664=DIRECTION('ref_axis',(1.,0.,0.));
#21665=DIRECTION('',(0.,-1.,0.));
#21666=DIRECTION('',(0.,1.,0.));
#21667=DIRECTION('center_axis',(0.951056516295154,0.,0.309016994374948));
#21668=DIRECTION('ref_axis',(0.309016994374948,0.,-0.951056516295154));
#21669=DIRECTION('',(0.309016994374948,0.,-0.951056516295154));
#21670=DIRECTION('',(0.,1.,0.));
#21671=DIRECTION('',(0.,1.,0.));
#21672=DIRECTION('center_axis',(0.,1.,0.));
#21673=DIRECTION('ref_axis',(1.,0.,0.));
#21674=DIRECTION('center_axis',(0.,1.,0.));
#21675=DIRECTION('ref_axis',(1.,0.,0.));
#21676=DIRECTION('',(0.,-1.,0.));
#21677=DIRECTION('',(0.,1.,0.));
#21678=DIRECTION('center_axis',(0.809016994374947,0.,0.587785252292473));
#21679=DIRECTION('ref_axis',(0.587785252292473,0.,-0.809016994374947));
#21680=DIRECTION('',(0.587785252292473,0.,-0.809016994374947));
#21681=DIRECTION('',(0.,1.,0.));
#21682=DIRECTION('',(0.,1.,0.));
#21683=DIRECTION('center_axis',(0.,1.,0.));
#21684=DIRECTION('ref_axis',(1.,0.,0.));
#21685=DIRECTION('center_axis',(0.,1.,0.));
#21686=DIRECTION('ref_axis',(1.,0.,0.));
#21687=DIRECTION('',(0.,-1.,0.));
#21688=DIRECTION('',(0.,1.,0.));
#21689=DIRECTION('center_axis',(0.587785252292473,0.,0.809016994374948));
#21690=DIRECTION('ref_axis',(0.809016994374948,0.,-0.587785252292473));
#21691=DIRECTION('',(0.809016994374948,0.,-0.587785252292473));
#21692=DIRECTION('',(0.,1.,0.));
#21693=DIRECTION('',(0.,1.,0.));
#21694=DIRECTION('center_axis',(0.,1.,0.));
#21695=DIRECTION('ref_axis',(1.,0.,0.));
#21696=DIRECTION('center_axis',(0.,1.,0.));
#21697=DIRECTION('ref_axis',(1.,0.,0.));
#21698=DIRECTION('',(0.,-1.,0.));
#21699=DIRECTION('',(0.,1.,0.));
#21700=DIRECTION('center_axis',(0.309016994374947,0.,0.951056516295154));
#21701=DIRECTION('ref_axis',(0.951056516295154,0.,-0.309016994374947));
#21702=DIRECTION('',(0.951056516295154,0.,-0.309016994374947));
#21703=DIRECTION('',(0.,1.,0.));
#21704=DIRECTION('',(0.,1.,0.));
#21705=DIRECTION('center_axis',(0.,1.,0.));
#21706=DIRECTION('ref_axis',(1.,0.,0.));
#21707=DIRECTION('center_axis',(0.,1.,0.));
#21708=DIRECTION('ref_axis',(1.,0.,0.));
#21709=DIRECTION('',(0.,-1.,0.));
#21710=DIRECTION('',(0.,1.,0.));
#21711=DIRECTION('center_axis',(-1.83697019872103E-16,0.,1.));
#21712=DIRECTION('ref_axis',(1.,0.,1.83697019872103E-16));
#21713=DIRECTION('',(1.,0.,1.83697019872103E-16));
#21714=DIRECTION('',(0.,1.,0.));
#21715=DIRECTION('',(0.,1.,0.));
#21716=DIRECTION('center_axis',(0.,1.,0.));
#21717=DIRECTION('ref_axis',(1.,0.,0.));
#21718=DIRECTION('center_axis',(0.,1.,0.));
#21719=DIRECTION('ref_axis',(1.,0.,0.));
#21720=DIRECTION('',(0.,-1.,0.));
#21721=DIRECTION('',(0.,1.,0.));
#21722=DIRECTION('center_axis',(-0.309016994374948,0.,0.951056516295154));
#21723=DIRECTION('ref_axis',(0.951056516295154,0.,0.309016994374948));
#21724=DIRECTION('',(0.951056516295154,0.,0.309016994374948));
#21725=DIRECTION('',(0.,1.,0.));
#21726=DIRECTION('',(0.,1.,0.));
#21727=DIRECTION('center_axis',(0.,1.,0.));
#21728=DIRECTION('ref_axis',(1.,0.,0.));
#21729=DIRECTION('center_axis',(0.,1.,0.));
#21730=DIRECTION('ref_axis',(1.,0.,0.));
#21731=DIRECTION('',(0.,-1.,0.));
#21732=DIRECTION('',(0.,1.,0.));
#21733=DIRECTION('center_axis',(-0.587785252292473,0.,0.809016994374947));
#21734=DIRECTION('ref_axis',(0.809016994374947,0.,0.587785252292473));
#21735=DIRECTION('',(0.809016994374947,0.,0.587785252292473));
#21736=DIRECTION('',(0.,1.,0.));
#21737=DIRECTION('',(0.,1.,0.));
#21738=DIRECTION('center_axis',(0.,1.,0.));
#21739=DIRECTION('ref_axis',(1.,0.,0.));
#21740=DIRECTION('center_axis',(0.,1.,0.));
#21741=DIRECTION('ref_axis',(1.,0.,0.));
#21742=DIRECTION('',(0.,-1.,0.));
#21743=DIRECTION('',(0.,1.,0.));
#21744=DIRECTION('center_axis',(-0.809016994374948,0.,0.587785252292473));
#21745=DIRECTION('ref_axis',(0.587785252292473,0.,0.809016994374948));
#21746=DIRECTION('',(0.587785252292473,0.,0.809016994374948));
#21747=DIRECTION('',(0.,1.,0.));
#21748=DIRECTION('',(0.,1.,0.));
#21749=DIRECTION('center_axis',(0.,1.,0.));
#21750=DIRECTION('ref_axis',(1.,0.,0.));
#21751=DIRECTION('center_axis',(0.,1.,0.));
#21752=DIRECTION('ref_axis',(1.,0.,0.));
#21753=DIRECTION('',(0.,-1.,0.));
#21754=DIRECTION('',(0.,1.,0.));
#21755=DIRECTION('center_axis',(-0.951056516295154,0.,0.309016994374947));
#21756=DIRECTION('ref_axis',(0.309016994374947,0.,0.951056516295154));
#21757=DIRECTION('',(0.309016994374947,0.,0.951056516295154));
#21758=DIRECTION('',(0.,1.,0.));
#21759=DIRECTION('',(0.,1.,0.));
#21760=DIRECTION('center_axis',(0.,1.,0.));
#21761=DIRECTION('ref_axis',(1.,0.,0.));
#21762=DIRECTION('center_axis',(0.,1.,0.));
#21763=DIRECTION('ref_axis',(1.,0.,0.));
#21764=DIRECTION('',(0.,-1.,0.));
#21765=DIRECTION('',(0.,1.,0.));
#21766=DIRECTION('center_axis',(-1.,0.,-1.22464679914735E-16));
#21767=DIRECTION('ref_axis',(-1.22464679914735E-16,0.,1.));
#21768=DIRECTION('',(-1.22464679914735E-16,0.,1.));
#21769=DIRECTION('',(0.,1.,0.));
#21770=DIRECTION('',(0.,1.,0.));
#21771=DIRECTION('center_axis',(0.,1.,0.));
#21772=DIRECTION('ref_axis',(1.,0.,0.));
#21773=DIRECTION('center_axis',(0.,1.,0.));
#21774=DIRECTION('ref_axis',(1.,0.,0.));
#21775=DIRECTION('',(0.,-1.,0.));
#21776=DIRECTION('',(0.,1.,0.));
#21777=DIRECTION('center_axis',(-0.951056516295154,0.,-0.309016994374948));
#21778=DIRECTION('ref_axis',(-0.309016994374948,0.,0.951056516295154));
#21779=DIRECTION('',(-0.309016994374948,0.,0.951056516295154));
#21780=DIRECTION('',(0.,1.,0.));
#21781=DIRECTION('',(0.,1.,0.));
#21782=DIRECTION('center_axis',(0.,1.,0.));
#21783=DIRECTION('ref_axis',(1.,0.,0.));
#21784=DIRECTION('center_axis',(0.,1.,0.));
#21785=DIRECTION('ref_axis',(1.,0.,0.));
#21786=DIRECTION('',(0.,-1.,0.));
#21787=DIRECTION('',(0.,1.,0.));
#21788=DIRECTION('center_axis',(-0.809016994374947,0.,-0.587785252292473));
#21789=DIRECTION('ref_axis',(-0.587785252292473,0.,0.809016994374947));
#21790=DIRECTION('',(-0.587785252292473,0.,0.809016994374947));
#21791=DIRECTION('',(0.,1.,0.));
#21792=DIRECTION('',(0.,1.,0.));
#21793=DIRECTION('center_axis',(0.,1.,0.));
#21794=DIRECTION('ref_axis',(1.,0.,0.));
#21795=DIRECTION('center_axis',(0.,1.,0.));
#21796=DIRECTION('ref_axis',(1.,0.,0.));
#21797=DIRECTION('',(0.,-1.,0.));
#21798=DIRECTION('',(0.,1.,0.));
#21799=DIRECTION('center_axis',(-0.587785252292473,0.,-0.809016994374948));
#21800=DIRECTION('ref_axis',(-0.809016994374948,0.,0.587785252292473));
#21801=DIRECTION('',(-0.809016994374948,0.,0.587785252292473));
#21802=DIRECTION('',(0.,1.,0.));
#21803=DIRECTION('',(0.,1.,0.));
#21804=DIRECTION('center_axis',(0.,1.,0.));
#21805=DIRECTION('ref_axis',(1.,0.,0.));
#21806=DIRECTION('center_axis',(0.,1.,0.));
#21807=DIRECTION('ref_axis',(1.,0.,0.));
#21808=DIRECTION('',(0.,-1.,0.));
#21809=DIRECTION('',(0.,1.,0.));
#21810=DIRECTION('center_axis',(-0.309016994374947,0.,-0.951056516295154));
#21811=DIRECTION('ref_axis',(-0.951056516295154,0.,0.309016994374947));
#21812=DIRECTION('',(-0.951056516295154,0.,0.309016994374947));
#21813=DIRECTION('',(0.,1.,0.));
#21814=DIRECTION('',(0.,1.,0.));
#21815=DIRECTION('center_axis',(0.,1.,0.));
#21816=DIRECTION('ref_axis',(1.,0.,0.));
#21817=DIRECTION('center_axis',(0.,1.,0.));
#21818=DIRECTION('ref_axis',(1.,0.,0.));
#21819=DIRECTION('',(0.,-1.,0.));
#21820=DIRECTION('',(0.,1.,0.));
#21821=DIRECTION('center_axis',(6.12323399573677E-17,0.,-1.));
#21822=DIRECTION('ref_axis',(-1.,0.,-6.12323399573677E-17));
#21823=DIRECTION('',(-1.,0.,-6.12323399573677E-17));
#21824=DIRECTION('',(0.,1.,0.));
#21825=DIRECTION('',(0.,1.,0.));
#21826=DIRECTION('center_axis',(0.,1.,0.));
#21827=DIRECTION('ref_axis',(1.,0.,0.));
#21828=DIRECTION('center_axis',(0.,1.,0.));
#21829=DIRECTION('ref_axis',(1.,0.,0.));
#21830=DIRECTION('',(0.,-1.,0.));
#21831=DIRECTION('',(0.,1.,0.));
#21832=DIRECTION('center_axis',(0.309016994374948,0.,-0.951056516295154));
#21833=DIRECTION('ref_axis',(-0.951056516295154,0.,-0.309016994374948));
#21834=DIRECTION('',(-0.951056516295154,0.,-0.309016994374948));
#21835=DIRECTION('',(0.,1.,0.));
#21836=DIRECTION('',(0.,1.,0.));
#21837=DIRECTION('center_axis',(0.,1.,0.));
#21838=DIRECTION('ref_axis',(1.,0.,0.));
#21839=DIRECTION('center_axis',(0.,1.,0.));
#21840=DIRECTION('ref_axis',(1.,0.,0.));
#21841=DIRECTION('',(0.,-1.,0.));
#21842=DIRECTION('',(0.,1.,0.));
#21843=DIRECTION('center_axis',(0.587785252292473,0.,-0.809016994374947));
#21844=DIRECTION('ref_axis',(-0.809016994374947,0.,-0.587785252292473));
#21845=DIRECTION('',(-0.809016994374947,0.,-0.587785252292473));
#21846=DIRECTION('',(0.,1.,0.));
#21847=DIRECTION('',(0.,1.,0.));
#21848=DIRECTION('center_axis',(0.,1.,0.));
#21849=DIRECTION('ref_axis',(1.,0.,0.));
#21850=DIRECTION('center_axis',(0.,1.,0.));
#21851=DIRECTION('ref_axis',(1.,0.,0.));
#21852=DIRECTION('',(0.,-1.,0.));
#21853=DIRECTION('',(0.,1.,0.));
#21854=DIRECTION('center_axis',(0.809016994374947,0.,-0.587785252292473));
#21855=DIRECTION('ref_axis',(-0.587785252292473,0.,-0.809016994374947));
#21856=DIRECTION('',(-0.587785252292473,0.,-0.809016994374947));
#21857=DIRECTION('',(0.,1.,0.));
#21858=DIRECTION('',(0.,1.,0.));
#21859=DIRECTION('center_axis',(0.,1.,0.));
#21860=DIRECTION('ref_axis',(1.,0.,0.));
#21861=DIRECTION('center_axis',(0.,1.,0.));
#21862=DIRECTION('ref_axis',(1.,0.,0.));
#21863=DIRECTION('',(0.,-1.,0.));
#21864=DIRECTION('',(0.,1.,0.));
#21865=DIRECTION('center_axis',(0.951056516295154,0.,-0.309016994374947));
#21866=DIRECTION('ref_axis',(-0.309016994374947,0.,-0.951056516295154));
#21867=DIRECTION('',(-0.309016994374947,0.,-0.951056516295154));
#21868=DIRECTION('',(0.,1.,0.));
#21869=DIRECTION('',(0.,1.,0.));
#21870=DIRECTION('center_axis',(0.,1.,0.));
#21871=DIRECTION('ref_axis',(1.,0.,0.));
#21872=DIRECTION('center_axis',(0.,1.,0.));
#21873=DIRECTION('ref_axis',(1.,0.,0.));
#21874=DIRECTION('',(0.,-1.,0.));
#21875=DIRECTION('',(0.,1.,0.));
#21876=DIRECTION('center_axis',(1.,0.,0.));
#21877=DIRECTION('ref_axis',(0.,0.,-1.));
#21878=DIRECTION('',(0.,0.,-1.));
#21879=DIRECTION('',(0.,1.,0.));
#21880=DIRECTION('',(0.,1.,0.));
#21881=DIRECTION('center_axis',(0.,1.,0.));
#21882=DIRECTION('ref_axis',(1.,0.,0.));
#21883=DIRECTION('center_axis',(0.,1.,0.));
#21884=DIRECTION('ref_axis',(1.,0.,0.));
#21885=DIRECTION('center_axis',(0.,1.,0.));
#21886=DIRECTION('ref_axis',(1.,0.,0.));
#21887=DIRECTION('axis',(0.,0.,1.));
#21888=DIRECTION('refdir',(1.,0.,0.));
#21889=DIRECTION('axis',(0.,0.,1.));
#21890=DIRECTION('refdir',(1.,0.,0.));
#21891=DIRECTION('center_axis',(-0.996917333733128,0.,0.0784590957278455));
#21892=DIRECTION('ref_axis',(0.0784590957278455,0.,0.996917333733128));
#21893=DIRECTION('',(0.,-1.,0.));
#21894=DIRECTION('',(0.0784590957278455,0.,0.996917333733128));
#21895=DIRECTION('',(0.,1.,0.));
#21896=DIRECTION('',(-0.0784590957278455,0.,-0.996917333733128));
#21897=DIRECTION('center_axis',(0.,1.,0.));
#21898=DIRECTION('ref_axis',(1.,0.,0.));
#21899=DIRECTION('center_axis',(0.,-1.,0.));
#21900=DIRECTION('ref_axis',(1.,0.,0.));
#21901=DIRECTION('',(-0.996917333733128,0.,0.0784590957278476));
#21902=DIRECTION('',(0.0784590957278442,0.,0.996917333733128));
#21903=DIRECTION('center_axis',(0.996917333733128,0.,-0.0784590957278442));
#21904=DIRECTION('ref_axis',(-0.0784590957278442,0.,-0.996917333733128));
#21905=DIRECTION('',(0.,1.,0.));
#21906=DIRECTION('',(0.,1.,0.));
#21907=DIRECTION('',(-0.0784590957278442,0.,-0.996917333733128));
#21908=DIRECTION('center_axis',(0.0784590957278476,0.,0.996917333733128));
#21909=DIRECTION('ref_axis',(0.996917333733128,0.,-0.0784590957278476));
#21910=DIRECTION('',(0.996917333733128,0.,-0.0784590957278476));
#21911=DIRECTION('center_axis',(0.,1.,0.));
#21912=DIRECTION('ref_axis',(0.,0.,1.));
#21913=DIRECTION('center_axis',(0.,1.,0.));
#21914=DIRECTION('ref_axis',(1.,0.,0.));
#21915=DIRECTION('center_axis',(0.,1.,0.));
#21916=DIRECTION('ref_axis',(1.,0.,0.));
#21917=DIRECTION('center_axis',(0.,1.,0.));
#21918=DIRECTION('ref_axis',(1.,0.,0.));
#21919=DIRECTION('',(0.,-1.,0.));
#21920=DIRECTION('center_axis',(0.,1.,0.));
#21921=DIRECTION('ref_axis',(1.,0.,0.));
#21922=DIRECTION('center_axis',(0.,1.,0.));
#21923=DIRECTION('ref_axis',(1.,0.,0.));
#21924=DIRECTION('center_axis',(0.,1.,0.));
#21925=DIRECTION('ref_axis',(1.,0.,0.));
#21926=DIRECTION('axis',(0.,0.,1.));
#21927=DIRECTION('refdir',(1.,0.,0.));
#21928=DIRECTION('center_axis',(0.,0.,1.));
#21929=DIRECTION('ref_axis',(1.,0.,0.));
#21930=DIRECTION('',(0.,1.,0.));
#21931=DIRECTION('center_axis',(0.,0.,1.));
#21932=DIRECTION('ref_axis',(1.,0.,0.));
#21933=DIRECTION('center_axis',(0.,0.,1.));
#21934=DIRECTION('ref_axis',(1.,0.,0.));
#21935=DIRECTION('center_axis',(0.,0.,1.));
#21936=DIRECTION('ref_axis',(1.,0.,0.));
#21937=DIRECTION('',(0.,0.,1.));
#21938=DIRECTION('center_axis',(0.,0.,1.));
#21939=DIRECTION('ref_axis',(1.,0.,0.));
#21940=DIRECTION('center_axis',(0.,0.,1.));
#21941=DIRECTION('ref_axis',(1.,0.,0.));
#21942=DIRECTION('',(0.,-1.,0.));
#21943=DIRECTION('center_axis',(0.,1.,0.));
#21944=DIRECTION('ref_axis',(1.,0.,0.));
#21945=DIRECTION('center_axis',(0.,-1.,0.));
#21946=DIRECTION('ref_axis',(1.,0.,0.));
#21947=DIRECTION('',(0.,-1.,0.));
#21948=DIRECTION('center_axis',(0.,-1.,0.));
#21949=DIRECTION('ref_axis',(1.,0.,0.));
#21950=DIRECTION('center_axis',(0.,1.,0.));
#21951=DIRECTION('ref_axis',(1.,0.,0.));
#21952=DIRECTION('center_axis',(0.,1.,0.));
#21953=DIRECTION('ref_axis',(1.,0.,0.));
#21954=DIRECTION('',(0.,-1.,0.));
#21955=DIRECTION('center_axis',(0.,1.,0.));
#21956=DIRECTION('ref_axis',(1.,0.,0.));
#21957=DIRECTION('center_axis',(0.,1.,0.));
#21958=DIRECTION('ref_axis',(1.,0.,0.));
#21959=DIRECTION('center_axis',(0.,1.,0.));
#21960=DIRECTION('ref_axis',(1.,0.,0.));
#21961=DIRECTION('axis',(0.,0.,1.));
#21962=DIRECTION('refdir',(1.,0.,0.));
#21963=DIRECTION('center_axis',(0.,0.,1.));
#21964=DIRECTION('ref_axis',(1.,0.,0.));
#21965=DIRECTION('',(0.,1.,0.));
#21966=DIRECTION('center_axis',(0.,0.,1.));
#21967=DIRECTION('ref_axis',(1.,0.,0.));
#21968=DIRECTION('center_axis',(0.,0.,1.));
#21969=DIRECTION('ref_axis',(1.,0.,0.));
#21970=DIRECTION('center_axis',(0.,0.,1.));
#21971=DIRECTION('ref_axis',(1.,0.,0.));
#21972=DIRECTION('',(0.,0.,1.));
#21973=DIRECTION('center_axis',(0.,0.,1.));
#21974=DIRECTION('ref_axis',(1.,0.,0.));
#21975=DIRECTION('center_axis',(0.,0.,1.));
#21976=DIRECTION('ref_axis',(1.,0.,0.));
#21977=DIRECTION('',(0.,-1.,0.));
#21978=DIRECTION('center_axis',(0.,1.,0.));
#21979=DIRECTION('ref_axis',(1.,0.,0.));
#21980=DIRECTION('center_axis',(0.,-1.,0.));
#21981=DIRECTION('ref_axis',(1.,0.,0.));
#21982=DIRECTION('',(0.,-1.,0.));
#21983=DIRECTION('center_axis',(0.,-1.,0.));
#21984=DIRECTION('ref_axis',(1.,0.,0.));
#21985=DIRECTION('center_axis',(0.,1.,0.));
#21986=DIRECTION('ref_axis',(1.,0.,0.));
#21987=DIRECTION('center_axis',(0.,1.,0.));
#21988=DIRECTION('ref_axis',(1.,0.,0.));
#21989=DIRECTION('',(0.,-1.,0.));
#21990=DIRECTION('center_axis',(0.,1.,0.));
#21991=DIRECTION('ref_axis',(1.,0.,0.));
#21992=DIRECTION('center_axis',(0.,1.,0.));
#21993=DIRECTION('ref_axis',(1.,0.,0.));
#21994=DIRECTION('center_axis',(0.,1.,0.));
#21995=DIRECTION('ref_axis',(1.,0.,0.));
#21996=DIRECTION('axis',(0.,0.,1.));
#21997=DIRECTION('refdir',(1.,0.,0.));
#21998=DIRECTION('center_axis',(0.,1.,0.));
#21999=DIRECTION('ref_axis',(1.,0.,0.));
#22000=DIRECTION('center_axis',(0.,-1.,0.));
#22001=DIRECTION('ref_axis',(1.,0.,0.));
#22002=DIRECTION('',(0.,-1.,0.));
#22003=DIRECTION('center_axis',(0.,-1.,0.));
#22004=DIRECTION('ref_axis',(1.,0.,0.));
#22005=DIRECTION('center_axis',(0.,1.,0.));
#22006=DIRECTION('ref_axis',(1.,0.,0.));
#22007=DIRECTION('center_axis',(0.,1.,0.));
#22008=DIRECTION('ref_axis',(1.,0.,0.));
#22009=DIRECTION('',(0.,-1.,0.));
#22010=DIRECTION('center_axis',(0.,1.,0.));
#22011=DIRECTION('ref_axis',(1.,0.,0.));
#22012=DIRECTION('center_axis',(0.,1.,0.));
#22013=DIRECTION('ref_axis',(1.,0.,0.));
#22014=DIRECTION('center_axis',(0.,1.,0.));
#22015=DIRECTION('ref_axis',(1.,0.,0.));
#22016=DIRECTION('axis',(0.,0.,1.));
#22017=DIRECTION('refdir',(1.,0.,0.));
#22018=DIRECTION('center_axis',(0.,1.,0.));
#22019=DIRECTION('ref_axis',(1.,0.,0.));
#22020=DIRECTION('center_axis',(0.,-1.,0.));
#22021=DIRECTION('ref_axis',(1.,0.,0.));
#22022=DIRECTION('',(0.,-1.,0.));
#22023=DIRECTION('center_axis',(0.,-1.,0.));
#22024=DIRECTION('ref_axis',(1.,0.,0.));
#22025=DIRECTION('center_axis',(0.,1.,0.));
#22026=DIRECTION('ref_axis',(1.,0.,0.));
#22027=DIRECTION('center_axis',(0.,1.,0.));
#22028=DIRECTION('ref_axis',(1.,0.,0.));
#22029=DIRECTION('',(0.,-1.,0.));
#22030=DIRECTION('center_axis',(0.,1.,0.));
#22031=DIRECTION('ref_axis',(1.,0.,0.));
#22032=DIRECTION('center_axis',(0.,1.,0.));
#22033=DIRECTION('ref_axis',(1.,0.,0.));
#22034=DIRECTION('center_axis',(0.,1.,0.));
#22035=DIRECTION('ref_axis',(1.,0.,0.));
#22036=DIRECTION('axis',(0.,0.,1.));
#22037=DIRECTION('refdir',(1.,0.,0.));
#22038=DIRECTION('center_axis',(0.,1.,0.));
#22039=DIRECTION('ref_axis',(1.,0.,0.));
#22040=DIRECTION('center_axis',(0.,-1.,0.));
#22041=DIRECTION('ref_axis',(1.,0.,0.));
#22042=DIRECTION('',(0.,-1.,0.));
#22043=DIRECTION('center_axis',(0.,-1.,0.));
#22044=DIRECTION('ref_axis',(1.,0.,0.));
#22045=DIRECTION('center_axis',(0.,1.,0.));
#22046=DIRECTION('ref_axis',(1.,0.,0.));
#22047=DIRECTION('center_axis',(0.,1.,0.));
#22048=DIRECTION('ref_axis',(1.,0.,0.));
#22049=DIRECTION('',(0.,-1.,0.));
#22050=DIRECTION('center_axis',(0.,1.,0.));
#22051=DIRECTION('ref_axis',(1.,0.,0.));
#22052=DIRECTION('center_axis',(0.,1.,0.));
#22053=DIRECTION('ref_axis',(1.,0.,0.));
#22054=DIRECTION('center_axis',(0.,1.,0.));
#22055=DIRECTION('ref_axis',(1.,0.,0.));
#22056=DIRECTION('axis',(0.,0.,1.));
#22057=DIRECTION('refdir',(1.,0.,0.));
#22058=DIRECTION('center_axis',(0.,1.,0.));
#22059=DIRECTION('ref_axis',(1.,0.,0.));
#22060=DIRECTION('center_axis',(0.,-1.,0.));
#22061=DIRECTION('ref_axis',(1.,0.,0.));
#22062=DIRECTION('',(0.,-1.,0.));
#22063=DIRECTION('center_axis',(0.,-1.,0.));
#22064=DIRECTION('ref_axis',(1.,0.,0.));
#22065=DIRECTION('center_axis',(0.,1.,0.));
#22066=DIRECTION('ref_axis',(1.,0.,0.));
#22067=DIRECTION('center_axis',(0.,1.,0.));
#22068=DIRECTION('ref_axis',(1.,0.,0.));
#22069=DIRECTION('',(0.,-1.,0.));
#22070=DIRECTION('center_axis',(0.,1.,0.));
#22071=DIRECTION('ref_axis',(1.,0.,0.));
#22072=DIRECTION('center_axis',(0.,1.,0.));
#22073=DIRECTION('ref_axis',(1.,0.,0.));
#22074=DIRECTION('center_axis',(0.,1.,0.));
#22075=DIRECTION('ref_axis',(1.,0.,0.));
#22076=DIRECTION('axis',(0.,0.,1.));
#22077=DIRECTION('refdir',(1.,0.,0.));
#22078=DIRECTION('center_axis',(0.866025403784439,0.,-0.5));
#22079=DIRECTION('ref_axis',(0.5,0.,0.866025403784439));
#22080=DIRECTION('',(0.5,0.,0.866025403784439));
#22081=DIRECTION('',(0.,-1.,0.));
#22082=DIRECTION('',(0.5,0.,0.866025403784439));
#22083=DIRECTION('',(0.,-1.,0.));
#22084=DIRECTION('center_axis',(1.92296268638356E-16,0.,-1.));
#22085=DIRECTION('ref_axis',(1.,0.,1.92296268638356E-16));
#22086=DIRECTION('',(1.,0.,1.92296268638356E-16));
#22087=DIRECTION('',(0.,-1.,0.));
#22088=DIRECTION('',(1.,0.,1.92296268638356E-16));
#22089=DIRECTION('center_axis',(-0.866025403784439,0.,-0.5));
#22090=DIRECTION('ref_axis',(0.5,0.,-0.866025403784439));
#22091=DIRECTION('',(0.5,0.,-0.866025403784439));
#22092=DIRECTION('',(0.,-1.,0.));
#22093=DIRECTION('',(0.5,0.,-0.866025403784438));
#22094=DIRECTION('center_axis',(-0.866025403784439,0.,0.5));
#22095=DIRECTION('ref_axis',(-0.5,0.,-0.866025403784439));
#22096=DIRECTION('',(-0.5,0.,-0.866025403784439));
#22097=DIRECTION('',(0.,-1.,0.));
#22098=DIRECTION('',(-0.5,0.,-0.866025403784439));
#22099=DIRECTION('center_axis',(-1.92296268638356E-16,0.,1.));
#22100=DIRECTION('ref_axis',(-1.,0.,-1.92296268638356E-16));
#22101=DIRECTION('',(-1.,0.,-1.92296268638356E-16));
#22102=DIRECTION('',(0.,-1.,0.));
#22103=DIRECTION('',(-1.,0.,-1.92296268638356E-16));
#22104=DIRECTION('center_axis',(0.866025403784439,0.,0.5));
#22105=DIRECTION('ref_axis',(-0.5,0.,0.866025403784439));
#22106=DIRECTION('',(-0.5,0.,0.866025403784439));
#22107=DIRECTION('',(-0.5,0.,0.866025403784439));
#22108=DIRECTION('center_axis',(0.,-1.,0.));
#22109=DIRECTION('ref_axis',(0.,0.,-1.));
#22110=DIRECTION('center_axis',(0.,1.,0.));
#22111=DIRECTION('ref_axis',(0.,0.,1.));
#22112=DIRECTION('center_axis',(0.,-1.,0.));
#22113=DIRECTION('ref_axis',(1.,0.,0.));
#22114=DIRECTION('center_axis',(0.,-1.,0.));
#22115=DIRECTION('ref_axis',(1.,0.,0.));
#22116=DIRECTION('center_axis',(0.,-1.,0.));
#22117=DIRECTION('ref_axis',(1.,0.,0.));
#22118=DIRECTION('',(0.707106781186547,0.707106781186548,8.65956056235493E-17));
#22119=DIRECTION('center_axis',(0.,-1.,0.));
#22120=DIRECTION('ref_axis',(1.,0.,0.));
#22121=DIRECTION('center_axis',(0.,1.,0.));
#22122=DIRECTION('ref_axis',(1.,0.,0.));
#22123=DIRECTION('',(0.,1.,0.));
#22124=DIRECTION('center_axis',(0.,1.,0.));
#22125=DIRECTION('ref_axis',(1.,0.,0.));
#22126=DIRECTION('center_axis',(0.,-1.,0.));
#22127=DIRECTION('ref_axis',(1.,0.,0.));
#22128=DIRECTION('',(-0.707106781186547,0.707106781186548,-8.65956056235493E-17));
#22129=DIRECTION('center_axis',(0.,-1.,0.));
#22130=DIRECTION('ref_axis',(0.,0.,-1.));
#22131=DIRECTION('',(0.,0.,1.));
#22132=DIRECTION('',(1.,0.,0.));
#22133=DIRECTION('',(0.,0.,1.));
#22134=DIRECTION('',(1.,0.,0.));
#22135=DIRECTION('',(0.,0.,1.));
#22136=DIRECTION('',(1.,0.,0.));
#22137=DIRECTION('',(0.,0.,1.));
#22138=DIRECTION('',(1.,0.,0.));
#22139=DIRECTION('',(0.,0.,1.));
#22140=DIRECTION('',(1.,0.,0.));
#22141=DIRECTION('',(0.,0.,1.));
#22142=DIRECTION('',(1.,0.,0.));
#22143=DIRECTION('',(0.,0.,1.));
#22144=DIRECTION('',(1.,0.,0.));
#22145=DIRECTION('',(0.,-1.,2.22044604925031E-16));
#22146=DIRECTION('',(1.,0.,0.));
#22147=DIRECTION('',(0.,-1.,2.22044604925031E-16));
#22148=DIRECTION('',(1.,0.,0.));
#22149=DIRECTION('',(0.,0.,1.));
#22150=DIRECTION('',(1.,0.,0.));
#22151=DIRECTION('',(0.,0.,-1.));
#22152=DIRECTION('',(0.,1.,0.));
#22153=DIRECTION('axis',(0.,0.,1.));
#22154=DIRECTION('refdir',(1.,0.,0.));
#22155=DIRECTION('center_axis',(1.,0.,0.));
#22156=DIRECTION('ref_axis',(0.,0.,-1.));
#22157=DIRECTION('',(0.,0.,1.));
#22158=DIRECTION('',(0.,1.,0.));
#22159=DIRECTION('',(0.,0.,-1.));
#22160=DIRECTION('',(0.,-1.,0.));
#22161=DIRECTION('center_axis',(0.,0.,-1.));
#22162=DIRECTION('ref_axis',(-1.,0.,0.));
#22163=DIRECTION('',(1.,0.,0.));
#22164=DIRECTION('',(0.,-1.,0.));
#22165=DIRECTION('',(-1.,0.,0.));
#22166=DIRECTION('center_axis',(-1.,0.,0.));
#22167=DIRECTION('ref_axis',(0.,0.,1.));
#22168=DIRECTION('',(0.,0.,-1.));
#22169=DIRECTION('',(0.,1.,0.));
#22170=DIRECTION('',(0.,0.,1.));
#22171=DIRECTION('center_axis',(0.,1.,0.));
#22172=DIRECTION('ref_axis',(1.,0.,0.));
#22173=DIRECTION('center_axis',(0.,-1.,0.));
#22174=DIRECTION('ref_axis',(1.,0.,0.));
#22175=DIRECTION('',(-0.309016994374948,0.,0.951056516295154));
#22176=DIRECTION('center_axis',(0.,-1.,0.));
#22177=DIRECTION('ref_axis',(1.,0.,0.));
#22178=DIRECTION('',(-0.453990499739547,0.,0.891006524188368));
#22179=DIRECTION('center_axis',(0.,-1.,0.));
#22180=DIRECTION('ref_axis',(1.,0.,0.));
#22181=DIRECTION('',(-0.587785252292473,0.,0.809016994374947));
#22182=DIRECTION('center_axis',(0.,-1.,0.));
#22183=DIRECTION('ref_axis',(1.,0.,0.));
#22184=DIRECTION('',(-0.707106781186548,0.,0.707106781186547));
#22185=DIRECTION('center_axis',(0.,-1.,0.));
#22186=DIRECTION('ref_axis',(1.,0.,0.));
#22187=DIRECTION('',(-0.809016994374948,0.,0.587785252292473));
#22188=DIRECTION('center_axis',(0.,-1.,0.));
#22189=DIRECTION('ref_axis',(1.,0.,0.));
#22190=DIRECTION('',(-0.891006524188368,0.,0.453990499739547));
#22191=DIRECTION('center_axis',(0.,-1.,0.));
#22192=DIRECTION('ref_axis',(1.,0.,0.));
#22193=DIRECTION('',(-0.951056516295154,0.,0.309016994374947));
#22194=DIRECTION('center_axis',(0.,-1.,0.));
#22195=DIRECTION('ref_axis',(1.,0.,0.));
#22196=DIRECTION('',(-0.987688340595138,0.,0.156434465040231));
#22197=DIRECTION('center_axis',(0.,-1.,0.));
#22198=DIRECTION('ref_axis',(1.,0.,0.));
#22199=DIRECTION('',(-1.,0.,-1.83697019872103E-16));
#22200=DIRECTION('center_axis',(0.,-1.,0.));
#22201=DIRECTION('ref_axis',(1.,0.,0.));
#22202=DIRECTION('',(-0.987688340595138,0.,-0.156434465040231));
#22203=DIRECTION('center_axis',(0.,-1.,0.));
#22204=DIRECTION('ref_axis',(1.,0.,0.));
#22205=DIRECTION('',(-0.951056516295154,0.,-0.309016994374948));
#22206=DIRECTION('center_axis',(0.,-1.,0.));
#22207=DIRECTION('ref_axis',(1.,0.,0.));
#22208=DIRECTION('',(-0.891006524188368,0.,-0.453990499739547));
#22209=DIRECTION('center_axis',(0.,-1.,0.));
#22210=DIRECTION('ref_axis',(1.,0.,0.));
#22211=DIRECTION('',(-0.809016994374947,0.,-0.587785252292473));
#22212=DIRECTION('center_axis',(0.,-1.,0.));
#22213=DIRECTION('ref_axis',(1.,0.,0.));
#22214=DIRECTION('',(-0.707106781186547,0.,-0.707106781186548));
#22215=DIRECTION('center_axis',(0.,-1.,0.));
#22216=DIRECTION('ref_axis',(1.,0.,0.));
#22217=DIRECTION('',(-0.587785252292473,0.,-0.809016994374948));
#22218=DIRECTION('center_axis',(0.,-1.,0.));
#22219=DIRECTION('ref_axis',(1.,0.,0.));
#22220=DIRECTION('',(-0.453990499739547,0.,-0.891006524188368));
#22221=DIRECTION('center_axis',(0.,-1.,0.));
#22222=DIRECTION('ref_axis',(1.,0.,0.));
#22223=DIRECTION('',(-0.309016994374947,0.,-0.951056516295154));
#22224=DIRECTION('center_axis',(0.,-1.,0.));
#22225=DIRECTION('ref_axis',(1.,0.,0.));
#22226=DIRECTION('',(-0.156434465040231,0.,-0.987688340595138));
#22227=DIRECTION('center_axis',(0.,-1.,0.));
#22228=DIRECTION('ref_axis',(1.,0.,0.));
#22229=DIRECTION('',(1.22464679914735E-16,0.,-1.));
#22230=DIRECTION('center_axis',(0.,-1.,0.));
#22231=DIRECTION('ref_axis',(1.,0.,0.));
#22232=DIRECTION('',(0.156434465040231,0.,-0.987688340595138));
#22233=DIRECTION('center_axis',(0.,-1.,0.));
#22234=DIRECTION('ref_axis',(1.,0.,0.));
#22235=DIRECTION('',(0.309016994374948,0.,-0.951056516295154));
#22236=DIRECTION('center_axis',(0.,-1.,0.));
#22237=DIRECTION('ref_axis',(1.,0.,0.));
#22238=DIRECTION('',(0.453990499739547,0.,-0.891006524188368));
#22239=DIRECTION('center_axis',(0.,-1.,0.));
#22240=DIRECTION('ref_axis',(1.,0.,0.));
#22241=DIRECTION('',(0.587785252292473,0.,-0.809016994374947));
#22242=DIRECTION('center_axis',(0.,-1.,0.));
#22243=DIRECTION('ref_axis',(1.,0.,0.));
#22244=DIRECTION('',(0.707106781186548,0.,-0.707106781186547));
#22245=DIRECTION('center_axis',(0.,-1.,0.));
#22246=DIRECTION('ref_axis',(1.,0.,0.));
#22247=DIRECTION('',(0.809016994374948,0.,-0.587785252292473));
#22248=DIRECTION('center_axis',(0.,-1.,0.));
#22249=DIRECTION('ref_axis',(1.,0.,0.));
#22250=DIRECTION('',(0.891006524188368,0.,-0.453990499739547));
#22251=DIRECTION('center_axis',(0.,-1.,0.));
#22252=DIRECTION('ref_axis',(1.,0.,0.));
#22253=DIRECTION('',(0.951056516295154,0.,-0.309016994374947));
#22254=DIRECTION('center_axis',(0.,-1.,0.));
#22255=DIRECTION('ref_axis',(1.,0.,0.));
#22256=DIRECTION('',(0.987688340595138,0.,-0.156434465040231));
#22257=DIRECTION('center_axis',(0.,-1.,0.));
#22258=DIRECTION('ref_axis',(1.,0.,0.));
#22259=DIRECTION('',(1.,0.,6.12323399573677E-17));
#22260=DIRECTION('center_axis',(0.,-1.,0.));
#22261=DIRECTION('ref_axis',(1.,0.,0.));
#22262=DIRECTION('',(0.987688340595138,0.,0.156434465040231));
#22263=DIRECTION('center_axis',(0.,-1.,0.));
#22264=DIRECTION('ref_axis',(1.,0.,0.));
#22265=DIRECTION('',(0.951056516295154,0.,0.309016994374948));
#22266=DIRECTION('center_axis',(0.,-1.,0.));
#22267=DIRECTION('ref_axis',(1.,0.,0.));
#22268=DIRECTION('',(0.891006524188368,0.,0.453990499739547));
#22269=DIRECTION('center_axis',(0.,-1.,0.));
#22270=DIRECTION('ref_axis',(1.,0.,0.));
#22271=DIRECTION('',(0.809016994374947,0.,0.587785252292473));
#22272=DIRECTION('center_axis',(0.,-1.,0.));
#22273=DIRECTION('ref_axis',(1.,0.,0.));
#22274=DIRECTION('',(0.707106781186547,0.,0.707106781186548));
#22275=DIRECTION('center_axis',(0.,-1.,0.));
#22276=DIRECTION('ref_axis',(1.,0.,0.));
#22277=DIRECTION('',(0.587785252292473,0.,0.809016994374947));
#22278=DIRECTION('center_axis',(0.,-1.,0.));
#22279=DIRECTION('ref_axis',(1.,0.,0.));
#22280=DIRECTION('',(0.453990499739547,0.,0.891006524188368));
#22281=DIRECTION('center_axis',(0.,-1.,0.));
#22282=DIRECTION('ref_axis',(1.,0.,0.));
#22283=DIRECTION('',(0.309016994374947,0.,0.951056516295154));
#22284=DIRECTION('center_axis',(0.,-1.,0.));
#22285=DIRECTION('ref_axis',(1.,0.,0.));
#22286=DIRECTION('',(0.156434465040231,0.,0.987688340595138));
#22287=DIRECTION('center_axis',(0.,-1.,0.));
#22288=DIRECTION('ref_axis',(1.,0.,0.));
#22289=DIRECTION('',(0.,0.,1.));
#22290=DIRECTION('center_axis',(0.,-1.,0.));
#22291=DIRECTION('ref_axis',(1.,0.,0.));
#22292=DIRECTION('',(-0.156434465040231,0.,0.987688340595138));
#22293=DIRECTION('center_axis',(0.,1.,0.));
#22294=DIRECTION('ref_axis',(1.,0.,0.));
#22295=DIRECTION('center_axis',(0.,1.,0.));
#22296=DIRECTION('ref_axis',(6.12323399573677E-17,0.,1.));
#22297=DIRECTION('center_axis',(0.,-1.,0.));
#22298=DIRECTION('ref_axis',(1.,0.,0.));
#22299=DIRECTION('center_axis',(0.,1.,0.));
#22300=DIRECTION('ref_axis',(1.,0.,0.));
#22301=DIRECTION('center_axis',(0.,1.,0.));
#22302=DIRECTION('ref_axis',(1.,0.,0.));
#22303=DIRECTION('',(0.,-1.,0.));
#22304=DIRECTION('center_axis',(0.,-1.,0.));
#22305=DIRECTION('ref_axis',(1.,0.,0.));
#22306=DIRECTION('center_axis',(0.,1.,0.));
#22307=DIRECTION('ref_axis',(1.,0.,0.));
#22308=DIRECTION('',(0.,1.,0.));
#22309=DIRECTION('',(0.,1.,0.));
#22310=DIRECTION('center_axis',(0.987688340595138,0.,0.156434465040231));
#22311=DIRECTION('ref_axis',(0.156434465040231,0.,-0.987688340595138));
#22312=DIRECTION('',(0.156434465040231,0.,-0.987688340595138));
#22313=DIRECTION('center_axis',(0.,1.,0.));
#22314=DIRECTION('ref_axis',(1.,0.,0.));
#22315=DIRECTION('center_axis',(0.,1.,0.));
#22316=DIRECTION('ref_axis',(1.,0.,0.));
#22317=DIRECTION('',(0.,1.,0.));
#22318=DIRECTION('',(0.,1.,0.));
#22319=DIRECTION('center_axis',(0.951056516295154,0.,0.309016994374948));
#22320=DIRECTION('ref_axis',(0.309016994374948,0.,-0.951056516295154));
#22321=DIRECTION('',(0.309016994374948,0.,-0.951056516295154));
#22322=DIRECTION('center_axis',(0.,1.,0.));
#22323=DIRECTION('ref_axis',(1.,0.,0.));
#22324=DIRECTION('center_axis',(0.,1.,0.));
#22325=DIRECTION('ref_axis',(1.,0.,0.));
#22326=DIRECTION('',(0.,1.,0.));
#22327=DIRECTION('',(0.,1.,0.));
#22328=DIRECTION('center_axis',(0.891006524188368,0.,0.453990499739547));
#22329=DIRECTION('ref_axis',(0.453990499739547,0.,-0.891006524188368));
#22330=DIRECTION('',(0.453990499739547,0.,-0.891006524188368));
#22331=DIRECTION('center_axis',(0.,1.,0.));
#22332=DIRECTION('ref_axis',(1.,0.,0.));
#22333=DIRECTION('center_axis',(0.,1.,0.));
#22334=DIRECTION('ref_axis',(1.,0.,0.));
#22335=DIRECTION('',(0.,1.,0.));
#22336=DIRECTION('',(0.,1.,0.));
#22337=DIRECTION('center_axis',(0.809016994374947,0.,0.587785252292473));
#22338=DIRECTION('ref_axis',(0.587785252292473,0.,-0.809016994374947));
#22339=DIRECTION('',(0.587785252292473,0.,-0.809016994374947));
#22340=DIRECTION('center_axis',(0.,1.,0.));
#22341=DIRECTION('ref_axis',(1.,0.,0.));
#22342=DIRECTION('center_axis',(0.,1.,0.));
#22343=DIRECTION('ref_axis',(1.,0.,0.));
#22344=DIRECTION('',(0.,1.,0.));
#22345=DIRECTION('',(0.,1.,0.));
#22346=DIRECTION('center_axis',(0.707106781186547,0.,0.707106781186548));
#22347=DIRECTION('ref_axis',(0.707106781186548,0.,-0.707106781186547));
#22348=DIRECTION('',(0.707106781186548,0.,-0.707106781186547));
#22349=DIRECTION('center_axis',(0.,1.,0.));
#22350=DIRECTION('ref_axis',(1.,0.,0.));
#22351=DIRECTION('center_axis',(0.,1.,0.));
#22352=DIRECTION('ref_axis',(1.,0.,0.));
#22353=DIRECTION('',(0.,1.,0.));
#22354=DIRECTION('',(0.,1.,0.));
#22355=DIRECTION('center_axis',(0.587785252292473,0.,0.809016994374948));
#22356=DIRECTION('ref_axis',(0.809016994374948,0.,-0.587785252292473));
#22357=DIRECTION('',(0.809016994374948,0.,-0.587785252292473));
#22358=DIRECTION('center_axis',(0.,1.,0.));
#22359=DIRECTION('ref_axis',(1.,0.,0.));
#22360=DIRECTION('center_axis',(0.,1.,0.));
#22361=DIRECTION('ref_axis',(1.,0.,0.));
#22362=DIRECTION('',(0.,1.,0.));
#22363=DIRECTION('',(0.,1.,0.));
#22364=DIRECTION('center_axis',(0.453990499739547,0.,0.891006524188368));
#22365=DIRECTION('ref_axis',(0.891006524188368,0.,-0.453990499739547));
#22366=DIRECTION('',(0.891006524188368,0.,-0.453990499739547));
#22367=DIRECTION('center_axis',(0.,1.,0.));
#22368=DIRECTION('ref_axis',(1.,0.,0.));
#22369=DIRECTION('center_axis',(0.,1.,0.));
#22370=DIRECTION('ref_axis',(1.,0.,0.));
#22371=DIRECTION('',(0.,1.,0.));
#22372=DIRECTION('',(0.,1.,0.));
#22373=DIRECTION('center_axis',(0.309016994374947,0.,0.951056516295154));
#22374=DIRECTION('ref_axis',(0.951056516295154,0.,-0.309016994374947));
#22375=DIRECTION('',(0.951056516295154,0.,-0.309016994374947));
#22376=DIRECTION('center_axis',(0.,1.,0.));
#22377=DIRECTION('ref_axis',(1.,0.,0.));
#22378=DIRECTION('center_axis',(0.,1.,0.));
#22379=DIRECTION('ref_axis',(1.,0.,0.));
#22380=DIRECTION('',(0.,1.,0.));
#22381=DIRECTION('',(0.,1.,0.));
#22382=DIRECTION('center_axis',(0.156434465040231,0.,0.987688340595138));
#22383=DIRECTION('ref_axis',(0.987688340595138,0.,-0.156434465040231));
#22384=DIRECTION('',(0.987688340595138,0.,-0.156434465040231));
#22385=DIRECTION('center_axis',(0.,1.,0.));
#22386=DIRECTION('ref_axis',(1.,0.,0.));
#22387=DIRECTION('center_axis',(0.,1.,0.));
#22388=DIRECTION('ref_axis',(1.,0.,0.));
#22389=DIRECTION('',(0.,1.,0.));
#22390=DIRECTION('',(0.,1.,0.));
#22391=DIRECTION('center_axis',(-1.83697019872103E-16,0.,1.));
#22392=DIRECTION('ref_axis',(1.,0.,1.83697019872103E-16));
#22393=DIRECTION('',(1.,0.,1.83697019872103E-16));
#22394=DIRECTION('center_axis',(0.,1.,0.));
#22395=DIRECTION('ref_axis',(1.,0.,0.));
#22396=DIRECTION('center_axis',(0.,1.,0.));
#22397=DIRECTION('ref_axis',(1.,0.,0.));
#22398=DIRECTION('',(0.,1.,0.));
#22399=DIRECTION('',(0.,1.,0.));
#22400=DIRECTION('center_axis',(-0.156434465040231,0.,0.987688340595138));
#22401=DIRECTION('ref_axis',(0.987688340595138,0.,0.156434465040231));
#22402=DIRECTION('',(0.987688340595138,0.,0.156434465040231));
#22403=DIRECTION('center_axis',(0.,1.,0.));
#22404=DIRECTION('ref_axis',(1.,0.,0.));
#22405=DIRECTION('center_axis',(0.,1.,0.));
#22406=DIRECTION('ref_axis',(1.,0.,0.));
#22407=DIRECTION('',(0.,1.,0.));
#22408=DIRECTION('',(0.,1.,0.));
#22409=DIRECTION('center_axis',(-0.309016994374948,0.,0.951056516295154));
#22410=DIRECTION('ref_axis',(0.951056516295154,0.,0.309016994374948));
#22411=DIRECTION('',(0.951056516295154,0.,0.309016994374948));
#22412=DIRECTION('center_axis',(0.,1.,0.));
#22413=DIRECTION('ref_axis',(1.,0.,0.));
#22414=DIRECTION('center_axis',(0.,1.,0.));
#22415=DIRECTION('ref_axis',(1.,0.,0.));
#22416=DIRECTION('',(0.,1.,0.));
#22417=DIRECTION('',(0.,1.,0.));
#22418=DIRECTION('center_axis',(-0.453990499739547,0.,0.891006524188368));
#22419=DIRECTION('ref_axis',(0.891006524188368,0.,0.453990499739547));
#22420=DIRECTION('',(0.891006524188368,0.,0.453990499739547));
#22421=DIRECTION('center_axis',(0.,1.,0.));
#22422=DIRECTION('ref_axis',(1.,0.,0.));
#22423=DIRECTION('center_axis',(0.,1.,0.));
#22424=DIRECTION('ref_axis',(1.,0.,0.));
#22425=DIRECTION('',(0.,1.,0.));
#22426=DIRECTION('',(0.,1.,0.));
#22427=DIRECTION('center_axis',(-0.587785252292473,0.,0.809016994374947));
#22428=DIRECTION('ref_axis',(0.809016994374947,0.,0.587785252292473));
#22429=DIRECTION('',(0.809016994374947,0.,0.587785252292473));
#22430=DIRECTION('center_axis',(0.,1.,0.));
#22431=DIRECTION('ref_axis',(1.,0.,0.));
#22432=DIRECTION('center_axis',(0.,1.,0.));
#22433=DIRECTION('ref_axis',(1.,0.,0.));
#22434=DIRECTION('',(0.,1.,0.));
#22435=DIRECTION('',(0.,1.,0.));
#22436=DIRECTION('center_axis',(-0.707106781186548,0.,0.707106781186547));
#22437=DIRECTION('ref_axis',(0.707106781186547,0.,0.707106781186548));
#22438=DIRECTION('',(0.707106781186547,0.,0.707106781186548));
#22439=DIRECTION('center_axis',(0.,1.,0.));
#22440=DIRECTION('ref_axis',(1.,0.,0.));
#22441=DIRECTION('center_axis',(0.,1.,0.));
#22442=DIRECTION('ref_axis',(1.,0.,0.));
#22443=DIRECTION('',(0.,1.,0.));
#22444=DIRECTION('',(0.,1.,0.));
#22445=DIRECTION('center_axis',(-0.809016994374948,0.,0.587785252292473));
#22446=DIRECTION('ref_axis',(0.587785252292473,0.,0.809016994374948));
#22447=DIRECTION('',(0.587785252292473,0.,0.809016994374948));
#22448=DIRECTION('center_axis',(0.,1.,0.));
#22449=DIRECTION('ref_axis',(1.,0.,0.));
#22450=DIRECTION('center_axis',(0.,1.,0.));
#22451=DIRECTION('ref_axis',(1.,0.,0.));
#22452=DIRECTION('',(0.,1.,0.));
#22453=DIRECTION('',(0.,1.,0.));
#22454=DIRECTION('center_axis',(-0.891006524188368,0.,0.453990499739547));
#22455=DIRECTION('ref_axis',(0.453990499739547,0.,0.891006524188368));
#22456=DIRECTION('',(0.453990499739547,0.,0.891006524188368));
#22457=DIRECTION('center_axis',(0.,1.,0.));
#22458=DIRECTION('ref_axis',(1.,0.,0.));
#22459=DIRECTION('center_axis',(0.,1.,0.));
#22460=DIRECTION('ref_axis',(1.,0.,0.));
#22461=DIRECTION('',(0.,1.,0.));
#22462=DIRECTION('',(0.,1.,0.));
#22463=DIRECTION('center_axis',(-0.951056516295154,0.,0.309016994374947));
#22464=DIRECTION('ref_axis',(0.309016994374947,0.,0.951056516295154));
#22465=DIRECTION('',(0.309016994374947,0.,0.951056516295154));
#22466=DIRECTION('center_axis',(0.,1.,0.));
#22467=DIRECTION('ref_axis',(1.,0.,0.));
#22468=DIRECTION('center_axis',(0.,1.,0.));
#22469=DIRECTION('ref_axis',(1.,0.,0.));
#22470=DIRECTION('',(0.,1.,0.));
#22471=DIRECTION('',(0.,1.,0.));
#22472=DIRECTION('center_axis',(-0.987688340595138,0.,0.156434465040231));
#22473=DIRECTION('ref_axis',(0.156434465040231,0.,0.987688340595138));
#22474=DIRECTION('',(0.156434465040231,0.,0.987688340595138));
#22475=DIRECTION('center_axis',(0.,1.,0.));
#22476=DIRECTION('ref_axis',(1.,0.,0.));
#22477=DIRECTION('center_axis',(0.,1.,0.));
#22478=DIRECTION('ref_axis',(1.,0.,0.));
#22479=DIRECTION('',(0.,1.,0.));
#22480=DIRECTION('',(0.,1.,0.));
#22481=DIRECTION('center_axis',(-1.,0.,-1.22464679914735E-16));
#22482=DIRECTION('ref_axis',(-1.22464679914735E-16,0.,1.));
#22483=DIRECTION('',(-1.22464679914735E-16,0.,1.));
#22484=DIRECTION('center_axis',(0.,1.,0.));
#22485=DIRECTION('ref_axis',(1.,0.,0.));
#22486=DIRECTION('center_axis',(0.,1.,0.));
#22487=DIRECTION('ref_axis',(1.,0.,0.));
#22488=DIRECTION('',(0.,1.,0.));
#22489=DIRECTION('',(0.,1.,0.));
#22490=DIRECTION('center_axis',(-0.987688340595138,0.,-0.156434465040231));
#22491=DIRECTION('ref_axis',(-0.156434465040231,0.,0.987688340595138));
#22492=DIRECTION('',(-0.156434465040231,0.,0.987688340595138));
#22493=DIRECTION('center_axis',(0.,1.,0.));
#22494=DIRECTION('ref_axis',(1.,0.,0.));
#22495=DIRECTION('center_axis',(0.,1.,0.));
#22496=DIRECTION('ref_axis',(1.,0.,0.));
#22497=DIRECTION('',(0.,1.,0.));
#22498=DIRECTION('',(0.,1.,0.));
#22499=DIRECTION('center_axis',(-0.951056516295154,0.,-0.309016994374948));
#22500=DIRECTION('ref_axis',(-0.309016994374948,0.,0.951056516295154));
#22501=DIRECTION('',(-0.309016994374948,0.,0.951056516295154));
#22502=DIRECTION('center_axis',(0.,1.,0.));
#22503=DIRECTION('ref_axis',(1.,0.,0.));
#22504=DIRECTION('center_axis',(0.,1.,0.));
#22505=DIRECTION('ref_axis',(1.,0.,0.));
#22506=DIRECTION('',(0.,1.,0.));
#22507=DIRECTION('',(0.,1.,0.));
#22508=DIRECTION('center_axis',(-0.891006524188368,0.,-0.453990499739547));
#22509=DIRECTION('ref_axis',(-0.453990499739547,0.,0.891006524188368));
#22510=DIRECTION('',(-0.453990499739547,0.,0.891006524188368));
#22511=DIRECTION('center_axis',(0.,1.,0.));
#22512=DIRECTION('ref_axis',(1.,0.,0.));
#22513=DIRECTION('center_axis',(0.,1.,0.));
#22514=DIRECTION('ref_axis',(1.,0.,0.));
#22515=DIRECTION('',(0.,1.,0.));
#22516=DIRECTION('',(0.,1.,0.));
#22517=DIRECTION('center_axis',(-0.809016994374947,0.,-0.587785252292473));
#22518=DIRECTION('ref_axis',(-0.587785252292473,0.,0.809016994374947));
#22519=DIRECTION('',(-0.587785252292473,0.,0.809016994374947));
#22520=DIRECTION('center_axis',(0.,1.,0.));
#22521=DIRECTION('ref_axis',(1.,0.,0.));
#22522=DIRECTION('center_axis',(0.,1.,0.));
#22523=DIRECTION('ref_axis',(1.,0.,0.));
#22524=DIRECTION('',(0.,1.,0.));
#22525=DIRECTION('',(0.,1.,0.));
#22526=DIRECTION('center_axis',(-0.707106781186547,0.,-0.707106781186548));
#22527=DIRECTION('ref_axis',(-0.707106781186548,0.,0.707106781186547));
#22528=DIRECTION('',(-0.707106781186548,0.,0.707106781186547));
#22529=DIRECTION('center_axis',(0.,1.,0.));
#22530=DIRECTION('ref_axis',(1.,0.,0.));
#22531=DIRECTION('center_axis',(0.,1.,0.));
#22532=DIRECTION('ref_axis',(1.,0.,0.));
#22533=DIRECTION('',(0.,1.,0.));
#22534=DIRECTION('',(0.,1.,0.));
#22535=DIRECTION('center_axis',(-0.587785252292473,0.,-0.809016994374948));
#22536=DIRECTION('ref_axis',(-0.809016994374948,0.,0.587785252292473));
#22537=DIRECTION('',(-0.809016994374948,0.,0.587785252292473));
#22538=DIRECTION('center_axis',(0.,1.,0.));
#22539=DIRECTION('ref_axis',(1.,0.,0.));
#22540=DIRECTION('center_axis',(0.,1.,0.));
#22541=DIRECTION('ref_axis',(1.,0.,0.));
#22542=DIRECTION('',(0.,1.,0.));
#22543=DIRECTION('',(0.,1.,0.));
#22544=DIRECTION('center_axis',(-0.453990499739547,0.,-0.891006524188368));
#22545=DIRECTION('ref_axis',(-0.891006524188368,0.,0.453990499739547));
#22546=DIRECTION('',(-0.891006524188368,0.,0.453990499739547));
#22547=DIRECTION('center_axis',(0.,1.,0.));
#22548=DIRECTION('ref_axis',(1.,0.,0.));
#22549=DIRECTION('center_axis',(0.,1.,0.));
#22550=DIRECTION('ref_axis',(1.,0.,0.));
#22551=DIRECTION('',(0.,1.,0.));
#22552=DIRECTION('',(0.,1.,0.));
#22553=DIRECTION('center_axis',(-0.309016994374947,0.,-0.951056516295154));
#22554=DIRECTION('ref_axis',(-0.951056516295154,0.,0.309016994374947));
#22555=DIRECTION('',(-0.951056516295154,0.,0.309016994374947));
#22556=DIRECTION('center_axis',(0.,1.,0.));
#22557=DIRECTION('ref_axis',(1.,0.,0.));
#22558=DIRECTION('center_axis',(0.,1.,0.));
#22559=DIRECTION('ref_axis',(1.,0.,0.));
#22560=DIRECTION('',(0.,1.,0.));
#22561=DIRECTION('',(0.,1.,0.));
#22562=DIRECTION('center_axis',(-0.156434465040231,0.,-0.987688340595138));
#22563=DIRECTION('ref_axis',(-0.987688340595138,0.,0.156434465040231));
#22564=DIRECTION('',(-0.987688340595138,0.,0.156434465040231));
#22565=DIRECTION('center_axis',(0.,1.,0.));
#22566=DIRECTION('ref_axis',(1.,0.,0.));
#22567=DIRECTION('center_axis',(0.,1.,0.));
#22568=DIRECTION('ref_axis',(1.,0.,0.));
#22569=DIRECTION('',(0.,1.,0.));
#22570=DIRECTION('',(0.,1.,0.));
#22571=DIRECTION('center_axis',(6.12323399573677E-17,0.,-1.));
#22572=DIRECTION('ref_axis',(-1.,0.,-6.12323399573677E-17));
#22573=DIRECTION('',(-1.,0.,-6.12323399573677E-17));
#22574=DIRECTION('center_axis',(0.,1.,0.));
#22575=DIRECTION('ref_axis',(1.,0.,0.));
#22576=DIRECTION('center_axis',(0.,1.,0.));
#22577=DIRECTION('ref_axis',(1.,0.,0.));
#22578=DIRECTION('',(0.,1.,0.));
#22579=DIRECTION('',(0.,1.,0.));
#22580=DIRECTION('center_axis',(0.156434465040231,0.,-0.987688340595138));
#22581=DIRECTION('ref_axis',(-0.987688340595138,0.,-0.156434465040231));
#22582=DIRECTION('',(-0.987688340595138,0.,-0.156434465040231));
#22583=DIRECTION('center_axis',(0.,1.,0.));
#22584=DIRECTION('ref_axis',(1.,0.,0.));
#22585=DIRECTION('center_axis',(0.,1.,0.));
#22586=DIRECTION('ref_axis',(1.,0.,0.));
#22587=DIRECTION('',(0.,1.,0.));
#22588=DIRECTION('',(0.,1.,0.));
#22589=DIRECTION('center_axis',(0.309016994374948,0.,-0.951056516295154));
#22590=DIRECTION('ref_axis',(-0.951056516295154,0.,-0.309016994374948));
#22591=DIRECTION('',(-0.951056516295154,0.,-0.309016994374948));
#22592=DIRECTION('center_axis',(0.,1.,0.));
#22593=DIRECTION('ref_axis',(1.,0.,0.));
#22594=DIRECTION('center_axis',(0.,1.,0.));
#22595=DIRECTION('ref_axis',(1.,0.,0.));
#22596=DIRECTION('',(0.,1.,0.));
#22597=DIRECTION('',(0.,1.,0.));
#22598=DIRECTION('center_axis',(0.453990499739547,0.,-0.891006524188368));
#22599=DIRECTION('ref_axis',(-0.891006524188368,0.,-0.453990499739547));
#22600=DIRECTION('',(-0.891006524188368,0.,-0.453990499739547));
#22601=DIRECTION('center_axis',(0.,1.,0.));
#22602=DIRECTION('ref_axis',(1.,0.,0.));
#22603=DIRECTION('center_axis',(0.,1.,0.));
#22604=DIRECTION('ref_axis',(1.,0.,0.));
#22605=DIRECTION('',(0.,1.,0.));
#22606=DIRECTION('',(0.,1.,0.));
#22607=DIRECTION('center_axis',(0.587785252292473,0.,-0.809016994374947));
#22608=DIRECTION('ref_axis',(-0.809016994374947,0.,-0.587785252292473));
#22609=DIRECTION('',(-0.809016994374947,0.,-0.587785252292473));
#22610=DIRECTION('center_axis',(0.,1.,0.));
#22611=DIRECTION('ref_axis',(1.,0.,0.));
#22612=DIRECTION('center_axis',(0.,1.,0.));
#22613=DIRECTION('ref_axis',(1.,0.,0.));
#22614=DIRECTION('',(0.,1.,0.));
#22615=DIRECTION('',(0.,1.,0.));
#22616=DIRECTION('center_axis',(0.707106781186548,0.,-0.707106781186547));
#22617=DIRECTION('ref_axis',(-0.707106781186547,0.,-0.707106781186548));
#22618=DIRECTION('',(-0.707106781186547,0.,-0.707106781186548));
#22619=DIRECTION('center_axis',(0.,1.,0.));
#22620=DIRECTION('ref_axis',(1.,0.,0.));
#22621=DIRECTION('center_axis',(0.,1.,0.));
#22622=DIRECTION('ref_axis',(1.,0.,0.));
#22623=DIRECTION('',(0.,1.,0.));
#22624=DIRECTION('',(0.,1.,0.));
#22625=DIRECTION('center_axis',(0.809016994374947,0.,-0.587785252292473));
#22626=DIRECTION('ref_axis',(-0.587785252292473,0.,-0.809016994374947));
#22627=DIRECTION('',(-0.587785252292473,0.,-0.809016994374947));
#22628=DIRECTION('center_axis',(0.,1.,0.));
#22629=DIRECTION('ref_axis',(1.,0.,0.));
#22630=DIRECTION('center_axis',(0.,1.,0.));
#22631=DIRECTION('ref_axis',(1.,0.,0.));
#22632=DIRECTION('',(0.,1.,0.));
#22633=DIRECTION('',(0.,1.,0.));
#22634=DIRECTION('center_axis',(0.891006524188368,0.,-0.453990499739547));
#22635=DIRECTION('ref_axis',(-0.453990499739547,0.,-0.891006524188368));
#22636=DIRECTION('',(-0.453990499739547,0.,-0.891006524188368));
#22637=DIRECTION('center_axis',(0.,1.,0.));
#22638=DIRECTION('ref_axis',(1.,0.,0.));
#22639=DIRECTION('center_axis',(0.,1.,0.));
#22640=DIRECTION('ref_axis',(1.,0.,0.));
#22641=DIRECTION('',(0.,1.,0.));
#22642=DIRECTION('',(0.,1.,0.));
#22643=DIRECTION('center_axis',(0.951056516295154,0.,-0.309016994374947));
#22644=DIRECTION('ref_axis',(-0.309016994374947,0.,-0.951056516295154));
#22645=DIRECTION('',(-0.309016994374947,0.,-0.951056516295154));
#22646=DIRECTION('center_axis',(0.,1.,0.));
#22647=DIRECTION('ref_axis',(1.,0.,0.));
#22648=DIRECTION('center_axis',(0.,1.,0.));
#22649=DIRECTION('ref_axis',(1.,0.,0.));
#22650=DIRECTION('',(0.,1.,0.));
#22651=DIRECTION('center_axis',(0.987688340595138,0.,-0.156434465040231));
#22652=DIRECTION('ref_axis',(-0.156434465040231,0.,-0.987688340595138));
#22653=DIRECTION('',(-0.156434465040231,0.,-0.987688340595138));
#22654=DIRECTION('',(0.,1.,0.));
#22655=DIRECTION('center_axis',(0.,1.,0.));
#22656=DIRECTION('ref_axis',(1.,0.,0.));
#22657=DIRECTION('center_axis',(0.,1.,0.));
#22658=DIRECTION('ref_axis',(1.,0.,0.));
#22659=DIRECTION('',(0.,1.,0.));
#22660=DIRECTION('',(0.,1.,0.));
#22661=DIRECTION('center_axis',(1.,0.,0.));
#22662=DIRECTION('ref_axis',(0.,0.,-1.));
#22663=DIRECTION('',(0.,0.,-1.));
#22664=DIRECTION('center_axis',(0.,1.,0.));
#22665=DIRECTION('ref_axis',(1.,0.,0.));
#22666=DIRECTION('center_axis',(0.,1.,0.));
#22667=DIRECTION('ref_axis',(1.,0.,0.));
#22668=DIRECTION('center_axis',(0.,1.,0.));
#22669=DIRECTION('ref_axis',(1.,0.,0.));
#22670=DIRECTION('axis',(0.,0.,1.));
#22671=DIRECTION('refdir',(1.,0.,0.));
#22672=DIRECTION('center_axis',(1.,0.,0.));
#22673=DIRECTION('ref_axis',(0.,0.,-1.));
#22674=DIRECTION('',(0.,-0.707106781186547,-0.707106781186548));
#22675=DIRECTION('',(0.,-1.,0.));
#22676=DIRECTION('',(0.,-0.707106781186547,0.707106781186548));
#22677=DIRECTION('',(0.,0.,1.));
#22678=DIRECTION('',(0.,0.707106781186547,0.707106781186548));
#22679=DIRECTION('',(0.,1.,0.));
#22680=DIRECTION('',(0.,0.707106781186547,-0.707106781186548));
#22681=DIRECTION('',(0.,0.,-1.));
#22682=DIRECTION('center_axis',(0.,0.707106781186548,-0.707106781186547));
#22683=DIRECTION('ref_axis',(-1.,0.,0.));
#22684=DIRECTION('',(1.,0.,0.));
#22685=DIRECTION('',(0.,-0.707106781186547,-0.707106781186548));
#22686=DIRECTION('',(-1.,0.,0.));
#22687=DIRECTION('center_axis',(0.,1.,0.));
#22688=DIRECTION('ref_axis',(-1.,0.,0.));
#22689=DIRECTION('',(-1.,0.,0.));
#22690=DIRECTION('',(0.,0.,-1.));
#22691=DIRECTION('center_axis',(0.,0.707106781186548,0.707106781186547));
#22692=DIRECTION('ref_axis',(1.,0.,0.));
#22693=DIRECTION('',(1.,0.,0.));
#22694=DIRECTION('',(0.,0.707106781186547,-0.707106781186548));
#22695=DIRECTION('center_axis',(0.,0.,1.));
#22696=DIRECTION('ref_axis',(1.,0.,0.));
#22697=DIRECTION('',(-1.,0.,0.));
#22698=DIRECTION('',(0.,1.,0.));
#22699=DIRECTION('center_axis',(1.,0.,0.));
#22700=DIRECTION('ref_axis',(0.,0.,-1.));
#22701=DIRECTION('',(0.,-0.707106781186547,0.707106781186548));
#22702=DIRECTION('',(0.,-1.,0.));
#22703=DIRECTION('',(0.,0.707106781186547,0.707106781186548));
#22704=DIRECTION('',(0.,0.,1.));
#22705=DIRECTION('center_axis',(0.,0.,1.));
#22706=DIRECTION('ref_axis',(1.,0.,0.));
#22707=DIRECTION('',(1.,0.,0.));
#22708=DIRECTION('center_axis',(0.,-0.707106781186548,0.707106781186547));
#22709=DIRECTION('ref_axis',(1.,0.,0.));
#22710=DIRECTION('',(1.,0.,0.));
#22711=DIRECTION('center_axis',(0.,-0.707106781186548,-0.707106781186547));
#22712=DIRECTION('ref_axis',(-1.,0.,0.));
#22713=DIRECTION('',(-1.,0.,0.));
#22714=DIRECTION('center_axis',(0.,-1.,0.));
#22715=DIRECTION('ref_axis',(1.,0.,0.));
#22716=DIRECTION('',(0.,0.,1.));
#22717=DIRECTION('',(1.,0.,0.));
#22718=DIRECTION('',(0.,0.,1.));
#22719=DIRECTION('',(1.,0.,0.));
#22720=DIRECTION('',(0.,0.,1.));
#22721=DIRECTION('',(1.,0.,0.));
#22722=DIRECTION('',(0.,0.,1.));
#22723=DIRECTION('',(1.,0.,0.));
#22724=DIRECTION('',(0.,0.,1.));
#22725=DIRECTION('',(1.,0.,0.));
#22726=DIRECTION('',(0.,0.,1.));
#22727=DIRECTION('',(1.,0.,0.));
#22728=DIRECTION('',(0.,0.,1.));
#22729=DIRECTION('',(1.,0.,0.));
#22730=DIRECTION('',(0.,0.,1.));
#22731=DIRECTION('',(1.,0.,0.));
#22732=DIRECTION('',(0.,-1.,2.22044604925031E-16));
#22733=DIRECTION('',(1.,0.,0.));
#22734=DIRECTION('',(0.,-1.,2.22044604925031E-16));
#22735=DIRECTION('',(1.,0.,0.));
#22736=DIRECTION('',(0.0784590957278449,0.,0.996917333733128));
#22737=DIRECTION('',(0.996917333733128,0.,-0.0784590957278449));
#22738=DIRECTION('',(-0.0784590957278449,0.,-0.996917333733128));
#22739=DIRECTION('',(0.,1.,0.));
#22740=DIRECTION('',(0.,0.,1.));
#22741=DIRECTION('',(1.,0.,0.));
#22742=DIRECTION('',(0.,0.,-1.));
#22743=DIRECTION('',(0.,1.,0.));
#22744=DIRECTION('',(0.,0.,1.));
#22745=DIRECTION('',(1.,0.,0.));
#22746=DIRECTION('',(0.,0.,1.));
#22747=DIRECTION('',(1.,0.,0.));
#22748=DIRECTION('',(0.,0.,1.));
#22749=DIRECTION('',(1.,0.,0.));
#22750=DIRECTION('',(0.,0.,1.));
#22751=DIRECTION('',(1.,0.,0.));
#22752=DIRECTION('',(0.,0.,1.));
#22753=DIRECTION('',(1.,0.,0.));
#22754=DIRECTION('',(0.,0.,1.));
#22755=DIRECTION('',(1.,0.,0.));
#22756=DIRECTION('',(0.,0.,1.));
#22757=DIRECTION('',(1.,0.,0.));
#22758=DIRECTION('',(0.,-1.,2.22044604925031E-16));
#22759=DIRECTION('',(1.,0.,0.));
#22760=DIRECTION('',(0.,-1.,2.22044604925031E-16));
#22761=DIRECTION('',(1.,0.,0.));
#22762=DIRECTION('',(0.0784590957278449,0.,0.996917333733128));
#22763=DIRECTION('',(0.996917333733128,0.,-0.0784590957278449));
#22764=DIRECTION('',(-0.0784590957278449,0.,-0.996917333733128));
#22765=DIRECTION('',(0.,1.,0.));
#22766=DIRECTION('',(0.,0.,1.));
#22767=DIRECTION('',(1.,0.,0.));
#22768=DIRECTION('',(0.,0.,1.));
#22769=DIRECTION('',(1.,0.,0.));
#22770=DIRECTION('',(0.,0.,1.));
#22771=DIRECTION('',(1.,0.,0.));
#22772=DIRECTION('',(0.,0.,1.));
#22773=DIRECTION('',(1.,0.,0.));
#22774=CARTESIAN_POINT('',(0.,0.,0.));
#22775=CARTESIAN_POINT('',(0.,0.,0.));
#22776=CARTESIAN_POINT('',(0.,0.,0.));
#22777=CARTESIAN_POINT('Origin',(15.,-3.5,-0.1));
#22778=CARTESIAN_POINT('',(14.75,-3.5,0.));
#22779=CARTESIAN_POINT('Origin',(15.,-3.5,0.));
#22780=CARTESIAN_POINT('',(14.75,-3.5,1.));
#22781=CARTESIAN_POINT('',(14.75,-3.5,-0.1));
#22782=CARTESIAN_POINT('Origin',(15.,-3.5,1.));
#22783=CARTESIAN_POINT('Origin',(-2.,3.5,-0.1));
#22784=CARTESIAN_POINT('',(-2.25,3.5,0.));
#22785=CARTESIAN_POINT('Origin',(-2.,3.5,0.));
#22786=CARTESIAN_POINT('',(-2.25,3.5,1.));
#22787=CARTESIAN_POINT('',(-2.25,3.5,-0.1));
#22788=CARTESIAN_POINT('Origin',(-2.,3.5,1.));
#22789=CARTESIAN_POINT('Origin',(-2.,-3.5,-0.1));
#22790=CARTESIAN_POINT('',(-2.25,-3.5,0.));
#22791=CARTESIAN_POINT('Origin',(-2.,-3.5,0.));
#22792=CARTESIAN_POINT('',(-2.25,-3.5,1.));
#22793=CARTESIAN_POINT('',(-2.25,-3.5,-0.1));
#22794=CARTESIAN_POINT('Origin',(-2.,-3.5,1.));
#22795=CARTESIAN_POINT('Origin',(15.,3.5,-0.1));
#22796=CARTESIAN_POINT('',(14.75,3.5,0.));
#22797=CARTESIAN_POINT('Origin',(15.,3.5,0.));
#22798=CARTESIAN_POINT('',(14.75,3.5,1.));
#22799=CARTESIAN_POINT('',(14.75,3.5,-0.1));
#22800=CARTESIAN_POINT('Origin',(15.,3.5,1.));
#22801=CARTESIAN_POINT('Origin',(18.5,8.5,0.));
#22802=CARTESIAN_POINT('',(18.5,8.5,0.));
#22803=CARTESIAN_POINT('',(-5.5,8.5,0.));
#22804=CARTESIAN_POINT('',(18.5,8.5,0.));
#22805=CARTESIAN_POINT('',(-5.5,8.5,1.));
#22806=CARTESIAN_POINT('',(-5.5,8.5,0.));
#22807=CARTESIAN_POINT('',(18.5,8.5,1.));
#22808=CARTESIAN_POINT('',(18.5,8.5,1.));
#22809=CARTESIAN_POINT('',(18.5,8.5,0.));
#22810=CARTESIAN_POINT('Origin',(18.5,-8.5,0.));
#22811=CARTESIAN_POINT('',(18.5,-8.5,0.));
#22812=CARTESIAN_POINT('',(18.5,-8.5,0.));
#22813=CARTESIAN_POINT('',(18.5,-8.5,1.));
#22814=CARTESIAN_POINT('',(18.5,-8.5,1.));
#22815=CARTESIAN_POINT('',(18.5,-8.5,0.));
#22816=CARTESIAN_POINT('Origin',(-5.5,-8.5,0.));
#22817=CARTESIAN_POINT('',(-5.5,-8.5,0.));
#22818=CARTESIAN_POINT('',(-5.5,-8.5,0.));
#22819=CARTESIAN_POINT('',(-5.5,-8.5,1.));
#22820=CARTESIAN_POINT('',(-5.5,-8.5,1.));
#22821=CARTESIAN_POINT('',(-5.5,-8.5,0.));
#22822=CARTESIAN_POINT('Origin',(-5.5,8.5,0.));
#22823=CARTESIAN_POINT('',(-5.5,8.5,0.));
#22824=CARTESIAN_POINT('',(-5.5,8.5,1.));
#22825=CARTESIAN_POINT('Origin',(6.5,0.,1.));
#22826=CARTESIAN_POINT('Origin',(6.5,0.,0.));
#22827=CARTESIAN_POINT('',(0.,0.,0.));
#22828=CARTESIAN_POINT('Origin',(10.161522368915,6.1,8.16152236891498));
#22829=CARTESIAN_POINT('',(9.99652236891498,6.1,8.16152236891498));
#22830=CARTESIAN_POINT('Origin',(10.161522368915,6.1,8.16152236891498));
#22831=CARTESIAN_POINT('',(9.99652236891498,7.5,8.16152236891498));
#22832=CARTESIAN_POINT('',(9.99652236891498,6.1,8.16152236891498));
#22833=CARTESIAN_POINT('Origin',(10.161522368915,7.5,8.16152236891498));
#22834=CARTESIAN_POINT('Origin',(10.161522368915,6.1,8.16152236891498));
#22835=CARTESIAN_POINT('Origin',(13.838477631085,6.1,8.16152236891498));
#22836=CARTESIAN_POINT('',(13.673477631085,6.1,8.16152236891498));
#22837=CARTESIAN_POINT('Origin',(13.838477631085,6.1,8.16152236891498));
#22838=CARTESIAN_POINT('',(13.673477631085,7.5,8.16152236891498));
#22839=CARTESIAN_POINT('',(13.673477631085,6.1,8.16152236891498));
#22840=CARTESIAN_POINT('Origin',(13.838477631085,7.5,8.16152236891498));
#22841=CARTESIAN_POINT('Origin',(13.838477631085,6.1,8.16152236891498));
#22842=CARTESIAN_POINT('Origin',(10.161522368915,-7.6,8.16152236891498));
#22843=CARTESIAN_POINT('',(9.99652236891498,-7.5,8.16152236891498));
#22844=CARTESIAN_POINT('Origin',(10.161522368915,-7.5,8.16152236891498));
#22845=CARTESIAN_POINT('',(9.99652236891498,-6.1,8.16152236891498));
#22846=CARTESIAN_POINT('',(9.99652236891498,-7.6,8.16152236891498));
#22847=CARTESIAN_POINT('Origin',(10.161522368915,-6.1,8.16152236891498));
#22848=CARTESIAN_POINT('Origin',(10.161522368915,-6.1,8.16152236891498));
#22849=CARTESIAN_POINT('Origin',(13.838477631085,-7.6,8.16152236891498));
#22850=CARTESIAN_POINT('',(13.673477631085,-7.5,8.16152236891498));
#22851=CARTESIAN_POINT('Origin',(13.838477631085,-7.5,8.16152236891498));
#22852=CARTESIAN_POINT('',(13.673477631085,-6.1,8.16152236891498));
#22853=CARTESIAN_POINT('',(13.673477631085,-7.6,8.16152236891498));
#22854=CARTESIAN_POINT('Origin',(13.838477631085,-6.1,8.16152236891498));
#22855=CARTESIAN_POINT('Origin',(13.838477631085,-6.1,8.16152236891498));
#22856=CARTESIAN_POINT('Origin',(12.,5.3,10.));
#22857=CARTESIAN_POINT('',(9.65,5.3,10.));
#22858=CARTESIAN_POINT('',(9.65,7.5,10.));
#22859=CARTESIAN_POINT('',(9.65,5.3,10.));
#22860=CARTESIAN_POINT('',(14.35,5.3,10.));
#22861=CARTESIAN_POINT('Origin',(12.,5.3,10.));
#22862=CARTESIAN_POINT('',(14.35,7.5,10.));
#22863=CARTESIAN_POINT('',(14.35,5.3,10.));
#22864=CARTESIAN_POINT('Origin',(12.,7.5,10.));
#22865=CARTESIAN_POINT('Origin',(12.,5.3,10.));
#22866=CARTESIAN_POINT('',(10.1,5.3,10.));
#22867=CARTESIAN_POINT('',(9.25,5.3,10.));
#22868=CARTESIAN_POINT('',(13.9,5.3,10.));
#22869=CARTESIAN_POINT('Origin',(12.,5.3,10.));
#22870=CARTESIAN_POINT('',(9.25,5.3,10.));
#22871=CARTESIAN_POINT('Origin',(17.,7.5,1.));
#22872=CARTESIAN_POINT('',(18.5,7.5,10.));
#22873=CARTESIAN_POINT('',(18.5,7.5,10.));
#22874=CARTESIAN_POINT('',(18.5,7.5,9.2));
#22875=CARTESIAN_POINT('',(18.5,7.5,9.2));
#22876=CARTESIAN_POINT('',(17.,7.5,9.2));
#22877=CARTESIAN_POINT('',(18.5,7.5,9.2));
#22878=CARTESIAN_POINT('',(17.,7.5,1.));
#22879=CARTESIAN_POINT('',(17.,7.5,1.));
#22880=CARTESIAN_POINT('',(-4.,7.5,1.));
#22881=CARTESIAN_POINT('',(17.,7.5,1.));
#22882=CARTESIAN_POINT('',(-4.,7.5,9.2));
#22883=CARTESIAN_POINT('',(-4.,7.5,1.));
#22884=CARTESIAN_POINT('',(-5.5,7.5,9.2));
#22885=CARTESIAN_POINT('',(-4.,7.5,9.2));
#22886=CARTESIAN_POINT('',(-5.5,7.5,10.));
#22887=CARTESIAN_POINT('',(-5.5,7.5,9.2));
#22888=CARTESIAN_POINT('',(-1.6,7.5,10.));
#22889=CARTESIAN_POINT('',(18.5,7.5,10.));
#22890=CARTESIAN_POINT('',(1.6,7.5,10.));
#22891=CARTESIAN_POINT('Origin',(0.,7.5,10.));
#22892=CARTESIAN_POINT('',(3.65,7.5,10.));
#22893=CARTESIAN_POINT('',(18.5,7.5,10.));
#22894=CARTESIAN_POINT('',(8.35,7.5,10.));
#22895=CARTESIAN_POINT('Origin',(6.,7.5,10.));
#22896=CARTESIAN_POINT('',(18.5,7.5,10.));
#22897=CARTESIAN_POINT('',(1.24921356237309,7.5,8.5857864376269));
#22898=CARTESIAN_POINT('Origin',(1.41421356237309,7.5,8.5857864376269));
#22899=CARTESIAN_POINT('',(-1.5792135623731,7.5,8.5857864376269));
#22900=CARTESIAN_POINT('Origin',(-1.4142135623731,7.5,8.5857864376269));
#22901=CARTESIAN_POINT('',(7.67347763108502,7.5,8.16152236891498));
#22902=CARTESIAN_POINT('Origin',(7.83847763108502,7.5,8.16152236891498));
#22903=CARTESIAN_POINT('',(3.99652236891498,7.5,8.16152236891498));
#22904=CARTESIAN_POINT('Origin',(4.16152236891498,7.5,8.16152236891498));
#22905=CARTESIAN_POINT('Origin',(6.5,0.,10.));
#22906=CARTESIAN_POINT('',(13.9,5.,10.));
#22907=CARTESIAN_POINT('',(13.9,-7.6,10.));
#22908=CARTESIAN_POINT('',(16.4,5.,10.));
#22909=CARTESIAN_POINT('',(11.45,5.,10.));
#22910=CARTESIAN_POINT('',(16.4,-5.,10.));
#22911=CARTESIAN_POINT('',(16.4,-2.5,10.));
#22912=CARTESIAN_POINT('',(13.9,-5.,10.));
#22913=CARTESIAN_POINT('',(1.65,-5.,10.));
#22914=CARTESIAN_POINT('',(13.9,-5.3,10.));
#22915=CARTESIAN_POINT('',(13.9,-7.6,10.));
#22916=CARTESIAN_POINT('',(14.35,-5.3,10.));
#22917=CARTESIAN_POINT('',(9.25,-5.3,10.));
#22918=CARTESIAN_POINT('',(14.35,-7.5,10.));
#22919=CARTESIAN_POINT('',(14.35,-7.6,10.));
#22920=CARTESIAN_POINT('',(18.5,-7.5,10.));
#22921=CARTESIAN_POINT('',(-5.5,-7.5,10.));
#22922=CARTESIAN_POINT('',(18.5,-7.5,10.));
#22923=CARTESIAN_POINT('',(17.6,3.,10.));
#22924=CARTESIAN_POINT('Origin',(17.75,3.,10.));
#22925=CARTESIAN_POINT('',(17.5,3.06161699786838E-17,10.));
#22926=CARTESIAN_POINT('Origin',(17.75,0.,10.));
#22927=CARTESIAN_POINT('',(17.5,-6.,10.));
#22928=CARTESIAN_POINT('Origin',(17.75,-6.,10.));
#22929=CARTESIAN_POINT('',(17.5,6.,10.));
#22930=CARTESIAN_POINT('Origin',(17.75,6.,10.));
#22931=CARTESIAN_POINT('',(17.6,-3.,10.));
#22932=CARTESIAN_POINT('Origin',(17.75,-3.,10.));
#22933=CARTESIAN_POINT('Origin',(12.,-7.6,10.));
#22934=CARTESIAN_POINT('',(9.65,-5.3,10.));
#22935=CARTESIAN_POINT('Origin',(12.,-5.3,10.));
#22936=CARTESIAN_POINT('',(9.65,-7.5,10.));
#22937=CARTESIAN_POINT('',(9.65,-7.6,10.));
#22938=CARTESIAN_POINT('Origin',(12.,-7.5,10.));
#22939=CARTESIAN_POINT('Origin',(12.,-5.3,10.));
#22940=CARTESIAN_POINT('',(10.1,-5.3,10.));
#22941=CARTESIAN_POINT('Origin',(12.,-5.3,10.));
#22942=CARTESIAN_POINT('',(9.25,-5.3,10.));
#22943=CARTESIAN_POINT('Origin',(-4.,-7.5,1.));
#22944=CARTESIAN_POINT('',(8.35,-7.5,10.));
#22945=CARTESIAN_POINT('',(-5.5,-7.5,10.));
#22946=CARTESIAN_POINT('',(3.65,-7.5,10.));
#22947=CARTESIAN_POINT('Origin',(6.,-7.5,10.));
#22948=CARTESIAN_POINT('',(1.6,-7.5,10.));
#22949=CARTESIAN_POINT('',(-5.5,-7.5,10.));
#22950=CARTESIAN_POINT('',(-1.6,-7.5,10.));
#22951=CARTESIAN_POINT('Origin',(0.,-7.5,10.));
#22952=CARTESIAN_POINT('',(-5.5,-7.5,10.));
#22953=CARTESIAN_POINT('',(-5.5,-7.5,10.));
#22954=CARTESIAN_POINT('',(-5.5,-7.5,9.2));
#22955=CARTESIAN_POINT('',(-5.5,-7.5,9.2));
#22956=CARTESIAN_POINT('',(-4.,-7.5,9.2));
#22957=CARTESIAN_POINT('',(-5.5,-7.5,9.2));
#22958=CARTESIAN_POINT('',(-4.,-7.5,1.));
#22959=CARTESIAN_POINT('',(-4.,-7.5,1.));
#22960=CARTESIAN_POINT('',(17.,-7.5,1.));
#22961=CARTESIAN_POINT('',(-4.,-7.5,1.));
#22962=CARTESIAN_POINT('',(17.,-7.5,9.2));
#22963=CARTESIAN_POINT('',(17.,-7.5,1.));
#22964=CARTESIAN_POINT('',(18.5,-7.5,9.2));
#22965=CARTESIAN_POINT('',(17.,-7.5,9.2));
#22966=CARTESIAN_POINT('',(18.5,-7.5,9.2));
#22967=CARTESIAN_POINT('',(3.99652236891498,-7.5,8.16152236891498));
#22968=CARTESIAN_POINT('Origin',(4.16152236891498,-7.5,8.16152236891498));
#22969=CARTESIAN_POINT('',(7.67347763108502,-7.5,8.16152236891498));
#22970=CARTESIAN_POINT('Origin',(7.83847763108502,-7.5,8.16152236891498));
#22971=CARTESIAN_POINT('',(1.24921356237309,-7.5,8.5857864376269));
#22972=CARTESIAN_POINT('Origin',(1.41421356237309,-7.5,8.5857864376269));
#22973=CARTESIAN_POINT('',(-1.5792135623731,-7.5,8.5857864376269));
#22974=CARTESIAN_POINT('Origin',(-1.4142135623731,-7.5,8.5857864376269));
#22975=CARTESIAN_POINT('Origin',(6.5,0.,10.));
#22976=CARTESIAN_POINT('',(10.1,-5.,10.));
#22977=CARTESIAN_POINT('',(10.1,-7.6,10.));
#22978=CARTESIAN_POINT('',(7.9,-5.,10.));
#22979=CARTESIAN_POINT('',(1.65,-5.,10.));
#22980=CARTESIAN_POINT('',(7.9,-5.3,10.));
#22981=CARTESIAN_POINT('',(7.9,-7.6,10.));
#22982=CARTESIAN_POINT('',(8.35,-5.3,10.));
#22983=CARTESIAN_POINT('',(6.25,-5.3,10.));
#22984=CARTESIAN_POINT('',(8.35,-7.6,10.));
#22985=CARTESIAN_POINT('Origin',(12.,-7.6,10.));
#22986=CARTESIAN_POINT('Origin',(12.,-5.,10.));
#22987=CARTESIAN_POINT('Origin',(12.,-7.6,10.));
#22988=CARTESIAN_POINT('',(10.1,5.,10.));
#22989=CARTESIAN_POINT('',(10.1,-7.6,10.));
#22990=CARTESIAN_POINT('Origin',(12.,5.,10.));
#22991=CARTESIAN_POINT('Origin',(16.4,5.,5.));
#22992=CARTESIAN_POINT('',(7.9,5.,10.));
#22993=CARTESIAN_POINT('',(11.45,5.,10.));
#22994=CARTESIAN_POINT('',(4.1,5.,10.));
#22995=CARTESIAN_POINT('Origin',(6.,5.,10.));
#22996=CARTESIAN_POINT('',(1.2,5.,10.));
#22997=CARTESIAN_POINT('',(11.45,5.,10.));
#22998=CARTESIAN_POINT('',(-1.2,5.,10.));
#22999=CARTESIAN_POINT('Origin',(0.,5.,10.));
#23000=CARTESIAN_POINT('',(-3.2,5.,10.));
#23001=CARTESIAN_POINT('',(11.45,5.,10.));
#23002=CARTESIAN_POINT('',(-3.2,5.,5.));
#23003=CARTESIAN_POINT('',(-3.2,5.,5.));
#23004=CARTESIAN_POINT('',(16.4,5.,5.));
#23005=CARTESIAN_POINT('',(16.4,5.,5.));
#23006=CARTESIAN_POINT('',(16.4,5.,5.));
#23007=CARTESIAN_POINT('Origin',(6.5,0.,10.));
#23008=CARTESIAN_POINT('',(8.35,5.3,10.));
#23009=CARTESIAN_POINT('',(8.35,5.3,10.));
#23010=CARTESIAN_POINT('',(7.9,5.3,10.));
#23011=CARTESIAN_POINT('',(6.25,5.3,10.));
#23012=CARTESIAN_POINT('',(7.9,-7.6,10.));
#23013=CARTESIAN_POINT('Origin',(4.16152236891498,6.1,8.16152236891498));
#23014=CARTESIAN_POINT('',(3.99652236891498,6.1,8.16152236891498));
#23015=CARTESIAN_POINT('Origin',(4.16152236891498,6.1,8.16152236891498));
#23016=CARTESIAN_POINT('',(3.99652236891498,6.1,8.16152236891498));
#23017=CARTESIAN_POINT('Origin',(4.16152236891498,6.1,8.16152236891498));
#23018=CARTESIAN_POINT('Origin',(7.83847763108502,6.1,8.16152236891498));
#23019=CARTESIAN_POINT('',(7.67347763108502,6.1,8.16152236891498));
#23020=CARTESIAN_POINT('Origin',(7.83847763108502,6.1,8.16152236891498));
#23021=CARTESIAN_POINT('',(7.67347763108502,6.1,8.16152236891498));
#23022=CARTESIAN_POINT('Origin',(7.83847763108502,6.1,8.16152236891498));
#23023=CARTESIAN_POINT('Origin',(4.16152236891498,-7.6,8.16152236891498));
#23024=CARTESIAN_POINT('',(3.99652236891498,-6.1,8.16152236891498));
#23025=CARTESIAN_POINT('',(3.99652236891498,-7.6,8.16152236891498));
#23026=CARTESIAN_POINT('Origin',(4.16152236891498,-6.1,8.16152236891498));
#23027=CARTESIAN_POINT('Origin',(4.16152236891498,-6.1,8.16152236891498));
#23028=CARTESIAN_POINT('Origin',(7.83847763108502,-7.6,8.16152236891498));
#23029=CARTESIAN_POINT('',(7.67347763108502,-6.1,8.16152236891498));
#23030=CARTESIAN_POINT('',(7.67347763108502,-7.6,8.16152236891498));
#23031=CARTESIAN_POINT('Origin',(7.83847763108502,-6.1,8.16152236891498));
#23032=CARTESIAN_POINT('Origin',(7.83847763108502,-6.1,8.16152236891498));
#23033=CARTESIAN_POINT('Origin',(6.,5.3,10.));
#23034=CARTESIAN_POINT('',(3.65,5.3,10.));
#23035=CARTESIAN_POINT('',(3.65,5.3,10.));
#23036=CARTESIAN_POINT('Origin',(6.,5.3,10.));
#23037=CARTESIAN_POINT('Origin',(6.,5.3,10.));
#23038=CARTESIAN_POINT('',(4.1,5.3,10.));
#23039=CARTESIAN_POINT('',(6.25,5.3,10.));
#23040=CARTESIAN_POINT('Origin',(6.,5.3,10.));
#23041=CARTESIAN_POINT('Origin',(6.,-7.6,10.));
#23042=CARTESIAN_POINT('',(3.65,-5.3,10.));
#23043=CARTESIAN_POINT('Origin',(6.,-5.3,10.));
#23044=CARTESIAN_POINT('',(3.65,-7.6,10.));
#23045=CARTESIAN_POINT('Origin',(6.,-5.3,10.));
#23046=CARTESIAN_POINT('',(4.1,-5.3,10.));
#23047=CARTESIAN_POINT('Origin',(6.,-5.3,10.));
#23048=CARTESIAN_POINT('',(6.25,-5.3,10.));
#23049=CARTESIAN_POINT('Origin',(6.5,0.,10.));
#23050=CARTESIAN_POINT('',(4.1,-5.,10.));
#23051=CARTESIAN_POINT('',(4.1,-7.6,10.));
#23052=CARTESIAN_POINT('',(1.2,-5.,10.));
#23053=CARTESIAN_POINT('',(1.65,-5.,10.));
#23054=CARTESIAN_POINT('',(1.2,-5.5,10.));
#23055=CARTESIAN_POINT('',(1.2,-7.6,10.));
#23056=CARTESIAN_POINT('',(1.6,-5.5,10.));
#23057=CARTESIAN_POINT('',(3.25,-5.5,10.));
#23058=CARTESIAN_POINT('',(1.6,-7.6,10.));
#23059=CARTESIAN_POINT('Origin',(6.,-7.6,10.));
#23060=CARTESIAN_POINT('',(4.1,-7.6,10.));
#23061=CARTESIAN_POINT('Origin',(6.,-7.6,10.));
#23062=CARTESIAN_POINT('Origin',(6.,-5.,10.));
#23063=CARTESIAN_POINT('Origin',(-3.2,-5.,5.));
#23064=CARTESIAN_POINT('',(16.4,-5.,5.));
#23065=CARTESIAN_POINT('',(16.4,-5.,5.));
#23066=CARTESIAN_POINT('',(-3.2,-5.,5.));
#23067=CARTESIAN_POINT('',(-3.2,-5.,5.));
#23068=CARTESIAN_POINT('',(-3.2,-5.,10.));
#23069=CARTESIAN_POINT('',(-3.2,-5.,5.));
#23070=CARTESIAN_POINT('',(-1.2,-5.,10.));
#23071=CARTESIAN_POINT('',(1.65,-5.,10.));
#23072=CARTESIAN_POINT('Origin',(0.,-5.,10.));
#23073=CARTESIAN_POINT('Origin',(6.5,0.,10.));
#23074=CARTESIAN_POINT('',(1.6,5.5,10.));
#23075=CARTESIAN_POINT('',(1.6,5.5,10.));
#23076=CARTESIAN_POINT('',(1.2,5.5,10.));
#23077=CARTESIAN_POINT('',(3.25,5.5,10.));
#23078=CARTESIAN_POINT('',(1.2,-7.6,10.));
#23079=CARTESIAN_POINT('Origin',(-1.4142135623731,6.1,8.5857864376269));
#23080=CARTESIAN_POINT('',(-1.5792135623731,6.1,8.5857864376269));
#23081=CARTESIAN_POINT('Origin',(-1.4142135623731,6.1,8.5857864376269));
#23082=CARTESIAN_POINT('',(-1.5792135623731,6.1,8.5857864376269));
#23083=CARTESIAN_POINT('Origin',(-1.4142135623731,6.1,8.5857864376269));
#23084=CARTESIAN_POINT('Origin',(1.41421356237309,6.1,8.5857864376269));
#23085=CARTESIAN_POINT('',(1.24921356237309,6.1,8.5857864376269));
#23086=CARTESIAN_POINT('Origin',(1.41421356237309,6.1,8.5857864376269));
#23087=CARTESIAN_POINT('',(1.24921356237309,6.1,8.5857864376269));
#23088=CARTESIAN_POINT('Origin',(1.41421356237309,6.1,8.5857864376269));
#23089=CARTESIAN_POINT('Origin',(-1.4142135623731,-7.6,8.5857864376269));
#23090=CARTESIAN_POINT('',(-1.5792135623731,-6.1,8.5857864376269));
#23091=CARTESIAN_POINT('',(-1.5792135623731,-7.6,8.5857864376269));
#23092=CARTESIAN_POINT('Origin',(-1.4142135623731,-6.1,8.5857864376269));
#23093=CARTESIAN_POINT('Origin',(-1.4142135623731,-6.1,8.5857864376269));
#23094=CARTESIAN_POINT('Origin',(1.41421356237309,-7.6,8.5857864376269));
#23095=CARTESIAN_POINT('',(1.24921356237309,-6.1,8.5857864376269));
#23096=CARTESIAN_POINT('',(1.24921356237309,-7.6,8.5857864376269));
#23097=CARTESIAN_POINT('Origin',(1.41421356237309,-6.1,8.5857864376269));
#23098=CARTESIAN_POINT('Origin',(1.41421356237309,-6.1,8.5857864376269));
#23099=CARTESIAN_POINT('Origin',(0.,5.5,10.));
#23100=CARTESIAN_POINT('',(-1.6,5.5,10.));
#23101=CARTESIAN_POINT('',(-1.6,5.5,10.));
#23102=CARTESIAN_POINT('Origin',(0.,5.5,10.));
#23103=CARTESIAN_POINT('Origin',(0.,5.5,10.));
#23104=CARTESIAN_POINT('',(-1.2,5.5,10.));
#23105=CARTESIAN_POINT('',(3.25,5.5,10.));
#23106=CARTESIAN_POINT('Origin',(0.,5.5,10.));
#23107=CARTESIAN_POINT('Origin',(6.5,0.,10.));
#23108=CARTESIAN_POINT('',(-5.5,7.5,10.));
#23109=CARTESIAN_POINT('',(-1.6,-5.5,10.));
#23110=CARTESIAN_POINT('',(-1.6,-7.6,10.));
#23111=CARTESIAN_POINT('',(-1.2,-5.5,10.));
#23112=CARTESIAN_POINT('',(3.25,-5.5,10.));
#23113=CARTESIAN_POINT('',(-1.2,-7.6,10.));
#23114=CARTESIAN_POINT('',(-3.2,2.5,10.));
#23115=CARTESIAN_POINT('',(-1.2,-7.6,10.));
#23116=CARTESIAN_POINT('',(-4.9,3.,10.));
#23117=CARTESIAN_POINT('Origin',(-4.75,3.,10.));
#23118=CARTESIAN_POINT('',(-5.,-6.,10.));
#23119=CARTESIAN_POINT('Origin',(-4.75,-6.,10.));
#23120=CARTESIAN_POINT('',(-5.,3.06161699786838E-17,10.));
#23121=CARTESIAN_POINT('Origin',(-4.75,0.,10.));
#23122=CARTESIAN_POINT('',(-5.,6.,10.));
#23123=CARTESIAN_POINT('Origin',(-4.75,6.,10.));
#23124=CARTESIAN_POINT('',(-4.9,-3.,10.));
#23125=CARTESIAN_POINT('Origin',(-4.75,-3.,10.));
#23126=CARTESIAN_POINT('Origin',(0.,-7.6,10.));
#23127=CARTESIAN_POINT('Origin',(0.,-5.5,10.));
#23128=CARTESIAN_POINT('Origin',(0.,-5.5,10.));
#23129=CARTESIAN_POINT('Origin',(0.,-5.5,10.));
#23130=CARTESIAN_POINT('Origin',(0.,-7.6,10.));
#23131=CARTESIAN_POINT('Origin',(0.,-7.6,10.));
#23132=CARTESIAN_POINT('Origin',(15.,-3.5,1.8));
#23133=CARTESIAN_POINT('',(14.4,-3.5,1.8));
#23134=CARTESIAN_POINT('Origin',(15.,-3.5,1.8));
#23135=CARTESIAN_POINT('',(14.4,-3.5,5.));
#23136=CARTESIAN_POINT('',(14.4,-3.5,1.8));
#23137=CARTESIAN_POINT('Origin',(15.,-3.5,5.));
#23138=CARTESIAN_POINT('Origin',(15.,-3.5,1.8));
#23139=CARTESIAN_POINT('',(14.67,-3.5,1.8));
#23140=CARTESIAN_POINT('Origin',(15.,-3.5,1.8));
#23141=CARTESIAN_POINT('Origin',(-2.,3.5,1.8));
#23142=CARTESIAN_POINT('',(-2.6,3.5,1.8));
#23143=CARTESIAN_POINT('Origin',(-2.,3.5,1.8));
#23144=CARTESIAN_POINT('',(-2.6,3.5,5.));
#23145=CARTESIAN_POINT('',(-2.6,3.5,1.8));
#23146=CARTESIAN_POINT('Origin',(-2.,3.5,5.));
#23147=CARTESIAN_POINT('Origin',(-2.,3.5,1.8));
#23148=CARTESIAN_POINT('',(-2.33,3.5,1.8));
#23149=CARTESIAN_POINT('Origin',(-2.,3.5,1.8));
#23150=CARTESIAN_POINT('Origin',(-2.,-3.5,1.8));
#23151=CARTESIAN_POINT('',(-2.6,-3.5,1.8));
#23152=CARTESIAN_POINT('Origin',(-2.,-3.5,1.8));
#23153=CARTESIAN_POINT('',(-2.6,-3.5,5.));
#23154=CARTESIAN_POINT('',(-2.6,-3.5,1.8));
#23155=CARTESIAN_POINT('Origin',(-2.,-3.5,5.));
#23156=CARTESIAN_POINT('Origin',(-2.,-3.5,1.8));
#23157=CARTESIAN_POINT('',(-2.33,-3.5,1.8));
#23158=CARTESIAN_POINT('Origin',(-2.,-3.5,1.8));
#23159=CARTESIAN_POINT('Origin',(15.,3.5,1.8));
#23160=CARTESIAN_POINT('',(14.4,3.5,1.8));
#23161=CARTESIAN_POINT('Origin',(15.,3.5,1.8));
#23162=CARTESIAN_POINT('',(14.4,3.5,5.));
#23163=CARTESIAN_POINT('',(14.4,3.5,1.8));
#23164=CARTESIAN_POINT('Origin',(15.,3.5,5.));
#23165=CARTESIAN_POINT('Origin',(15.,3.5,1.8));
#23166=CARTESIAN_POINT('',(14.67,3.5,1.8));
#23167=CARTESIAN_POINT('Origin',(15.,3.5,1.8));
#23168=CARTESIAN_POINT('Origin',(15.,-3.5,0.9));
#23169=CARTESIAN_POINT('',(14.67,-3.5,1.));
#23170=CARTESIAN_POINT('Origin',(15.,-3.5,1.));
#23171=CARTESIAN_POINT('',(14.67,-3.5,0.9));
#23172=CARTESIAN_POINT('Origin',(-2.,3.5,0.9));
#23173=CARTESIAN_POINT('',(-2.33,3.5,1.));
#23174=CARTESIAN_POINT('Origin',(-2.,3.5,1.));
#23175=CARTESIAN_POINT('',(-2.33,3.5,0.9));
#23176=CARTESIAN_POINT('Origin',(-2.,-3.5,0.9));
#23177=CARTESIAN_POINT('',(-2.33,-3.5,1.));
#23178=CARTESIAN_POINT('Origin',(-2.,-3.5,1.));
#23179=CARTESIAN_POINT('',(-2.33,-3.5,0.9));
#23180=CARTESIAN_POINT('Origin',(15.,3.5,0.9));
#23181=CARTESIAN_POINT('',(14.67,3.5,1.));
#23182=CARTESIAN_POINT('Origin',(15.,3.5,1.));
#23183=CARTESIAN_POINT('',(14.67,3.5,0.9));
#23184=CARTESIAN_POINT('Origin',(17.75,3.,9.5));
#23185=CARTESIAN_POINT('',(17.6,3.,9.5));
#23186=CARTESIAN_POINT('Origin',(17.75,3.,9.5));
#23187=CARTESIAN_POINT('',(17.6,3.,9.5));
#23188=CARTESIAN_POINT('Origin',(17.75,3.,9.5));
#23189=CARTESIAN_POINT('Origin',(17.75,-3.,9.5));
#23190=CARTESIAN_POINT('',(17.6,-3.,9.5));
#23191=CARTESIAN_POINT('Origin',(17.75,-3.,9.5));
#23192=CARTESIAN_POINT('',(17.6,-3.,9.5));
#23193=CARTESIAN_POINT('Origin',(17.75,-3.,9.5));
#23194=CARTESIAN_POINT('Origin',(-4.75,3.,9.5));
#23195=CARTESIAN_POINT('',(-4.9,3.,9.5));
#23196=CARTESIAN_POINT('Origin',(-4.75,3.,9.5));
#23197=CARTESIAN_POINT('',(-4.9,3.,9.5));
#23198=CARTESIAN_POINT('Origin',(-4.75,3.,9.5));
#23199=CARTESIAN_POINT('Origin',(-4.75,-3.,9.5));
#23200=CARTESIAN_POINT('',(-4.9,-3.,9.5));
#23201=CARTESIAN_POINT('Origin',(-4.75,-3.,9.5));
#23202=CARTESIAN_POINT('',(-4.9,-3.,9.5));
#23203=CARTESIAN_POINT('Origin',(-4.75,-3.,9.5));
#23204=CARTESIAN_POINT('Origin',(17.75,0.,9.1));
#23205=CARTESIAN_POINT('',(17.5,-3.06161699786838E-17,9.2));
#23206=CARTESIAN_POINT('Origin',(17.75,0.,9.2));
#23207=CARTESIAN_POINT('',(17.5,-3.06161699786838E-17,9.1));
#23208=CARTESIAN_POINT('Origin',(-4.75,-6.,9.1));
#23209=CARTESIAN_POINT('',(-5.,-6.,9.2));
#23210=CARTESIAN_POINT('Origin',(-4.75,-6.,9.2));
#23211=CARTESIAN_POINT('',(-5.,-6.,9.1));
#23212=CARTESIAN_POINT('Origin',(-4.75,0.,9.1));
#23213=CARTESIAN_POINT('',(-5.,-3.06161699786838E-17,9.2));
#23214=CARTESIAN_POINT('Origin',(-4.75,0.,9.2));
#23215=CARTESIAN_POINT('',(-5.,-3.06161699786838E-17,9.1));
#23216=CARTESIAN_POINT('Origin',(-4.75,6.,9.1));
#23217=CARTESIAN_POINT('',(-5.,6.,9.2));
#23218=CARTESIAN_POINT('Origin',(-4.75,6.,9.2));
#23219=CARTESIAN_POINT('',(-5.,6.,9.1));
#23220=CARTESIAN_POINT('Origin',(17.75,-6.,9.1));
#23221=CARTESIAN_POINT('',(17.5,-6.,9.2));
#23222=CARTESIAN_POINT('Origin',(17.75,-6.,9.2));
#23223=CARTESIAN_POINT('',(17.5,-6.,9.1));
#23224=CARTESIAN_POINT('Origin',(17.75,6.,9.1));
#23225=CARTESIAN_POINT('',(17.5,6.,9.2));
#23226=CARTESIAN_POINT('Origin',(17.75,6.,9.2));
#23227=CARTESIAN_POINT('',(17.5,6.,9.1));
#23228=CARTESIAN_POINT('Origin',(18.5,-7.5,9.2));
#23229=CARTESIAN_POINT('',(18.5,-7.5,9.2));
#23230=CARTESIAN_POINT('Origin',(17.75,0.,9.2));
#23231=CARTESIAN_POINT('',(17.,-3.75,9.2));
#23232=CARTESIAN_POINT('Origin',(17.,-7.5,1.));
#23233=CARTESIAN_POINT('',(17.,-7.5,1.));
#23234=CARTESIAN_POINT('Origin',(-5.5,7.5,9.2));
#23235=CARTESIAN_POINT('',(-5.5,7.5,9.2));
#23236=CARTESIAN_POINT('Origin',(-4.75,0.,9.2));
#23237=CARTESIAN_POINT('',(-4.,3.75,9.2));
#23238=CARTESIAN_POINT('Origin',(-3.2,5.,5.));
#23239=CARTESIAN_POINT('',(-3.2,5.,5.));
#23240=CARTESIAN_POINT('Origin',(16.4,-5.,5.));
#23241=CARTESIAN_POINT('',(16.4,-5.,5.));
#23242=CARTESIAN_POINT('Origin',(6.6,0.,5.));
#23243=CARTESIAN_POINT('Origin',(-4.,7.5,1.));
#23244=CARTESIAN_POINT('',(-4.,7.5,1.));
#23245=CARTESIAN_POINT('Origin',(6.5,0.,1.));
#23246=CARTESIAN_POINT('',(0.,0.,0.));
#23247=CARTESIAN_POINT('Origin',(14.5,-3.5,14.8));
#23248=CARTESIAN_POINT('',(14.335,-3.5,15.));
#23249=CARTESIAN_POINT('Origin',(14.5,-3.5,15.));
#23250=CARTESIAN_POINT('',(14.335,-3.5,16.));
#23251=CARTESIAN_POINT('',(14.335,-3.5,14.8));
#23252=CARTESIAN_POINT('Origin',(14.5,-3.5,16.));
#23253=CARTESIAN_POINT('Origin',(1.5,3.5,14.8));
#23254=CARTESIAN_POINT('',(1.335,3.5,15.));
#23255=CARTESIAN_POINT('Origin',(1.5,3.5,15.));
#23256=CARTESIAN_POINT('',(1.335,3.5,16.));
#23257=CARTESIAN_POINT('',(1.335,3.5,14.8));
#23258=CARTESIAN_POINT('Origin',(1.5,3.5,16.));
#23259=CARTESIAN_POINT('Origin',(1.5,-3.5,14.8));
#23260=CARTESIAN_POINT('',(1.335,-3.5,15.));
#23261=CARTESIAN_POINT('Origin',(1.5,-3.5,15.));
#23262=CARTESIAN_POINT('',(1.335,-3.5,16.));
#23263=CARTESIAN_POINT('',(1.335,-3.5,14.8));
#23264=CARTESIAN_POINT('Origin',(1.5,-3.5,16.));
#23265=CARTESIAN_POINT('Origin',(14.5,3.5,14.8));
#23266=CARTESIAN_POINT('',(14.335,3.5,15.));
#23267=CARTESIAN_POINT('Origin',(14.5,3.5,15.));
#23268=CARTESIAN_POINT('',(14.335,3.5,16.));
#23269=CARTESIAN_POINT('',(14.335,3.5,14.8));
#23270=CARTESIAN_POINT('Origin',(14.5,3.5,16.));
#23271=CARTESIAN_POINT('Origin',(2.,-3.,14.9));
#23272=CARTESIAN_POINT('',(2.,-3.,15.));
#23273=CARTESIAN_POINT('',(14.,-3.,15.));
#23274=CARTESIAN_POINT('',(4.3,-3.,15.));
#23275=CARTESIAN_POINT('',(2.,-3.,16.));
#23276=CARTESIAN_POINT('',(2.,-3.,14.9));
#23277=CARTESIAN_POINT('',(14.,-3.,16.));
#23278=CARTESIAN_POINT('',(4.25,-3.,16.));
#23279=CARTESIAN_POINT('',(14.,-3.,14.9));
#23280=CARTESIAN_POINT('Origin',(14.,-3.,14.9));
#23281=CARTESIAN_POINT('',(14.,3.,15.));
#23282=CARTESIAN_POINT('',(14.,-1.5,15.));
#23283=CARTESIAN_POINT('',(14.,3.,16.));
#23284=CARTESIAN_POINT('',(14.,-1.5,16.));
#23285=CARTESIAN_POINT('',(14.,3.,14.9));
#23286=CARTESIAN_POINT('Origin',(14.,3.,14.9));
#23287=CARTESIAN_POINT('',(2.,3.,15.));
#23288=CARTESIAN_POINT('',(10.3,3.,15.));
#23289=CARTESIAN_POINT('',(2.,3.,16.));
#23290=CARTESIAN_POINT('',(10.25,3.,16.));
#23291=CARTESIAN_POINT('',(2.,3.,14.9));
#23292=CARTESIAN_POINT('Origin',(2.,3.,14.9));
#23293=CARTESIAN_POINT('',(2.,1.5,15.));
#23294=CARTESIAN_POINT('',(2.,1.5,16.));
#23295=CARTESIAN_POINT('Origin',(10.161522368915,6.1,11.838477631085));
#23296=CARTESIAN_POINT('',(9.99652236891498,6.1,11.838477631085));
#23297=CARTESIAN_POINT('Origin',(10.161522368915,6.1,11.838477631085));
#23298=CARTESIAN_POINT('',(9.99652236891498,7.5,11.838477631085));
#23299=CARTESIAN_POINT('',(9.99652236891498,6.1,11.838477631085));
#23300=CARTESIAN_POINT('Origin',(10.161522368915,7.5,11.838477631085));
#23301=CARTESIAN_POINT('Origin',(10.161522368915,6.1,11.838477631085));
#23302=CARTESIAN_POINT('Origin',(13.838477631085,6.1,11.838477631085));
#23303=CARTESIAN_POINT('',(13.673477631085,6.1,11.838477631085));
#23304=CARTESIAN_POINT('Origin',(13.838477631085,6.1,11.838477631085));
#23305=CARTESIAN_POINT('',(13.673477631085,7.5,11.838477631085));
#23306=CARTESIAN_POINT('',(13.673477631085,6.1,11.838477631085));
#23307=CARTESIAN_POINT('Origin',(13.838477631085,7.5,11.838477631085));
#23308=CARTESIAN_POINT('Origin',(13.838477631085,6.1,11.838477631085));
#23309=CARTESIAN_POINT('Origin',(10.161522368915,-7.6,11.838477631085));
#23310=CARTESIAN_POINT('',(9.99652236891498,-7.5,11.838477631085));
#23311=CARTESIAN_POINT('Origin',(10.161522368915,-7.5,11.838477631085));
#23312=CARTESIAN_POINT('',(9.99652236891498,-6.1,11.838477631085));
#23313=CARTESIAN_POINT('',(9.99652236891498,-7.6,11.838477631085));
#23314=CARTESIAN_POINT('Origin',(10.161522368915,-6.1,11.838477631085));
#23315=CARTESIAN_POINT('Origin',(10.161522368915,-6.1,11.838477631085));
#23316=CARTESIAN_POINT('Origin',(13.838477631085,-7.6,11.838477631085));
#23317=CARTESIAN_POINT('',(13.673477631085,-7.5,11.838477631085));
#23318=CARTESIAN_POINT('Origin',(13.838477631085,-7.5,11.838477631085));
#23319=CARTESIAN_POINT('',(13.673477631085,-6.1,11.838477631085));
#23320=CARTESIAN_POINT('',(13.673477631085,-7.6,11.838477631085));
#23321=CARTESIAN_POINT('Origin',(13.838477631085,-6.1,11.838477631085));
#23322=CARTESIAN_POINT('Origin',(13.838477631085,-6.1,11.838477631085));
#23323=CARTESIAN_POINT('Origin',(12.,5.3,10.));
#23324=CARTESIAN_POINT('',(9.65,5.3,10.));
#23325=CARTESIAN_POINT('',(10.1,5.3,10.));
#23326=CARTESIAN_POINT('',(9.25,5.3,10.));
#23327=CARTESIAN_POINT('',(14.35,5.3,10.));
#23328=CARTESIAN_POINT('Origin',(12.,5.3,10.));
#23329=CARTESIAN_POINT('',(13.9,5.3,10.));
#23330=CARTESIAN_POINT('',(9.25,5.3,10.));
#23331=CARTESIAN_POINT('Origin',(12.,5.3,10.));
#23332=CARTESIAN_POINT('Origin',(12.,5.3,10.));
#23333=CARTESIAN_POINT('',(9.65,7.5,10.));
#23334=CARTESIAN_POINT('',(9.65,5.3,10.));
#23335=CARTESIAN_POINT('',(14.35,7.5,10.));
#23336=CARTESIAN_POINT('Origin',(12.,7.5,10.));
#23337=CARTESIAN_POINT('',(14.35,5.3,10.));
#23338=CARTESIAN_POINT('Origin',(12.,-7.6,10.));
#23339=CARTESIAN_POINT('',(13.9,5.,10.));
#23340=CARTESIAN_POINT('',(13.9,-7.6,10.));
#23341=CARTESIAN_POINT('',(10.1,5.,10.));
#23342=CARTESIAN_POINT('Origin',(12.,5.,10.));
#23343=CARTESIAN_POINT('',(10.1,-7.6,10.));
#23344=CARTESIAN_POINT('Origin',(6.5,0.,10.));
#23345=CARTESIAN_POINT('',(18.5,7.5,10.));
#23346=CARTESIAN_POINT('',(18.5,7.5,10.));
#23347=CARTESIAN_POINT('',(18.5,-7.5,10.));
#23348=CARTESIAN_POINT('',(18.5,-7.5,10.));
#23349=CARTESIAN_POINT('',(14.35,-7.5,10.));
#23350=CARTESIAN_POINT('',(-5.5,-7.5,10.));
#23351=CARTESIAN_POINT('',(14.35,-5.3,10.));
#23352=CARTESIAN_POINT('',(14.35,-7.6,10.));
#23353=CARTESIAN_POINT('',(13.9,-5.3,10.));
#23354=CARTESIAN_POINT('',(9.25,-5.3,10.));
#23355=CARTESIAN_POINT('',(13.9,-5.,10.));
#23356=CARTESIAN_POINT('',(13.9,-7.6,10.));
#23357=CARTESIAN_POINT('',(16.4,-5.,10.));
#23358=CARTESIAN_POINT('',(1.65,-5.,10.));
#23359=CARTESIAN_POINT('',(16.4,5.,10.));
#23360=CARTESIAN_POINT('',(16.4,-2.5,10.));
#23361=CARTESIAN_POINT('',(11.45,5.,10.));
#23362=CARTESIAN_POINT('',(17.6,3.,10.));
#23363=CARTESIAN_POINT('Origin',(17.75,3.,10.));
#23364=CARTESIAN_POINT('',(17.42,-4.04133443718624E-17,10.));
#23365=CARTESIAN_POINT('Origin',(17.75,0.,10.));
#23366=CARTESIAN_POINT('',(17.42,-6.,10.));
#23367=CARTESIAN_POINT('Origin',(17.75,-6.,10.));
#23368=CARTESIAN_POINT('',(17.42,6.,10.));
#23369=CARTESIAN_POINT('Origin',(17.75,6.,10.));
#23370=CARTESIAN_POINT('',(17.6,-3.,10.));
#23371=CARTESIAN_POINT('Origin',(17.75,-3.,10.));
#23372=CARTESIAN_POINT('Origin',(12.,-7.6,10.));
#23373=CARTESIAN_POINT('',(9.65,-5.3,10.));
#23374=CARTESIAN_POINT('',(9.65,-7.5,10.));
#23375=CARTESIAN_POINT('',(9.65,-7.6,10.));
#23376=CARTESIAN_POINT('Origin',(12.,-5.3,10.));
#23377=CARTESIAN_POINT('Origin',(12.,-7.5,10.));
#23378=CARTESIAN_POINT('Origin',(12.,-5.3,10.));
#23379=CARTESIAN_POINT('',(10.1,-5.3,10.));
#23380=CARTESIAN_POINT('',(9.25,-5.3,10.));
#23381=CARTESIAN_POINT('Origin',(12.,-5.3,10.));
#23382=CARTESIAN_POINT('Origin',(-4.,-7.5,10.));
#23383=CARTESIAN_POINT('',(18.5,-7.5,10.8));
#23384=CARTESIAN_POINT('',(18.5,-7.5,10.));
#23385=CARTESIAN_POINT('',(17.,-7.5,10.8));
#23386=CARTESIAN_POINT('',(17.,-7.5,10.8));
#23387=CARTESIAN_POINT('',(17.,-7.5,16.));
#23388=CARTESIAN_POINT('',(17.,-7.5,10.));
#23389=CARTESIAN_POINT('',(-4.,-7.5,16.));
#23390=CARTESIAN_POINT('',(-4.,-7.5,16.));
#23391=CARTESIAN_POINT('',(-4.,-7.5,10.8));
#23392=CARTESIAN_POINT('',(-4.,-7.5,10.));
#23393=CARTESIAN_POINT('',(-5.5,-7.5,10.8));
#23394=CARTESIAN_POINT('',(-5.5,-7.5,10.8));
#23395=CARTESIAN_POINT('',(-5.5,-7.5,10.));
#23396=CARTESIAN_POINT('',(-5.5,-7.5,10.));
#23397=CARTESIAN_POINT('',(-1.6,-7.5,10.));
#23398=CARTESIAN_POINT('',(-5.5,-7.5,10.));
#23399=CARTESIAN_POINT('',(1.6,-7.5,10.));
#23400=CARTESIAN_POINT('Origin',(0.,-7.5,10.));
#23401=CARTESIAN_POINT('',(3.65,-7.5,10.));
#23402=CARTESIAN_POINT('',(-5.5,-7.5,10.));
#23403=CARTESIAN_POINT('',(8.35,-7.5,10.));
#23404=CARTESIAN_POINT('Origin',(6.,-7.5,10.));
#23405=CARTESIAN_POINT('',(-5.5,-7.5,10.));
#23406=CARTESIAN_POINT('',(-1.57921356237309,-7.5,11.4142135623731));
#23407=CARTESIAN_POINT('Origin',(-1.41421356237309,-7.5,11.4142135623731));
#23408=CARTESIAN_POINT('',(1.2492135623731,-7.5,11.4142135623731));
#23409=CARTESIAN_POINT('Origin',(1.4142135623731,-7.5,11.4142135623731));
#23410=CARTESIAN_POINT('',(7.67347763108502,-7.5,11.838477631085));
#23411=CARTESIAN_POINT('Origin',(7.83847763108502,-7.5,11.838477631085));
#23412=CARTESIAN_POINT('',(3.99652236891498,-7.5,11.838477631085));
#23413=CARTESIAN_POINT('Origin',(4.16152236891498,-7.5,11.838477631085));
#23414=CARTESIAN_POINT('Origin',(12.,-7.6,10.));
#23415=CARTESIAN_POINT('',(10.1,-5.,10.));
#23416=CARTESIAN_POINT('',(10.1,-7.6,10.));
#23417=CARTESIAN_POINT('Origin',(12.,-5.,10.));
#23418=CARTESIAN_POINT('Origin',(17.,7.5,10.));
#23419=CARTESIAN_POINT('',(8.35,7.5,10.));
#23420=CARTESIAN_POINT('',(18.5,7.5,10.));
#23421=CARTESIAN_POINT('',(3.65,7.5,10.));
#23422=CARTESIAN_POINT('Origin',(6.,7.5,10.));
#23423=CARTESIAN_POINT('',(1.6,7.5,10.));
#23424=CARTESIAN_POINT('',(18.5,7.5,10.));
#23425=CARTESIAN_POINT('',(-1.6,7.5,10.));
#23426=CARTESIAN_POINT('Origin',(0.,7.5,10.));
#23427=CARTESIAN_POINT('',(-5.5,7.5,10.));
#23428=CARTESIAN_POINT('',(18.5,7.5,10.));
#23429=CARTESIAN_POINT('',(-5.5,7.5,10.8));
#23430=CARTESIAN_POINT('',(-5.5,7.5,10.));
#23431=CARTESIAN_POINT('',(-4.,7.5,10.8));
#23432=CARTESIAN_POINT('',(-4.,7.5,10.8));
#23433=CARTESIAN_POINT('',(-4.,7.5,16.));
#23434=CARTESIAN_POINT('',(-4.,7.5,10.));
#23435=CARTESIAN_POINT('',(17.,7.5,16.));
#23436=CARTESIAN_POINT('',(17.,7.5,16.));
#23437=CARTESIAN_POINT('',(17.,7.5,10.8));
#23438=CARTESIAN_POINT('',(17.,7.5,10.));
#23439=CARTESIAN_POINT('',(18.5,7.5,10.8));
#23440=CARTESIAN_POINT('',(18.5,7.5,10.8));
#23441=CARTESIAN_POINT('',(18.5,7.5,10.));
#23442=CARTESIAN_POINT('',(-1.57921356237309,7.5,11.4142135623731));
#23443=CARTESIAN_POINT('Origin',(-1.41421356237309,7.5,11.4142135623731));
#23444=CARTESIAN_POINT('',(1.2492135623731,7.5,11.4142135623731));
#23445=CARTESIAN_POINT('Origin',(1.4142135623731,7.5,11.4142135623731));
#23446=CARTESIAN_POINT('',(7.67347763108502,7.5,11.838477631085));
#23447=CARTESIAN_POINT('Origin',(7.83847763108502,7.5,11.838477631085));
#23448=CARTESIAN_POINT('',(3.99652236891498,7.5,11.838477631085));
#23449=CARTESIAN_POINT('Origin',(4.16152236891498,7.5,11.838477631085));
#23450=CARTESIAN_POINT('Origin',(-3.2,-5.,9.9));
#23451=CARTESIAN_POINT('',(7.9,-5.,10.));
#23452=CARTESIAN_POINT('',(1.65,-5.,10.));
#23453=CARTESIAN_POINT('',(4.1,-5.,10.));
#23454=CARTESIAN_POINT('Origin',(6.,-5.,10.));
#23455=CARTESIAN_POINT('',(1.2,-5.,10.));
#23456=CARTESIAN_POINT('',(1.65,-5.,10.));
#23457=CARTESIAN_POINT('',(-1.2,-5.,10.));
#23458=CARTESIAN_POINT('Origin',(0.,-5.,10.));
#23459=CARTESIAN_POINT('',(-3.2,-5.,10.));
#23460=CARTESIAN_POINT('',(1.65,-5.,10.));
#23461=CARTESIAN_POINT('',(-3.2,-5.,15.));
#23462=CARTESIAN_POINT('',(-3.2,-5.,9.9));
#23463=CARTESIAN_POINT('',(16.4,-5.,15.));
#23464=CARTESIAN_POINT('',(-3.2,-5.,15.));
#23465=CARTESIAN_POINT('',(16.4,-5.,9.9));
#23466=CARTESIAN_POINT('Origin',(6.5,0.,10.));
#23467=CARTESIAN_POINT('',(8.35,-5.3,10.));
#23468=CARTESIAN_POINT('',(8.35,-7.6,10.));
#23469=CARTESIAN_POINT('',(7.9,-5.3,10.));
#23470=CARTESIAN_POINT('',(6.25,-5.3,10.));
#23471=CARTESIAN_POINT('',(7.9,-7.6,10.));
#23472=CARTESIAN_POINT('Origin',(6.5,0.,10.));
#23473=CARTESIAN_POINT('',(7.9,5.,10.));
#23474=CARTESIAN_POINT('',(11.45,5.,10.));
#23475=CARTESIAN_POINT('',(7.9,5.3,10.));
#23476=CARTESIAN_POINT('',(7.9,-7.6,10.));
#23477=CARTESIAN_POINT('',(8.35,5.3,10.));
#23478=CARTESIAN_POINT('',(6.25,5.3,10.));
#23479=CARTESIAN_POINT('',(8.35,5.3,10.));
#23480=CARTESIAN_POINT('Origin',(4.16152236891498,6.1,11.838477631085));
#23481=CARTESIAN_POINT('',(3.99652236891498,6.1,11.838477631085));
#23482=CARTESIAN_POINT('Origin',(4.16152236891498,6.1,11.838477631085));
#23483=CARTESIAN_POINT('',(3.99652236891498,6.1,11.838477631085));
#23484=CARTESIAN_POINT('Origin',(4.16152236891498,6.1,11.838477631085));
#23485=CARTESIAN_POINT('Origin',(7.83847763108502,6.1,11.838477631085));
#23486=CARTESIAN_POINT('',(7.67347763108502,6.1,11.838477631085));
#23487=CARTESIAN_POINT('Origin',(7.83847763108502,6.1,11.838477631085));
#23488=CARTESIAN_POINT('',(7.67347763108502,6.1,11.838477631085));
#23489=CARTESIAN_POINT('Origin',(7.83847763108502,6.1,11.838477631085));
#23490=CARTESIAN_POINT('Origin',(4.16152236891498,-7.6,11.838477631085));
#23491=CARTESIAN_POINT('',(3.99652236891498,-6.1,11.838477631085));
#23492=CARTESIAN_POINT('',(3.99652236891498,-7.6,11.838477631085));
#23493=CARTESIAN_POINT('Origin',(4.16152236891498,-6.1,11.838477631085));
#23494=CARTESIAN_POINT('Origin',(4.16152236891498,-6.1,11.838477631085));
#23495=CARTESIAN_POINT('Origin',(7.83847763108502,-7.6,11.838477631085));
#23496=CARTESIAN_POINT('',(7.67347763108502,-6.1,11.838477631085));
#23497=CARTESIAN_POINT('',(7.67347763108502,-7.6,11.838477631085));
#23498=CARTESIAN_POINT('Origin',(7.83847763108502,-6.1,11.838477631085));
#23499=CARTESIAN_POINT('Origin',(7.83847763108502,-6.1,11.838477631085));
#23500=CARTESIAN_POINT('Origin',(6.,5.3,10.));
#23501=CARTESIAN_POINT('',(3.65,5.3,10.));
#23502=CARTESIAN_POINT('',(4.1,5.3,10.));
#23503=CARTESIAN_POINT('',(6.25,5.3,10.));
#23504=CARTESIAN_POINT('Origin',(6.,5.3,10.));
#23505=CARTESIAN_POINT('Origin',(6.,5.3,10.));
#23506=CARTESIAN_POINT('Origin',(6.,5.3,10.));
#23507=CARTESIAN_POINT('',(3.65,5.3,10.));
#23508=CARTESIAN_POINT('Origin',(6.,-7.6,10.));
#23509=CARTESIAN_POINT('',(4.1,5.,10.));
#23510=CARTESIAN_POINT('Origin',(6.,5.,10.));
#23511=CARTESIAN_POINT('',(4.1,-7.6,10.));
#23512=CARTESIAN_POINT('Origin',(6.,-7.6,10.));
#23513=CARTESIAN_POINT('',(3.65,-5.3,10.));
#23514=CARTESIAN_POINT('',(3.65,-7.6,10.));
#23515=CARTESIAN_POINT('Origin',(6.,-5.3,10.));
#23516=CARTESIAN_POINT('Origin',(6.,-5.3,10.));
#23517=CARTESIAN_POINT('',(4.1,-5.3,10.));
#23518=CARTESIAN_POINT('',(6.25,-5.3,10.));
#23519=CARTESIAN_POINT('Origin',(6.,-5.3,10.));
#23520=CARTESIAN_POINT('Origin',(6.,-7.6,10.));
#23521=CARTESIAN_POINT('',(4.1,-7.6,10.));
#23522=CARTESIAN_POINT('Origin',(6.5,0.,10.));
#23523=CARTESIAN_POINT('',(1.6,-5.5,10.));
#23524=CARTESIAN_POINT('',(1.6,-7.6,10.));
#23525=CARTESIAN_POINT('',(1.2,-5.5,10.));
#23526=CARTESIAN_POINT('',(3.25,-5.5,10.));
#23527=CARTESIAN_POINT('',(1.2,-7.6,10.));
#23528=CARTESIAN_POINT('Origin',(6.5,0.,10.));
#23529=CARTESIAN_POINT('',(1.2,5.,10.));
#23530=CARTESIAN_POINT('',(11.45,5.,10.));
#23531=CARTESIAN_POINT('',(1.2,5.5,10.));
#23532=CARTESIAN_POINT('',(1.2,-7.6,10.));
#23533=CARTESIAN_POINT('',(1.6,5.5,10.));
#23534=CARTESIAN_POINT('',(3.25,5.5,10.));
#23535=CARTESIAN_POINT('',(1.6,5.5,10.));
#23536=CARTESIAN_POINT('Origin',(-1.41421356237309,6.1,11.4142135623731));
#23537=CARTESIAN_POINT('',(-1.57921356237309,6.1,11.4142135623731));
#23538=CARTESIAN_POINT('Origin',(-1.41421356237309,6.1,11.4142135623731));
#23539=CARTESIAN_POINT('',(-1.57921356237309,6.1,11.4142135623731));
#23540=CARTESIAN_POINT('Origin',(-1.41421356237309,6.1,11.4142135623731));
#23541=CARTESIAN_POINT('Origin',(1.4142135623731,6.1,11.4142135623731));
#23542=CARTESIAN_POINT('',(1.2492135623731,6.1,11.4142135623731));
#23543=CARTESIAN_POINT('Origin',(1.4142135623731,6.1,11.4142135623731));
#23544=CARTESIAN_POINT('',(1.2492135623731,6.1,11.4142135623731));
#23545=CARTESIAN_POINT('Origin',(1.4142135623731,6.1,11.4142135623731));
#23546=CARTESIAN_POINT('Origin',(-1.41421356237309,-7.6,11.4142135623731));
#23547=CARTESIAN_POINT('',(-1.57921356237309,-6.1,11.4142135623731));
#23548=CARTESIAN_POINT('',(-1.57921356237309,-7.6,11.4142135623731));
#23549=CARTESIAN_POINT('Origin',(-1.41421356237309,-6.1,11.4142135623731));
#23550=CARTESIAN_POINT('Origin',(-1.41421356237309,-6.1,11.4142135623731));
#23551=CARTESIAN_POINT('Origin',(1.4142135623731,-7.6,11.4142135623731));
#23552=CARTESIAN_POINT('',(1.2492135623731,-6.1,11.4142135623731));
#23553=CARTESIAN_POINT('',(1.2492135623731,-7.6,11.4142135623731));
#23554=CARTESIAN_POINT('Origin',(1.4142135623731,-6.1,11.4142135623731));
#23555=CARTESIAN_POINT('Origin',(1.4142135623731,-6.1,11.4142135623731));
#23556=CARTESIAN_POINT('Origin',(0.,5.5,10.));
#23557=CARTESIAN_POINT('',(-1.6,5.5,10.));
#23558=CARTESIAN_POINT('Origin',(0.,5.5,10.));
#23559=CARTESIAN_POINT('',(-1.6,5.5,10.));
#23560=CARTESIAN_POINT('Origin',(0.,5.5,10.));
#23561=CARTESIAN_POINT('',(-1.2,5.5,10.));
#23562=CARTESIAN_POINT('Origin',(0.,5.5,10.));
#23563=CARTESIAN_POINT('',(3.25,5.5,10.));
#23564=CARTESIAN_POINT('Origin',(0.,-7.6,10.));
#23565=CARTESIAN_POINT('',(-1.6,-5.5,10.));
#23566=CARTESIAN_POINT('',(-1.6,-7.6,10.));
#23567=CARTESIAN_POINT('Origin',(0.,-5.5,10.));
#23568=CARTESIAN_POINT('Origin',(0.,-5.5,10.));
#23569=CARTESIAN_POINT('',(-1.2,-5.5,10.));
#23570=CARTESIAN_POINT('',(3.25,-5.5,10.));
#23571=CARTESIAN_POINT('Origin',(0.,-5.5,10.));
#23572=CARTESIAN_POINT('Origin',(0.,-7.6,10.));
#23573=CARTESIAN_POINT('',(-1.2,-7.6,10.));
#23574=CARTESIAN_POINT('Origin',(0.,-7.6,10.));
#23575=CARTESIAN_POINT('',(-1.2,5.,10.));
#23576=CARTESIAN_POINT('Origin',(0.,5.,10.));
#23577=CARTESIAN_POINT('',(-1.2,-7.6,10.));
#23578=CARTESIAN_POINT('Origin',(16.4,5.,9.9));
#23579=CARTESIAN_POINT('',(16.4,5.,15.));
#23580=CARTESIAN_POINT('',(16.4,5.,9.9));
#23581=CARTESIAN_POINT('',(-3.2,5.,15.));
#23582=CARTESIAN_POINT('',(16.4,5.,15.));
#23583=CARTESIAN_POINT('',(-3.2,5.,10.));
#23584=CARTESIAN_POINT('',(-3.2,5.,9.9));
#23585=CARTESIAN_POINT('',(11.45,5.,10.));
#23586=CARTESIAN_POINT('Origin',(6.5,0.,10.));
#23587=CARTESIAN_POINT('',(-3.2,2.5,10.));
#23588=CARTESIAN_POINT('',(-5.5,7.5,10.));
#23589=CARTESIAN_POINT('',(-4.9,3.,10.));
#23590=CARTESIAN_POINT('Origin',(-4.75,3.,10.));
#23591=CARTESIAN_POINT('',(-5.08,-6.,10.));
#23592=CARTESIAN_POINT('Origin',(-4.75,-6.,10.));
#23593=CARTESIAN_POINT('',(-5.08,-4.04133443718627E-17,10.));
#23594=CARTESIAN_POINT('Origin',(-4.75,0.,10.));
#23595=CARTESIAN_POINT('',(-5.08,6.,10.));
#23596=CARTESIAN_POINT('Origin',(-4.75,6.,10.));
#23597=CARTESIAN_POINT('',(-4.9,-3.,10.));
#23598=CARTESIAN_POINT('Origin',(-4.75,-3.,10.));
#23599=CARTESIAN_POINT('Origin',(17.75,3.,9.5));
#23600=CARTESIAN_POINT('',(17.6,3.,10.5));
#23601=CARTESIAN_POINT('',(17.6,3.,9.5));
#23602=CARTESIAN_POINT('Origin',(17.75,3.,10.5));
#23603=CARTESIAN_POINT('Origin',(17.75,3.,10.5));
#23604=CARTESIAN_POINT('Origin',(17.75,-3.,9.5));
#23605=CARTESIAN_POINT('',(17.6,-3.,10.5));
#23606=CARTESIAN_POINT('',(17.6,-3.,9.5));
#23607=CARTESIAN_POINT('Origin',(17.75,-3.,10.5));
#23608=CARTESIAN_POINT('Origin',(17.75,-3.,10.5));
#23609=CARTESIAN_POINT('Origin',(-4.75,3.,9.5));
#23610=CARTESIAN_POINT('',(-4.9,3.,10.5));
#23611=CARTESIAN_POINT('',(-4.9,3.,9.5));
#23612=CARTESIAN_POINT('Origin',(-4.75,3.,10.5));
#23613=CARTESIAN_POINT('Origin',(-4.75,3.,10.5));
#23614=CARTESIAN_POINT('Origin',(-4.75,-3.,9.5));
#23615=CARTESIAN_POINT('',(-4.9,-3.,10.5));
#23616=CARTESIAN_POINT('',(-4.9,-3.,9.5));
#23617=CARTESIAN_POINT('Origin',(-4.75,-3.,10.5));
#23618=CARTESIAN_POINT('Origin',(-4.75,-3.,10.5));
#23619=CARTESIAN_POINT('Origin',(17.75,0.,9.9));
#23620=CARTESIAN_POINT('',(17.42,4.04133443718624E-17,10.8));
#23621=CARTESIAN_POINT('',(17.42,-4.04133443718624E-17,9.9));
#23622=CARTESIAN_POINT('Origin',(17.75,0.,10.8));
#23623=CARTESIAN_POINT('Origin',(-4.75,-6.,9.9));
#23624=CARTESIAN_POINT('',(-5.08,-6.,10.8));
#23625=CARTESIAN_POINT('',(-5.08,-6.,9.9));
#23626=CARTESIAN_POINT('Origin',(-4.75,-6.,10.8));
#23627=CARTESIAN_POINT('Origin',(-4.75,0.,9.9));
#23628=CARTESIAN_POINT('',(-5.08,4.04133443718627E-17,10.8));
#23629=CARTESIAN_POINT('',(-5.08,-4.04133443718627E-17,9.9));
#23630=CARTESIAN_POINT('Origin',(-4.75,0.,10.8));
#23631=CARTESIAN_POINT('Origin',(-4.75,6.,9.9));
#23632=CARTESIAN_POINT('',(-5.08,6.,10.8));
#23633=CARTESIAN_POINT('',(-5.08,6.,9.9));
#23634=CARTESIAN_POINT('Origin',(-4.75,6.,10.8));
#23635=CARTESIAN_POINT('Origin',(17.75,-6.,9.9));
#23636=CARTESIAN_POINT('',(17.42,-6.,10.8));
#23637=CARTESIAN_POINT('',(17.42,-6.,9.9));
#23638=CARTESIAN_POINT('Origin',(17.75,-6.,10.8));
#23639=CARTESIAN_POINT('Origin',(17.75,6.,9.9));
#23640=CARTESIAN_POINT('',(17.42,6.,10.8));
#23641=CARTESIAN_POINT('',(17.42,6.,9.9));
#23642=CARTESIAN_POINT('Origin',(17.75,6.,10.8));
#23643=CARTESIAN_POINT('Origin',(18.5,-7.5,10.));
#23644=CARTESIAN_POINT('',(18.5,-7.5,10.8));
#23645=CARTESIAN_POINT('Origin',(17.75,0.,10.8));
#23646=CARTESIAN_POINT('',(17.,-3.75,10.8));
#23647=CARTESIAN_POINT('Origin',(-5.5,7.5,10.));
#23648=CARTESIAN_POINT('',(-5.5,7.5,10.8));
#23649=CARTESIAN_POINT('Origin',(-4.75,0.,10.8));
#23650=CARTESIAN_POINT('',(-4.,3.75,10.8));
#23651=CARTESIAN_POINT('Origin',(-4.,7.5,10.));
#23652=CARTESIAN_POINT('',(-4.,7.5,16.));
#23653=CARTESIAN_POINT('Origin',(16.4,-5.,9.9));
#23654=CARTESIAN_POINT('',(16.4,-5.,15.));
#23655=CARTESIAN_POINT('Origin',(-3.2,5.,9.9));
#23656=CARTESIAN_POINT('',(-3.2,5.,15.));
#23657=CARTESIAN_POINT('Origin',(6.6,0.,15.));
#23658=CARTESIAN_POINT('Origin',(17.,-7.5,10.));
#23659=CARTESIAN_POINT('',(17.,-7.5,16.));
#23660=CARTESIAN_POINT('Origin',(6.5,0.,16.));
#23661=CARTESIAN_POINT('',(0.,0.,0.));
#23662=CARTESIAN_POINT('Origin',(-4.75,-3.,9.6));
#23663=CARTESIAN_POINT('',(-4.9,-3.,10.4));
#23664=CARTESIAN_POINT('Origin',(-4.75,-3.,10.4));
#23665=CARTESIAN_POINT('',(-4.9,-3.,9.6));
#23666=CARTESIAN_POINT('',(-4.9,-3.,9.6));
#23667=CARTESIAN_POINT('Origin',(-4.75,-3.,9.6));
#23668=CARTESIAN_POINT('Origin',(-4.75,-3.,10.4));
#23669=CARTESIAN_POINT('Origin',(-4.75,-3.,9.6));
#23670=CARTESIAN_POINT('',(0.,0.,0.));
#23671=CARTESIAN_POINT('Origin',(-4.75,3.,9.6));
#23672=CARTESIAN_POINT('',(-4.9,3.,10.4));
#23673=CARTESIAN_POINT('Origin',(-4.75,3.,10.4));
#23674=CARTESIAN_POINT('',(-4.9,3.,9.6));
#23675=CARTESIAN_POINT('',(-4.9,3.,9.6));
#23676=CARTESIAN_POINT('Origin',(-4.75,3.,9.6));
#23677=CARTESIAN_POINT('Origin',(-4.75,3.,10.4));
#23678=CARTESIAN_POINT('Origin',(-4.75,3.,9.6));
#23679=CARTESIAN_POINT('',(0.,0.,0.));
#23680=CARTESIAN_POINT('Origin',(17.75,-3.,9.6));
#23681=CARTESIAN_POINT('',(17.6,-3.,10.4));
#23682=CARTESIAN_POINT('Origin',(17.75,-3.,10.4));
#23683=CARTESIAN_POINT('',(17.6,-3.,9.6));
#23684=CARTESIAN_POINT('',(17.6,-3.,9.6));
#23685=CARTESIAN_POINT('Origin',(17.75,-3.,9.6));
#23686=CARTESIAN_POINT('Origin',(17.75,-3.,10.4));
#23687=CARTESIAN_POINT('Origin',(17.75,-3.,9.6));
#23688=CARTESIAN_POINT('',(0.,0.,0.));
#23689=CARTESIAN_POINT('Origin',(17.75,3.,9.6));
#23690=CARTESIAN_POINT('',(17.6,3.,10.4));
#23691=CARTESIAN_POINT('Origin',(17.75,3.,10.4));
#23692=CARTESIAN_POINT('',(17.6,3.,9.6));
#23693=CARTESIAN_POINT('',(17.6,3.,9.6));
#23694=CARTESIAN_POINT('Origin',(17.75,3.,9.6));
#23695=CARTESIAN_POINT('Origin',(17.75,3.,10.4));
#23696=CARTESIAN_POINT('Origin',(17.75,3.,9.6));
#23697=CARTESIAN_POINT('',(0.,0.,0.));
#23698=CARTESIAN_POINT('Origin',(-1.4142135623731,-7.9,8.5857864376269));
#23699=CARTESIAN_POINT('',(-1.47733531993816,-7.8,8.3698219874924));
#23700=CARTESIAN_POINT('',(-1.47733531993816,-7.5,8.3698219874924));
#23701=CARTESIAN_POINT('',(-1.47733531993816,-7.9,8.3698219874924));
#23702=CARTESIAN_POINT('',(-1.6301780125076,-7.8,8.52266468006184));
#23703=CARTESIAN_POINT('Origin',(-1.4142135623731,-7.8,8.5857864376269));
#23704=CARTESIAN_POINT('',(-1.6301780125076,-7.5,8.52266468006184));
#23705=CARTESIAN_POINT('',(-1.6301780125076,-7.9,8.52266468006184));
#23706=CARTESIAN_POINT('Origin',(-1.4142135623731,-7.5,8.5857864376269));
#23707=CARTESIAN_POINT('Origin',(-1.41421356237309,-7.9,11.4142135623731));
#23708=CARTESIAN_POINT('',(-1.6301780125076,-7.8,11.4773353199382));
#23709=CARTESIAN_POINT('',(-1.6301780125076,-7.5,11.4773353199382));
#23710=CARTESIAN_POINT('',(-1.6301780125076,-7.9,11.4773353199382));
#23711=CARTESIAN_POINT('',(-1.47733531993816,-7.8,11.6301780125076));
#23712=CARTESIAN_POINT('Origin',(-1.41421356237309,-7.8,11.4142135623731));
#23713=CARTESIAN_POINT('',(-1.47733531993816,-7.5,11.6301780125076));
#23714=CARTESIAN_POINT('',(-1.47733531993816,-7.9,11.6301780125076));
#23715=CARTESIAN_POINT('Origin',(-1.41421356237309,-7.5,11.4142135623731));
#23716=CARTESIAN_POINT('Origin',(1.4142135623731,-7.9,11.4142135623731));
#23717=CARTESIAN_POINT('',(1.47733531993816,-7.8,11.6301780125076));
#23718=CARTESIAN_POINT('',(1.47733531993816,-7.5,11.6301780125076));
#23719=CARTESIAN_POINT('',(1.47733531993816,-7.9,11.6301780125076));
#23720=CARTESIAN_POINT('',(1.6301780125076,-7.8,11.4773353199382));
#23721=CARTESIAN_POINT('Origin',(1.4142135623731,-7.8,11.4142135623731));
#23722=CARTESIAN_POINT('',(1.6301780125076,-7.5,11.4773353199382));
#23723=CARTESIAN_POINT('',(1.6301780125076,-7.9,11.4773353199382));
#23724=CARTESIAN_POINT('Origin',(1.4142135623731,-7.5,11.4142135623731));
#23725=CARTESIAN_POINT('Origin',(1.41421356237309,-7.9,8.5857864376269));
#23726=CARTESIAN_POINT('',(1.6301780125076,-7.8,8.52266468006184));
#23727=CARTESIAN_POINT('',(1.6301780125076,-7.5,8.52266468006184));
#23728=CARTESIAN_POINT('',(1.6301780125076,-7.9,8.52266468006184));
#23729=CARTESIAN_POINT('',(1.47733531993816,-7.8,8.3698219874924));
#23730=CARTESIAN_POINT('Origin',(1.41421356237309,-7.8,8.5857864376269));
#23731=CARTESIAN_POINT('',(1.47733531993816,-7.5,8.3698219874924));
#23732=CARTESIAN_POINT('',(1.47733531993816,-7.9,8.3698219874924));
#23733=CARTESIAN_POINT('Origin',(1.41421356237309,-7.5,8.5857864376269));
#23734=CARTESIAN_POINT('Origin',(0.,-7.8,10.));
#23735=CARTESIAN_POINT('Origin',(0.,-7.8,10.));
#23736=CARTESIAN_POINT('Origin',(0.,-7.8,10.));
#23737=CARTESIAN_POINT('Origin',(0.,-7.8,10.));
#23738=CARTESIAN_POINT('Origin',(0.,-7.8,10.));
#23739=CARTESIAN_POINT('',(-1.2,-7.8,10.));
#23740=CARTESIAN_POINT('Origin',(0.,-7.8,10.));
#23741=CARTESIAN_POINT('Origin',(0.,-7.8,10.));
#23742=CARTESIAN_POINT('Origin',(0.,-7.5,10.));
#23743=CARTESIAN_POINT('Origin',(0.,-7.8,10.));
#23744=CARTESIAN_POINT('Origin',(0.,-7.5,10.));
#23745=CARTESIAN_POINT('Origin',(0.,-7.8,10.));
#23746=CARTESIAN_POINT('Origin',(0.,-7.5,10.));
#23747=CARTESIAN_POINT('Origin',(0.,-7.8,10.));
#23748=CARTESIAN_POINT('Origin',(0.,-7.5,10.));
#23749=CARTESIAN_POINT('Origin',(0.,-7.5,10.));
#23750=CARTESIAN_POINT('',(-1.59,-6.5,10.));
#23751=CARTESIAN_POINT('Origin',(0.,-6.5,10.));
#23752=CARTESIAN_POINT('',(-1.59,-7.5,10.));
#23753=CARTESIAN_POINT('',(-1.59,-7.5,10.));
#23754=CARTESIAN_POINT('Origin',(0.,-7.5,10.));
#23755=CARTESIAN_POINT('Origin',(0.,-6.5,10.));
#23756=CARTESIAN_POINT('',(-1.2,-6.5,10.));
#23757=CARTESIAN_POINT('Origin',(0.,-6.5,10.));
#23758=CARTESIAN_POINT('Origin',(0.,-7.8,10.));
#23759=CARTESIAN_POINT('',(-1.2,-7.8,10.));
#23760=CARTESIAN_POINT('Origin',(0.,-7.5,10.));
#23761=CARTESIAN_POINT('',(0.,0.,0.));
#23762=CARTESIAN_POINT('Origin',(-1.4142135623731,7.4,8.5857864376269));
#23763=CARTESIAN_POINT('',(-1.47733531993816,7.5,8.3698219874924));
#23764=CARTESIAN_POINT('',(-1.47733531993816,7.8,8.3698219874924));
#23765=CARTESIAN_POINT('',(-1.47733531993816,7.4,8.3698219874924));
#23766=CARTESIAN_POINT('',(-1.6301780125076,7.5,8.52266468006184));
#23767=CARTESIAN_POINT('Origin',(-1.4142135623731,7.5,8.5857864376269));
#23768=CARTESIAN_POINT('',(-1.6301780125076,7.8,8.52266468006184));
#23769=CARTESIAN_POINT('',(-1.6301780125076,7.4,8.52266468006184));
#23770=CARTESIAN_POINT('Origin',(-1.4142135623731,7.8,8.5857864376269));
#23771=CARTESIAN_POINT('Origin',(-1.41421356237309,7.4,11.4142135623731));
#23772=CARTESIAN_POINT('',(-1.6301780125076,7.5,11.4773353199382));
#23773=CARTESIAN_POINT('',(-1.6301780125076,7.8,11.4773353199382));
#23774=CARTESIAN_POINT('',(-1.6301780125076,7.4,11.4773353199382));
#23775=CARTESIAN_POINT('',(-1.47733531993816,7.5,11.6301780125076));
#23776=CARTESIAN_POINT('Origin',(-1.41421356237309,7.5,11.4142135623731));
#23777=CARTESIAN_POINT('',(-1.47733531993816,7.8,11.6301780125076));
#23778=CARTESIAN_POINT('',(-1.47733531993816,7.4,11.6301780125076));
#23779=CARTESIAN_POINT('Origin',(-1.41421356237309,7.8,11.4142135623731));
#23780=CARTESIAN_POINT('Origin',(1.4142135623731,7.4,11.4142135623731));
#23781=CARTESIAN_POINT('',(1.47733531993816,7.5,11.6301780125076));
#23782=CARTESIAN_POINT('',(1.47733531993816,7.8,11.6301780125076));
#23783=CARTESIAN_POINT('',(1.47733531993816,7.4,11.6301780125076));
#23784=CARTESIAN_POINT('',(1.6301780125076,7.5,11.4773353199382));
#23785=CARTESIAN_POINT('Origin',(1.4142135623731,7.5,11.4142135623731));
#23786=CARTESIAN_POINT('',(1.6301780125076,7.8,11.4773353199382));
#23787=CARTESIAN_POINT('',(1.6301780125076,7.4,11.4773353199382));
#23788=CARTESIAN_POINT('Origin',(1.4142135623731,7.8,11.4142135623731));
#23789=CARTESIAN_POINT('Origin',(1.41421356237309,7.4,8.5857864376269));
#23790=CARTESIAN_POINT('',(1.6301780125076,7.5,8.52266468006184));
#23791=CARTESIAN_POINT('',(1.6301780125076,7.8,8.52266468006184));
#23792=CARTESIAN_POINT('',(1.6301780125076,7.4,8.52266468006184));
#23793=CARTESIAN_POINT('',(1.47733531993816,7.5,8.3698219874924));
#23794=CARTESIAN_POINT('Origin',(1.41421356237309,7.5,8.5857864376269));
#23795=CARTESIAN_POINT('',(1.47733531993816,7.8,8.3698219874924));
#23796=CARTESIAN_POINT('',(1.47733531993816,7.4,8.3698219874924));
#23797=CARTESIAN_POINT('Origin',(1.41421356237309,7.8,8.5857864376269));
#23798=CARTESIAN_POINT('Origin',(0.,7.5,10.));
#23799=CARTESIAN_POINT('Origin',(0.,7.5,10.));
#23800=CARTESIAN_POINT('Origin',(0.,7.5,10.));
#23801=CARTESIAN_POINT('Origin',(0.,7.5,10.));
#23802=CARTESIAN_POINT('Origin',(0.,7.5,10.));
#23803=CARTESIAN_POINT('',(-1.59,7.5,10.));
#23804=CARTESIAN_POINT('Origin',(0.,7.5,10.));
#23805=CARTESIAN_POINT('Origin',(0.,7.5,10.));
#23806=CARTESIAN_POINT('Origin',(0.,7.8,10.));
#23807=CARTESIAN_POINT('Origin',(0.,7.5,10.));
#23808=CARTESIAN_POINT('Origin',(0.,7.8,10.));
#23809=CARTESIAN_POINT('Origin',(0.,7.5,10.));
#23810=CARTESIAN_POINT('Origin',(0.,7.8,10.));
#23811=CARTESIAN_POINT('Origin',(0.,7.5,10.));
#23812=CARTESIAN_POINT('Origin',(0.,7.8,10.));
#23813=CARTESIAN_POINT('Origin',(0.,6.5,10.));
#23814=CARTESIAN_POINT('',(-1.59,6.5,10.));
#23815=CARTESIAN_POINT('',(-1.59,6.5,10.));
#23816=CARTESIAN_POINT('Origin',(0.,6.5,10.));
#23817=CARTESIAN_POINT('Origin',(0.,6.5,10.));
#23818=CARTESIAN_POINT('',(-1.2,6.5,10.));
#23819=CARTESIAN_POINT('Origin',(0.,6.5,10.));
#23820=CARTESIAN_POINT('Origin',(0.,7.5,10.));
#23821=CARTESIAN_POINT('',(-1.2,7.8,10.));
#23822=CARTESIAN_POINT('Origin',(0.,7.8,10.));
#23823=CARTESIAN_POINT('',(-1.2,7.5,10.));
#23824=CARTESIAN_POINT('Origin',(0.,7.8,10.));
#23825=CARTESIAN_POINT('',(0.,0.,0.));
#23826=CARTESIAN_POINT('Origin',(4.16152236891498,-7.9,8.16152236891498));
#23827=CARTESIAN_POINT('',(3.93652236891498,-7.8,8.16152236891498));
#23828=CARTESIAN_POINT('Origin',(4.16152236891498,-7.8,8.16152236891498));
#23829=CARTESIAN_POINT('',(3.93652236891498,-7.5,8.16152236891498));
#23830=CARTESIAN_POINT('',(3.93652236891498,-7.9,8.16152236891498));
#23831=CARTESIAN_POINT('Origin',(4.16152236891498,-7.5,8.16152236891498));
#23832=CARTESIAN_POINT('Origin',(4.16152236891498,-7.9,11.838477631085));
#23833=CARTESIAN_POINT('',(3.93652236891498,-7.8,11.838477631085));
#23834=CARTESIAN_POINT('Origin',(4.16152236891498,-7.8,11.838477631085));
#23835=CARTESIAN_POINT('',(3.93652236891498,-7.5,11.838477631085));
#23836=CARTESIAN_POINT('',(3.93652236891498,-7.9,11.838477631085));
#23837=CARTESIAN_POINT('Origin',(4.16152236891498,-7.5,11.838477631085));
#23838=CARTESIAN_POINT('Origin',(7.83847763108502,-7.9,11.838477631085));
#23839=CARTESIAN_POINT('',(7.61347763108502,-7.8,11.838477631085));
#23840=CARTESIAN_POINT('Origin',(7.83847763108502,-7.8,11.838477631085));
#23841=CARTESIAN_POINT('',(7.61347763108502,-7.5,11.838477631085));
#23842=CARTESIAN_POINT('',(7.61347763108502,-7.9,11.838477631085));
#23843=CARTESIAN_POINT('Origin',(7.83847763108502,-7.5,11.838477631085));
#23844=CARTESIAN_POINT('Origin',(7.83847763108502,-7.9,8.16152236891498));
#23845=CARTESIAN_POINT('',(7.61347763108502,-7.8,8.16152236891498));
#23846=CARTESIAN_POINT('Origin',(7.83847763108502,-7.8,8.16152236891498));
#23847=CARTESIAN_POINT('',(7.61347763108502,-7.5,8.16152236891498));
#23848=CARTESIAN_POINT('',(7.61347763108502,-7.9,8.16152236891498));
#23849=CARTESIAN_POINT('Origin',(7.83847763108502,-7.5,8.16152236891498));
#23850=CARTESIAN_POINT('Origin',(6.,-7.5,10.));
#23851=CARTESIAN_POINT('',(3.66,-6.7,10.));
#23852=CARTESIAN_POINT('Origin',(6.,-6.7,10.));
#23853=CARTESIAN_POINT('',(3.66,-7.5,10.));
#23854=CARTESIAN_POINT('',(3.66,-7.5,10.));
#23855=CARTESIAN_POINT('Origin',(6.,-7.5,10.));
#23856=CARTESIAN_POINT('Origin',(6.,-6.7,10.));
#23857=CARTESIAN_POINT('',(4.1,-6.7,10.));
#23858=CARTESIAN_POINT('Origin',(6.,-6.7,10.));
#23859=CARTESIAN_POINT('Origin',(6.,-7.8,10.));
#23860=CARTESIAN_POINT('',(4.1,-7.8,10.));
#23861=CARTESIAN_POINT('',(4.1,-7.8,10.));
#23862=CARTESIAN_POINT('Origin',(6.,-7.8,10.));
#23863=CARTESIAN_POINT('Origin',(6.,-7.8,10.));
#23864=CARTESIAN_POINT('',(3.1,-7.5,10.));
#23865=CARTESIAN_POINT('Origin',(6.,-7.5,10.));
#23866=CARTESIAN_POINT('',(3.1,-7.8,10.));
#23867=CARTESIAN_POINT('',(3.1,-7.8,10.));
#23868=CARTESIAN_POINT('Origin',(6.,-7.8,10.));
#23869=CARTESIAN_POINT('Origin',(6.,-7.5,10.));
#23870=CARTESIAN_POINT('Origin',(6.,-7.8,10.));
#23871=CARTESIAN_POINT('',(0.,0.,0.));
#23872=CARTESIAN_POINT('Origin',(4.16152236891498,7.4,8.16152236891498));
#23873=CARTESIAN_POINT('',(3.93652236891498,7.5,8.16152236891498));
#23874=CARTESIAN_POINT('Origin',(4.16152236891498,7.5,8.16152236891498));
#23875=CARTESIAN_POINT('',(3.93652236891498,7.8,8.16152236891498));
#23876=CARTESIAN_POINT('',(3.93652236891498,7.4,8.16152236891498));
#23877=CARTESIAN_POINT('Origin',(4.16152236891498,7.8,8.16152236891498));
#23878=CARTESIAN_POINT('Origin',(4.16152236891498,7.4,11.838477631085));
#23879=CARTESIAN_POINT('',(3.93652236891498,7.5,11.838477631085));
#23880=CARTESIAN_POINT('Origin',(4.16152236891498,7.5,11.838477631085));
#23881=CARTESIAN_POINT('',(3.93652236891498,7.8,11.838477631085));
#23882=CARTESIAN_POINT('',(3.93652236891498,7.4,11.838477631085));
#23883=CARTESIAN_POINT('Origin',(4.16152236891498,7.8,11.838477631085));
#23884=CARTESIAN_POINT('Origin',(7.83847763108502,7.4,11.838477631085));
#23885=CARTESIAN_POINT('',(7.61347763108502,7.5,11.838477631085));
#23886=CARTESIAN_POINT('Origin',(7.83847763108502,7.5,11.838477631085));
#23887=CARTESIAN_POINT('',(7.61347763108502,7.8,11.838477631085));
#23888=CARTESIAN_POINT('',(7.61347763108502,7.4,11.838477631085));
#23889=CARTESIAN_POINT('Origin',(7.83847763108502,7.8,11.838477631085));
#23890=CARTESIAN_POINT('Origin',(7.83847763108502,7.4,8.16152236891498));
#23891=CARTESIAN_POINT('',(7.61347763108502,7.5,8.16152236891498));
#23892=CARTESIAN_POINT('Origin',(7.83847763108502,7.5,8.16152236891498));
#23893=CARTESIAN_POINT('',(7.61347763108502,7.8,8.16152236891498));
#23894=CARTESIAN_POINT('',(7.61347763108502,7.4,8.16152236891498));
#23895=CARTESIAN_POINT('Origin',(7.83847763108502,7.8,8.16152236891498));
#23896=CARTESIAN_POINT('Origin',(6.,6.7,10.));
#23897=CARTESIAN_POINT('',(3.66,7.5,10.));
#23898=CARTESIAN_POINT('Origin',(6.,7.5,10.));
#23899=CARTESIAN_POINT('',(3.66,6.7,10.));
#23900=CARTESIAN_POINT('',(3.66,6.7,10.));
#23901=CARTESIAN_POINT('Origin',(6.,6.7,10.));
#23902=CARTESIAN_POINT('Origin',(6.,6.7,10.));
#23903=CARTESIAN_POINT('',(4.1,6.7,10.));
#23904=CARTESIAN_POINT('Origin',(6.,6.7,10.));
#23905=CARTESIAN_POINT('Origin',(6.,7.5,10.));
#23906=CARTESIAN_POINT('',(4.1,7.8,10.));
#23907=CARTESIAN_POINT('Origin',(6.,7.8,10.));
#23908=CARTESIAN_POINT('',(4.1,7.5,10.));
#23909=CARTESIAN_POINT('Origin',(6.,7.5,10.));
#23910=CARTESIAN_POINT('',(3.1,7.8,10.));
#23911=CARTESIAN_POINT('Origin',(6.,7.8,10.));
#23912=CARTESIAN_POINT('',(3.1,7.5,10.));
#23913=CARTESIAN_POINT('',(3.1,7.5,10.));
#23914=CARTESIAN_POINT('Origin',(6.,7.5,10.));
#23915=CARTESIAN_POINT('Origin',(6.,7.8,10.));
#23916=CARTESIAN_POINT('Origin',(6.,7.5,10.));
#23917=CARTESIAN_POINT('',(0.,0.,0.));
#23918=CARTESIAN_POINT('Origin',(10.161522368915,-7.9,8.16152236891498));
#23919=CARTESIAN_POINT('',(9.93652236891498,-7.8,8.16152236891498));
#23920=CARTESIAN_POINT('Origin',(10.161522368915,-7.8,8.16152236891498));
#23921=CARTESIAN_POINT('',(9.93652236891498,-7.5,8.16152236891498));
#23922=CARTESIAN_POINT('',(9.93652236891498,-7.9,8.16152236891498));
#23923=CARTESIAN_POINT('Origin',(10.161522368915,-7.5,8.16152236891498));
#23924=CARTESIAN_POINT('Origin',(10.161522368915,-7.9,11.838477631085));
#23925=CARTESIAN_POINT('',(9.93652236891498,-7.8,11.838477631085));
#23926=CARTESIAN_POINT('Origin',(10.161522368915,-7.8,11.838477631085));
#23927=CARTESIAN_POINT('',(9.93652236891498,-7.5,11.838477631085));
#23928=CARTESIAN_POINT('',(9.93652236891498,-7.9,11.838477631085));
#23929=CARTESIAN_POINT('Origin',(10.161522368915,-7.5,11.838477631085));
#23930=CARTESIAN_POINT('Origin',(13.838477631085,-7.9,11.838477631085));
#23931=CARTESIAN_POINT('',(13.613477631085,-7.8,11.838477631085));
#23932=CARTESIAN_POINT('Origin',(13.838477631085,-7.8,11.838477631085));
#23933=CARTESIAN_POINT('',(13.613477631085,-7.5,11.838477631085));
#23934=CARTESIAN_POINT('',(13.613477631085,-7.9,11.838477631085));
#23935=CARTESIAN_POINT('Origin',(13.838477631085,-7.5,11.838477631085));
#23936=CARTESIAN_POINT('Origin',(13.838477631085,-7.9,8.16152236891498));
#23937=CARTESIAN_POINT('',(13.613477631085,-7.8,8.16152236891498));
#23938=CARTESIAN_POINT('Origin',(13.838477631085,-7.8,8.16152236891498));
#23939=CARTESIAN_POINT('',(13.613477631085,-7.5,8.16152236891498));
#23940=CARTESIAN_POINT('',(13.613477631085,-7.9,8.16152236891498));
#23941=CARTESIAN_POINT('Origin',(13.838477631085,-7.5,8.16152236891498));
#23942=CARTESIAN_POINT('Origin',(12.,-7.5,10.));
#23943=CARTESIAN_POINT('',(9.66,-6.7,10.));
#23944=CARTESIAN_POINT('Origin',(12.,-6.7,10.));
#23945=CARTESIAN_POINT('',(9.66,-7.5,10.));
#23946=CARTESIAN_POINT('',(9.66,-7.5,10.));
#23947=CARTESIAN_POINT('Origin',(12.,-7.5,10.));
#23948=CARTESIAN_POINT('Origin',(12.,-6.7,10.));
#23949=CARTESIAN_POINT('',(10.1,-6.7,10.));
#23950=CARTESIAN_POINT('Origin',(12.,-6.7,10.));
#23951=CARTESIAN_POINT('Origin',(12.,-7.8,10.));
#23952=CARTESIAN_POINT('',(10.1,-7.8,10.));
#23953=CARTESIAN_POINT('',(10.1,-7.8,10.));
#23954=CARTESIAN_POINT('Origin',(12.,-7.8,10.));
#23955=CARTESIAN_POINT('Origin',(12.,-7.8,10.));
#23956=CARTESIAN_POINT('',(9.1,-7.5,10.));
#23957=CARTESIAN_POINT('Origin',(12.,-7.5,10.));
#23958=CARTESIAN_POINT('',(9.1,-7.8,10.));
#23959=CARTESIAN_POINT('',(9.1,-7.8,10.));
#23960=CARTESIAN_POINT('Origin',(12.,-7.8,10.));
#23961=CARTESIAN_POINT('Origin',(12.,-7.5,10.));
#23962=CARTESIAN_POINT('Origin',(12.,-7.8,10.));
#23963=CARTESIAN_POINT('',(0.,0.,0.));
#23964=CARTESIAN_POINT('Origin',(10.161522368915,7.4,8.16152236891498));
#23965=CARTESIAN_POINT('',(9.93652236891498,7.5,8.16152236891498));
#23966=CARTESIAN_POINT('Origin',(10.161522368915,7.5,8.16152236891498));
#23967=CARTESIAN_POINT('',(9.93652236891498,7.8,8.16152236891498));
#23968=CARTESIAN_POINT('',(9.93652236891498,7.4,8.16152236891498));
#23969=CARTESIAN_POINT('Origin',(10.161522368915,7.8,8.16152236891498));
#23970=CARTESIAN_POINT('Origin',(10.161522368915,7.4,11.838477631085));
#23971=CARTESIAN_POINT('',(9.93652236891498,7.5,11.838477631085));
#23972=CARTESIAN_POINT('Origin',(10.161522368915,7.5,11.838477631085));
#23973=CARTESIAN_POINT('',(9.93652236891498,7.8,11.838477631085));
#23974=CARTESIAN_POINT('',(9.93652236891498,7.4,11.838477631085));
#23975=CARTESIAN_POINT('Origin',(10.161522368915,7.8,11.838477631085));
#23976=CARTESIAN_POINT('Origin',(13.838477631085,7.4,11.838477631085));
#23977=CARTESIAN_POINT('',(13.613477631085,7.5,11.838477631085));
#23978=CARTESIAN_POINT('Origin',(13.838477631085,7.5,11.838477631085));
#23979=CARTESIAN_POINT('',(13.613477631085,7.8,11.838477631085));
#23980=CARTESIAN_POINT('',(13.613477631085,7.4,11.838477631085));
#23981=CARTESIAN_POINT('Origin',(13.838477631085,7.8,11.838477631085));
#23982=CARTESIAN_POINT('Origin',(13.838477631085,7.4,8.16152236891498));
#23983=CARTESIAN_POINT('',(13.613477631085,7.5,8.16152236891498));
#23984=CARTESIAN_POINT('Origin',(13.838477631085,7.5,8.16152236891498));
#23985=CARTESIAN_POINT('',(13.613477631085,7.8,8.16152236891498));
#23986=CARTESIAN_POINT('',(13.613477631085,7.4,8.16152236891498));
#23987=CARTESIAN_POINT('Origin',(13.838477631085,7.8,8.16152236891498));
#23988=CARTESIAN_POINT('Origin',(12.,6.7,10.));
#23989=CARTESIAN_POINT('',(9.66,7.5,10.));
#23990=CARTESIAN_POINT('Origin',(12.,7.5,10.));
#23991=CARTESIAN_POINT('',(9.66,6.7,10.));
#23992=CARTESIAN_POINT('',(9.66,6.7,10.));
#23993=CARTESIAN_POINT('Origin',(12.,6.7,10.));
#23994=CARTESIAN_POINT('Origin',(12.,6.7,10.));
#23995=CARTESIAN_POINT('',(10.1,6.7,10.));
#23996=CARTESIAN_POINT('Origin',(12.,6.7,10.));
#23997=CARTESIAN_POINT('Origin',(12.,7.5,10.));
#23998=CARTESIAN_POINT('',(10.1,7.8,10.));
#23999=CARTESIAN_POINT('Origin',(12.,7.8,10.));
#24000=CARTESIAN_POINT('',(10.1,7.5,10.));
#24001=CARTESIAN_POINT('Origin',(12.,7.5,10.));
#24002=CARTESIAN_POINT('',(9.1,7.8,10.));
#24003=CARTESIAN_POINT('Origin',(12.,7.8,10.));
#24004=CARTESIAN_POINT('',(9.1,7.5,10.));
#24005=CARTESIAN_POINT('',(9.1,7.5,10.));
#24006=CARTESIAN_POINT('Origin',(12.,7.5,10.));
#24007=CARTESIAN_POINT('Origin',(12.,7.8,10.));
#24008=CARTESIAN_POINT('Origin',(12.,7.5,10.));
#24009=CARTESIAN_POINT('',(0.,0.,0.));
#24010=CARTESIAN_POINT('Origin',(14.5,-3.5,15.9));
#24011=CARTESIAN_POINT('',(14.275,-3.5,16.));
#24012=CARTESIAN_POINT('Origin',(14.5,-3.5,16.));
#24013=CARTESIAN_POINT('',(14.275,-3.5,16.5));
#24014=CARTESIAN_POINT('',(14.275,-3.5,15.9));
#24015=CARTESIAN_POINT('Origin',(14.5,-3.5,16.5));
#24016=CARTESIAN_POINT('Origin',(1.5,3.5,15.9));
#24017=CARTESIAN_POINT('',(1.275,3.5,16.));
#24018=CARTESIAN_POINT('Origin',(1.5,3.5,16.));
#24019=CARTESIAN_POINT('',(1.275,3.5,16.5));
#24020=CARTESIAN_POINT('',(1.275,3.5,15.9));
#24021=CARTESIAN_POINT('Origin',(1.5,3.5,16.5));
#24022=CARTESIAN_POINT('Origin',(1.5,-3.5,15.9));
#24023=CARTESIAN_POINT('',(1.275,-3.5,16.));
#24024=CARTESIAN_POINT('Origin',(1.5,-3.5,16.));
#24025=CARTESIAN_POINT('',(1.275,-3.5,16.5));
#24026=CARTESIAN_POINT('',(1.275,-3.5,15.9));
#24027=CARTESIAN_POINT('Origin',(1.5,-3.5,16.5));
#24028=CARTESIAN_POINT('Origin',(14.5,3.5,15.9));
#24029=CARTESIAN_POINT('',(14.275,3.5,16.));
#24030=CARTESIAN_POINT('Origin',(14.5,3.5,16.));
#24031=CARTESIAN_POINT('',(14.275,3.5,16.5));
#24032=CARTESIAN_POINT('',(14.275,3.5,15.9));
#24033=CARTESIAN_POINT('Origin',(14.5,3.5,16.5));
#24034=CARTESIAN_POINT('Origin',(15.,4.,16.));
#24035=CARTESIAN_POINT('',(15.,4.,16.));
#24036=CARTESIAN_POINT('',(1.,4.,16.));
#24037=CARTESIAN_POINT('',(15.,4.,16.));
#24038=CARTESIAN_POINT('',(1.,4.,16.5));
#24039=CARTESIAN_POINT('',(1.,4.,16.));
#24040=CARTESIAN_POINT('',(15.,4.,16.5));
#24041=CARTESIAN_POINT('',(15.,4.,16.5));
#24042=CARTESIAN_POINT('',(15.,4.,16.));
#24043=CARTESIAN_POINT('Origin',(15.,-4.,16.));
#24044=CARTESIAN_POINT('',(15.,-4.,16.));
#24045=CARTESIAN_POINT('',(15.,-4.,16.));
#24046=CARTESIAN_POINT('',(15.,-4.,16.5));
#24047=CARTESIAN_POINT('',(15.,-4.,16.5));
#24048=CARTESIAN_POINT('',(15.,-4.,16.));
#24049=CARTESIAN_POINT('Origin',(1.,-4.,16.));
#24050=CARTESIAN_POINT('',(1.,-4.,16.));
#24051=CARTESIAN_POINT('',(1.,-4.,16.));
#24052=CARTESIAN_POINT('',(1.,-4.,16.5));
#24053=CARTESIAN_POINT('',(1.,-4.,16.5));
#24054=CARTESIAN_POINT('',(1.,-4.,16.));
#24055=CARTESIAN_POINT('Origin',(1.,4.,16.));
#24056=CARTESIAN_POINT('',(1.,4.,16.));
#24057=CARTESIAN_POINT('',(1.,4.,16.5));
#24058=CARTESIAN_POINT('Origin',(8.,0.,16.5));
#24059=CARTESIAN_POINT('Origin',(8.,0.,16.));
#24060=CARTESIAN_POINT('',(0.,0.,0.));
#24061=CARTESIAN_POINT('Origin',(-3.5,8.5,-0.5));
#24062=CARTESIAN_POINT('',(-3.5,8.5,-0.5));
#24063=CARTESIAN_POINT('',(-5.5,8.5,-0.5));
#24064=CARTESIAN_POINT('',(-3.5,8.5,-0.5));
#24065=CARTESIAN_POINT('',(-5.5,8.5,0.));
#24066=CARTESIAN_POINT('',(-5.5,8.5,-0.5));
#24067=CARTESIAN_POINT('',(-3.5,8.5,0.));
#24068=CARTESIAN_POINT('',(-3.5,8.5,0.));
#24069=CARTESIAN_POINT('',(-3.5,8.5,-0.5));
#24070=CARTESIAN_POINT('Origin',(-3.5,-8.5,-0.5));
#24071=CARTESIAN_POINT('',(-3.5,-8.5,-0.5));
#24072=CARTESIAN_POINT('',(-3.5,-8.5,-0.5));
#24073=CARTESIAN_POINT('',(-3.5,-8.5,0.));
#24074=CARTESIAN_POINT('',(-3.5,-8.5,0.));
#24075=CARTESIAN_POINT('',(-3.5,-8.5,-0.5));
#24076=CARTESIAN_POINT('Origin',(-5.5,-8.5,-0.5));
#24077=CARTESIAN_POINT('',(-5.5,-8.5,-0.5));
#24078=CARTESIAN_POINT('',(-5.5,-8.5,-0.5));
#24079=CARTESIAN_POINT('',(-5.5,-8.5,0.));
#24080=CARTESIAN_POINT('',(-5.5,-8.5,0.));
#24081=CARTESIAN_POINT('',(-5.5,-8.5,-0.5));
#24082=CARTESIAN_POINT('Origin',(-5.5,8.5,-0.5));
#24083=CARTESIAN_POINT('',(-5.5,8.5,-0.5));
#24084=CARTESIAN_POINT('',(-5.5,8.5,0.));
#24085=CARTESIAN_POINT('Origin',(-4.5,0.,0.));
#24086=CARTESIAN_POINT('Origin',(-4.5,0.,-0.5));
#24087=CARTESIAN_POINT('',(0.,0.,0.));
#24088=CARTESIAN_POINT('Origin',(18.5,8.5,-0.5));
#24089=CARTESIAN_POINT('',(18.5,8.5,-0.5));
#24090=CARTESIAN_POINT('',(16.5,8.5,-0.5));
#24091=CARTESIAN_POINT('',(18.5,8.5,-0.5));
#24092=CARTESIAN_POINT('',(16.5,8.5,0.));
#24093=CARTESIAN_POINT('',(16.5,8.5,-0.5));
#24094=CARTESIAN_POINT('',(18.5,8.5,0.));
#24095=CARTESIAN_POINT('',(18.5,8.5,0.));
#24096=CARTESIAN_POINT('',(18.5,8.5,-0.5));
#24097=CARTESIAN_POINT('Origin',(18.5,-8.5,-0.5));
#24098=CARTESIAN_POINT('',(18.5,-8.5,-0.5));
#24099=CARTESIAN_POINT('',(18.5,-8.5,-0.5));
#24100=CARTESIAN_POINT('',(18.5,-8.5,0.));
#24101=CARTESIAN_POINT('',(18.5,-8.5,0.));
#24102=CARTESIAN_POINT('',(18.5,-8.5,-0.5));
#24103=CARTESIAN_POINT('Origin',(16.5,-8.5,-0.5));
#24104=CARTESIAN_POINT('',(16.5,-8.5,-0.5));
#24105=CARTESIAN_POINT('',(16.5,-8.5,-0.5));
#24106=CARTESIAN_POINT('',(16.5,-8.5,0.));
#24107=CARTESIAN_POINT('',(16.5,-8.5,0.));
#24108=CARTESIAN_POINT('',(16.5,-8.5,-0.5));
#24109=CARTESIAN_POINT('Origin',(16.5,8.5,-0.5));
#24110=CARTESIAN_POINT('',(16.5,8.5,-0.5));
#24111=CARTESIAN_POINT('',(16.5,8.5,0.));
#24112=CARTESIAN_POINT('Origin',(17.5,0.,0.));
#24113=CARTESIAN_POINT('Origin',(17.5,0.,-0.5));
#24114=CARTESIAN_POINT('',(0.,0.,0.));
#24115=CARTESIAN_POINT('Origin',(0.144337567297406,-0.6,-0.25));
#24116=CARTESIAN_POINT('',(0.288675134594813,-0.6,0.));
#24117=CARTESIAN_POINT('',(0.144337567297406,-0.6,-0.25));
#24118=CARTESIAN_POINT('',(0.288675134594813,-0.6,0.));
#24119=CARTESIAN_POINT('',(0.144337567297406,-0.96,-0.25));
#24120=CARTESIAN_POINT('',(0.144337567297406,-0.6,-0.25));
#24121=CARTESIAN_POINT('',(0.288675134594813,-0.96,0.));
#24122=CARTESIAN_POINT('',(0.288675134594813,-0.96,0.));
#24123=CARTESIAN_POINT('',(0.288675134594813,-0.6,0.));
#24124=CARTESIAN_POINT('Origin',(-0.144337567297406,-0.6,-0.25));
#24125=CARTESIAN_POINT('',(-0.144337567297406,-0.6,-0.25));
#24126=CARTESIAN_POINT('',(0.144337567297406,-0.6,-0.25));
#24127=CARTESIAN_POINT('',(-0.144337567297406,-0.96,-0.25));
#24128=CARTESIAN_POINT('',(-0.144337567297406,-0.6,-0.25));
#24129=CARTESIAN_POINT('',(0.144337567297406,-0.96,-0.25));
#24130=CARTESIAN_POINT('Origin',(-0.288675134594813,-0.6,-8.32667268468867E-17));
#24131=CARTESIAN_POINT('',(-0.288675134594813,-0.6,-3.53525079574969E-17));
#24132=CARTESIAN_POINT('',(-0.144337567297406,-0.6,-0.25));
#24133=CARTESIAN_POINT('',(-0.288675134594813,-0.96,-5.55111512312578E-17));
#24134=CARTESIAN_POINT('',(-0.288675134594813,-0.6,-3.53525079574969E-17));
#24135=CARTESIAN_POINT('',(-0.144337567297406,-0.96,-0.25));
#24136=CARTESIAN_POINT('Origin',(-0.144337567297407,-0.6,0.25));
#24137=CARTESIAN_POINT('',(-0.144337567297407,-0.6,0.25));
#24138=CARTESIAN_POINT('',(-0.288675134594813,-0.6,-3.53525079574969E-17));
#24139=CARTESIAN_POINT('',(-0.144337567297407,-0.96,0.25));
#24140=CARTESIAN_POINT('',(-0.144337567297407,-0.6,0.25));
#24141=CARTESIAN_POINT('',(-0.288675134594813,-0.96,-3.53525079574969E-17));
#24142=CARTESIAN_POINT('Origin',(0.144337567297406,-0.6,0.25));
#24143=CARTESIAN_POINT('',(0.144337567297406,-0.6,0.25));
#24144=CARTESIAN_POINT('',(-0.144337567297407,-0.6,0.25));
#24145=CARTESIAN_POINT('',(0.144337567297406,-0.96,0.25));
#24146=CARTESIAN_POINT('',(0.144337567297406,-0.6,0.25));
#24147=CARTESIAN_POINT('',(-0.144337567297407,-0.96,0.25));
#24148=CARTESIAN_POINT('Origin',(0.288675134594813,-0.6,0.));
#24149=CARTESIAN_POINT('',(0.144337567297406,-0.6,0.25));
#24150=CARTESIAN_POINT('',(0.144337567297406,-0.96,0.25));
#24151=CARTESIAN_POINT('Origin',(0.,-0.6,0.));
#24152=CARTESIAN_POINT('Origin',(0.,-0.96,0.));
#24153=CARTESIAN_POINT('Origin',(0.,-1.8,0.));
#24154=CARTESIAN_POINT('',(-0.2942,-1.8,3.60291088309151E-17));
#24155=CARTESIAN_POINT('Origin',(0.,-1.8,0.));
#24156=CARTESIAN_POINT('Origin',(0.45,0.6,0.));
#24157=CARTESIAN_POINT('',(-0.45,0.6,-5.51091059616309E-17));
#24158=CARTESIAN_POINT('Origin',(0.,0.6,0.));
#24159=CARTESIAN_POINT('Origin',(0.,0.575,0.));
#24160=CARTESIAN_POINT('',(-0.5,0.55,-6.12323399573677E-17));
#24161=CARTESIAN_POINT('Origin',(0.,0.55,0.));
#24162=CARTESIAN_POINT('',(-0.475,0.575,-5.81707229594993E-17));
#24163=CARTESIAN_POINT('Origin',(0.,0.29,0.));
#24164=CARTESIAN_POINT('',(-0.5,0.0299999999999998,-6.12323399573677E-17));
#24165=CARTESIAN_POINT('Origin',(0.,0.0299999999999998,0.));
#24166=CARTESIAN_POINT('',(-0.5,0.29,-6.12323399573677E-17));
#24167=CARTESIAN_POINT('Origin',(0.,0.0150000000000001,0.));
#24168=CARTESIAN_POINT('',(-0.47,7.11236625150491E-17,-5.75583995599256E-17));
#24169=CARTESIAN_POINT('Origin',(0.,0.,0.));
#24170=CARTESIAN_POINT('',(-0.485,0.0150000000000001,-5.93953697586466E-17));
#24171=CARTESIAN_POINT('Origin',(0.32,0.,0.));
#24172=CARTESIAN_POINT('',(-0.32,-6.93889390390723E-18,-3.91886975727153E-17));
#24173=CARTESIAN_POINT('Origin',(0.,0.,0.));
#24174=CARTESIAN_POINT('Origin',(0.,-0.02,0.));
#24175=CARTESIAN_POINT('',(-0.2942,-0.0515999999999999,3.60291088309151E-17));
#24176=CARTESIAN_POINT('Origin',(0.,-0.0515999999999999,0.));
#24177=CARTESIAN_POINT('',(-0.31,-0.02,-3.7964050773568E-17));
#24178=CARTESIAN_POINT('Origin',(0.,-1.24,0.));
#24179=CARTESIAN_POINT('',(-0.2942,-1.24,-3.60291088309151E-17));
#24180=CARTESIAN_POINT('',(0.,0.,0.));
#24181=CARTESIAN_POINT('',(0.,0.,0.));
#24182=CARTESIAN_POINT('Origin',(0.,0.,0.));
#24183=CARTESIAN_POINT('',(-1.070235,-0.308121667383195,-1.31065986708547E-16));
#24184=CARTESIAN_POINT('',(-1.31065986708547E-16,-0.308121667383195,1.070235));
#24185=CARTESIAN_POINT('Origin',(0.,-0.308121667383195,0.));
#24186=CARTESIAN_POINT('Origin',(0.,-0.308121667383195,0.));
#24187=CARTESIAN_POINT('',(-1.31065986708547E-16,0.308121667383195,1.070235));
#24188=CARTESIAN_POINT('Origin',(-1.34711147906209E-16,0.,1.1));
#24189=CARTESIAN_POINT('',(-1.070235,0.308121667383195,1.31065986708547E-16));
#24190=CARTESIAN_POINT('Origin',(0.,0.308121667383195,0.));
#24191=CARTESIAN_POINT('Origin',(0.,0.308121667383195,0.));
#24192=CARTESIAN_POINT('Origin',(0.,0.,0.));
#24193=CARTESIAN_POINT('',(-1.070235,0.5,-1.31065986708547E-16));
#24194=CARTESIAN_POINT('',(-1.070235,0.,-1.31065986708547E-16));
#24195=CARTESIAN_POINT('Origin',(0.,0.5,0.));
#24196=CARTESIAN_POINT('Origin',(0.,0.,0.));
#24197=CARTESIAN_POINT('',(-0.6,-0.44,-7.34788079488412E-17));
#24198=CARTESIAN_POINT('Origin',(0.,-0.44,0.));
#24199=CARTESIAN_POINT('',(-0.6,0.44,-7.34788079488412E-17));
#24200=CARTESIAN_POINT('',(-0.6,0.,-7.34788079488412E-17));
#24201=CARTESIAN_POINT('Origin',(0.,0.44,0.));
#24202=CARTESIAN_POINT('Origin',(0.,0.47,0.));
#24203=CARTESIAN_POINT('',(-0.66,0.5,-8.08266887437253E-17));
#24204=CARTESIAN_POINT('',(-0.63,0.47,-7.71527483462832E-17));
#24205=CARTESIAN_POINT('Origin',(0.,0.5,0.));
#24206=CARTESIAN_POINT('Origin',(1.070235,0.5,0.));
#24207=CARTESIAN_POINT('Origin',(0.,0.,0.));
#24208=CARTESIAN_POINT('',(-1.070235,-0.5,-1.31065986708547E-16));
#24209=CARTESIAN_POINT('Origin',(0.,-0.5,0.));
#24210=CARTESIAN_POINT('',(-1.070235,0.,-1.31065986708547E-16));
#24211=CARTESIAN_POINT('Origin',(0.66,-0.5,0.));
#24212=CARTESIAN_POINT('',(-0.66,-0.5,-8.08266887437253E-17));
#24213=CARTESIAN_POINT('Origin',(0.,-0.5,0.));
#24214=CARTESIAN_POINT('Origin',(0.,-0.47,0.));
#24215=CARTESIAN_POINT('',(-0.63,-0.47,-7.71527483462832E-17));
#24216=CARTESIAN_POINT('',(0.,0.,0.));
#24217=CARTESIAN_POINT('Origin',(0.,0.,0.));
#24218=CARTESIAN_POINT('',(-1.129765,0.308121667383195,-1.38356309103871E-16));
#24219=CARTESIAN_POINT('',(-1.38356309103871E-16,0.308121667383195,1.129765));
#24220=CARTESIAN_POINT('Origin',(0.,0.308121667383195,0.));
#24221=CARTESIAN_POINT('Origin',(0.,0.308121667383195,0.));
#24222=CARTESIAN_POINT('',(-1.38356309103871E-16,-0.308121667383195,1.129765));
#24223=CARTESIAN_POINT('Origin',(-1.34711147906209E-16,0.,1.1));
#24224=CARTESIAN_POINT('',(-1.129765,-0.308121667383195,1.38356309103871E-16));
#24225=CARTESIAN_POINT('Origin',(0.,-0.308121667383195,0.));
#24226=CARTESIAN_POINT('Origin',(0.,-0.308121667383195,0.));
#24227=CARTESIAN_POINT('Origin',(0.,0.,0.));
#24228=CARTESIAN_POINT('',(-1.129765,-0.5,-1.38356309103871E-16));
#24229=CARTESIAN_POINT('Origin',(0.,-0.5,0.));
#24230=CARTESIAN_POINT('',(-1.129765,0.,-1.38356309103871E-16));
#24231=CARTESIAN_POINT('Origin',(1.54,0.5,0.));
#24232=CARTESIAN_POINT('',(-1.54,0.5,-1.88595607068692E-16));
#24233=CARTESIAN_POINT('Origin',(0.,0.5,0.));
#24234=CARTESIAN_POINT('',(-1.129765,0.5,-1.38356309103871E-16));
#24235=CARTESIAN_POINT('Origin',(0.,0.5,0.));
#24236=CARTESIAN_POINT('Origin',(0.,0.47,0.));
#24237=CARTESIAN_POINT('',(-1.6,0.44,-1.95943487863577E-16));
#24238=CARTESIAN_POINT('Origin',(0.,0.44,0.));
#24239=CARTESIAN_POINT('',(-1.57,0.47,-1.92269547466134E-16));
#24240=CARTESIAN_POINT('Origin',(0.,0.,0.));
#24241=CARTESIAN_POINT('',(-1.6,-0.44,-1.95943487863577E-16));
#24242=CARTESIAN_POINT('Origin',(0.,-0.44,0.));
#24243=CARTESIAN_POINT('',(-1.6,0.,-1.95943487863577E-16));
#24244=CARTESIAN_POINT('Origin',(0.,-0.47,0.));
#24245=CARTESIAN_POINT('',(-1.54,-0.5,-1.88595607068692E-16));
#24246=CARTESIAN_POINT('Origin',(0.,-0.5,0.));
#24247=CARTESIAN_POINT('',(-1.57,-0.47,-1.92269547466134E-16));
#24248=CARTESIAN_POINT('Origin',(1.129765,-0.5,0.));
#24249=CARTESIAN_POINT('Origin',(0.,0.,0.));
#24250=CARTESIAN_POINT('',(-1.129765,0.,-1.38356309103871E-16));
#24251=CARTESIAN_POINT('',(0.,0.,0.));
#24252=CARTESIAN_POINT('Origin',(1.1,0.,0.));
#24253=CARTESIAN_POINT('',(1.1,-2.23201749654651E-33,0.29765));
#24254=CARTESIAN_POINT('',(1.1,-2.23201749654651E-33,-0.29765));
#24255=CARTESIAN_POINT('Origin',(1.1,0.,0.));
#24256=CARTESIAN_POINT('Origin',(0.685838782044607,0.,-0.860014630714833));
#24257=CARTESIAN_POINT('',(0.918550922801216,-5.31350540756609E-33,-0.674432891191581));
#24258=CARTESIAN_POINT('',(0.453126641287998,8.49470414473068E-34,-1.04559637023808));
#24259=CARTESIAN_POINT('Origin',(0.685838782044607,0.,-0.860014630714833));
#24260=CARTESIAN_POINT('Origin',(-0.244773027351946,0.,-1.07242070340001));
#24261=CARTESIAN_POINT('',(0.0454142657089739,-2.23201749654651E-33,-1.1386540593921));
#24262=CARTESIAN_POINT('',(-0.534960320412865,-2.23201749654651E-33,-1.00618734740791));
#24263=CARTESIAN_POINT('Origin',(-0.244773027351946,0.,-1.07242070340001));
#24264=CARTESIAN_POINT('Origin',(-0.991065754692661,0.,-0.477272113029314));
#24265=CARTESIAN_POINT('',(-0.86192025974432,8.49470414473067E-34,-0.745445496560469));
#24266=CARTESIAN_POINT('',(-1.120211249641,-5.31350540756609E-33,-0.209098729498159));
#24267=CARTESIAN_POINT('Origin',(-0.991065754692661,0.,-0.477272113029314));
#24268=CARTESIAN_POINT('Origin',(-0.991065754692661,0.,0.477272113029314));
#24269=CARTESIAN_POINT('',(-1.120211249641,-2.23201749654651E-33,0.209098729498159));
#24270=CARTESIAN_POINT('',(-0.86192025974432,-2.23201749654651E-33,0.745445496560469));
#24271=CARTESIAN_POINT('Origin',(-0.991065754692661,0.,0.477272113029314));
#24272=CARTESIAN_POINT('Origin',(-0.244773027351946,0.,1.07242070340001));
#24273=CARTESIAN_POINT('',(-0.534960320412866,-2.23201749654651E-33,1.00618734740791));
#24274=CARTESIAN_POINT('',(0.0454142657089737,-2.23201749654651E-33,1.1386540593921));
#24275=CARTESIAN_POINT('Origin',(-0.244773027351946,0.,1.07242070340001));
#24276=CARTESIAN_POINT('Origin',(0.685838782044607,0.,0.860014630714833));
#24277=CARTESIAN_POINT('',(0.453126641287998,-2.23201749654651E-33,1.04559637023808));
#24278=CARTESIAN_POINT('',(0.918550922801216,-2.23201749654651E-33,0.674432891191581));
#24279=CARTESIAN_POINT('Origin',(0.685838782044607,0.,0.860014630714833));
#24280=CARTESIAN_POINT('',(0.,0.,0.));
#24281=CARTESIAN_POINT('Origin',(0.685838782044607,0.,0.860014630714833));
#24282=CARTESIAN_POINT('',(0.413083465285518,-0.05953,0.993751811093549));
#24283=CARTESIAN_POINT('',(0.876916659919095,-0.05953,0.623857181492959));
#24284=CARTESIAN_POINT('Ctrl Pts',(0.413083465285518,-0.05953,0.993751811093549));
#24285=CARTESIAN_POINT('Ctrl Pts',(0.419070565453383,-0.0925528133349865,
0.991263089003441));
#24286=CARTESIAN_POINT('Ctrl Pts',(0.430199341854858,-0.124911173756694,
0.986608710139579));
#24287=CARTESIAN_POINT('Ctrl Pts',(0.457978755888596,-0.177924977804098,
0.973971221090534));
#24288=CARTESIAN_POINT('Ctrl Pts',(0.473077587363685,-0.199697230012983,
0.966820759530997));
#24289=CARTESIAN_POINT('Ctrl Pts',(0.507057380724533,-0.237895043532788,
0.949440676105255));
#24290=CARTESIAN_POINT('Ctrl Pts',(0.525933334162555,-0.254319232363049,
0.939198248544428));
#24291=CARTESIAN_POINT('Ctrl Pts',(0.564362943424238,-0.28018331644634,
0.916597376014514));
#24292=CARTESIAN_POINT('Ctrl Pts',(0.585840553788742,-0.29104845371857,
0.903141581680914));
#24293=CARTESIAN_POINT('Ctrl Pts',(0.629305439856167,-0.30527573347708,
0.873412008702649));
#24294=CARTESIAN_POINT('Ctrl Pts',(0.651278921914856,-0.308638795020976,
0.857118508332695));
#24295=CARTESIAN_POINT('Ctrl Pts',(0.690705563850638,-0.308638795020976,
0.825676810575914));
#24296=CARTESIAN_POINT('Ctrl Pts',(0.711480111898423,-0.30527573347708,
0.807879894508811));
#24297=CARTESIAN_POINT('Ctrl Pts',(0.750136149454208,-0.29104845371857,
0.772120216227122));
#24298=CARTESIAN_POINT('Ctrl Pts',(0.768033796848072,-0.28018331644634,
0.754175290318038));
#24299=CARTESIAN_POINT('Ctrl Pts',(0.798619410861634,-0.254319232363049,
0.721738358858166));
#24300=CARTESIAN_POINT('Ctrl Pts',(0.812805334167529,-0.237895043532788,
0.705614819529209));
#24301=CARTESIAN_POINT('Ctrl Pts',(0.837310877969633,-0.199697230012983,
0.676354402927683));
#24302=CARTESIAN_POINT('Ctrl Pts',(0.847641868610495,-0.177924977804098,
0.663225258065736));
#24303=CARTESIAN_POINT('Ctrl Pts',(0.866144010579847,-0.124911173756694,
0.638954437806245));
#24304=CARTESIAN_POINT('Ctrl Pts',(0.873158080166742,-0.0925528133349865,
0.62914037979579));
#24305=CARTESIAN_POINT('Ctrl Pts',(0.876916659919095,-0.05953,0.623857181492959));
#24306=CARTESIAN_POINT('',(0.437601487681057,-0.05953,1.03511272300331));
#24307=CARTESIAN_POINT('Origin',(0.685838782044607,-0.05953,0.860014630714833));
#24308=CARTESIAN_POINT('',(0.911784794170997,-0.05953,0.656964154625313));
#24309=CARTESIAN_POINT('Ctrl Pts',(0.911784794170998,-0.0595300000000001,
0.656964154625312));
#24310=CARTESIAN_POINT('Ctrl Pts',(0.909827729890942,-0.0762225747374255,
0.659680317203144));
#24311=CARTESIAN_POINT('Ctrl Pts',(0.907004864562642,-0.0928409665394228,
0.663576540841106));
#24312=CARTESIAN_POINT('Ctrl Pts',(0.895234408667242,-0.144299303100741,
0.679480524217551));
#24313=CARTESIAN_POINT('Ctrl Pts',(0.882797231409153,-0.177024326825049,
0.695831250979106));
#24314=CARTESIAN_POINT('Ctrl Pts',(0.854332839576145,-0.227269801620064,
0.73042219438957));
#24315=CARTESIAN_POINT('Ctrl Pts',(0.834863020612702,-0.251265615809407,
0.752807465209441));
#24316=CARTESIAN_POINT('Ctrl Pts',(0.800439809856111,-0.279889827963178,
0.789147407129766));
#24317=CARTESIAN_POINT('Ctrl Pts',(0.781998747691871,-0.290879136862659,
0.80756613568454));
#24318=CARTESIAN_POINT('Ctrl Pts',(0.742239891936898,-0.305251990234487,
0.844254137480382));
#24319=CARTESIAN_POINT('Ctrl Pts',(0.720906778729541,-0.308638795020976,
0.862505527716294));
#24320=CARTESIAN_POINT('Ctrl Pts',(0.680463863683392,-0.308638795020976,
0.894757676234429));
#24321=CARTESIAN_POINT('Ctrl Pts',(0.657923009631182,-0.305251990234488,
0.91149460735272));
#24322=CARTESIAN_POINT('Ctrl Pts',(0.613307674922609,-0.290879136862659,
0.942092777160053));
#24323=CARTESIAN_POINT('Ctrl Pts',(0.591247219971725,-0.279889827963178,
0.955972930713954));
#24324=CARTESIAN_POINT('Ctrl Pts',(0.548158511259202,-0.251265615809407,
0.981446681891443));
#24325=CARTESIAN_POINT('Ctrl Pts',(0.522002043615455,-0.227269801620063,
0.995447160474328));
#24326=CARTESIAN_POINT('Ctrl Pts',(0.481944444320713,-0.177024326825049,
1.01550068154148));
#24327=CARTESIAN_POINT('Ctrl Pts',(0.463236132117164,-0.14429930310074,
1.0239876538093));
#24328=CARTESIAN_POINT('Ctrl Pts',(0.445111721969657,-0.0928409665394226,
1.03192403056628));
#24329=CARTESIAN_POINT('Ctrl Pts',(0.440685038163619,-0.0762225747374254,
1.03380912944435));
#24330=CARTESIAN_POINT('Ctrl Pts',(0.437601487681056,-0.05953,1.03511272300331));
#24331=CARTESIAN_POINT('Origin',(0.685838782044607,-0.05953,0.860014630714833));
#24332=CARTESIAN_POINT('Origin',(0.,-0.208355,0.));
#24333=CARTESIAN_POINT('',(0.0548532617164168,-0.05953,1.12247250791415));
#24334=CARTESIAN_POINT('Origin',(0.,-0.05953,0.));
#24335=CARTESIAN_POINT('',(-0.536443649899848,-0.05953,0.987512846410683));
#24336=CARTESIAN_POINT('Ctrl Pts',(0.0548532617164173,-0.0595300000000001,
1.12247250791414));
#24337=CARTESIAN_POINT('Ctrl Pts',(0.05150947068137,-0.0762225747374254,
1.12263591311425));
#24338=CARTESIAN_POINT('Ctrl Pts',(0.0467032526342597,-0.0928409665394227,
1.12285816383385));
#24339=CARTESIAN_POINT('Ctrl Pts',(0.0269302585198975,-0.144299303100741,
1.12357162229597));
#24340=CARTESIAN_POINT('Ctrl Pts',(0.006392292392153,-0.177024326825049,
1.12404235695137));
#24341=CARTESIAN_POINT('Ctrl Pts',(-0.0383992541984087,-0.227269801620063,
1.12335509974011));
#24342=CARTESIAN_POINT('Ctrl Pts',(-0.0680399972366993,-0.251265615809407,
1.12208997038458));
#24343=CARTESIAN_POINT('Ctrl Pts',(-0.117914228755037,-0.279889827963178,
1.1178344036749));
#24344=CARTESIAN_POINT('Ctrl Pts',(-0.14381238480104,-0.290879136862659,
1.11490049012186));
#24345=CARTESIAN_POINT('Ctrl Pts',(-0.19728546073067,-0.305251990234488,
1.10669035995599));
#24346=CARTESIAN_POINT('Ctrl Pts',(-0.224855950742601,-0.308638795020976,
1.10139101611326));
#24347=CARTESIAN_POINT('Ctrl Pts',(-0.275287440920027,-0.308638795020976,
1.0898803575765));
#24348=CARTESIAN_POINT('Ctrl Pts',(-0.302426893214945,-0.305251990234488,
1.08269251410343));
#24349=CARTESIAN_POINT('Ctrl Pts',(-0.35416671187353,-0.290879136862659,
1.06688848765783));
#24350=CARTESIAN_POINT('Ctrl Pts',(-0.3787731215897,-0.279889827963178,
1.05829506364875));
#24351=CARTESIAN_POINT('Ctrl Pts',(-0.425554672694338,-0.251265615809407,
1.04048957871266));
#24352=CARTESIAN_POINT('Ctrl Pts',(-0.452808978448581,-0.227269801620063,
1.02876878445619));
#24353=CARTESIAN_POINT('Ctrl Pts',(-0.493462957200432,-0.177024326825049,
1.0099536580922));
#24354=CARTESIAN_POINT('Ctrl Pts',(-0.511762781179148,-0.14429930310074,
1.00061845128527));
#24355=CARTESIAN_POINT('Ctrl Pts',(-0.529268075276157,-0.0928409665394226,
0.991396466802468));
#24356=CARTESIAN_POINT('Ctrl Pts',(-0.533501897135713,-0.0762225747374254,
0.989110885965947));
#24357=CARTESIAN_POINT('Ctrl Pts',(-0.536443649899848,-0.0595300000000001,
0.987512846410683));
#24358=CARTESIAN_POINT('',(-0.843383895613249,-0.05953,0.742736168477219));
#24359=CARTESIAN_POINT('Origin',(0.,-0.05953,0.));
#24360=CARTESIAN_POINT('',(-1.10653577764992,-0.05953,0.196295654879792));
#24361=CARTESIAN_POINT('Ctrl Pts',(-0.843383895613249,-0.0595300000000001,
0.742736168477219));
#24362=CARTESIAN_POINT('Ctrl Pts',(-0.84559647055299,-0.0762225747374255,
0.740223768851062));
#24363=CARTESIAN_POINT('Ctrl Pts',(-0.848766861100456,-0.0928409665394227,
0.736604687327351));
#24364=CARTESIAN_POINT('Ctrl Pts',(-0.861652925570091,-0.144299303100741,
0.721590372101268));
#24365=CARTESIAN_POINT('Ctrl Pts',(-0.87482617317514,-0.177024326825049,
0.705826641853758));
#24366=CARTESIAN_POINT('Ctrl Pts',(-0.902215926359523,-0.227269801620063,
0.670378702718353));
#24367=CARTESIAN_POINT('Ctrl Pts',(-0.919707509403859,-0.251265615809407,
0.646415841396062));
#24368=CARTESIAN_POINT('Ctrl Pts',(-0.947476448101718,-0.279889827963178,
0.604769294586516));
#24369=CARTESIAN_POINT('Ctrl Pts',(-0.961329858300736,-0.290879136862659,
0.582692035672022));
#24370=CARTESIAN_POINT('Ctrl Pts',(-0.988250837578047,-0.305251990234488,
0.535766169015486));
#24371=CARTESIAN_POINT('Ctrl Pts',(-1.00129756308006,-0.308638795020976,
0.510906605094603));
#24372=CARTESIAN_POINT('Ctrl Pts',(-1.02374168767024,-0.308638795020976,
0.46430090015576));
#24373=CARTESIAN_POINT('Ctrl Pts',(-1.03504317708586,-0.305251990234488,
0.438600874831839));
#24374=CARTESIAN_POINT('Ctrl Pts',(-1.05494634094458,-0.290879136862659,
0.388295406390235));
#24375=CARTESIAN_POINT('Ctrl Pts',(-1.06356957703048,-0.279889827963178,
0.363699428370917));
#24376=CARTESIAN_POINT('Ctrl Pts',(-1.0788165083757,-0.251265615809407,
0.316022600643821));
#24377=CARTESIAN_POINT('Ctrl Pts',(-1.08664560412098,-0.227269801620063,
0.287406530683752));
#24378=CARTESIAN_POINT('Ctrl Pts',(-1.09728268713976,-0.177024326825049,
0.243890930799337));
#24379=CARTESIAN_POINT('Ctrl Pts',(-1.10139388218929,-0.144299303100741,
0.22376314604679));
#24380=CARTESIAN_POINT('Ctrl Pts',(-1.10509821673782,-0.0928409665394227,
0.204327142733961));
#24381=CARTESIAN_POINT('Ctrl Pts',(-1.10595102243643,-0.0762225747374254,
0.199591971170104));
#24382=CARTESIAN_POINT('Ctrl Pts',(-1.10653577764992,-0.0595300000000001,
0.196295654879792));
#24383=CARTESIAN_POINT('',(-1.123812,-0.05953,1.37627276864339E-16));
#24384=CARTESIAN_POINT('Origin',(0.,-0.05953,0.));
#24385=CARTESIAN_POINT('',(-1.123812,-0.35718,1.37627276864339E-16));
#24386=CARTESIAN_POINT('',(-1.123812,-0.208355,1.37627276864339E-16));
#24387=CARTESIAN_POINT('Origin',(0.,-0.35718,0.));
#24388=CARTESIAN_POINT('',(-1.10653577764992,-0.05953,-0.196295654879793));
#24389=CARTESIAN_POINT('Origin',(0.,-0.05953,0.));
#24390=CARTESIAN_POINT('',(-0.843383895613249,-0.05953,-0.742736168477219));
#24391=CARTESIAN_POINT('Ctrl Pts',(-1.10653577764992,-0.0595300000000001,
-0.196295654879792));
#24392=CARTESIAN_POINT('Ctrl Pts',(-1.10595102243643,-0.0762225747374255,
-0.199591971170104));
#24393=CARTESIAN_POINT('Ctrl Pts',(-1.10509821673782,-0.0928409665394228,
-0.204327142733962));
#24394=CARTESIAN_POINT('Ctrl Pts',(-1.10139388218929,-0.144299303100741,
-0.22376314604679));
#24395=CARTESIAN_POINT('Ctrl Pts',(-1.09728268713976,-0.177024326825049,
-0.243890930799338));
#24396=CARTESIAN_POINT('Ctrl Pts',(-1.08664560412098,-0.227269801620063,
-0.287406530683753));
#24397=CARTESIAN_POINT('Ctrl Pts',(-1.0788165083757,-0.251265615809407,
-0.316022600643821));
#24398=CARTESIAN_POINT('Ctrl Pts',(-1.06356957703048,-0.279889827963178,
-0.363699428370918));
#24399=CARTESIAN_POINT('Ctrl Pts',(-1.05494634094458,-0.290879136862659,
-0.388295406390235));
#24400=CARTESIAN_POINT('Ctrl Pts',(-1.03504317708586,-0.305251990234488,
-0.438600874831839));
#24401=CARTESIAN_POINT('Ctrl Pts',(-1.02374168767024,-0.308638795020976,
-0.46430090015576));
#24402=CARTESIAN_POINT('Ctrl Pts',(-1.00129756308006,-0.308638795020976,
-0.510906605094603));
#24403=CARTESIAN_POINT('Ctrl Pts',(-0.988250837578047,-0.305251990234488,
-0.535766169015486));
#24404=CARTESIAN_POINT('Ctrl Pts',(-0.961329858300736,-0.290879136862659,
-0.582692035672022));
#24405=CARTESIAN_POINT('Ctrl Pts',(-0.947476448101718,-0.279889827963178,
-0.604769294586516));
#24406=CARTESIAN_POINT('Ctrl Pts',(-0.919707509403859,-0.251265615809407,
-0.646415841396062));
#24407=CARTESIAN_POINT('Ctrl Pts',(-0.902215926359523,-0.227269801620064,
-0.670378702718353));
#24408=CARTESIAN_POINT('Ctrl Pts',(-0.87482617317514,-0.177024326825049,
-0.705826641853758));
#24409=CARTESIAN_POINT('Ctrl Pts',(-0.861652925570091,-0.144299303100741,
-0.721590372101268));
#24410=CARTESIAN_POINT('Ctrl Pts',(-0.848766861100456,-0.0928409665394229,
-0.736604687327351));
#24411=CARTESIAN_POINT('Ctrl Pts',(-0.84559647055299,-0.0762225747374255,
-0.740223768851063));
#24412=CARTESIAN_POINT('Ctrl Pts',(-0.843383895613249,-0.0595300000000001,
-0.742736168477219));
#24413=CARTESIAN_POINT('',(-0.536443649899847,-0.05953,-0.987512846410683));
#24414=CARTESIAN_POINT('Origin',(0.,-0.05953,0.));
#24415=CARTESIAN_POINT('',(0.0548532617164172,-0.05953,-1.12247250791415));
#24416=CARTESIAN_POINT('Ctrl Pts',(-0.536443649899848,-0.0595300000000001,
-0.987512846410683));
#24417=CARTESIAN_POINT('Ctrl Pts',(-0.533501897135712,-0.0762225747374254,
-0.989110885965947));
#24418=CARTESIAN_POINT('Ctrl Pts',(-0.529268075276156,-0.0928409665394227,
-0.991396466802469));
#24419=CARTESIAN_POINT('Ctrl Pts',(-0.511762781179147,-0.144299303100741,
-1.00061845128527));
#24420=CARTESIAN_POINT('Ctrl Pts',(-0.493462957200432,-0.177024326825049,
-1.0099536580922));
#24421=CARTESIAN_POINT('Ctrl Pts',(-0.45280897844858,-0.227269801620063,
-1.02876878445619));
#24422=CARTESIAN_POINT('Ctrl Pts',(-0.425554672694337,-0.251265615809407,
-1.04048957871266));
#24423=CARTESIAN_POINT('Ctrl Pts',(-0.3787731215897,-0.279889827963178,
-1.05829506364875));
#24424=CARTESIAN_POINT('Ctrl Pts',(-0.354166711873529,-0.290879136862659,
-1.06688848765783));
#24425=CARTESIAN_POINT('Ctrl Pts',(-0.302426893214944,-0.305251990234488,
-1.08269251410343));
#24426=CARTESIAN_POINT('Ctrl Pts',(-0.275287440920027,-0.308638795020976,
-1.0898803575765));
#24427=CARTESIAN_POINT('Ctrl Pts',(-0.224855950742601,-0.308638795020976,
-1.10139101611326));
#24428=CARTESIAN_POINT('Ctrl Pts',(-0.19728546073067,-0.305251990234488,
-1.10669035995599));
#24429=CARTESIAN_POINT('Ctrl Pts',(-0.143812384801039,-0.290879136862659,
-1.11490049012186));
#24430=CARTESIAN_POINT('Ctrl Pts',(-0.117914228755037,-0.279889827963178,
-1.1178344036749));
#24431=CARTESIAN_POINT('Ctrl Pts',(-0.0680399972366989,-0.251265615809407,
-1.12208997038458));
#24432=CARTESIAN_POINT('Ctrl Pts',(-0.0383992541984084,-0.227269801620063,
-1.12335509974011));
#24433=CARTESIAN_POINT('Ctrl Pts',(0.00639229239215326,-0.177024326825049,
-1.12404235695137));
#24434=CARTESIAN_POINT('Ctrl Pts',(0.0269302585198977,-0.144299303100741,
-1.12357162229597));
#24435=CARTESIAN_POINT('Ctrl Pts',(0.04670325263426,-0.0928409665394228,
-1.12285816383385));
#24436=CARTESIAN_POINT('Ctrl Pts',(0.0515094706813703,-0.0762225747374255,
-1.12263591311425));
#24437=CARTESIAN_POINT('Ctrl Pts',(0.0548532617164176,-0.0595300000000001,
-1.12247250791414));
#24438=CARTESIAN_POINT('',(0.437601487681057,-0.05953,-1.03511272300331));
#24439=CARTESIAN_POINT('Origin',(0.,-0.05953,0.));
#24440=CARTESIAN_POINT('',(0.911784794170997,-0.05953,-0.656964154625313));
#24441=CARTESIAN_POINT('Ctrl Pts',(0.437601487681056,-0.0595300000000001,
-1.03511272300331));
#24442=CARTESIAN_POINT('Ctrl Pts',(0.440685038163619,-0.0762225747374255,
-1.03380912944435));
#24443=CARTESIAN_POINT('Ctrl Pts',(0.445111721969657,-0.0928409665394228,
-1.03192403056628));
#24444=CARTESIAN_POINT('Ctrl Pts',(0.463236132117164,-0.144299303100741,
-1.0239876538093));
#24445=CARTESIAN_POINT('Ctrl Pts',(0.481944444320713,-0.177024326825049,
-1.01550068154148));
#24446=CARTESIAN_POINT('Ctrl Pts',(0.522002043615455,-0.227269801620064,
-0.995447160474328));
#24447=CARTESIAN_POINT('Ctrl Pts',(0.548158511259203,-0.251265615809407,
-0.981446681891443));
#24448=CARTESIAN_POINT('Ctrl Pts',(0.591247219971725,-0.279889827963178,
-0.955972930713954));
#24449=CARTESIAN_POINT('Ctrl Pts',(0.613307674922609,-0.290879136862659,
-0.942092777160053));
#24450=CARTESIAN_POINT('Ctrl Pts',(0.657923009631182,-0.305251990234487,
-0.91149460735272));
#24451=CARTESIAN_POINT('Ctrl Pts',(0.680463863683393,-0.308638795020976,
-0.894757676234429));
#24452=CARTESIAN_POINT('Ctrl Pts',(0.720906778729542,-0.308638795020976,
-0.862505527716294));
#24453=CARTESIAN_POINT('Ctrl Pts',(0.742239891936899,-0.305251990234488,
-0.844254137480381));
#24454=CARTESIAN_POINT('Ctrl Pts',(0.781998747691872,-0.290879136862659,
-0.80756613568454));
#24455=CARTESIAN_POINT('Ctrl Pts',(0.800439809856112,-0.279889827963178,
-0.789147407129765));
#24456=CARTESIAN_POINT('Ctrl Pts',(0.834863020612702,-0.251265615809407,
-0.752807465209441));
#24457=CARTESIAN_POINT('Ctrl Pts',(0.854332839576145,-0.227269801620064,
-0.73042219438957));
#24458=CARTESIAN_POINT('Ctrl Pts',(0.882797231409153,-0.177024326825049,
-0.695831250979106));
#24459=CARTESIAN_POINT('Ctrl Pts',(0.895234408667242,-0.144299303100741,
-0.679480524217551));
#24460=CARTESIAN_POINT('Ctrl Pts',(0.907004864562642,-0.0928409665394228,
-0.663576540841106));
#24461=CARTESIAN_POINT('Ctrl Pts',(0.909827729890942,-0.0762225747374256,
-0.659680317203144));
#24462=CARTESIAN_POINT('Ctrl Pts',(0.911784794170998,-0.0595300000000001,
-0.656964154625312));
#24463=CARTESIAN_POINT('',(1.08212377959455,-0.05953,-0.303251606722892));
#24464=CARTESIAN_POINT('Origin',(0.,-0.05953,0.));
#24465=CARTESIAN_POINT('',(1.08212377959455,-0.05953,0.303251606722892));
#24466=CARTESIAN_POINT('Ctrl Pts',(1.08212377959455,-0.0595300000000001,
-0.303251606722892));
#24467=CARTESIAN_POINT('Ctrl Pts',(1.0830271513892,-0.0762225747374255,
-0.300028012588062));
#24468=CARTESIAN_POINT('Ctrl Pts',(1.08431331394788,-0.0928409665394228,
-0.2953917518996));
#24469=CARTESIAN_POINT('Ctrl Pts',(1.08940878963422,-0.144299303100741,
-0.276273267473431));
#24470=CARTESIAN_POINT('Ctrl Pts',(1.09443784939331,-0.177024326825049,
-0.256354979351213));
#24471=CARTESIAN_POINT('Ctrl Pts',(1.10373487993589,-0.227269801620064,
-0.212533521233765));
#24472=CARTESIAN_POINT('Ctrl Pts',(1.10909715583869,-0.251265615809407,
-0.183354415742157));
#24473=CARTESIAN_POINT('Ctrl Pts',(1.1160463456491,-0.279889827963178,-0.133783682657561));
#24474=CARTESIAN_POINT('Ctrl Pts',(1.11894887330541,-0.290879136862659,
-0.107881990270302));
#24475=CARTESIAN_POINT('Ctrl Pts',(1.12284346704144,-0.305251990234488,
-0.0539226701638766));
#24476=CARTESIAN_POINT('Ctrl Pts',(1.123812,-0.308638795020976,-0.025864214957475));
#24477=CARTESIAN_POINT('Ctrl Pts',(1.123812,-0.308638795020976,0.025864214957475));
#24478=CARTESIAN_POINT('Ctrl Pts',(1.12284346704144,-0.305251990234488,
0.0539226701638766));
#24479=CARTESIAN_POINT('Ctrl Pts',(1.11894887330541,-0.290879136862659,
0.107881990270302));
#24480=CARTESIAN_POINT('Ctrl Pts',(1.1160463456491,-0.279889827963178,0.133783682657561));
#24481=CARTESIAN_POINT('Ctrl Pts',(1.10909715583869,-0.251265615809407,
0.183354415742157));
#24482=CARTESIAN_POINT('Ctrl Pts',(1.10373487993589,-0.227269801620064,
0.212533521233765));
#24483=CARTESIAN_POINT('Ctrl Pts',(1.09443784939331,-0.177024326825049,
0.256354979351213));
#24484=CARTESIAN_POINT('Ctrl Pts',(1.08940878963422,-0.144299303100741,
0.276273267473431));
#24485=CARTESIAN_POINT('Ctrl Pts',(1.08431331394788,-0.0928409665394228,
0.2953917518996));
#24486=CARTESIAN_POINT('Ctrl Pts',(1.0830271513892,-0.0762225747374255,
0.300028012588062));
#24487=CARTESIAN_POINT('Ctrl Pts',(1.08212377959455,-0.0595300000000001,
0.303251606722892));
#24488=CARTESIAN_POINT('Origin',(0.,-0.05953,0.));
#24489=CARTESIAN_POINT('Origin',(0.,-0.05953,0.));
#24490=CARTESIAN_POINT('',(0.0589974094846122,-0.05953,1.07456964270265));
#24491=CARTESIAN_POINT('Origin',(0.,-0.05953,0.));
#24492=CARTESIAN_POINT('Origin',(-0.244773027351946,-0.05953,1.07242070340001));
#24493=CARTESIAN_POINT('Origin',(-0.244773027351946,0.,1.07242070340001));
#24494=CARTESIAN_POINT('',(-0.519393123750572,-0.05953,0.942555777842682));
#24495=CARTESIAN_POINT('Ctrl Pts',(-0.519393123750572,-0.05953,0.942555777842682));
#24496=CARTESIAN_POINT('Ctrl Pts',(-0.513714466572041,-0.0925528133349865,
0.945684988399766));
#24497=CARTESIAN_POINT('Ctrl Pts',(-0.503136848051455,-0.124911173756694,
0.951483858396181));
#24498=CARTESIAN_POINT('Ctrl Pts',(-0.47593627990192,-0.177924977804098,
0.965323333309091));
#24499=CARTESIAN_POINT('Ctrl Pts',(-0.460931856495794,-0.199697230012983,
0.972669835243841));
#24500=CARTESIAN_POINT('Ctrl Pts',(-0.426157505475872,-0.237895043532788,
0.988400002689705));
#24501=CARTESIAN_POINT('Ctrl Pts',(-0.406380688682952,-0.254319232363049,
0.996771768218699));
#24502=CARTESIAN_POINT('Ctrl Pts',(-0.364750145543744,-0.28018331644634,
1.01272583306292));
#24503=CARTESIAN_POINT('Ctrl Pts',(-0.340838910881557,-0.29104845371857,
1.02112815447116));
#24504=CARTESIAN_POINT('Ctrl Pts',(-0.290495481564827,-0.30527573347708,
1.036574285215));
#24505=CARTESIAN_POINT('Ctrl Pts',(-0.264056468041074,-0.308638795020976,
1.04359501395068));
#24506=CARTESIAN_POINT('Ctrl Pts',(-0.214892249704082,-0.308638795020976,
1.05481642595959));
#24507=CARTESIAN_POINT('Ctrl Pts',(-0.188025341585962,-0.30527573347708,
1.05996242598502));
#24508=CARTESIAN_POINT('Ctrl Pts',(-0.135965654106109,-0.29104845371857,
1.06788913840721));
#24509=CARTESIAN_POINT('Ctrl Pts',(-0.110776745452494,-0.28018331644634,
1.07069360430242));
#24510=CARTESIAN_POINT('Ctrl Pts',(-0.0663467128214646,-0.254319232363049,
1.07438230428002));
#24511=CARTESIAN_POINT('Ctrl Pts',(-0.0448960436540983,-0.237895043532788,
1.07542044338697));
#24512=CARTESIAN_POINT('Ctrl Pts',(-0.00674037211528124,-0.199697230012983,
1.07633607767727));
#24513=CARTESIAN_POINT('Ctrl Pts',(0.00996567398334777,-0.177924977804098,
1.07622728347683));
#24514=CARTESIAN_POINT('Ctrl Pts',(0.0404772621979741,-0.124911173756694,
1.07556023164702));
#24515=CARTESIAN_POINT('Ctrl Pts',(0.0525234025782719,-0.0925528133349865,
1.07492508698591));
#24516=CARTESIAN_POINT('Ctrl Pts',(0.0589974094846124,-0.05953,1.07456964270265));
#24517=CARTESIAN_POINT('Origin',(-0.244773027351946,-0.05953,1.07242070340001));
#24518=CARTESIAN_POINT('Origin',(0.,-0.05953,0.));
#24519=CARTESIAN_POINT('',(-0.803348093619616,-0.05953,0.716109245731214));
#24520=CARTESIAN_POINT('Origin',(0.,-0.05953,0.));
#24521=CARTESIAN_POINT('Origin',(-0.991065754692661,-0.05953,0.477272113029314));
#24522=CARTESIAN_POINT('Origin',(-0.991065754692661,0.,0.477272113029314));
#24523=CARTESIAN_POINT('',(-1.06075609691358,-0.05953,0.181596019242328));
#24524=CARTESIAN_POINT('Ctrl Pts',(-1.06075609691358,-0.05953,0.181596019242328));
#24525=CARTESIAN_POINT('Ctrl Pts',(-1.05966202740332,-0.0925528133349865,
0.187986803072856));
#24526=CARTESIAN_POINT('Ctrl Pts',(-1.05760072925372,-0.124911173756694,
0.199872254546857));
#24527=CARTESIAN_POINT('Ctrl Pts',(-1.05146158959546,-0.177924977804098,
0.22976728653846));
#24528=CARTESIAN_POINT('Ctrl Pts',(-1.04785021111757,-0.199697230012983,
0.246078686169301));
#24529=CARTESIAN_POINT('Ctrl Pts',(-1.03846709802406,-0.237895043532788,
0.283073967563097));
#24530=CARTESIAN_POINT('Ctrl Pts',(-1.03268176429485,-0.254319232363049,
0.303755815985685));
#24531=CARTESIAN_POINT('Ctrl Pts',(-1.01919893537026,-0.28018331644634,
0.346251081972725));
#24532=CARTESIAN_POINT('Ctrl Pts',(-1.01085972381132,-0.29104845371857,
0.370184399726282));
#24533=CARTESIAN_POINT('Ctrl Pts',(-0.99154738033959,-0.30527573347708,
0.419174982698463));
#24534=CARTESIAN_POINT('Ctrl Pts',(-0.980551951791748,-0.308638795020976,
0.444223188605045));
#24535=CARTESIAN_POINT('Ctrl Pts',(-0.958671816228589,-0.308638795020976,
0.489657758261848));
#24536=CARTESIAN_POINT('Ctrl Pts',(-0.945943877838127,-0.30527573347708,
0.51387163140139));
#24537=CARTESIAN_POINT('Ctrl Pts',(-0.91968254693063,-0.29104845371857,
0.559515758398093));
#24538=CARTESIAN_POINT('Ctrl Pts',(-0.906170138993533,-0.28018331644634,
0.580957796077825));
#24539=CARTESIAN_POINT('Ctrl Pts',(-0.8813524085237,-0.254319232363049,
0.617994461173994));
#24540=CARTESIAN_POINT('Ctrl Pts',(-0.868789784891799,-0.237895043532788,
0.635412538795143));
#24541=CARTESIAN_POINT('Ctrl Pts',(-0.845715984518854,-0.199697230012983,
0.66581473268113));
#24542=CARTESIAN_POINT('Ctrl Pts',(-0.835214876415962,-0.177924977804098,
0.678808213394124));
#24543=CARTESIAN_POINT('Ctrl Pts',(-0.815669690204649,-0.124911173756694,
0.702247233627224));
#24544=CARTESIAN_POINT('Ctrl Pts',(-0.807662468433796,-0.0925528133349865,
0.711269279199861));
#24545=CARTESIAN_POINT('Ctrl Pts',(-0.803348093619616,-0.05953,0.716109245731214));
#24546=CARTESIAN_POINT('Origin',(-0.991065754692661,-0.05953,0.477272113029314));
#24547=CARTESIAN_POINT('Origin',(0.,-0.05953,0.));
#24548=CARTESIAN_POINT('',(-1.076188,-0.05953,1.31795018948079E-16));
#24549=CARTESIAN_POINT('Origin',(0.,-0.05953,0.));
#24550=CARTESIAN_POINT('',(-1.06075609691358,-0.05953,-0.181596019242328));
#24551=CARTESIAN_POINT('Origin',(0.,-0.05953,0.));
#24552=CARTESIAN_POINT('Origin',(-0.991065754692661,-0.05953,-0.477272113029314));
#24553=CARTESIAN_POINT('Origin',(-0.991065754692661,0.,-0.477272113029314));
#24554=CARTESIAN_POINT('',(-0.803348093619616,-0.05953,-0.716109245731215));
#24555=CARTESIAN_POINT('Ctrl Pts',(-0.803348093619616,-0.05953,-0.716109245731215));
#24556=CARTESIAN_POINT('Ctrl Pts',(-0.807662468433795,-0.0925528133349865,
-0.711269279199862));
#24557=CARTESIAN_POINT('Ctrl Pts',(-0.815669690204649,-0.124911173756694,
-0.702247233627224));
#24558=CARTESIAN_POINT('Ctrl Pts',(-0.835214876415962,-0.177924977804098,
-0.678808213394124));
#24559=CARTESIAN_POINT('Ctrl Pts',(-0.845715984518854,-0.199697230012983,
-0.66581473268113));
#24560=CARTESIAN_POINT('Ctrl Pts',(-0.868789784891799,-0.237895043532788,
-0.635412538795143));
#24561=CARTESIAN_POINT('Ctrl Pts',(-0.8813524085237,-0.254319232363049,
-0.617994461173994));
#24562=CARTESIAN_POINT('Ctrl Pts',(-0.906170138993533,-0.28018331644634,
-0.580957796077826));
#24563=CARTESIAN_POINT('Ctrl Pts',(-0.91968254693063,-0.29104845371857,
-0.559515758398093));
#24564=CARTESIAN_POINT('Ctrl Pts',(-0.945943877838127,-0.30527573347708,
-0.51387163140139));
#24565=CARTESIAN_POINT('Ctrl Pts',(-0.958671816228589,-0.308638795020976,
-0.489657758261848));
#24566=CARTESIAN_POINT('Ctrl Pts',(-0.980551951791748,-0.308638795020976,
-0.444223188605045));
#24567=CARTESIAN_POINT('Ctrl Pts',(-0.99154738033959,-0.30527573347708,
-0.419174982698463));
#24568=CARTESIAN_POINT('Ctrl Pts',(-1.01085972381132,-0.29104845371857,
-0.370184399726282));
#24569=CARTESIAN_POINT('Ctrl Pts',(-1.01919893537026,-0.28018331644634,
-0.346251081972725));
#24570=CARTESIAN_POINT('Ctrl Pts',(-1.03268176429485,-0.254319232363049,
-0.303755815985685));
#24571=CARTESIAN_POINT('Ctrl Pts',(-1.03846709802406,-0.237895043532788,
-0.283073967563097));
#24572=CARTESIAN_POINT('Ctrl Pts',(-1.04785021111757,-0.199697230012983,
-0.246078686169302));
#24573=CARTESIAN_POINT('Ctrl Pts',(-1.05146158959546,-0.177924977804098,
-0.229767286538461));
#24574=CARTESIAN_POINT('Ctrl Pts',(-1.05760072925372,-0.124911173756694,
-0.199872254546858));
#24575=CARTESIAN_POINT('Ctrl Pts',(-1.05966202740332,-0.0925528133349864,
-0.187986803072857));
#24576=CARTESIAN_POINT('Ctrl Pts',(-1.06075609691358,-0.05953,-0.181596019242328));
#24577=CARTESIAN_POINT('Origin',(-0.991065754692661,-0.05953,-0.477272113029314));
#24578=CARTESIAN_POINT('Origin',(0.,-0.05953,0.));
#24579=CARTESIAN_POINT('',(-0.519393123750572,-0.05953,-0.942555777842682));
#24580=CARTESIAN_POINT('Origin',(0.,-0.05953,0.));
#24581=CARTESIAN_POINT('Origin',(-0.244773027351946,-0.05953,-1.07242070340001));
#24582=CARTESIAN_POINT('Origin',(-0.244773027351946,0.,-1.07242070340001));
#24583=CARTESIAN_POINT('',(0.0589974094846125,-0.05953,-1.07456964270265));
#24584=CARTESIAN_POINT('Ctrl Pts',(0.0589974094846127,-0.05953,-1.07456964270265));
#24585=CARTESIAN_POINT('Ctrl Pts',(0.0525234025782722,-0.0925528133349865,
-1.07492508698591));
#24586=CARTESIAN_POINT('Ctrl Pts',(0.0404772621979744,-0.124911173756694,
-1.07556023164702));
#24587=CARTESIAN_POINT('Ctrl Pts',(0.0099656739833481,-0.177924977804098,
-1.07622728347683));
#24588=CARTESIAN_POINT('Ctrl Pts',(-0.00674037211528096,-0.199697230012983,
-1.07633607767727));
#24589=CARTESIAN_POINT('Ctrl Pts',(-0.044896043654098,-0.237895043532788,
-1.07542044338697));
#24590=CARTESIAN_POINT('Ctrl Pts',(-0.0663467128214644,-0.254319232363049,
-1.07438230428002));
#24591=CARTESIAN_POINT('Ctrl Pts',(-0.110776745452493,-0.28018331644634,
-1.07069360430242));
#24592=CARTESIAN_POINT('Ctrl Pts',(-0.135965654106109,-0.29104845371857,
-1.06788913840721));
#24593=CARTESIAN_POINT('Ctrl Pts',(-0.188025341585962,-0.30527573347708,
-1.05996242598502));
#24594=CARTESIAN_POINT('Ctrl Pts',(-0.214892249704082,-0.308638795020976,
-1.05481642595959));
#24595=CARTESIAN_POINT('Ctrl Pts',(-0.264056468041074,-0.308638795020976,
-1.04359501395068));
#24596=CARTESIAN_POINT('Ctrl Pts',(-0.290495481564827,-0.30527573347708,
-1.036574285215));
#24597=CARTESIAN_POINT('Ctrl Pts',(-0.340838910881557,-0.291048453718569,
-1.02112815447116));
#24598=CARTESIAN_POINT('Ctrl Pts',(-0.364750145543744,-0.28018331644634,
-1.01272583306292));
#24599=CARTESIAN_POINT('Ctrl Pts',(-0.406380688682952,-0.254319232363049,
-0.996771768218699));
#24600=CARTESIAN_POINT('Ctrl Pts',(-0.426157505475872,-0.237895043532788,
-0.988400002689705));
#24601=CARTESIAN_POINT('Ctrl Pts',(-0.460931856495794,-0.199697230012983,
-0.972669835243841));
#24602=CARTESIAN_POINT('Ctrl Pts',(-0.475936279901919,-0.177924977804098,
-0.965323333309091));
#24603=CARTESIAN_POINT('Ctrl Pts',(-0.503136848051454,-0.124911173756694,
-0.951483858396181));
#24604=CARTESIAN_POINT('Ctrl Pts',(-0.513714466572041,-0.0925528133349865,
-0.945684988399766));
#24605=CARTESIAN_POINT('Ctrl Pts',(-0.519393123750572,-0.05953,-0.942555777842682));
#24606=CARTESIAN_POINT('Origin',(-0.244773027351946,-0.05953,-1.07242070340001));
#24607=CARTESIAN_POINT('Origin',(0.,-0.05953,0.));
#24608=CARTESIAN_POINT('',(0.413083465285518,-0.05953,-0.993751811093549));
#24609=CARTESIAN_POINT('Origin',(0.,-0.05953,0.));
#24610=CARTESIAN_POINT('Origin',(0.685838782044607,-0.05953,-0.860014630714833));
#24611=CARTESIAN_POINT('Origin',(0.685838782044607,0.,-0.860014630714833));
#24612=CARTESIAN_POINT('',(0.876916659919095,-0.05953,-0.623857181492959));
#24613=CARTESIAN_POINT('Ctrl Pts',(0.876916659919095,-0.05953,-0.623857181492958));
#24614=CARTESIAN_POINT('Ctrl Pts',(0.873158080166742,-0.0925528133349865,
-0.62914037979579));
#24615=CARTESIAN_POINT('Ctrl Pts',(0.866144010579847,-0.124911173756694,
-0.638954437806245));
#24616=CARTESIAN_POINT('Ctrl Pts',(0.847641868610495,-0.177924977804098,
-0.663225258065736));
#24617=CARTESIAN_POINT('Ctrl Pts',(0.837310877969633,-0.199697230012983,
-0.676354402927683));
#24618=CARTESIAN_POINT('Ctrl Pts',(0.81280533416753,-0.237895043532788,
-0.705614819529209));
#24619=CARTESIAN_POINT('Ctrl Pts',(0.798619410861634,-0.254319232363049,
-0.721738358858166));
#24620=CARTESIAN_POINT('Ctrl Pts',(0.768033796848072,-0.28018331644634,
-0.754175290318038));
#24621=CARTESIAN_POINT('Ctrl Pts',(0.750136149454208,-0.29104845371857,
-0.772120216227122));
#24622=CARTESIAN_POINT('Ctrl Pts',(0.711480111898423,-0.30527573347708,
-0.807879894508811));
#24623=CARTESIAN_POINT('Ctrl Pts',(0.690705563850638,-0.308638795020976,
-0.825676810575913));
#24624=CARTESIAN_POINT('Ctrl Pts',(0.651278921914856,-0.308638795020976,
-0.857118508332695));
#24625=CARTESIAN_POINT('Ctrl Pts',(0.629305439856167,-0.30527573347708,
-0.873412008702649));
#24626=CARTESIAN_POINT('Ctrl Pts',(0.585840553788742,-0.29104845371857,
-0.903141581680914));
#24627=CARTESIAN_POINT('Ctrl Pts',(0.564362943424239,-0.28018331644634,
-0.916597376014514));
#24628=CARTESIAN_POINT('Ctrl Pts',(0.525933334162556,-0.254319232363049,
-0.939198248544427));
#24629=CARTESIAN_POINT('Ctrl Pts',(0.507057380724533,-0.237895043532788,
-0.949440676105255));
#24630=CARTESIAN_POINT('Ctrl Pts',(0.473077587363686,-0.199697230012983,
-0.966820759530997));
#24631=CARTESIAN_POINT('Ctrl Pts',(0.457978755888596,-0.177924977804098,
-0.973971221090534));
#24632=CARTESIAN_POINT('Ctrl Pts',(0.430199341854858,-0.124911173756694,
-0.986608710139579));
#24633=CARTESIAN_POINT('Ctrl Pts',(0.419070565453384,-0.0925528133349865,
-0.991263089003441));
#24634=CARTESIAN_POINT('Ctrl Pts',(0.413083465285518,-0.05953,-0.993751811093549));
#24635=CARTESIAN_POINT('Origin',(0.685838782044607,-0.05953,-0.860014630714833));
#24636=CARTESIAN_POINT('Origin',(0.,-0.208355,0.));
#24637=CARTESIAN_POINT('',(-1.076188,-0.35718,1.31795018948079E-16));
#24638=CARTESIAN_POINT('Origin',(0.,-0.35718,0.));
#24639=CARTESIAN_POINT('',(-1.076188,-0.208355,1.31795018948079E-16));
#24640=CARTESIAN_POINT('',(1.03449977959455,-0.05953,0.296632461748266));
#24641=CARTESIAN_POINT('Origin',(0.,-0.05953,0.));
#24642=CARTESIAN_POINT('',(1.03449977959455,-0.05953,-0.296632461748266));
#24643=CARTESIAN_POINT('Ctrl Pts',(1.03449977959455,-0.05953,0.296632461748267));
#24644=CARTESIAN_POINT('Ctrl Pts',(1.03628691421076,-0.0925528133349865,
0.290399865505497));
#24645=CARTESIAN_POINT('Ctrl Pts',(1.03958665287714,-0.124911173756694,
0.278797079997872));
#24646=CARTESIAN_POINT('Ctrl Pts',(1.0470264474309,-0.177924977804098,0.249198913998601));
#24647=CARTESIAN_POINT('Ctrl Pts',(1.05084995891418,-0.199697230012983,
0.232935932341942));
#24648=CARTESIAN_POINT('Ctrl Pts',(1.05844771715377,-0.237895043532788,
0.195533155353269));
#24649=CARTESIAN_POINT('Ctrl Pts',(1.06220882929878,-0.254319232363049,
0.17438929156337));
#24650=CARTESIAN_POINT('Ctrl Pts',(1.06849922508772,-0.28018331644634,0.130252399648131));
#24651=CARTESIAN_POINT('Ctrl Pts',(1.07137013248666,-0.29104845371857,0.105070977154072));
#24652=CARTESIAN_POINT('Ctrl Pts',(1.07522652957392,-0.30527573347708,0.0525526752791107));
#24653=CARTESIAN_POINT('Ctrl Pts',(1.076188,-0.308638795020976,0.025214283908933));
#24654=CARTESIAN_POINT('Ctrl Pts',(1.076188,-0.308638795020976,-0.025214283908933));
#24655=CARTESIAN_POINT('Ctrl Pts',(1.07522652957392,-0.30527573347708,-0.0525526752791107));
#24656=CARTESIAN_POINT('Ctrl Pts',(1.07137013248666,-0.29104845371857,-0.105070977154072));
#24657=CARTESIAN_POINT('Ctrl Pts',(1.06849922508772,-0.28018331644634,-0.130252399648131));
#24658=CARTESIAN_POINT('Ctrl Pts',(1.06220882929878,-0.254319232363049,
-0.17438929156337));
#24659=CARTESIAN_POINT('Ctrl Pts',(1.05844771715377,-0.237895043532788,
-0.195533155353269));
#24660=CARTESIAN_POINT('Ctrl Pts',(1.05084995891418,-0.199697230012983,
-0.232935932341942));
#24661=CARTESIAN_POINT('Ctrl Pts',(1.0470264474309,-0.177924977804098,-0.249198913998601));
#24662=CARTESIAN_POINT('Ctrl Pts',(1.03958665287714,-0.124911173756694,
-0.278797079997872));
#24663=CARTESIAN_POINT('Ctrl Pts',(1.03628691421076,-0.0925528133349865,
-0.290399865505497));
#24664=CARTESIAN_POINT('Ctrl Pts',(1.03449977959455,-0.05953,-0.296632461748267));
#24665=CARTESIAN_POINT('Origin',(0.,-0.05953,0.));
#24666=CARTESIAN_POINT('Origin',(0.,-0.05953,0.));
#24667=CARTESIAN_POINT('Origin',(1.1,-0.05953,0.));
#24668=CARTESIAN_POINT('Origin',(1.1,0.,0.));
#24669=CARTESIAN_POINT('Origin',(1.1,-0.05953,0.));
#24670=CARTESIAN_POINT('Origin',(0.,-0.35718,0.));
#24671=CARTESIAN_POINT('Origin',(0.,-0.05953,0.));
#24672=CARTESIAN_POINT('',(0.,0.,0.));
#24673=CARTESIAN_POINT('Origin',(1.119765,0.495,0.));
#24674=CARTESIAN_POINT('',(-1.119765,0.495,-1.37131662304724E-16));
#24675=CARTESIAN_POINT('Origin',(0.,0.495,0.));
#24676=CARTESIAN_POINT('',(-1.085235,0.495,-1.32902956907268E-16));
#24677=CARTESIAN_POINT('Origin',(0.,0.495,0.));
#24678=CARTESIAN_POINT('Origin',(0.,0.4575,0.));
#24679=CARTESIAN_POINT('',(-1.119765,0.42,-1.37131662304724E-16));
#24680=CARTESIAN_POINT('Origin',(0.,0.42,0.));
#24681=CARTESIAN_POINT('',(-1.119765,0.4575,-1.37131662304724E-16));
#24682=CARTESIAN_POINT('Origin',(1.085235,0.42,0.));
#24683=CARTESIAN_POINT('',(-1.085235,0.42,-1.32902956907268E-16));
#24684=CARTESIAN_POINT('Origin',(0.,0.42,0.));
#24685=CARTESIAN_POINT('Origin',(0.,0.4575,0.));
#24686=CARTESIAN_POINT('',(-1.085235,0.4575,-1.32902956907268E-16));
#24687=CARTESIAN_POINT('Origin',(1.119765,-0.42,0.));
#24688=CARTESIAN_POINT('',(-1.119765,-0.42,-1.37131662304724E-16));
#24689=CARTESIAN_POINT('Origin',(0.,-0.42,0.));
#24690=CARTESIAN_POINT('',(-1.085235,-0.42,-1.32902956907268E-16));
#24691=CARTESIAN_POINT('Origin',(0.,-0.42,0.));
#24692=CARTESIAN_POINT('Origin',(0.,-0.4575,0.));
#24693=CARTESIAN_POINT('',(-1.119765,-0.495,-1.37131662304724E-16));
#24694=CARTESIAN_POINT('Origin',(0.,-0.495,0.));
#24695=CARTESIAN_POINT('',(-1.119765,-0.4575,-1.37131662304724E-16));
#24696=CARTESIAN_POINT('Origin',(1.085235,-0.495,0.));
#24697=CARTESIAN_POINT('',(-1.085235,-0.495,-1.32902956907268E-16));
#24698=CARTESIAN_POINT('Origin',(0.,-0.495,0.));
#24699=CARTESIAN_POINT('Origin',(0.,-0.4575,0.));
#24700=CARTESIAN_POINT('',(-1.085235,-0.4575,-1.32902956907268E-16));
#24701=CARTESIAN_POINT('',(0.,0.,0.));
#24702=CARTESIAN_POINT('',(0.,0.,0.));
#24703=CARTESIAN_POINT('',(0.,0.,0.));
#24704=CARTESIAN_POINT('',(0.,0.,0.));
#24705=CARTESIAN_POINT('',(0.,0.,0.));
#24706=CARTESIAN_POINT('',(0.,0.,0.));
#24707=CARTESIAN_POINT('',(0.,0.,0.));
#24708=CARTESIAN_POINT('Origin',(0.,0.,0.));
#24709=CARTESIAN_POINT('',(-1.63531,-0.410863395882378,-2.00267715711366E-16));
#24710=CARTESIAN_POINT('',(-2.00267715711366E-16,-0.410863395882378,1.63531));
#24711=CARTESIAN_POINT('Origin',(0.,-0.410863395882378,0.));
#24712=CARTESIAN_POINT('Origin',(0.,-0.410863395882378,0.));
#24713=CARTESIAN_POINT('',(-2.00267715711366E-16,0.410863395882378,1.63531));
#24714=CARTESIAN_POINT('Origin',(-2.05128338857182E-16,0.,1.675));
#24715=CARTESIAN_POINT('',(-1.63531,0.410863395882378,2.00267715711366E-16));
#24716=CARTESIAN_POINT('Origin',(0.,0.410863395882378,0.));
#24717=CARTESIAN_POINT('Origin',(0.,0.410863395882378,0.));
#24718=CARTESIAN_POINT('Origin',(0.,0.,0.));
#24719=CARTESIAN_POINT('',(-1.63531,0.7,-2.00267715711366E-16));
#24720=CARTESIAN_POINT('',(-1.63531,0.,-2.00267715711366E-16));
#24721=CARTESIAN_POINT('Origin',(0.,0.7,0.));
#24722=CARTESIAN_POINT('Origin',(0.,0.,0.));
#24723=CARTESIAN_POINT('',(-1.,-0.6,-1.22464679914735E-16));
#24724=CARTESIAN_POINT('Origin',(0.,-0.6,0.));
#24725=CARTESIAN_POINT('',(-1.,0.6,-1.22464679914735E-16));
#24726=CARTESIAN_POINT('',(-1.,0.,-1.22464679914735E-16));
#24727=CARTESIAN_POINT('Origin',(0.,0.6,0.));
#24728=CARTESIAN_POINT('Origin',(0.,0.65,0.));
#24729=CARTESIAN_POINT('',(-1.1,0.7,-1.34711147906209E-16));
#24730=CARTESIAN_POINT('',(-1.05,0.65,-1.28587913910472E-16));
#24731=CARTESIAN_POINT('Origin',(0.,0.7,0.));
#24732=CARTESIAN_POINT('Origin',(1.63531,0.7,0.));
#24733=CARTESIAN_POINT('Origin',(0.,0.,0.));
#24734=CARTESIAN_POINT('',(-1.63531,-0.7,-2.00267715711366E-16));
#24735=CARTESIAN_POINT('Origin',(0.,-0.7,0.));
#24736=CARTESIAN_POINT('',(-1.63531,0.,-2.00267715711366E-16));
#24737=CARTESIAN_POINT('Origin',(1.1,-0.7,0.));
#24738=CARTESIAN_POINT('',(-1.1,-0.7,-1.34711147906209E-16));
#24739=CARTESIAN_POINT('Origin',(0.,-0.7,0.));
#24740=CARTESIAN_POINT('Origin',(0.,-0.65,0.));
#24741=CARTESIAN_POINT('',(-1.05,-0.65,-1.28587913910472E-16));
#24742=CARTESIAN_POINT('',(0.,0.,0.));
#24743=CARTESIAN_POINT('Origin',(0.,0.,0.));
#24744=CARTESIAN_POINT('',(-1.71469,0.410863395882378,-2.09988962002998E-16));
#24745=CARTESIAN_POINT('',(-2.09988962002998E-16,0.410863395882378,1.71469));
#24746=CARTESIAN_POINT('Origin',(0.,0.410863395882378,0.));
#24747=CARTESIAN_POINT('Origin',(0.,0.410863395882378,0.));
#24748=CARTESIAN_POINT('',(-2.09988962002998E-16,-0.410863395882378,1.71469));
#24749=CARTESIAN_POINT('Origin',(-2.05128338857182E-16,0.,1.675));
#24750=CARTESIAN_POINT('',(-1.71469,-0.410863395882378,2.09988962002998E-16));
#24751=CARTESIAN_POINT('Origin',(0.,-0.410863395882378,0.));
#24752=CARTESIAN_POINT('Origin',(0.,-0.410863395882378,0.));
#24753=CARTESIAN_POINT('Origin',(0.,0.,0.));
#24754=CARTESIAN_POINT('',(-1.71469,-0.7,-2.09988962002998E-16));
#24755=CARTESIAN_POINT('Origin',(0.,-0.7,0.));
#24756=CARTESIAN_POINT('',(-1.71469,0.,-2.09988962002998E-16));
#24757=CARTESIAN_POINT('Origin',(2.25,0.7,0.));
#24758=CARTESIAN_POINT('',(-2.25,0.7,-2.75545529808154E-16));
#24759=CARTESIAN_POINT('Origin',(0.,0.7,0.));
#24760=CARTESIAN_POINT('',(-1.71469,0.7,-2.09988962002998E-16));
#24761=CARTESIAN_POINT('Origin',(0.,0.7,0.));
#24762=CARTESIAN_POINT('Origin',(0.,0.65,0.));
#24763=CARTESIAN_POINT('',(-2.35,0.6,-2.87791997799628E-16));
#24764=CARTESIAN_POINT('Origin',(0.,0.6,0.));
#24765=CARTESIAN_POINT('',(-2.3,0.65,-2.81668763803891E-16));
#24766=CARTESIAN_POINT('Origin',(0.,0.,0.));
#24767=CARTESIAN_POINT('',(-2.35,-0.6,-2.87791997799628E-16));
#24768=CARTESIAN_POINT('Origin',(0.,-0.6,0.));
#24769=CARTESIAN_POINT('',(-2.35,0.,-2.87791997799628E-16));
#24770=CARTESIAN_POINT('Origin',(0.,-0.65,0.));
#24771=CARTESIAN_POINT('',(-2.25,-0.7,-2.75545529808154E-16));
#24772=CARTESIAN_POINT('Origin',(0.,-0.7,0.));
#24773=CARTESIAN_POINT('',(-2.3,-0.65,-2.81668763803891E-16));
#24774=CARTESIAN_POINT('Origin',(1.71469,-0.7,0.));
#24775=CARTESIAN_POINT('Origin',(0.,0.,0.));
#24776=CARTESIAN_POINT('',(-1.71469,0.,-2.09988962002998E-16));
#24777=CARTESIAN_POINT('',(0.,0.,0.));
#24778=CARTESIAN_POINT('Origin',(1.675,0.,0.));
#24779=CARTESIAN_POINT('',(1.675,-2.97627328869245E-33,0.3969));
#24780=CARTESIAN_POINT('',(1.675,-2.97627328869245E-33,-0.3969));
#24781=CARTESIAN_POINT('Origin',(1.675,0.,0.));
#24782=CARTESIAN_POINT('Origin',(1.18440385848747,0.,-1.18440385848747));
#24783=CARTESIAN_POINT('',(1.46505453994041,3.1867025333467E-33,-0.903753177034526));
#24784=CARTESIAN_POINT('',(0.903753177034527,-9.13924911073161E-33,-1.46505453994041));
#24785=CARTESIAN_POINT('Origin',(1.18440385848747,0.,-1.18440385848747));
#24786=CARTESIAN_POINT('Origin',(1.02564169428591E-16,0.,-1.675));
#24787=CARTESIAN_POINT('',(0.3969,-2.97627328869246E-33,-1.675));
#24788=CARTESIAN_POINT('',(-0.3969,-2.97627328869245E-33,-1.675));
#24789=CARTESIAN_POINT('Origin',(1.02564169428591E-16,0.,-1.675));
#24790=CARTESIAN_POINT('Origin',(-1.18440385848747,0.,-1.18440385848747));
#24791=CARTESIAN_POINT('',(-0.903753177034526,3.1867025333467E-33,-1.46505453994041));
#24792=CARTESIAN_POINT('',(-1.46505453994041,-9.13924911073161E-33,-0.903753177034527));
#24793=CARTESIAN_POINT('Origin',(-1.18440385848747,0.,-1.18440385848747));
#24794=CARTESIAN_POINT('Origin',(-1.675,0.,-2.05128338857182E-16));
#24795=CARTESIAN_POINT('',(-1.675,-2.97627328869246E-33,-0.3969));
#24796=CARTESIAN_POINT('',(-1.675,-2.97627328869245E-33,0.3969));
#24797=CARTESIAN_POINT('Origin',(-1.675,0.,-2.05128338857182E-16));
#24798=CARTESIAN_POINT('Origin',(-1.18440385848747,0.,1.18440385848747));
#24799=CARTESIAN_POINT('',(-1.46505453994041,6.26819044436628E-33,0.903753177034526));
#24800=CARTESIAN_POINT('',(-0.903753177034527,-1.22207370217512E-32,1.46505453994041));
#24801=CARTESIAN_POINT('Origin',(-1.18440385848747,0.,1.18440385848747));
#24802=CARTESIAN_POINT('Origin',(-3.07692508285772E-16,0.,1.675));
#24803=CARTESIAN_POINT('',(-0.3969,-2.97627328869246E-33,1.675));
#24804=CARTESIAN_POINT('',(0.396899999999999,-2.97627328869245E-33,1.675));
#24805=CARTESIAN_POINT('Origin',(-3.07692508285772E-16,0.,1.675));
#24806=CARTESIAN_POINT('Origin',(1.18440385848747,0.,1.18440385848747));
#24807=CARTESIAN_POINT('',(0.903753177034526,9.34967835538585E-33,1.46505453994041));
#24808=CARTESIAN_POINT('',(1.46505453994041,-1.53022249327708E-32,0.903753177034527));
#24809=CARTESIAN_POINT('Origin',(1.18440385848747,0.,1.18440385848747));
#24810=CARTESIAN_POINT('',(0.,0.,0.));
#24811=CARTESIAN_POINT('Origin',(1.18440385848747,0.,1.18440385848747));
#24812=CARTESIAN_POINT('',(0.846804978391753,-0.07938,1.40825612658882));
#24813=CARTESIAN_POINT('',(1.40825612658882,-0.07938,0.846804978391754));
#24814=CARTESIAN_POINT('Ctrl Pts',(0.846804978391752,-0.0793800000000001,
1.40825612658882));
#24815=CARTESIAN_POINT('Ctrl Pts',(0.854205272175554,-0.123401821157026,
1.40380622184538));
#24816=CARTESIAN_POINT('Ctrl Pts',(0.867957148219441,-0.166543350814306,
1.39550172959303));
#24817=CARTESIAN_POINT('Ctrl Pts',(0.902193646979982,-0.237231147975234,
1.3735491215176));
#24818=CARTESIAN_POINT('Ctrl Pts',(0.920778333482564,-0.266264900654909,
1.36127834356734));
#24819=CARTESIAN_POINT('Ctrl Pts',(0.962485392528369,-0.317195968905306,
1.33211611256184));
#24820=CARTESIAN_POINT('Ctrl Pts',(0.985600426557816,-0.33909093068465,
1.31521005565926));
#24821=CARTESIAN_POINT('Ctrl Pts',(1.03253285680459,-0.373586846396559,
1.27866649102984));
#24822=CARTESIAN_POINT('Ctrl Pts',(1.05871835910697,-0.388086240756494,
1.25722555095714));
#24823=CARTESIAN_POINT('Ctrl Pts',(1.11153475808518,-0.407068917407805,
1.2107812086231));
#24824=CARTESIAN_POINT('Ctrl Pts',(1.13814686046673,-0.411552957311693,
1.18575674747573));
#24825=CARTESIAN_POINT('Ctrl Pts',(1.18575674747573,-0.411552957311693,
1.13814686046673));
#24826=CARTESIAN_POINT('Ctrl Pts',(1.2107812086231,-0.407068917407805,1.11153475808518));
#24827=CARTESIAN_POINT('Ctrl Pts',(1.25722555095713,-0.388086240756494,
1.05871835910697));
#24828=CARTESIAN_POINT('Ctrl Pts',(1.27866649102984,-0.373586846396559,
1.03253285680459));
#24829=CARTESIAN_POINT('Ctrl Pts',(1.31521005565926,-0.33909093068465,0.985600426557816));
#24830=CARTESIAN_POINT('Ctrl Pts',(1.33211611256184,-0.317195968905306,
0.962485392528369));
#24831=CARTESIAN_POINT('Ctrl Pts',(1.36127834356734,-0.266264900654909,
0.920778333482565));
#24832=CARTESIAN_POINT('Ctrl Pts',(1.3735491215176,-0.237231147975234,0.902193646979983));
#24833=CARTESIAN_POINT('Ctrl Pts',(1.39550172959303,-0.166543350814306,
0.867957148219442));
#24834=CARTESIAN_POINT('Ctrl Pts',(1.40380622184538,-0.123401821157026,
0.854205272175555));
#24835=CARTESIAN_POINT('Ctrl Pts',(1.40825612658882,-0.0793800000000001,
0.846804978391753));
#24836=CARTESIAN_POINT('',(0.886256117232623,-0.07938,1.45861320581289));
#24837=CARTESIAN_POINT('Origin',(1.18440385848747,-0.07938,1.18440385848747));
#24838=CARTESIAN_POINT('',(1.45861320581289,-0.07938,0.886256117232624));
#24839=CARTESIAN_POINT('Ctrl Pts',(1.45861320581289,-0.0793800000000001,
0.886256117232623));
#24840=CARTESIAN_POINT('Ctrl Pts',(1.45630208793976,-0.101649918886749,
0.890059788636852));
#24841=CARTESIAN_POINT('Ctrl Pts',(1.45296717977858,-0.123823518623746,
0.895520212222107));
#24842=CARTESIAN_POINT('Ctrl Pts',(1.43904931717599,-0.192480977588836,
0.917859913453975));
#24843=CARTESIAN_POINT('Ctrl Pts',(1.4243271592157,-0.236152929235938,0.940896403863072));
#24844=CARTESIAN_POINT('Ctrl Pts',(1.39055359345152,-0.303141259068212,
0.990027513266106));
#24845=CARTESIAN_POINT('Ctrl Pts',(1.36743459453896,-0.335108247315849,
1.02199477007745));
#24846=CARTESIAN_POINT('Ctrl Pts',(1.32643091652006,-0.373243761060364,
1.07446535104584));
#24847=CARTESIAN_POINT('Ctrl Pts',(1.30441816675528,-0.387888272594439,
1.10126842659597));
#24848=CARTESIAN_POINT('Ctrl Pts',(1.25681160160691,-0.407041111792943,
1.15530234155453));
#24849=CARTESIAN_POINT('Ctrl Pts',(1.23119764287622,-0.411552957311693,
1.18251418313119));
#24850=CARTESIAN_POINT('Ctrl Pts',(1.18251418313119,-0.411552957311693,
1.23119764287622));
#24851=CARTESIAN_POINT('Ctrl Pts',(1.15530234155453,-0.407041111792943,
1.25681160160691));
#24852=CARTESIAN_POINT('Ctrl Pts',(1.10126842659597,-0.387888272594439,
1.30441816675528));
#24853=CARTESIAN_POINT('Ctrl Pts',(1.07446535104584,-0.373243761060364,
1.32643091652006));
#24854=CARTESIAN_POINT('Ctrl Pts',(1.02199477007745,-0.335108247315848,
1.36743459453896));
#24855=CARTESIAN_POINT('Ctrl Pts',(0.990027513266105,-0.303141259068211,
1.39055359345152));
#24856=CARTESIAN_POINT('Ctrl Pts',(0.940896403863071,-0.236152929235937,
1.42432715921571));
#24857=CARTESIAN_POINT('Ctrl Pts',(0.917859913453974,-0.192480977588835,
1.43904931717599));
#24858=CARTESIAN_POINT('Ctrl Pts',(0.895520212222106,-0.123823518623745,
1.45296717977858));
#24859=CARTESIAN_POINT('Ctrl Pts',(0.890059788636851,-0.101649918886749,
1.45630208793976));
#24860=CARTESIAN_POINT('Ctrl Pts',(0.886256117232622,-0.0793800000000001,
1.45861320581289));
#24861=CARTESIAN_POINT('Origin',(1.18440385848747,-0.07938,1.18440385848747));
#24862=CARTESIAN_POINT('Origin',(0.,-0.27783,0.));
#24863=CARTESIAN_POINT('',(0.404717578595295,-0.07938,1.65807299932179));
#24864=CARTESIAN_POINT('Origin',(0.,-0.07938,0.));
#24865=CARTESIAN_POINT('',(-0.404717578595296,-0.07938,1.65807299932179));
#24866=CARTESIAN_POINT('Ctrl Pts',(0.404717578595296,-0.0793800000000001,
1.65807299932179));
#24867=CARTESIAN_POINT('Ctrl Pts',(0.400393769631747,-0.101649918886749,
1.65912839404491));
#24868=CARTESIAN_POINT('Ctrl Pts',(0.394174530911058,-0.123823518623745,
1.66063136041479));
#24869=CARTESIAN_POINT('Ctrl Pts',(0.368536561654407,-0.192480977588835,
1.66658649961961));
#24870=CARTESIAN_POINT('Ctrl Pts',(0.341837165343982,-0.236152929235937,
1.67246562047521));
#24871=CARTESIAN_POINT('Ctrl Pts',(0.283214707341173,-0.303141259068211,
1.68332504372461));
#24872=CARTESIAN_POINT('Ctrl Pts',(0.244262842368623,-0.335108247315849,
1.68958170688653));
#24873=CARTESIAN_POINT('Ctrl Pts',(0.178166559972324,-0.373243761060364,
1.69769003172132));
#24874=CARTESIAN_POINT('Ctrl Pts',(0.143648558862931,-0.387888272594439,
1.70107730356824));
#24875=CARTESIAN_POINT('Ctrl Pts',(0.0717778861362652,-0.407041111792943,
1.70562212620408));
#24876=CARTESIAN_POINT('Ctrl Pts',(0.0344244045173309,-0.411552957311693,
1.706752));
#24877=CARTESIAN_POINT('Ctrl Pts',(-0.0344244045173315,-0.411552957311693,
1.706752));
#24878=CARTESIAN_POINT('Ctrl Pts',(-0.0717778861362658,-0.407041111792943,
1.70562212620408));
#24879=CARTESIAN_POINT('Ctrl Pts',(-0.143648558862932,-0.387888272594439,
1.70107730356824));
#24880=CARTESIAN_POINT('Ctrl Pts',(-0.178166559972325,-0.373243761060364,
1.69769003172132));
#24881=CARTESIAN_POINT('Ctrl Pts',(-0.244262842368624,-0.335108247315849,
1.68958170688653));
#24882=CARTESIAN_POINT('Ctrl Pts',(-0.283214707341173,-0.303141259068212,
1.68332504372461));
#24883=CARTESIAN_POINT('Ctrl Pts',(-0.341837165343982,-0.236152929235937,
1.67246562047521));
#24884=CARTESIAN_POINT('Ctrl Pts',(-0.368536561654408,-0.192480977588835,
1.66658649961961));
#24885=CARTESIAN_POINT('Ctrl Pts',(-0.394174530911059,-0.123823518623745,
1.66063136041479));
#24886=CARTESIAN_POINT('Ctrl Pts',(-0.400393769631748,-0.101649918886749,
1.65912839404491));
#24887=CARTESIAN_POINT('Ctrl Pts',(-0.404717578595297,-0.0793800000000001,
1.65807299932179));
#24888=CARTESIAN_POINT('',(-0.886256117232624,-0.07938,1.45861320581289));
#24889=CARTESIAN_POINT('Origin',(0.,-0.07938,0.));
#24890=CARTESIAN_POINT('',(-1.45861320581289,-0.07938,0.886256117232623));
#24891=CARTESIAN_POINT('Ctrl Pts',(-0.886256117232623,-0.0793800000000001,
1.45861320581289));
#24892=CARTESIAN_POINT('Ctrl Pts',(-0.890059788636852,-0.101649918886749,
1.45630208793976));
#24893=CARTESIAN_POINT('Ctrl Pts',(-0.895520212222106,-0.123823518623745,
1.45296717977858));
#24894=CARTESIAN_POINT('Ctrl Pts',(-0.917859913453974,-0.192480977588835,
1.43904931717599));
#24895=CARTESIAN_POINT('Ctrl Pts',(-0.940896403863071,-0.236152929235937,
1.4243271592157));
#24896=CARTESIAN_POINT('Ctrl Pts',(-0.990027513266105,-0.303141259068211,
1.39055359345152));
#24897=CARTESIAN_POINT('Ctrl Pts',(-1.02199477007745,-0.335108247315848,
1.36743459453896));
#24898=CARTESIAN_POINT('Ctrl Pts',(-1.07446535104584,-0.373243761060364,
1.32643091652006));
#24899=CARTESIAN_POINT('Ctrl Pts',(-1.10126842659597,-0.387888272594439,
1.30441816675528));
#24900=CARTESIAN_POINT('Ctrl Pts',(-1.15530234155453,-0.407041111792943,
1.25681160160691));
#24901=CARTESIAN_POINT('Ctrl Pts',(-1.18251418313119,-0.411552957311693,
1.23119764287622));
#24902=CARTESIAN_POINT('Ctrl Pts',(-1.23119764287622,-0.411552957311693,
1.18251418313119));
#24903=CARTESIAN_POINT('Ctrl Pts',(-1.25681160160691,-0.407041111792943,
1.15530234155453));
#24904=CARTESIAN_POINT('Ctrl Pts',(-1.30441816675528,-0.387888272594439,
1.10126842659597));
#24905=CARTESIAN_POINT('Ctrl Pts',(-1.32643091652006,-0.373243761060365,
1.07446535104584));
#24906=CARTESIAN_POINT('Ctrl Pts',(-1.36743459453896,-0.335108247315849,
1.02199477007745));
#24907=CARTESIAN_POINT('Ctrl Pts',(-1.39055359345152,-0.303141259068212,
0.990027513266106));
#24908=CARTESIAN_POINT('Ctrl Pts',(-1.4243271592157,-0.236152929235938,
0.940896403863071));
#24909=CARTESIAN_POINT('Ctrl Pts',(-1.43904931717599,-0.192480977588836,
0.917859913453974));
#24910=CARTESIAN_POINT('Ctrl Pts',(-1.45296717977858,-0.123823518623746,
0.895520212222106));
#24911=CARTESIAN_POINT('Ctrl Pts',(-1.45630208793976,-0.101649918886749,
0.890059788636852));
#24912=CARTESIAN_POINT('Ctrl Pts',(-1.45861320581289,-0.0793800000000001,
0.886256117232623));
#24913=CARTESIAN_POINT('',(-1.65807299932179,-0.07938,0.404717578595295));
#24914=CARTESIAN_POINT('Origin',(0.,-0.07938,0.));
#24915=CARTESIAN_POINT('',(-1.706752,-0.411552957311693,2.08591827245526E-16));
#24916=CARTESIAN_POINT('Ctrl Pts',(-1.65807299932179,-0.0793800000000001,
0.404717578595296));
#24917=CARTESIAN_POINT('Ctrl Pts',(-1.65912839404491,-0.101649918886749,
0.400393769631747));
#24918=CARTESIAN_POINT('Ctrl Pts',(-1.66063136041479,-0.123823518623745,
0.394174530911058));
#24919=CARTESIAN_POINT('Ctrl Pts',(-1.66658649961961,-0.192480977588835,
0.368536561654407));
#24920=CARTESIAN_POINT('Ctrl Pts',(-1.67246562047521,-0.236152929235937,
0.341837165343982));
#24921=CARTESIAN_POINT('Ctrl Pts',(-1.68332504372461,-0.303141259068211,
0.283214707341173));
#24922=CARTESIAN_POINT('Ctrl Pts',(-1.68958170688653,-0.335108247315848,
0.244262842368623));
#24923=CARTESIAN_POINT('Ctrl Pts',(-1.69769003172132,-0.373243761060364,
0.178166559972324));
#24924=CARTESIAN_POINT('Ctrl Pts',(-1.70107730356824,-0.387888272594439,
0.143648558862931));
#24925=CARTESIAN_POINT('Ctrl Pts',(-1.70562212620408,-0.407041111792943,
0.0717778861362656));
#24926=CARTESIAN_POINT('Ctrl Pts',(-1.706752,-0.411552957311693,0.0344244045173313));
#24927=CARTESIAN_POINT('Ctrl Pts',(-1.706752,-0.411552957311693,2.08166817117217E-16));
#24928=CARTESIAN_POINT('',(-1.706752,-0.47628,2.09016837373834E-16));
#24929=CARTESIAN_POINT('',(-1.706752,-0.27783,2.09016837373834E-16));
#24930=CARTESIAN_POINT('Origin',(0.,-0.47628,0.));
#24931=CARTESIAN_POINT('',(-1.65807299932179,-0.07938,-0.404717578595296));
#24932=CARTESIAN_POINT('Ctrl Pts',(-1.706752,-0.411552957311693,2.0122792321331E-16));
#24933=CARTESIAN_POINT('Ctrl Pts',(-1.706752,-0.411552957311693,-0.0344244045173309));
#24934=CARTESIAN_POINT('Ctrl Pts',(-1.70562212620408,-0.407041111792943,
-0.0717778861362652));
#24935=CARTESIAN_POINT('Ctrl Pts',(-1.70107730356824,-0.387888272594439,
-0.143648558862931));
#24936=CARTESIAN_POINT('Ctrl Pts',(-1.69769003172132,-0.373243761060365,
-0.178166559972324));
#24937=CARTESIAN_POINT('Ctrl Pts',(-1.68958170688653,-0.335108247315849,
-0.244262842368623));
#24938=CARTESIAN_POINT('Ctrl Pts',(-1.68332504372461,-0.303141259068212,
-0.283214707341173));
#24939=CARTESIAN_POINT('Ctrl Pts',(-1.67246562047521,-0.236152929235938,
-0.341837165343982));
#24940=CARTESIAN_POINT('Ctrl Pts',(-1.66658649961961,-0.192480977588836,
-0.368536561654407));
#24941=CARTESIAN_POINT('Ctrl Pts',(-1.66063136041479,-0.123823518623745,
-0.394174530911059));
#24942=CARTESIAN_POINT('Ctrl Pts',(-1.65912839404491,-0.101649918886749,
-0.400393769631748));
#24943=CARTESIAN_POINT('Ctrl Pts',(-1.65807299932179,-0.0793800000000001,
-0.404717578595296));
#24944=CARTESIAN_POINT('',(-1.45861320581289,-0.07938,-0.886256117232623));
#24945=CARTESIAN_POINT('Origin',(0.,-0.07938,0.));
#24946=CARTESIAN_POINT('',(-0.886256117232623,-0.07938,-1.45861320581289));
#24947=CARTESIAN_POINT('Ctrl Pts',(-1.45861320581289,-0.0793800000000001,
-0.886256117232623));
#24948=CARTESIAN_POINT('Ctrl Pts',(-1.45630208793976,-0.101649918886749,
-0.890059788636852));
#24949=CARTESIAN_POINT('Ctrl Pts',(-1.45296717977858,-0.123823518623745,
-0.895520212222106));
#24950=CARTESIAN_POINT('Ctrl Pts',(-1.43904931717599,-0.192480977588835,
-0.917859913453974));
#24951=CARTESIAN_POINT('Ctrl Pts',(-1.4243271592157,-0.236152929235937,
-0.940896403863072));
#24952=CARTESIAN_POINT('Ctrl Pts',(-1.39055359345152,-0.303141259068212,
-0.990027513266106));
#24953=CARTESIAN_POINT('Ctrl Pts',(-1.36743459453896,-0.335108247315849,
-1.02199477007745));
#24954=CARTESIAN_POINT('Ctrl Pts',(-1.32643091652006,-0.373243761060364,
-1.07446535104584));
#24955=CARTESIAN_POINT('Ctrl Pts',(-1.30441816675528,-0.387888272594439,
-1.10126842659597));
#24956=CARTESIAN_POINT('Ctrl Pts',(-1.25681160160691,-0.407041111792943,
-1.15530234155453));
#24957=CARTESIAN_POINT('Ctrl Pts',(-1.23119764287622,-0.411552957311693,
-1.18251418313119));
#24958=CARTESIAN_POINT('Ctrl Pts',(-1.18251418313119,-0.411552957311693,
-1.23119764287622));
#24959=CARTESIAN_POINT('Ctrl Pts',(-1.15530234155453,-0.407041111792943,
-1.25681160160691));
#24960=CARTESIAN_POINT('Ctrl Pts',(-1.10126842659597,-0.387888272594439,
-1.30441816675528));
#24961=CARTESIAN_POINT('Ctrl Pts',(-1.07446535104584,-0.373243761060364,
-1.32643091652006));
#24962=CARTESIAN_POINT('Ctrl Pts',(-1.02199477007745,-0.335108247315848,
-1.36743459453896));
#24963=CARTESIAN_POINT('Ctrl Pts',(-0.990027513266105,-0.303141259068211,
-1.39055359345152));
#24964=CARTESIAN_POINT('Ctrl Pts',(-0.940896403863071,-0.236152929235936,
-1.42432715921571));
#24965=CARTESIAN_POINT('Ctrl Pts',(-0.917859913453974,-0.192480977588835,
-1.43904931717599));
#24966=CARTESIAN_POINT('Ctrl Pts',(-0.895520212222106,-0.123823518623745,
-1.45296717977858));
#24967=CARTESIAN_POINT('Ctrl Pts',(-0.890059788636851,-0.101649918886749,
-1.45630208793976));
#24968=CARTESIAN_POINT('Ctrl Pts',(-0.886256117232623,-0.0793800000000001,
-1.45861320581289));
#24969=CARTESIAN_POINT('',(-0.404717578595295,-0.07938,-1.65807299932179));
#24970=CARTESIAN_POINT('Origin',(0.,-0.07938,0.));
#24971=CARTESIAN_POINT('',(0.404717578595296,-0.07938,-1.65807299932179));
#24972=CARTESIAN_POINT('Ctrl Pts',(-0.404717578595296,-0.0793800000000001,
-1.65807299932179));
#24973=CARTESIAN_POINT('Ctrl Pts',(-0.400393769631747,-0.101649918886749,
-1.65912839404491));
#24974=CARTESIAN_POINT('Ctrl Pts',(-0.394174530911058,-0.123823518623746,
-1.66063136041479));
#24975=CARTESIAN_POINT('Ctrl Pts',(-0.368536561654407,-0.192480977588836,
-1.66658649961961));
#24976=CARTESIAN_POINT('Ctrl Pts',(-0.341837165343982,-0.236152929235938,
-1.67246562047521));
#24977=CARTESIAN_POINT('Ctrl Pts',(-0.283214707341173,-0.303141259068212,
-1.68332504372461));
#24978=CARTESIAN_POINT('Ctrl Pts',(-0.244262842368623,-0.335108247315849,
-1.68958170688653));
#24979=CARTESIAN_POINT('Ctrl Pts',(-0.178166559972324,-0.373243761060364,
-1.69769003172132));
#24980=CARTESIAN_POINT('Ctrl Pts',(-0.143648558862931,-0.387888272594439,
-1.70107730356824));
#24981=CARTESIAN_POINT('Ctrl Pts',(-0.0717778861362653,-0.407041111792943,
-1.70562212620408));
#24982=CARTESIAN_POINT('Ctrl Pts',(-0.034424404517331,-0.411552957311693,
-1.706752));
#24983=CARTESIAN_POINT('Ctrl Pts',(0.0344244045173312,-0.411552957311693,
-1.706752));
#24984=CARTESIAN_POINT('Ctrl Pts',(0.0717778861362655,-0.407041111792943,
-1.70562212620408));
#24985=CARTESIAN_POINT('Ctrl Pts',(0.143648558862931,-0.387888272594439,
-1.70107730356824));
#24986=CARTESIAN_POINT('Ctrl Pts',(0.178166559972324,-0.373243761060364,
-1.69769003172132));
#24987=CARTESIAN_POINT('Ctrl Pts',(0.244262842368623,-0.335108247315849,
-1.68958170688653));
#24988=CARTESIAN_POINT('Ctrl Pts',(0.283214707341173,-0.303141259068212,
-1.68332504372461));
#24989=CARTESIAN_POINT('Ctrl Pts',(0.341837165343982,-0.236152929235937,
-1.67246562047521));
#24990=CARTESIAN_POINT('Ctrl Pts',(0.368536561654407,-0.192480977588835,
-1.66658649961961));
#24991=CARTESIAN_POINT('Ctrl Pts',(0.394174530911059,-0.123823518623745,
-1.66063136041479));
#24992=CARTESIAN_POINT('Ctrl Pts',(0.400393769631748,-0.101649918886749,
-1.65912839404491));
#24993=CARTESIAN_POINT('Ctrl Pts',(0.404717578595296,-0.0793800000000001,
-1.65807299932179));
#24994=CARTESIAN_POINT('',(0.886256117232623,-0.07938,-1.45861320581289));
#24995=CARTESIAN_POINT('Origin',(0.,-0.07938,0.));
#24996=CARTESIAN_POINT('',(1.45861320581289,-0.07938,-0.886256117232623));
#24997=CARTESIAN_POINT('Ctrl Pts',(0.886256117232623,-0.0793800000000001,
-1.45861320581289));
#24998=CARTESIAN_POINT('Ctrl Pts',(0.890059788636852,-0.101649918886749,
-1.45630208793976));
#24999=CARTESIAN_POINT('Ctrl Pts',(0.895520212222106,-0.123823518623745,
-1.45296717977858));
#25000=CARTESIAN_POINT('Ctrl Pts',(0.917859913453974,-0.192480977588835,
-1.43904931717599));
#25001=CARTESIAN_POINT('Ctrl Pts',(0.940896403863072,-0.236152929235937,
-1.4243271592157));
#25002=CARTESIAN_POINT('Ctrl Pts',(0.990027513266106,-0.303141259068211,
-1.39055359345152));
#25003=CARTESIAN_POINT('Ctrl Pts',(1.02199477007745,-0.335108247315849,
-1.36743459453896));
#25004=CARTESIAN_POINT('Ctrl Pts',(1.07446535104584,-0.373243761060364,
-1.32643091652006));
#25005=CARTESIAN_POINT('Ctrl Pts',(1.10126842659597,-0.387888272594439,
-1.30441816675528));
#25006=CARTESIAN_POINT('Ctrl Pts',(1.15530234155453,-0.407041111792943,
-1.25681160160691));
#25007=CARTESIAN_POINT('Ctrl Pts',(1.18251418313119,-0.411552957311693,
-1.23119764287622));
#25008=CARTESIAN_POINT('Ctrl Pts',(1.23119764287622,-0.411552957311693,
-1.18251418313119));
#25009=CARTESIAN_POINT('Ctrl Pts',(1.25681160160691,-0.407041111792943,
-1.15530234155453));
#25010=CARTESIAN_POINT('Ctrl Pts',(1.30441816675528,-0.387888272594439,
-1.10126842659597));
#25011=CARTESIAN_POINT('Ctrl Pts',(1.32643091652006,-0.373243761060364,
-1.07446535104584));
#25012=CARTESIAN_POINT('Ctrl Pts',(1.36743459453896,-0.335108247315849,
-1.02199477007745));
#25013=CARTESIAN_POINT('Ctrl Pts',(1.39055359345152,-0.303141259068212,
-0.990027513266105));
#25014=CARTESIAN_POINT('Ctrl Pts',(1.4243271592157,-0.236152929235937,-0.940896403863071));
#25015=CARTESIAN_POINT('Ctrl Pts',(1.43904931717599,-0.192480977588835,
-0.917859913453974));
#25016=CARTESIAN_POINT('Ctrl Pts',(1.45296717977858,-0.123823518623745,
-0.895520212222106));
#25017=CARTESIAN_POINT('Ctrl Pts',(1.45630208793976,-0.101649918886749,
-0.890059788636852));
#25018=CARTESIAN_POINT('Ctrl Pts',(1.45861320581289,-0.0793800000000001,
-0.886256117232623));
#25019=CARTESIAN_POINT('',(1.65807299932179,-0.07938,-0.404717578595296));
#25020=CARTESIAN_POINT('Origin',(0.,-0.07938,0.));
#25021=CARTESIAN_POINT('',(1.65807299932179,-0.07938,0.404717578595296));
#25022=CARTESIAN_POINT('Ctrl Pts',(1.65807299932179,-0.0793800000000001,
-0.404717578595296));
#25023=CARTESIAN_POINT('Ctrl Pts',(1.65912839404491,-0.101649918886749,
-0.400393769631747));
#25024=CARTESIAN_POINT('Ctrl Pts',(1.66063136041479,-0.123823518623745,
-0.394174530911058));
#25025=CARTESIAN_POINT('Ctrl Pts',(1.66658649961961,-0.192480977588835,
-0.368536561654407));
#25026=CARTESIAN_POINT('Ctrl Pts',(1.67246562047521,-0.236152929235937,
-0.341837165343982));
#25027=CARTESIAN_POINT('Ctrl Pts',(1.68332504372461,-0.303141259068212,
-0.283214707341173));
#25028=CARTESIAN_POINT('Ctrl Pts',(1.68958170688653,-0.335108247315849,
-0.244262842368623));
#25029=CARTESIAN_POINT('Ctrl Pts',(1.69769003172132,-0.373243761060364,
-0.178166559972324));
#25030=CARTESIAN_POINT('Ctrl Pts',(1.70107730356824,-0.387888272594439,
-0.143648558862931));
#25031=CARTESIAN_POINT('Ctrl Pts',(1.70562212620408,-0.407041111792943,
-0.0717778861362655));
#25032=CARTESIAN_POINT('Ctrl Pts',(1.706752,-0.411552957311693,-0.0344244045173312));
#25033=CARTESIAN_POINT('Ctrl Pts',(1.706752,-0.411552957311693,0.0344244045173312));
#25034=CARTESIAN_POINT('Ctrl Pts',(1.70562212620408,-0.407041111792943,
0.0717778861362655));
#25035=CARTESIAN_POINT('Ctrl Pts',(1.70107730356824,-0.387888272594439,
0.143648558862931));
#25036=CARTESIAN_POINT('Ctrl Pts',(1.69769003172132,-0.373243761060364,
0.178166559972324));
#25037=CARTESIAN_POINT('Ctrl Pts',(1.68958170688653,-0.335108247315849,
0.244262842368623));
#25038=CARTESIAN_POINT('Ctrl Pts',(1.68332504372461,-0.303141259068212,
0.283214707341173));
#25039=CARTESIAN_POINT('Ctrl Pts',(1.67246562047521,-0.236152929235937,
0.341837165343982));
#25040=CARTESIAN_POINT('Ctrl Pts',(1.66658649961961,-0.192480977588835,
0.368536561654407));
#25041=CARTESIAN_POINT('Ctrl Pts',(1.66063136041479,-0.123823518623745,
0.394174530911058));
#25042=CARTESIAN_POINT('Ctrl Pts',(1.65912839404491,-0.101649918886749,
0.400393769631747));
#25043=CARTESIAN_POINT('Ctrl Pts',(1.65807299932179,-0.0793800000000001,
0.404717578595296));
#25044=CARTESIAN_POINT('Origin',(0.,-0.07938,0.));
#25045=CARTESIAN_POINT('Origin',(0.,-0.07938,0.));
#25046=CARTESIAN_POINT('',(0.397005914195118,-0.07938,1.59456899932179));
#25047=CARTESIAN_POINT('Origin',(0.,-0.07938,0.));
#25048=CARTESIAN_POINT('Origin',(-3.33066907387547E-16,-0.07938,1.675));
#25049=CARTESIAN_POINT('Origin',(-3.33066907387547E-16,0.,1.675));
#25050=CARTESIAN_POINT('',(-0.397005914195118,-0.07938,1.59456899932179));
#25051=CARTESIAN_POINT('Ctrl Pts',(-0.397005914195119,-0.0793800000000001,
1.59456899932179));
#25052=CARTESIAN_POINT('Ctrl Pts',(-0.3886265584581,-0.123401821157026,
1.59665523941937));
#25053=CARTESIAN_POINT('Ctrl Pts',(-0.373030350867485,-0.166543350814306,
1.60050712143809));
#25054=CARTESIAN_POINT('Ctrl Pts',(-0.333298652394954,-0.237231147975234,
1.60919314384089));
#25055=CARTESIAN_POINT('Ctrl Pts',(-0.311480544243687,-0.266264900654909,
1.61365775139403));
#25056=CARTESIAN_POINT('Ctrl Pts',(-0.261368388670537,-0.317195968905306,
1.62252828437015));
#25057=CARTESIAN_POINT('Ctrl Pts',(-0.233069203882014,-0.33909093068465,
1.62691869420078));
#25058=CARTESIAN_POINT('Ctrl Pts',(-0.174042761838764,-0.373586846396559,
1.63426473152765));
#25059=CARTESIAN_POINT('Ctrl Pts',(-0.14036578147155,-0.388086240756494,
1.63761964365402));
#25060=CARTESIAN_POINT('Ctrl Pts',(-0.0701778381840615,-0.407068917407805,
1.64212536811722));
#25061=CARTESIAN_POINT('Ctrl Pts',(-0.0336652739555918,-0.411552957311693,
1.643248));
#25062=CARTESIAN_POINT('Ctrl Pts',(0.0336652739555913,-0.411552957311693,
1.643248));
#25063=CARTESIAN_POINT('Ctrl Pts',(0.070177838184061,-0.407068917407805,
1.64212536811722));
#25064=CARTESIAN_POINT('Ctrl Pts',(0.140365781471549,-0.388086240756494,
1.63761964365402));
#25065=CARTESIAN_POINT('Ctrl Pts',(0.174042761838763,-0.373586846396559,
1.63426473152765));
#25066=CARTESIAN_POINT('Ctrl Pts',(0.233069203882014,-0.33909093068465,
1.62691869420078));
#25067=CARTESIAN_POINT('Ctrl Pts',(0.261368388670536,-0.317195968905306,
1.62252828437015));
#25068=CARTESIAN_POINT('Ctrl Pts',(0.311480544243686,-0.266264900654908,
1.61365775139403));
#25069=CARTESIAN_POINT('Ctrl Pts',(0.333298652394954,-0.237231147975234,
1.60919314384089));
#25070=CARTESIAN_POINT('Ctrl Pts',(0.373030350867484,-0.166543350814306,
1.60050712143809));
#25071=CARTESIAN_POINT('Ctrl Pts',(0.388626558458099,-0.123401821157026,
1.59665523941937));
#25072=CARTESIAN_POINT('Ctrl Pts',(0.397005914195118,-0.07938,1.59456899932179));
#25073=CARTESIAN_POINT('Origin',(-3.33066907387547E-16,-0.07938,1.675));
#25074=CARTESIAN_POINT('Origin',(0.,-0.07938,0.));
#25075=CARTESIAN_POINT('',(-0.846804978391754,-0.07938,1.40825612658882));
#25076=CARTESIAN_POINT('Origin',(0.,-0.07938,0.));
#25077=CARTESIAN_POINT('Origin',(-1.18440385848747,-0.07938,1.18440385848747));
#25078=CARTESIAN_POINT('Origin',(-1.18440385848747,0.,1.18440385848747));
#25079=CARTESIAN_POINT('',(-1.40825612658882,-0.07938,0.846804978391753));
#25080=CARTESIAN_POINT('Ctrl Pts',(-1.40825612658882,-0.0793800000000001,
0.846804978391753));
#25081=CARTESIAN_POINT('Ctrl Pts',(-1.40380622184538,-0.123401821157026,
0.854205272175555));
#25082=CARTESIAN_POINT('Ctrl Pts',(-1.39550172959303,-0.166543350814306,
0.867957148219442));
#25083=CARTESIAN_POINT('Ctrl Pts',(-1.3735491215176,-0.237231147975235,
0.902193646979983));
#25084=CARTESIAN_POINT('Ctrl Pts',(-1.36127834356734,-0.266264900654909,
0.920778333482565));
#25085=CARTESIAN_POINT('Ctrl Pts',(-1.33211611256184,-0.317195968905306,
0.962485392528369));
#25086=CARTESIAN_POINT('Ctrl Pts',(-1.31521005565926,-0.339090930684651,
0.985600426557816));
#25087=CARTESIAN_POINT('Ctrl Pts',(-1.27866649102984,-0.373586846396559,
1.03253285680459));
#25088=CARTESIAN_POINT('Ctrl Pts',(-1.25722555095714,-0.388086240756494,
1.05871835910697));
#25089=CARTESIAN_POINT('Ctrl Pts',(-1.2107812086231,-0.407068917407805,
1.11153475808518));
#25090=CARTESIAN_POINT('Ctrl Pts',(-1.18575674747573,-0.411552957311693,
1.13814686046673));
#25091=CARTESIAN_POINT('Ctrl Pts',(-1.13814686046673,-0.411552957311693,
1.18575674747573));
#25092=CARTESIAN_POINT('Ctrl Pts',(-1.11153475808518,-0.407068917407805,
1.2107812086231));
#25093=CARTESIAN_POINT('Ctrl Pts',(-1.05871835910697,-0.388086240756494,
1.25722555095714));
#25094=CARTESIAN_POINT('Ctrl Pts',(-1.03253285680459,-0.373586846396559,
1.27866649102984));
#25095=CARTESIAN_POINT('Ctrl Pts',(-0.985600426557816,-0.33909093068465,
1.31521005565926));
#25096=CARTESIAN_POINT('Ctrl Pts',(-0.962485392528369,-0.317195968905306,
1.33211611256184));
#25097=CARTESIAN_POINT('Ctrl Pts',(-0.920778333482565,-0.266264900654908,
1.36127834356734));
#25098=CARTESIAN_POINT('Ctrl Pts',(-0.902193646979983,-0.237231147975234,
1.3735491215176));
#25099=CARTESIAN_POINT('Ctrl Pts',(-0.867957148219442,-0.166543350814306,
1.39550172959303));
#25100=CARTESIAN_POINT('Ctrl Pts',(-0.854205272175555,-0.123401821157026,
1.40380622184538));
#25101=CARTESIAN_POINT('Ctrl Pts',(-0.846804978391753,-0.0793800000000001,
1.40825612658882));
#25102=CARTESIAN_POINT('Origin',(-1.18440385848747,-0.07938,1.18440385848747));
#25103=CARTESIAN_POINT('Origin',(0.,-0.07938,0.));
#25104=CARTESIAN_POINT('',(-1.59456899932179,-0.07938,0.397005914195118));
#25105=CARTESIAN_POINT('Origin',(0.,-0.07938,0.));
#25106=CARTESIAN_POINT('Origin',(-1.675,-0.07938,-2.22044604925031E-16));
#25107=CARTESIAN_POINT('Origin',(-1.675,0.,-2.22044604925031E-16));
#25108=CARTESIAN_POINT('',(-1.59456899932179,-0.07938,-0.397005914195118));
#25109=CARTESIAN_POINT('',(-1.643248,-0.411552957311693,3.47540551556327E-18));
#25110=CARTESIAN_POINT('Ctrl Pts',(-1.59456899932179,-0.0793800000000001,
-0.397005914195119));
#25111=CARTESIAN_POINT('Ctrl Pts',(-1.59665523941937,-0.123401821157026,
-0.388626558458099));
#25112=CARTESIAN_POINT('Ctrl Pts',(-1.60050712143809,-0.166543350814306,
-0.373030350867485));
#25113=CARTESIAN_POINT('Ctrl Pts',(-1.60919314384089,-0.237231147975234,
-0.333298652394954));
#25114=CARTESIAN_POINT('Ctrl Pts',(-1.61365775139403,-0.266264900654909,
-0.311480544243686));
#25115=CARTESIAN_POINT('Ctrl Pts',(-1.62252828437015,-0.317195968905306,
-0.261368388670537));
#25116=CARTESIAN_POINT('Ctrl Pts',(-1.62691869420078,-0.33909093068465,
-0.233069203882014));
#25117=CARTESIAN_POINT('Ctrl Pts',(-1.63426473152765,-0.373586846396559,
-0.174042761838764));
#25118=CARTESIAN_POINT('Ctrl Pts',(-1.63761964365402,-0.388086240756494,
-0.140365781471549));
#25119=CARTESIAN_POINT('Ctrl Pts',(-1.64212536811722,-0.407068917407805,
-0.0701778381840614));
#25120=CARTESIAN_POINT('Ctrl Pts',(-1.643248,-0.411552957311693,-0.0336652739555917));
#25121=CARTESIAN_POINT('Ctrl Pts',(-1.643248,-0.411552957311693,-2.0122792321331E-16));
#25122=CARTESIAN_POINT('Origin',(-1.675,-0.07938,-2.22044604925031E-16));
#25123=CARTESIAN_POINT('Ctrl Pts',(-1.643248,-0.411552957311693,-1.94289029309402E-16));
#25124=CARTESIAN_POINT('Ctrl Pts',(-1.643248,-0.411552957311693,0.0336652739555913));
#25125=CARTESIAN_POINT('Ctrl Pts',(-1.64212536811722,-0.407068917407805,
0.0701778381840609));
#25126=CARTESIAN_POINT('Ctrl Pts',(-1.63761964365402,-0.388086240756494,
0.140365781471549));
#25127=CARTESIAN_POINT('Ctrl Pts',(-1.63426473152765,-0.373586846396559,
0.174042761838763));
#25128=CARTESIAN_POINT('Ctrl Pts',(-1.62691869420078,-0.33909093068465,
0.233069203882014));
#25129=CARTESIAN_POINT('Ctrl Pts',(-1.62252828437015,-0.317195968905306,
0.261368388670536));
#25130=CARTESIAN_POINT('Ctrl Pts',(-1.61365775139403,-0.266264900654909,
0.311480544243686));
#25131=CARTESIAN_POINT('Ctrl Pts',(-1.60919314384089,-0.237231147975235,
0.333298652394954));
#25132=CARTESIAN_POINT('Ctrl Pts',(-1.60050712143809,-0.166543350814306,
0.373030350867484));
#25133=CARTESIAN_POINT('Ctrl Pts',(-1.59665523941937,-0.123401821157026,
0.388626558458099));
#25134=CARTESIAN_POINT('Ctrl Pts',(-1.59456899932179,-0.0793800000000001,
0.397005914195118));
#25135=CARTESIAN_POINT('Origin',(0.,-0.07938,0.));
#25136=CARTESIAN_POINT('',(-1.40825612658882,-0.07938,-0.846804978391753));
#25137=CARTESIAN_POINT('Origin',(0.,-0.07938,0.));
#25138=CARTESIAN_POINT('Origin',(-1.18440385848747,-0.07938,-1.18440385848747));
#25139=CARTESIAN_POINT('Origin',(-1.18440385848747,0.,-1.18440385848747));
#25140=CARTESIAN_POINT('',(-0.846804978391753,-0.07938,-1.40825612658882));
#25141=CARTESIAN_POINT('Ctrl Pts',(-0.846804978391753,-0.0793800000000001,
-1.40825612658882));
#25142=CARTESIAN_POINT('Ctrl Pts',(-0.854205272175555,-0.123401821157026,
-1.40380622184538));
#25143=CARTESIAN_POINT('Ctrl Pts',(-0.867957148219442,-0.166543350814306,
-1.39550172959303));
#25144=CARTESIAN_POINT('Ctrl Pts',(-0.902193646979982,-0.237231147975234,
-1.3735491215176));
#25145=CARTESIAN_POINT('Ctrl Pts',(-0.920778333482564,-0.266264900654908,
-1.36127834356734));
#25146=CARTESIAN_POINT('Ctrl Pts',(-0.962485392528368,-0.317195968905306,
-1.33211611256184));
#25147=CARTESIAN_POINT('Ctrl Pts',(-0.985600426557816,-0.33909093068465,
-1.31521005565926));
#25148=CARTESIAN_POINT('Ctrl Pts',(-1.03253285680459,-0.373586846396559,
-1.27866649102984));
#25149=CARTESIAN_POINT('Ctrl Pts',(-1.05871835910697,-0.388086240756494,
-1.25722555095714));
#25150=CARTESIAN_POINT('Ctrl Pts',(-1.11153475808518,-0.407068917407805,
-1.2107812086231));
#25151=CARTESIAN_POINT('Ctrl Pts',(-1.13814686046673,-0.411552957311693,
-1.18575674747573));
#25152=CARTESIAN_POINT('Ctrl Pts',(-1.18575674747573,-0.411552957311693,
-1.13814686046673));
#25153=CARTESIAN_POINT('Ctrl Pts',(-1.2107812086231,-0.407068917407805,
-1.11153475808518));
#25154=CARTESIAN_POINT('Ctrl Pts',(-1.25722555095714,-0.388086240756494,
-1.05871835910697));
#25155=CARTESIAN_POINT('Ctrl Pts',(-1.27866649102984,-0.373586846396559,
-1.03253285680459));
#25156=CARTESIAN_POINT('Ctrl Pts',(-1.31521005565926,-0.33909093068465,
-0.985600426557816));
#25157=CARTESIAN_POINT('Ctrl Pts',(-1.33211611256184,-0.317195968905306,
-0.962485392528369));
#25158=CARTESIAN_POINT('Ctrl Pts',(-1.36127834356734,-0.266264900654909,
-0.920778333482565));
#25159=CARTESIAN_POINT('Ctrl Pts',(-1.3735491215176,-0.237231147975234,
-0.902193646979983));
#25160=CARTESIAN_POINT('Ctrl Pts',(-1.39550172959303,-0.166543350814306,
-0.867957148219442));
#25161=CARTESIAN_POINT('Ctrl Pts',(-1.40380622184538,-0.123401821157026,
-0.854205272175555));
#25162=CARTESIAN_POINT('Ctrl Pts',(-1.40825612658882,-0.07938,-0.846804978391753));
#25163=CARTESIAN_POINT('Origin',(-1.18440385848747,-0.07938,-1.18440385848747));
#25164=CARTESIAN_POINT('Origin',(0.,-0.07938,0.));
#25165=CARTESIAN_POINT('',(-0.397005914195118,-0.07938,-1.59456899932179));
#25166=CARTESIAN_POINT('Origin',(0.,-0.07938,0.));
#25167=CARTESIAN_POINT('Origin',(1.11022302462516E-16,-0.07938,-1.675));
#25168=CARTESIAN_POINT('Origin',(1.11022302462516E-16,0.,-1.675));
#25169=CARTESIAN_POINT('',(0.397005914195118,-0.07938,-1.59456899932179));
#25170=CARTESIAN_POINT('Ctrl Pts',(0.397005914195119,-0.0793800000000001,
-1.59456899932179));
#25171=CARTESIAN_POINT('Ctrl Pts',(0.388626558458099,-0.123401821157026,
-1.59665523941937));
#25172=CARTESIAN_POINT('Ctrl Pts',(0.373030350867485,-0.166543350814306,
-1.60050712143809));
#25173=CARTESIAN_POINT('Ctrl Pts',(0.333298652394954,-0.237231147975234,
-1.60919314384089));
#25174=CARTESIAN_POINT('Ctrl Pts',(0.311480544243686,-0.266264900654909,
-1.61365775139403));
#25175=CARTESIAN_POINT('Ctrl Pts',(0.261368388670537,-0.317195968905306,
-1.62252828437015));
#25176=CARTESIAN_POINT('Ctrl Pts',(0.233069203882014,-0.33909093068465,
-1.62691869420078));
#25177=CARTESIAN_POINT('Ctrl Pts',(0.174042761838763,-0.373586846396559,
-1.63426473152765));
#25178=CARTESIAN_POINT('Ctrl Pts',(0.140365781471549,-0.388086240756494,
-1.63761964365402));
#25179=CARTESIAN_POINT('Ctrl Pts',(0.0701778381840612,-0.407068917407805,
-1.64212536811722));
#25180=CARTESIAN_POINT('Ctrl Pts',(0.0336652739555916,-0.411552957311693,
-1.643248));
#25181=CARTESIAN_POINT('Ctrl Pts',(-0.0336652739555915,-0.411552957311693,
-1.643248));
#25182=CARTESIAN_POINT('Ctrl Pts',(-0.0701778381840612,-0.407068917407805,
-1.64212536811722));
#25183=CARTESIAN_POINT('Ctrl Pts',(-0.140365781471549,-0.388086240756494,
-1.63761964365402));
#25184=CARTESIAN_POINT('Ctrl Pts',(-0.174042761838764,-0.373586846396559,
-1.63426473152765));
#25185=CARTESIAN_POINT('Ctrl Pts',(-0.233069203882014,-0.33909093068465,
-1.62691869420078));
#25186=CARTESIAN_POINT('Ctrl Pts',(-0.261368388670536,-0.317195968905306,
-1.62252828437015));
#25187=CARTESIAN_POINT('Ctrl Pts',(-0.311480544243686,-0.266264900654908,
-1.61365775139403));
#25188=CARTESIAN_POINT('Ctrl Pts',(-0.333298652394954,-0.237231147975234,
-1.60919314384089));
#25189=CARTESIAN_POINT('Ctrl Pts',(-0.373030350867485,-0.166543350814306,
-1.60050712143809));
#25190=CARTESIAN_POINT('Ctrl Pts',(-0.388626558458099,-0.123401821157026,
-1.59665523941937));
#25191=CARTESIAN_POINT('Ctrl Pts',(-0.397005914195118,-0.07938,-1.59456899932179));
#25192=CARTESIAN_POINT('Origin',(1.11022302462516E-16,-0.07938,-1.675));
#25193=CARTESIAN_POINT('Origin',(0.,-0.07938,0.));
#25194=CARTESIAN_POINT('',(0.846804978391753,-0.07938,-1.40825612658882));
#25195=CARTESIAN_POINT('Origin',(0.,-0.07938,0.));
#25196=CARTESIAN_POINT('Origin',(1.18440385848747,-0.07938,-1.18440385848747));
#25197=CARTESIAN_POINT('Origin',(1.18440385848747,0.,-1.18440385848747));
#25198=CARTESIAN_POINT('',(1.40825612658882,-0.07938,-0.846804978391753));
#25199=CARTESIAN_POINT('Ctrl Pts',(1.40825612658882,-0.0793800000000001,
-0.846804978391753));
#25200=CARTESIAN_POINT('Ctrl Pts',(1.40380622184538,-0.123401821157026,
-0.854205272175555));
#25201=CARTESIAN_POINT('Ctrl Pts',(1.39550172959303,-0.166543350814306,
-0.867957148219442));
#25202=CARTESIAN_POINT('Ctrl Pts',(1.3735491215176,-0.237231147975234,-0.902193646979983));
#25203=CARTESIAN_POINT('Ctrl Pts',(1.36127834356734,-0.266264900654908,
-0.920778333482565));
#25204=CARTESIAN_POINT('Ctrl Pts',(1.33211611256184,-0.317195968905306,
-0.962485392528369));
#25205=CARTESIAN_POINT('Ctrl Pts',(1.31521005565926,-0.33909093068465,-0.985600426557816));
#25206=CARTESIAN_POINT('Ctrl Pts',(1.27866649102984,-0.373586846396559,
-1.03253285680459));
#25207=CARTESIAN_POINT('Ctrl Pts',(1.25722555095714,-0.388086240756494,
-1.05871835910697));
#25208=CARTESIAN_POINT('Ctrl Pts',(1.2107812086231,-0.407068917407805,-1.11153475808518));
#25209=CARTESIAN_POINT('Ctrl Pts',(1.18575674747573,-0.411552957311693,
-1.13814686046673));
#25210=CARTESIAN_POINT('Ctrl Pts',(1.13814686046673,-0.411552957311693,
-1.18575674747573));
#25211=CARTESIAN_POINT('Ctrl Pts',(1.11153475808518,-0.407068917407805,
-1.2107812086231));
#25212=CARTESIAN_POINT('Ctrl Pts',(1.05871835910697,-0.388086240756494,
-1.25722555095714));
#25213=CARTESIAN_POINT('Ctrl Pts',(1.03253285680459,-0.373586846396559,
-1.27866649102984));
#25214=CARTESIAN_POINT('Ctrl Pts',(0.985600426557816,-0.33909093068465,
-1.31521005565926));
#25215=CARTESIAN_POINT('Ctrl Pts',(0.962485392528369,-0.317195968905306,
-1.33211611256184));
#25216=CARTESIAN_POINT('Ctrl Pts',(0.920778333482565,-0.266264900654909,
-1.36127834356734));
#25217=CARTESIAN_POINT('Ctrl Pts',(0.902193646979983,-0.237231147975234,
-1.3735491215176));
#25218=CARTESIAN_POINT('Ctrl Pts',(0.867957148219442,-0.166543350814306,
-1.39550172959303));
#25219=CARTESIAN_POINT('Ctrl Pts',(0.854205272175555,-0.123401821157026,
-1.40380622184538));
#25220=CARTESIAN_POINT('Ctrl Pts',(0.846804978391753,-0.0793800000000001,
-1.40825612658882));
#25221=CARTESIAN_POINT('Origin',(1.18440385848747,-0.07938,-1.18440385848747));
#25222=CARTESIAN_POINT('Origin',(0.,-0.27783,0.));
#25223=CARTESIAN_POINT('',(-1.643248,-0.47628,2.01239840340529E-16));
#25224=CARTESIAN_POINT('Origin',(0.,-0.47628,0.));
#25225=CARTESIAN_POINT('',(-1.643248,-0.27783,2.01239840340529E-16));
#25226=CARTESIAN_POINT('',(1.59456899932179,-0.07938,0.397005914195118));
#25227=CARTESIAN_POINT('Origin',(0.,-0.07938,0.));
#25228=CARTESIAN_POINT('',(1.59456899932179,-0.07938,-0.397005914195118));
#25229=CARTESIAN_POINT('Ctrl Pts',(1.59456899932179,-0.0793800000000001,
0.397005914195118));
#25230=CARTESIAN_POINT('Ctrl Pts',(1.59665523941937,-0.123401821157026,
0.388626558458099));
#25231=CARTESIAN_POINT('Ctrl Pts',(1.60050712143809,-0.166543350814306,
0.373030350867485));
#25232=CARTESIAN_POINT('Ctrl Pts',(1.60919314384089,-0.237231147975234,
0.333298652394954));
#25233=CARTESIAN_POINT('Ctrl Pts',(1.61365775139403,-0.266264900654909,
0.311480544243686));
#25234=CARTESIAN_POINT('Ctrl Pts',(1.62252828437015,-0.317195968905306,
0.261368388670537));
#25235=CARTESIAN_POINT('Ctrl Pts',(1.62691869420078,-0.33909093068465,0.233069203882014));
#25236=CARTESIAN_POINT('Ctrl Pts',(1.63426473152765,-0.373586846396559,
0.174042761838764));
#25237=CARTESIAN_POINT('Ctrl Pts',(1.63761964365402,-0.388086240756494,
0.140365781471549));
#25238=CARTESIAN_POINT('Ctrl Pts',(1.64212536811722,-0.407068917407805,
0.0701778381840612));
#25239=CARTESIAN_POINT('Ctrl Pts',(1.643248,-0.411552957311693,0.0336652739555916));
#25240=CARTESIAN_POINT('Ctrl Pts',(1.643248,-0.411552957311693,-0.0336652739555916));
#25241=CARTESIAN_POINT('Ctrl Pts',(1.64212536811722,-0.407068917407805,
-0.0701778381840612));
#25242=CARTESIAN_POINT('Ctrl Pts',(1.63761964365402,-0.388086240756494,
-0.140365781471549));
#25243=CARTESIAN_POINT('Ctrl Pts',(1.63426473152765,-0.373586846396559,
-0.174042761838764));
#25244=CARTESIAN_POINT('Ctrl Pts',(1.62691869420078,-0.33909093068465,-0.233069203882014));
#25245=CARTESIAN_POINT('Ctrl Pts',(1.62252828437015,-0.317195968905306,
-0.261368388670537));
#25246=CARTESIAN_POINT('Ctrl Pts',(1.61365775139403,-0.266264900654909,
-0.311480544243686));
#25247=CARTESIAN_POINT('Ctrl Pts',(1.60919314384089,-0.237231147975234,
-0.333298652394954));
#25248=CARTESIAN_POINT('Ctrl Pts',(1.60050712143809,-0.166543350814306,
-0.373030350867485));
#25249=CARTESIAN_POINT('Ctrl Pts',(1.59665523941937,-0.123401821157026,
-0.388626558458099));
#25250=CARTESIAN_POINT('Ctrl Pts',(1.59456899932179,-0.07938,-0.397005914195118));
#25251=CARTESIAN_POINT('Origin',(0.,-0.07938,0.));
#25252=CARTESIAN_POINT('Origin',(0.,-0.07938,0.));
#25253=CARTESIAN_POINT('Origin',(1.675,-0.07938,0.));
#25254=CARTESIAN_POINT('Origin',(1.675,0.,0.));
#25255=CARTESIAN_POINT('Origin',(1.675,-0.07938,0.));
#25256=CARTESIAN_POINT('Origin',(0.,-0.47628,0.));
#25257=CARTESIAN_POINT('Origin',(0.,-0.07938,0.));
#25258=CARTESIAN_POINT('',(0.,0.,0.));
#25259=CARTESIAN_POINT('Origin',(1.70469,0.695,0.));
#25260=CARTESIAN_POINT('',(-1.70469,0.695,-2.0876431520385E-16));
#25261=CARTESIAN_POINT('Origin',(0.,0.695,0.));
#25262=CARTESIAN_POINT('',(-1.65031,0.695,-2.02104685910087E-16));
#25263=CARTESIAN_POINT('Origin',(0.,0.695,0.));
#25264=CARTESIAN_POINT('Origin',(0.,0.6575,0.));
#25265=CARTESIAN_POINT('',(-1.70469,0.62,-2.0876431520385E-16));
#25266=CARTESIAN_POINT('Origin',(0.,0.62,0.));
#25267=CARTESIAN_POINT('',(-1.70469,0.6575,-2.0876431520385E-16));
#25268=CARTESIAN_POINT('Origin',(1.65031,0.62,0.));
#25269=CARTESIAN_POINT('',(-1.65031,0.62,-2.02104685910087E-16));
#25270=CARTESIAN_POINT('Origin',(0.,0.62,0.));
#25271=CARTESIAN_POINT('Origin',(0.,0.6575,0.));
#25272=CARTESIAN_POINT('',(-1.65031,0.6575,-2.02104685910087E-16));
#25273=CARTESIAN_POINT('Origin',(1.70469,-0.62,0.));
#25274=CARTESIAN_POINT('',(-1.70469,-0.62,-2.0876431520385E-16));
#25275=CARTESIAN_POINT('Origin',(0.,-0.62,0.));
#25276=CARTESIAN_POINT('',(-1.65031,-0.62,-2.02104685910087E-16));
#25277=CARTESIAN_POINT('Origin',(0.,-0.62,0.));
#25278=CARTESIAN_POINT('Origin',(0.,-0.6575,0.));
#25279=CARTESIAN_POINT('',(-1.70469,-0.695,-2.0876431520385E-16));
#25280=CARTESIAN_POINT('Origin',(0.,-0.695,0.));
#25281=CARTESIAN_POINT('',(-1.70469,-0.6575,-2.0876431520385E-16));
#25282=CARTESIAN_POINT('Origin',(1.65031,-0.695,0.));
#25283=CARTESIAN_POINT('',(-1.65031,-0.695,-2.02104685910087E-16));
#25284=CARTESIAN_POINT('Origin',(0.,-0.695,0.));
#25285=CARTESIAN_POINT('Origin',(0.,-0.6575,0.));
#25286=CARTESIAN_POINT('',(-1.65031,-0.6575,-2.02104685910087E-16));
#25287=CARTESIAN_POINT('',(0.,0.,0.));
#25288=CARTESIAN_POINT('',(0.,0.,0.));
#25289=CARTESIAN_POINT('',(0.,0.,0.));
#25290=CARTESIAN_POINT('',(0.,0.,0.));
#25291=CARTESIAN_POINT('',(0.,0.,0.));
#25292=CARTESIAN_POINT('',(0.,0.,0.));
#25293=CARTESIAN_POINT('Origin',(0.3,0.4,0.));
#25294=CARTESIAN_POINT('',(-0.3,0.4,-3.67394039744206E-17));
#25295=CARTESIAN_POINT('Origin',(0.,0.4,0.));
#25296=CARTESIAN_POINT('Origin',(0.,0.375,0.));
#25297=CARTESIAN_POINT('',(-0.35,0.35,-4.28626379701573E-17));
#25298=CARTESIAN_POINT('Origin',(0.,0.35,0.));
#25299=CARTESIAN_POINT('',(-0.325,0.375,-3.9801020972289E-17));
#25300=CARTESIAN_POINT('Origin',(0.,0.19,0.));
#25301=CARTESIAN_POINT('',(-0.35,0.03,-4.28626379701574E-17));
#25302=CARTESIAN_POINT('Origin',(0.,0.03,0.));
#25303=CARTESIAN_POINT('',(-0.35,0.19,-4.28626379701574E-17));
#25304=CARTESIAN_POINT('Origin',(0.,0.0149999999999999,0.));
#25305=CARTESIAN_POINT('',(-0.32,-3.29597460435593E-17,-3.91886975727153E-17));
#25306=CARTESIAN_POINT('Origin',(0.,0.,0.));
#25307=CARTESIAN_POINT('',(-0.335,0.0149999999999999,-4.10256677714363E-17));
#25308=CARTESIAN_POINT('Origin',(0.22,0.,0.));
#25309=CARTESIAN_POINT('',(-0.22,-6.93889390390723E-18,-2.69422295812418E-17));
#25310=CARTESIAN_POINT('Origin',(0.,0.,0.));
#25311=CARTESIAN_POINT('Origin',(0.,-0.02,0.));
#25312=CARTESIAN_POINT('',(-0.1954,-0.0492,2.39295984553393E-17));
#25313=CARTESIAN_POINT('Origin',(0.,-0.0492,0.));
#25314=CARTESIAN_POINT('',(-0.21,-0.02,-2.57175827820944E-17));
#25315=CARTESIAN_POINT('Origin',(0.,-0.8,0.));
#25316=CARTESIAN_POINT('',(-0.1954,-1.5646,2.39295984553393E-17));
#25317=CARTESIAN_POINT('Origin',(0.,-1.5646,0.));
#25318=CARTESIAN_POINT('',(-0.1954,-0.8,-2.39295984553393E-17));
#25319=CARTESIAN_POINT('Origin',(0.,-1.58,0.));
#25320=CARTESIAN_POINT('',(-0.16,-1.6,-1.95943487863577E-17));
#25321=CARTESIAN_POINT('Origin',(0.,-1.6,0.));
#25322=CARTESIAN_POINT('',(-0.18,-1.58,-2.20436423846524E-17));
#25323=CARTESIAN_POINT('Origin',(0.,-1.6,0.));
#25324=CARTESIAN_POINT('Origin',(0.0866025403784439,-0.4,-0.15));
#25325=CARTESIAN_POINT('',(0.173205080756888,-0.4,0.));
#25326=CARTESIAN_POINT('',(0.0866025403784439,-0.4,-0.15));
#25327=CARTESIAN_POINT('',(0.173205080756888,-0.4,0.));
#25328=CARTESIAN_POINT('',(0.0866025403784439,-0.64,-0.15));
#25329=CARTESIAN_POINT('',(0.0866025403784439,-0.4,-0.15));
#25330=CARTESIAN_POINT('',(0.173205080756888,-0.64,0.));
#25331=CARTESIAN_POINT('',(0.173205080756888,-0.64,0.));
#25332=CARTESIAN_POINT('',(0.173205080756888,-0.4,0.));
#25333=CARTESIAN_POINT('Origin',(-0.0866025403784438,-0.4,-0.15));
#25334=CARTESIAN_POINT('',(-0.0866025403784438,-0.4,-0.15));
#25335=CARTESIAN_POINT('',(0.0866025403784439,-0.4,-0.15));
#25336=CARTESIAN_POINT('',(-0.0866025403784438,-0.64,-0.15));
#25337=CARTESIAN_POINT('',(-0.0866025403784438,-0.4,-0.15));
#25338=CARTESIAN_POINT('',(0.0866025403784439,-0.64,-0.15));
#25339=CARTESIAN_POINT('Origin',(-0.173205080756888,-0.4,-2.77555756156289E-17));
#25340=CARTESIAN_POINT('',(-0.173205080756888,-0.4,-2.12115047744981E-17));
#25341=CARTESIAN_POINT('',(-0.0866025403784438,-0.4,-0.15));
#25342=CARTESIAN_POINT('',(-0.173205080756888,-0.64,-2.77555756156289E-17));
#25343=CARTESIAN_POINT('',(-0.173205080756888,-0.4,-2.12115047744981E-17));
#25344=CARTESIAN_POINT('',(-0.0866025403784438,-0.64,-0.15));
#25345=CARTESIAN_POINT('Origin',(-0.0866025403784439,-0.4,0.15));
#25346=CARTESIAN_POINT('',(-0.0866025403784439,-0.4,0.15));
#25347=CARTESIAN_POINT('',(-0.173205080756888,-0.4,-2.12115047744981E-17));
#25348=CARTESIAN_POINT('',(-0.0866025403784439,-0.64,0.15));
#25349=CARTESIAN_POINT('',(-0.0866025403784439,-0.4,0.15));
#25350=CARTESIAN_POINT('',(-0.173205080756888,-0.64,-2.12115047744981E-17));
#25351=CARTESIAN_POINT('Origin',(0.0866025403784439,-0.4,0.15));
#25352=CARTESIAN_POINT('',(0.0866025403784439,-0.4,0.15));
#25353=CARTESIAN_POINT('',(-0.0866025403784439,-0.4,0.15));
#25354=CARTESIAN_POINT('',(0.0866025403784439,-0.64,0.15));
#25355=CARTESIAN_POINT('',(0.0866025403784439,-0.4,0.15));
#25356=CARTESIAN_POINT('',(-0.0866025403784439,-0.64,0.15));
#25357=CARTESIAN_POINT('Origin',(0.173205080756888,-0.4,0.));
#25358=CARTESIAN_POINT('',(0.0866025403784439,-0.4,0.15));
#25359=CARTESIAN_POINT('',(0.0866025403784439,-0.64,0.15));
#25360=CARTESIAN_POINT('Origin',(0.,-0.4,-2.77555756156289E-17));
#25361=CARTESIAN_POINT('Origin',(0.,-0.64,-2.77555756156289E-17));
#25362=CARTESIAN_POINT('',(0.,0.,0.));
#25363=CARTESIAN_POINT('',(0.,0.,0.));
#25364=CARTESIAN_POINT('',(0.,0.,0.));
#25365=CARTESIAN_POINT('',(0.,0.,0.));
#25366=CARTESIAN_POINT('',(0.,0.,0.));
#25367=CARTESIAN_POINT('',(0.,0.,0.));
#25368=CARTESIAN_POINT('',(0.,0.,0.));
#25369=CARTESIAN_POINT('',(0.,0.,0.));
#25370=CARTESIAN_POINT('',(0.,0.,0.));
#25371=CARTESIAN_POINT('',(0.,0.,0.));
#25372=CARTESIAN_POINT('',(0.,0.,0.));
#25373=CARTESIAN_POINT('',(0.,0.,0.));
#25374=CARTESIAN_POINT('',(0.,0.,0.));
#25375=CARTESIAN_POINT('',(0.,0.,0.));
#25376=CARTESIAN_POINT('',(0.,0.,0.));
#25377=CARTESIAN_POINT('',(0.,0.,0.));
#25378=CARTESIAN_POINT('',(-4.75,-6.,10.8));
#25379=CARTESIAN_POINT('',(-4.75,0.,10.8));
#25380=CARTESIAN_POINT('',(-4.75,6.,10.8));
#25381=CARTESIAN_POINT('',(17.75,-6.,10.8));
#25382=CARTESIAN_POINT('',(17.75,0.,10.8));
#25383=CARTESIAN_POINT('',(17.75,6.,10.8));
#25384=CARTESIAN_POINT('',(-2.,-3.5,1.8));
#25385=CARTESIAN_POINT('',(-2.,3.5,1.8));
#25386=CARTESIAN_POINT('',(15.,-3.5,1.8));
#25387=CARTESIAN_POINT('',(15.,3.5,1.8));
#25388=CARTESIAN_POINT('',(0.,-6.,10.));
#25389=CARTESIAN_POINT('',(0.,6.,10.));
#25390=CARTESIAN_POINT('',(1.4142135623731,-7.8,11.4142135623731));
#25391=CARTESIAN_POINT('',(-1.41421356237309,-7.8,11.4142135623731));
#25392=CARTESIAN_POINT('',(-1.4142135623731,-7.8,8.5857864376269));
#25393=CARTESIAN_POINT('',(1.41421356237309,-7.8,8.5857864376269));
#25394=CARTESIAN_POINT('',(1.4142135623731,7.8,11.4142135623731));
#25395=CARTESIAN_POINT('',(-1.41421356237309,7.8,11.4142135623731));
#25396=CARTESIAN_POINT('',(-1.4142135623731,7.8,8.5857864376269));
#25397=CARTESIAN_POINT('',(1.41421356237309,7.8,8.5857864376269));
#25398=CARTESIAN_POINT('',(6.,-6.,10.));
#25399=CARTESIAN_POINT('',(6.,6.,10.));
#25400=CARTESIAN_POINT('',(7.83847763108502,-7.8,11.838477631085));
#25401=CARTESIAN_POINT('',(4.16152236891498,-7.8,11.838477631085));
#25402=CARTESIAN_POINT('',(4.16152236891498,-7.8,8.16152236891498));
#25403=CARTESIAN_POINT('',(7.83847763108502,-7.8,8.16152236891498));
#25404=CARTESIAN_POINT('',(7.83847763108502,7.8,11.838477631085));
#25405=CARTESIAN_POINT('',(4.16152236891498,7.8,11.838477631085));
#25406=CARTESIAN_POINT('',(4.16152236891498,7.8,8.16152236891498));
#25407=CARTESIAN_POINT('',(7.83847763108502,7.8,8.16152236891498));
#25408=CARTESIAN_POINT('',(12.,-6.,10.));
#25409=CARTESIAN_POINT('',(12.,6.,10.));
#25410=CARTESIAN_POINT('',(13.838477631085,-7.8,11.838477631085));
#25411=CARTESIAN_POINT('',(10.161522368915,-7.8,11.838477631085));
#25412=CARTESIAN_POINT('',(10.161522368915,-7.8,8.16152236891498));
#25413=CARTESIAN_POINT('',(13.838477631085,-7.8,8.16152236891498));
#25414=CARTESIAN_POINT('',(13.838477631085,7.8,11.838477631085));
#25415=CARTESIAN_POINT('',(10.161522368915,7.8,11.838477631085));
#25416=CARTESIAN_POINT('',(10.161522368915,7.8,8.16152236891498));
#25417=CARTESIAN_POINT('',(13.838477631085,7.8,8.16152236891498));
#25418=CARTESIAN_POINT('',(1.5,-3.5,16.5));
#25419=CARTESIAN_POINT('',(1.5,3.5,16.5));
#25420=CARTESIAN_POINT('',(14.5,-3.5,16.5));
#25421=CARTESIAN_POINT('',(14.5,3.5,16.5));
#25422=CARTESIAN_POINT('',(0.,0.,0.));
#25423=CARTESIAN_POINT('',(0.,0.,0.));
#25424=CARTESIAN_POINT('Origin',(-0.2,-2.1,8.8));
#25425=CARTESIAN_POINT('',(-0.2,-0.699999999999999,9.43431457505076));
#25426=CARTESIAN_POINT('',(-0.2,-2.1,9.43431457505076));
#25427=CARTESIAN_POINT('',(-0.2,-9.4,9.43431457505076));
#25428=CARTESIAN_POINT('',(-0.2,-0.7,9.65));
#25429=CARTESIAN_POINT('',(-0.2,-0.7,9.65));
#25430=CARTESIAN_POINT('',(-0.2,-2.1,9.65));
#25431=CARTESIAN_POINT('',(-0.2,-2.1,9.65));
#25432=CARTESIAN_POINT('',(-0.2,-2.1,9.65));
#25433=CARTESIAN_POINT('Origin',(0.,-2.1,9.225));
#25434=CARTESIAN_POINT('',(0.2,-2.1,9.43431457505076));
#25435=CARTESIAN_POINT('Origin',(0.,-2.1,10.));
#25436=CARTESIAN_POINT('',(0.2,-2.1,9.65));
#25437=CARTESIAN_POINT('',(0.2,-2.1,9.65));
#25438=CARTESIAN_POINT('',(0.2,-2.1,8.8));
#25439=CARTESIAN_POINT('Origin',(0.2,-2.1,9.65));
#25440=CARTESIAN_POINT('',(0.2,-0.699999999999999,9.43431457505076));
#25441=CARTESIAN_POINT('',(0.2,-9.4,9.43431457505076));
#25442=CARTESIAN_POINT('',(0.2,-0.7,9.65));
#25443=CARTESIAN_POINT('',(0.2,-2.1,9.65));
#25444=CARTESIAN_POINT('',(0.2,-0.7,8.8));
#25445=CARTESIAN_POINT('Origin',(-0.2,-2.1,9.65));
#25446=CARTESIAN_POINT('',(0.2,-0.7,9.65));
#25447=CARTESIAN_POINT('Origin',(0.,-0.7,9.225));
#25448=CARTESIAN_POINT('Origin',(0.,-0.699999999999999,10.));
#25449=CARTESIAN_POINT('Origin',(0.,-9.4,10.));
#25450=CARTESIAN_POINT('',(-0.6,9.4,10.));
#25451=CARTESIAN_POINT('Origin',(0.,9.4,10.));
#25452=CARTESIAN_POINT('',(-0.6,-9.4,10.));
#25453=CARTESIAN_POINT('',(-0.6,-9.4,10.));
#25454=CARTESIAN_POINT('Origin',(0.,-9.4,10.));
#25455=CARTESIAN_POINT('Origin',(0.,9.4,10.));
#25456=CARTESIAN_POINT('Origin',(0.,-9.4,10.));
#25457=CARTESIAN_POINT('',(0.,0.,0.));
#25458=CARTESIAN_POINT('Origin',(0.,-8.2,10.59));
#25459=CARTESIAN_POINT('',(0.133884278389952,-8.36178689687364,10.59));
#25460=CARTESIAN_POINT('',(0.133884278389952,-8.03821310312636,10.59));
#25461=CARTESIAN_POINT('',(0.133884278389952,-8.6,10.59));
#25462=CARTESIAN_POINT('Origin',(0.,-8.2,10.59));
#25463=CARTESIAN_POINT('Origin',(0.,-8.2,10.59));
#25464=CARTESIAN_POINT('',(-0.133884278389952,-8.36178689687364,10.59));
#25465=CARTESIAN_POINT('Ctrl Pts',(-0.133884278389951,-8.36178689687364,
10.59));
#25466=CARTESIAN_POINT('Ctrl Pts',(-0.118254395260798,-8.37472116821763,
10.5935467722442));
#25467=CARTESIAN_POINT('Ctrl Pts',(-0.100109787682296,-8.38579931658744,
10.5969822478996));
#25468=CARTESIAN_POINT('Ctrl Pts',(-0.0548298721325181,-8.40463856105443,
10.6030741628997));
#25469=CARTESIAN_POINT('Ctrl Pts',(-0.0266020595922904,-8.41,10.605));
#25470=CARTESIAN_POINT('Ctrl Pts',(0.0266020595922903,-8.41,10.605));
#25471=CARTESIAN_POINT('Ctrl Pts',(0.0548298721325192,-8.40463856105443,
10.6030741628997));
#25472=CARTESIAN_POINT('Ctrl Pts',(0.100109787682297,-8.38579931658744,
10.5969822478996));
#25473=CARTESIAN_POINT('Ctrl Pts',(0.118254395260798,-8.37472116821763,
10.5935467722442));
#25474=CARTESIAN_POINT('Ctrl Pts',(0.133884278389951,-8.36178689687364,
10.59));
#25475=CARTESIAN_POINT('',(-0.21,-8.2,10.59));
#25476=CARTESIAN_POINT('Origin',(0.,-8.2,10.59));
#25477=CARTESIAN_POINT('',(-0.21,-8.2,10.9777013859047));
#25478=CARTESIAN_POINT('',(-0.21,-8.2,10.59));
#25479=CARTESIAN_POINT('',(0.21,-8.2,10.9777013859047));
#25480=CARTESIAN_POINT('Ctrl Pts',(0.21,-8.2,10.9777013859047));
#25481=CARTESIAN_POINT('Ctrl Pts',(0.21,-8.22645388258983,10.9777013859047));
#25482=CARTESIAN_POINT('Ctrl Pts',(0.204697017125528,-8.25461525830868,
10.9788864661322));
#25483=CARTESIAN_POINT('Ctrl Pts',(0.18324175151553,-8.30633042130174,10.9831286999115));
#25484=CARTESIAN_POINT('Ctrl Pts',(0.167093586802906,-8.32989126129544,
10.9861204479665));
#25485=CARTESIAN_POINT('Ctrl Pts',(0.129892533236543,-8.36709231486181,
10.9917064515638));
#25486=CARTESIAN_POINT('Ctrl Pts',(0.106331154992713,-8.38324147510569,
10.994669144466));
#25487=CARTESIAN_POINT('Ctrl Pts',(0.0546141143983528,-8.40469746372443,
10.9988444923724));
#25488=CARTESIAN_POINT('Ctrl Pts',(0.0264520736824499,-8.41,11.));
#25489=CARTESIAN_POINT('Ctrl Pts',(-0.0264520736824498,-8.41,11.));
#25490=CARTESIAN_POINT('Ctrl Pts',(-0.0546141143983527,-8.40469746372443,
10.9988444923724));
#25491=CARTESIAN_POINT('Ctrl Pts',(-0.106331154992713,-8.38324147510569,
10.994669144466));
#25492=CARTESIAN_POINT('Ctrl Pts',(-0.129892533236543,-8.36709231486181,
10.9917064515638));
#25493=CARTESIAN_POINT('Ctrl Pts',(-0.167093586802906,-8.32989126129544,
10.9861204479665));
#25494=CARTESIAN_POINT('Ctrl Pts',(-0.18324175151553,-8.30633042130174,
10.9831286999115));
#25495=CARTESIAN_POINT('Ctrl Pts',(-0.204697017125528,-8.25461525830868,
10.9788864661322));
#25496=CARTESIAN_POINT('Ctrl Pts',(-0.21,-8.22645388258983,10.9777013859047));
#25497=CARTESIAN_POINT('Ctrl Pts',(-0.21,-8.2,10.9777013859047));
#25498=CARTESIAN_POINT('Ctrl Pts',(-0.21,-8.2,10.9777013859047));
#25499=CARTESIAN_POINT('Ctrl Pts',(-0.21,-8.17354611741017,10.9777013859047));
#25500=CARTESIAN_POINT('Ctrl Pts',(-0.204697017125528,-8.14538474169131,
10.9788864661322));
#25501=CARTESIAN_POINT('Ctrl Pts',(-0.18324175151553,-8.09366957869826,
10.9831286999115));
#25502=CARTESIAN_POINT('Ctrl Pts',(-0.167093586802907,-8.07010873870455,
10.9861204479665));
#25503=CARTESIAN_POINT('Ctrl Pts',(-0.129892533236543,-8.03290768513819,
10.9917064515638));
#25504=CARTESIAN_POINT('Ctrl Pts',(-0.106331154992713,-8.01675852489431,
10.994669144466));
#25505=CARTESIAN_POINT('Ctrl Pts',(-0.0546141143983529,-7.99530253627557,
10.9988444923724));
#25506=CARTESIAN_POINT('Ctrl Pts',(-0.0264520736824499,-7.99,11.));
#25507=CARTESIAN_POINT('Ctrl Pts',(0.0264520736824497,-7.99,11.));
#25508=CARTESIAN_POINT('Ctrl Pts',(0.0546141143983529,-7.99530253627557,
10.9988444923724));
#25509=CARTESIAN_POINT('Ctrl Pts',(0.106331154992714,-8.01675852489431,
10.994669144466));
#25510=CARTESIAN_POINT('Ctrl Pts',(0.129892533236543,-8.03290768513819,
10.9917064515638));
#25511=CARTESIAN_POINT('Ctrl Pts',(0.167093586802906,-8.07010873870455,
10.9861204479665));
#25512=CARTESIAN_POINT('Ctrl Pts',(0.18324175151553,-8.09366957869826,10.9831286999115));
#25513=CARTESIAN_POINT('Ctrl Pts',(0.204697017125528,-8.14538474169131,
10.9788864661322));
#25514=CARTESIAN_POINT('Ctrl Pts',(0.21,-8.17354611741017,10.9777013859047));
#25515=CARTESIAN_POINT('Ctrl Pts',(0.21,-8.2,10.9777013859047));
#25516=CARTESIAN_POINT('',(-0.133884278389952,-8.03821310312636,10.59));
#25517=CARTESIAN_POINT('Origin',(0.,-8.2,10.59));
#25518=CARTESIAN_POINT('Ctrl Pts',(0.133884278389952,-8.03821310312636,
10.59));
#25519=CARTESIAN_POINT('Ctrl Pts',(0.118254395260798,-8.02527883178237,
10.5935467722442));
#25520=CARTESIAN_POINT('Ctrl Pts',(0.100109787682297,-8.01420068341256,
10.5969822478996));
#25521=CARTESIAN_POINT('Ctrl Pts',(0.0548298721325187,-7.99536143894557,
10.6030741628997));
#25522=CARTESIAN_POINT('Ctrl Pts',(0.0266020595922903,-7.99,10.605));
#25523=CARTESIAN_POINT('Ctrl Pts',(-0.0266020595922903,-7.99,10.605));
#25524=CARTESIAN_POINT('Ctrl Pts',(-0.0548298721325201,-7.99536143894557,
10.6030741628997));
#25525=CARTESIAN_POINT('Ctrl Pts',(-0.100109787682298,-8.01420068341256,
10.5969822478996));
#25526=CARTESIAN_POINT('Ctrl Pts',(-0.118254395260797,-8.02527883178237,
10.5935467722442));
#25527=CARTESIAN_POINT('Ctrl Pts',(-0.133884278389951,-8.03821310312636,
10.59));
#25528=CARTESIAN_POINT('Origin',(0.,-8.2,10.59));
#25529=CARTESIAN_POINT('',(-0.133884278389952,-8.6,10.59));
#25530=CARTESIAN_POINT('Origin',(0.,-8.6,10.));
#25531=CARTESIAN_POINT('',(-0.605,-7.8,10.));
#25532=CARTESIAN_POINT('Origin',(0.,-7.8,10.));
#25533=CARTESIAN_POINT('',(-0.605,-8.6,10.));
#25534=CARTESIAN_POINT('',(-0.605,-8.6,10.));
#25535=CARTESIAN_POINT('Origin',(0.,-8.6,10.));
#25536=CARTESIAN_POINT('Origin',(0.,-8.6,10.));
#25537=CARTESIAN_POINT('',(-1.,-7.8,10.));
#25538=CARTESIAN_POINT('Origin',(0.,-7.8,10.));
#25539=CARTESIAN_POINT('',(-1.,-8.6,10.));
#25540=CARTESIAN_POINT('',(-1.,-8.6,10.));
#25541=CARTESIAN_POINT('Origin',(0.,-8.6,10.));
#25542=CARTESIAN_POINT('Origin',(0.,-7.8,10.));
#25543=CARTESIAN_POINT('Origin',(0.,-8.6,10.));
#25544=CARTESIAN_POINT('',(0.,0.,0.));
#25545=CARTESIAN_POINT('Origin',(0.,8.2,10.59));
#25546=CARTESIAN_POINT('',(0.133884278389952,8.03821310312636,10.59));
#25547=CARTESIAN_POINT('',(0.133884278389952,8.36178689687364,10.59));
#25548=CARTESIAN_POINT('',(0.133884278389952,7.8,10.59));
#25549=CARTESIAN_POINT('Origin',(0.,8.2,10.59));
#25550=CARTESIAN_POINT('Origin',(0.,8.2,10.59));
#25551=CARTESIAN_POINT('',(-0.133884278389952,8.03821310312636,10.59));
#25552=CARTESIAN_POINT('Ctrl Pts',(-0.133884278389952,8.03821310312636,
10.59));
#25553=CARTESIAN_POINT('Ctrl Pts',(-0.118254395260798,8.02527883178237,
10.5935467722442));
#25554=CARTESIAN_POINT('Ctrl Pts',(-0.100109787682297,8.01420068341256,
10.5969822478996));
#25555=CARTESIAN_POINT('Ctrl Pts',(-0.0548298721325187,7.99536143894557,
10.6030741628997));
#25556=CARTESIAN_POINT('Ctrl Pts',(-0.0266020595922903,7.99,10.605));
#25557=CARTESIAN_POINT('Ctrl Pts',(0.0266020595922902,7.99,10.605));
#25558=CARTESIAN_POINT('Ctrl Pts',(0.0548298721325187,7.99536143894557,
10.6030741628997));
#25559=CARTESIAN_POINT('Ctrl Pts',(0.100109787682297,8.01420068341256,10.5969822478996));
#25560=CARTESIAN_POINT('Ctrl Pts',(0.118254395260798,8.02527883178237,10.5935467722442));
#25561=CARTESIAN_POINT('Ctrl Pts',(0.133884278389952,8.03821310312636,10.59));
#25562=CARTESIAN_POINT('',(-0.21,8.2,10.59));
#25563=CARTESIAN_POINT('Origin',(0.,8.2,10.59));
#25564=CARTESIAN_POINT('',(-0.21,8.2,10.9777013859047));
#25565=CARTESIAN_POINT('',(-0.21,8.2,10.59));
#25566=CARTESIAN_POINT('',(0.21,8.2,10.9777013859047));
#25567=CARTESIAN_POINT('Ctrl Pts',(0.21,8.2,10.9777013859047));
#25568=CARTESIAN_POINT('Ctrl Pts',(0.21,8.17354611741017,10.9777013859047));
#25569=CARTESIAN_POINT('Ctrl Pts',(0.204697017125528,8.14538474169131,10.9788864661322));
#25570=CARTESIAN_POINT('Ctrl Pts',(0.18324175151553,8.09366957869826,10.9831286999115));
#25571=CARTESIAN_POINT('Ctrl Pts',(0.167093586802907,8.07010873870455,10.9861204479665));
#25572=CARTESIAN_POINT('Ctrl Pts',(0.129892533236543,8.03290768513819,10.9917064515638));
#25573=CARTESIAN_POINT('Ctrl Pts',(0.106331154992713,8.01675852489431,10.994669144466));
#25574=CARTESIAN_POINT('Ctrl Pts',(0.0546141143983529,7.99530253627557,
10.9988444923724));
#25575=CARTESIAN_POINT('Ctrl Pts',(0.0264520736824498,7.99,11.));
#25576=CARTESIAN_POINT('Ctrl Pts',(-0.0264520736824498,7.99,11.));
#25577=CARTESIAN_POINT('Ctrl Pts',(-0.0546141143983529,7.99530253627557,
10.9988444923724));
#25578=CARTESIAN_POINT('Ctrl Pts',(-0.106331154992713,8.01675852489431,
10.994669144466));
#25579=CARTESIAN_POINT('Ctrl Pts',(-0.129892533236543,8.03290768513819,
10.9917064515638));
#25580=CARTESIAN_POINT('Ctrl Pts',(-0.167093586802907,8.07010873870455,
10.9861204479665));
#25581=CARTESIAN_POINT('Ctrl Pts',(-0.18324175151553,8.09366957869826,10.9831286999115));
#25582=CARTESIAN_POINT('Ctrl Pts',(-0.204697017125528,8.14538474169131,
10.9788864661322));
#25583=CARTESIAN_POINT('Ctrl Pts',(-0.21,8.17354611741017,10.9777013859047));
#25584=CARTESIAN_POINT('Ctrl Pts',(-0.21,8.2,10.9777013859047));
#25585=CARTESIAN_POINT('Ctrl Pts',(-0.21,8.2,10.9777013859047));
#25586=CARTESIAN_POINT('Ctrl Pts',(-0.21,8.22645388258983,10.9777013859047));
#25587=CARTESIAN_POINT('Ctrl Pts',(-0.204697017125528,8.25461525830868,
10.9788864661322));
#25588=CARTESIAN_POINT('Ctrl Pts',(-0.18324175151553,8.30633042130174,10.9831286999115));
#25589=CARTESIAN_POINT('Ctrl Pts',(-0.167093586802906,8.32989126129544,
10.9861204479665));
#25590=CARTESIAN_POINT('Ctrl Pts',(-0.129892533236543,8.36709231486181,
10.9917064515638));
#25591=CARTESIAN_POINT('Ctrl Pts',(-0.106331154992713,8.38324147510569,
10.994669144466));
#25592=CARTESIAN_POINT('Ctrl Pts',(-0.0546141143983529,8.40469746372443,
10.9988444923724));
#25593=CARTESIAN_POINT('Ctrl Pts',(-0.0264520736824499,8.41,11.));
#25594=CARTESIAN_POINT('Ctrl Pts',(0.0264520736824498,8.41,11.));
#25595=CARTESIAN_POINT('Ctrl Pts',(0.0546141143983528,8.40469746372443,
10.9988444923724));
#25596=CARTESIAN_POINT('Ctrl Pts',(0.106331154992713,8.38324147510569,10.994669144466));
#25597=CARTESIAN_POINT('Ctrl Pts',(0.129892533236543,8.36709231486181,10.9917064515638));
#25598=CARTESIAN_POINT('Ctrl Pts',(0.167093586802906,8.32989126129544,10.9861204479665));
#25599=CARTESIAN_POINT('Ctrl Pts',(0.18324175151553,8.30633042130174,10.9831286999115));
#25600=CARTESIAN_POINT('Ctrl Pts',(0.204697017125528,8.25461525830868,10.9788864661322));
#25601=CARTESIAN_POINT('Ctrl Pts',(0.21,8.22645388258983,10.9777013859047));
#25602=CARTESIAN_POINT('Ctrl Pts',(0.21,8.2,10.9777013859047));
#25603=CARTESIAN_POINT('',(-0.133884278389952,8.36178689687364,10.59));
#25604=CARTESIAN_POINT('Origin',(0.,8.2,10.59));
#25605=CARTESIAN_POINT('Ctrl Pts',(0.133884278389952,8.36178689687364,10.59));
#25606=CARTESIAN_POINT('Ctrl Pts',(0.1182543952608,8.37472116821763,10.5935467722442));
#25607=CARTESIAN_POINT('Ctrl Pts',(0.100109787682296,8.38579931658744,10.5969822478996));
#25608=CARTESIAN_POINT('Ctrl Pts',(0.0548298721325181,8.40463856105443,
10.6030741628997));
#25609=CARTESIAN_POINT('Ctrl Pts',(0.0266020595922904,8.41,10.605));
#25610=CARTESIAN_POINT('Ctrl Pts',(-0.0266020595922903,8.41,10.605));
#25611=CARTESIAN_POINT('Ctrl Pts',(-0.0548298721325181,8.40463856105443,
10.6030741628997));
#25612=CARTESIAN_POINT('Ctrl Pts',(-0.100109787682296,8.38579931658744,
10.5969822478996));
#25613=CARTESIAN_POINT('Ctrl Pts',(-0.118254395260799,8.37472116821763,
10.5935467722442));
#25614=CARTESIAN_POINT('Ctrl Pts',(-0.133884278389951,8.36178689687364,
10.59));
#25615=CARTESIAN_POINT('Origin',(0.,8.2,10.59));
#25616=CARTESIAN_POINT('',(-0.133884278389952,7.8,10.59));
#25617=CARTESIAN_POINT('Origin',(0.,7.8,10.));
#25618=CARTESIAN_POINT('',(-0.605,8.6,10.));
#25619=CARTESIAN_POINT('Origin',(0.,8.6,10.));
#25620=CARTESIAN_POINT('',(-0.605,7.8,10.));
#25621=CARTESIAN_POINT('',(-0.605,7.8,10.));
#25622=CARTESIAN_POINT('Origin',(0.,7.8,10.));
#25623=CARTESIAN_POINT('Origin',(0.,7.8,10.));
#25624=CARTESIAN_POINT('',(-1.,8.6,10.));
#25625=CARTESIAN_POINT('Origin',(0.,8.6,10.));
#25626=CARTESIAN_POINT('',(-1.,7.8,10.));
#25627=CARTESIAN_POINT('',(-1.,7.8,10.));
#25628=CARTESIAN_POINT('Origin',(0.,7.8,10.));
#25629=CARTESIAN_POINT('Origin',(0.,8.6,10.));
#25630=CARTESIAN_POINT('Origin',(0.,7.8,10.));
#25631=CARTESIAN_POINT('',(0.,0.,0.));
#25632=CARTESIAN_POINT('Origin',(0.,-7.8,10.));
#25633=CARTESIAN_POINT('',(-0.605,-6.5,10.));
#25634=CARTESIAN_POINT('Origin',(0.,-6.5,10.));
#25635=CARTESIAN_POINT('',(-0.605,-7.8,10.));
#25636=CARTESIAN_POINT('',(-0.605,-7.8,10.));
#25637=CARTESIAN_POINT('Origin',(0.,-7.8,10.));
#25638=CARTESIAN_POINT('Origin',(0.,-7.8,10.));
#25639=CARTESIAN_POINT('',(-0.9,-6.5,10.));
#25640=CARTESIAN_POINT('Origin',(0.,-6.5,10.));
#25641=CARTESIAN_POINT('',(-0.9,-7.8,10.));
#25642=CARTESIAN_POINT('',(-0.9,-7.8,10.));
#25643=CARTESIAN_POINT('Origin',(0.,-7.8,10.));
#25644=CARTESIAN_POINT('Origin',(0.,-6.5,10.));
#25645=CARTESIAN_POINT('Origin',(0.,-7.8,10.));
#25646=CARTESIAN_POINT('',(0.,0.,0.));
#25647=CARTESIAN_POINT('Origin',(0.,6.5,10.));
#25648=CARTESIAN_POINT('',(-0.605,7.8,10.));
#25649=CARTESIAN_POINT('Origin',(0.,7.8,10.));
#25650=CARTESIAN_POINT('',(-0.605,6.5,10.));
#25651=CARTESIAN_POINT('',(-0.605,6.5,10.));
#25652=CARTESIAN_POINT('Origin',(0.,6.5,10.));
#25653=CARTESIAN_POINT('Origin',(0.,6.5,10.));
#25654=CARTESIAN_POINT('',(-0.9,7.8,10.));
#25655=CARTESIAN_POINT('Origin',(0.,7.8,10.));
#25656=CARTESIAN_POINT('',(-0.9,6.5,10.));
#25657=CARTESIAN_POINT('',(-0.9,6.5,10.));
#25658=CARTESIAN_POINT('Origin',(0.,6.5,10.));
#25659=CARTESIAN_POINT('Origin',(0.,7.8,10.));
#25660=CARTESIAN_POINT('Origin',(0.,6.5,10.));
#25661=CARTESIAN_POINT('',(0.,0.,0.));
#25662=CARTESIAN_POINT('Origin',(0.,-5.5,10.));
#25663=CARTESIAN_POINT('',(-0.605,-3.,10.));
#25664=CARTESIAN_POINT('Origin',(0.,-3.,10.));
#25665=CARTESIAN_POINT('',(-0.605,-5.5,10.));
#25666=CARTESIAN_POINT('',(-0.605,-5.5,10.));
#25667=CARTESIAN_POINT('Origin',(0.,-5.5,10.));
#25668=CARTESIAN_POINT('Origin',(0.,-5.5,10.));
#25669=CARTESIAN_POINT('',(-0.9,-3.,10.));
#25670=CARTESIAN_POINT('Origin',(0.,-3.,10.));
#25671=CARTESIAN_POINT('',(-0.9,-5.5,10.));
#25672=CARTESIAN_POINT('',(-0.9,-5.5,10.));
#25673=CARTESIAN_POINT('Origin',(0.,-5.5,10.));
#25674=CARTESIAN_POINT('Origin',(0.,-3.,10.));
#25675=CARTESIAN_POINT('Origin',(0.,-5.5,10.));
#25676=CARTESIAN_POINT('',(0.,0.,0.));
#25677=CARTESIAN_POINT('Origin',(0.,0.2,10.));
#25678=CARTESIAN_POINT('',(-0.605,5.5,10.));
#25679=CARTESIAN_POINT('Origin',(0.,5.5,10.));
#25680=CARTESIAN_POINT('',(-0.605,0.2,10.));
#25681=CARTESIAN_POINT('',(-0.605,0.2,10.));
#25682=CARTESIAN_POINT('Origin',(0.,0.2,10.));
#25683=CARTESIAN_POINT('Origin',(0.,0.2,10.));
#25684=CARTESIAN_POINT('',(-0.9,5.5,10.));
#25685=CARTESIAN_POINT('Origin',(0.,5.5,10.));
#25686=CARTESIAN_POINT('',(-0.9,0.2,10.));
#25687=CARTESIAN_POINT('',(-0.9,0.2,10.));
#25688=CARTESIAN_POINT('Origin',(0.,0.2,10.));
#25689=CARTESIAN_POINT('Origin',(0.,5.5,10.));
#25690=CARTESIAN_POINT('Origin',(0.,0.2,10.));
#25691=CARTESIAN_POINT('',(0.,0.,0.));
#25692=CARTESIAN_POINT('Origin',(0.2,0.,0.));
#25693=CARTESIAN_POINT('',(0.2,2.2,-0.78));
#25694=CARTESIAN_POINT('',(0.2,2.2,-0.565685424949238));
#25695=CARTESIAN_POINT('',(0.2,2.2,0.));
#25696=CARTESIAN_POINT('',(0.2,-1.,-0.78));
#25697=CARTESIAN_POINT('',(0.2,0.,-0.78));
#25698=CARTESIAN_POINT('',(0.2,-1.,-0.565685424949238));
#25699=CARTESIAN_POINT('',(0.2,-1.,0.));
#25700=CARTESIAN_POINT('',(0.2,0.,-0.565685424949238));
#25701=CARTESIAN_POINT('Origin',(0.2,0.,-0.78));
#25702=CARTESIAN_POINT('',(-0.2,2.2,-0.78));
#25703=CARTESIAN_POINT('',(0.1,2.2,-0.78));
#25704=CARTESIAN_POINT('',(-0.2,-1.,-0.78));
#25705=CARTESIAN_POINT('',(-0.2,0.,-0.78));
#25706=CARTESIAN_POINT('',(0.1,-1.,-0.78));
#25707=CARTESIAN_POINT('Origin',(-0.2,0.,-0.78));
#25708=CARTESIAN_POINT('',(-0.2,2.2,-0.565685424949238));
#25709=CARTESIAN_POINT('',(-0.2,2.2,-0.39));
#25710=CARTESIAN_POINT('',(-0.2,-1.,-0.565685424949238));
#25711=CARTESIAN_POINT('',(-0.2,0.,-0.565685424949238));
#25712=CARTESIAN_POINT('',(-0.2,-1.,-0.39));
#25713=CARTESIAN_POINT('Origin',(0.,-1.,0.));
#25714=CARTESIAN_POINT('',(1.60662857109684,-1.,0.693717979106306));
#25715=CARTESIAN_POINT('',(1.5055822144029,-1.,0.892032620296856));
#25716=CARTESIAN_POINT('Origin',(0.,-1.,0.));
#25717=CARTESIAN_POINT('',(1.81978687191668,-1.,1.23627494547115));
#25718=CARTESIAN_POINT('Ctrl Pts',(1.5055822144029,-1.,0.892032620296856));
#25719=CARTESIAN_POINT('Ctrl Pts',(1.50980486806688,-1.,0.894452006964544));
#25720=CARTESIAN_POINT('Ctrl Pts',(1.51805569590094,-1.,0.899185047483511));
#25721=CARTESIAN_POINT('Ctrl Pts',(1.52984849887993,-1.,0.905967409625651));
#25722=CARTESIAN_POINT('Ctrl Pts',(1.54440491149498,-1.,0.914375919026456));
#25723=CARTESIAN_POINT('Ctrl Pts',(1.56065988578893,-1.,0.923832188944341));
#25724=CARTESIAN_POINT('Ctrl Pts',(1.57499388382243,-1.,0.932246680108685));
#25725=CARTESIAN_POINT('Ctrl Pts',(1.58744937487176,-1.,0.939646377893399));
#25726=CARTESIAN_POINT('Ctrl Pts',(1.59810042043673,-1.,0.946078063315257));
#25727=CARTESIAN_POINT('Ctrl Pts',(1.60706069896936,-1.,0.951613284356035));
#25728=CARTESIAN_POINT('Ctrl Pts',(1.61449324337085,-1.,0.956354422920671));
#25729=CARTESIAN_POINT('Ctrl Pts',(1.62061638140221,-1.,0.960438326101729));
#25730=CARTESIAN_POINT('Ctrl Pts',(1.62571930670187,-1.,0.964046107040536));
#25731=CARTESIAN_POINT('Ctrl Pts',(1.63013849959461,-1.,0.967387853230345));
#25732=CARTESIAN_POINT('Ctrl Pts',(1.63420665729798,-1.,0.970669715997509));
#25733=CARTESIAN_POINT('Ctrl Pts',(1.63820952658144,-1.,0.974066058287419));
#25734=CARTESIAN_POINT('Ctrl Pts',(1.64233990826687,-1.,0.977689794119417));
#25735=CARTESIAN_POINT('Ctrl Pts',(1.64665139190656,-1.,0.981562530939489));
#25736=CARTESIAN_POINT('Ctrl Pts',(1.65110016612638,-1.,0.985642622920821));
#25737=CARTESIAN_POINT('Ctrl Pts',(1.65559044289699,-1.,0.989855627854165));
#25738=CARTESIAN_POINT('Ctrl Pts',(1.66001553809947,-1.,0.994121836661306));
#25739=CARTESIAN_POINT('Ctrl Pts',(1.66430758030376,-1.,0.998389654952758));
#25740=CARTESIAN_POINT('Ctrl Pts',(1.66846059277303,-1.,1.00265091003727));
#25741=CARTESIAN_POINT('Ctrl Pts',(1.67250335383293,-1.,1.00692206696414));
#25742=CARTESIAN_POINT('Ctrl Pts',(1.67648246776464,-1.,1.01123236493511));
#25743=CARTESIAN_POINT('Ctrl Pts',(1.68044289894798,-1.,1.01561026162773));
#25744=CARTESIAN_POINT('Ctrl Pts',(1.68440578021706,-1.,1.02006795074201));
#25745=CARTESIAN_POINT('Ctrl Pts',(1.68836910178447,-1.,1.02460180535255));
#25746=CARTESIAN_POINT('Ctrl Pts',(1.69231840863458,-1.,1.02919977579147));
#25747=CARTESIAN_POINT('Ctrl Pts',(1.69623414782771,-1.,1.03384646003588));
#25748=CARTESIAN_POINT('Ctrl Pts',(1.70010052930962,-1.,1.03852922490789));
#25749=CARTESIAN_POINT('Ctrl Pts',(1.70391338707982,-1.,1.04324363334554));
#25750=CARTESIAN_POINT('Ctrl Pts',(1.70767646263649,-1.,1.04799085404995));
#25751=CARTESIAN_POINT('Ctrl Pts',(1.71139783543989,-1.,1.05277517202855));
#25752=CARTESIAN_POINT('Ctrl Pts',(1.7150865442702,-1.,1.05760163192479));
#25753=CARTESIAN_POINT('Ctrl Pts',(1.71874858456904,-1.,1.06247324680647));
#25754=CARTESIAN_POINT('Ctrl Pts',(1.72238500928453,-1.,1.06738966975462));
#25755=CARTESIAN_POINT('Ctrl Pts',(1.72599406198488,-1.,1.07234866990252));
#25756=CARTESIAN_POINT('Ctrl Pts',(1.72957248977424,-1.,1.0773470373727));
#25757=CARTESIAN_POINT('Ctrl Pts',(1.73311705663407,-1.,1.08238162784749));
#25758=CARTESIAN_POINT('Ctrl Pts',(1.73662628326091,-1.,1.08745056285427));
#25759=CARTESIAN_POINT('Ctrl Pts',(1.74010053962247,-1.,1.09255329056493));
#25760=CARTESIAN_POINT('Ctrl Pts',(1.74354119236208,-1.,1.09768999241226));
#25761=CARTESIAN_POINT('Ctrl Pts',(1.74695004214923,-1.,1.10286118991143));
#25762=CARTESIAN_POINT('Ctrl Pts',(1.7503286607592,-1.,1.10806728183007));
#25763=CARTESIAN_POINT('Ctrl Pts',(1.7536777209463,-1.,1.11330807582551));
#25764=CARTESIAN_POINT('Ctrl Pts',(1.75699720772105,-1.,1.11858293216763));
#25765=CARTESIAN_POINT('Ctrl Pts',(1.76028671825096,-1.,1.12389096855086));
#25766=CARTESIAN_POINT('Ctrl Pts',(1.7635457196617,-1.,1.12923123555075));
#25767=CARTESIAN_POINT('Ctrl Pts',(1.76677384551862,-1.,1.1346029180462));
#25768=CARTESIAN_POINT('Ctrl Pts',(1.76997111386769,-1.,1.14000548336975));
#25769=CARTESIAN_POINT('Ctrl Pts',(1.77313777896194,-1.,1.1454385822692));
#25770=CARTESIAN_POINT('Ctrl Pts',(1.7762742255701,-1.,1.15090197841515));
#25771=CARTESIAN_POINT('Ctrl Pts',(1.77938085564275,-1.,1.15639547194698));
#25772=CARTESIAN_POINT('Ctrl Pts',(1.78245795881009,-1.,1.16191881298499));
#25773=CARTESIAN_POINT('Ctrl Pts',(1.78550566040443,-1.,1.16747166312303));
#25774=CARTESIAN_POINT('Ctrl Pts',(1.78852398877616,-1.,1.17305363177328));
#25775=CARTESIAN_POINT('Ctrl Pts',(1.79151291552689,-1.,1.17866429440809));
#25776=CARTESIAN_POINT('Ctrl Pts',(1.79447240321515,-1.,1.18430321697432));
#25777=CARTESIAN_POINT('Ctrl Pts',(1.79740245923478,-1.,1.18996997934445));
#25778=CARTESIAN_POINT('Ctrl Pts',(1.80030314369879,-1.,1.19566418930242));
#25779=CARTESIAN_POINT('Ctrl Pts',(1.80317454838603,-1.,1.20138548938974));
#25780=CARTESIAN_POINT('Ctrl Pts',(1.80601678480707,-1.,1.20713356605475));
#25781=CARTESIAN_POINT('Ctrl Pts',(1.80882996917129,-1.,1.21290815708314));
#25782=CARTESIAN_POINT('Ctrl Pts',(1.81161420806656,-1.,1.21870906103557));
#25783=CARTESIAN_POINT('Ctrl Pts',(1.81436959210434,-1.,1.2245361330495));
#25784=CARTESIAN_POINT('Ctrl Pts',(1.8165508718364,-1.,1.2292186489137));
#25785=CARTESIAN_POINT('Ctrl Pts',(1.81817389921279,-1.,1.2327422452705));
#25786=CARTESIAN_POINT('Ctrl Pts',(1.81925017193666,-1.,1.23509651170476));
#25787=CARTESIAN_POINT('Ctrl Pts',(1.81978687191668,-1.,1.23627494547115));
#25788=CARTESIAN_POINT('',(1.73811241238545,-1.,1.34869019493419));
#25789=CARTESIAN_POINT('',(1.81978687191668,-1.,1.23627494547115));
#25790=CARTESIAN_POINT('',(1.31362392696032,-1.,1.15624053661742));
#25791=CARTESIAN_POINT('Ctrl Pts',(1.73811241238545,-1.,1.34869019493419));
#25792=CARTESIAN_POINT('Ctrl Pts',(1.73682580585691,-1.,1.34854391898045));
#25793=CARTESIAN_POINT('Ctrl Pts',(1.73425417885907,-1.,1.34824783112887));
#25794=CARTESIAN_POINT('Ctrl Pts',(1.7304014965394,-1.,1.34779309152035));
#25795=CARTESIAN_POINT('Ctrl Pts',(1.72527410680674,-1.,1.34716554819527));
#25796=CARTESIAN_POINT('Ctrl Pts',(1.7188807715049,-1.,1.34634568653227));
#25797=CARTESIAN_POINT('Ctrl Pts',(1.71250340686822,-1.,1.34549029589416));
#25798=CARTESIAN_POINT('Ctrl Pts',(1.70614212266738,-1.,1.34459924533831));
#25799=CARTESIAN_POINT('Ctrl Pts',(1.69979707754427,-1.,1.34367237124483));
#25800=CARTESIAN_POINT('Ctrl Pts',(1.6934684849687,-1.,1.34270948206319));
#25801=CARTESIAN_POINT('Ctrl Pts',(1.68715660868764,-1.,1.341710374848));
#25802=CARTESIAN_POINT('Ctrl Pts',(1.68086176030362,-1.,1.34067485185203));
#25803=CARTESIAN_POINT('Ctrl Pts',(1.67458429426086,-1.,1.3396027347034));
#25804=CARTESIAN_POINT('Ctrl Pts',(1.66832460783989,-1.,1.33849388654388));
#25805=CARTESIAN_POINT('Ctrl Pts',(1.66208312541983,-1.,1.33734820885262));
#25806=CARTESIAN_POINT('Ctrl Pts',(1.65586025952593,-1.,1.33616559745172));
#25807=CARTESIAN_POINT('Ctrl Pts',(1.6496563728683,-1.,1.33494590467993));
#25808=CARTESIAN_POINT('Ctrl Pts',(1.6434717485603,-1.,1.33368890676572));
#25809=CARTESIAN_POINT('Ctrl Pts',(1.63730653475089,-1.,1.33239425103724));
#25810=CARTESIAN_POINT('Ctrl Pts',(1.63116079730923,-1.,1.33106149345645));
#25811=CARTESIAN_POINT('Ctrl Pts',(1.62503464209797,-1.,1.3296901950568));
#25812=CARTESIAN_POINT('Ctrl Pts',(1.61892832270724,-1.,1.32828000610449));
#25813=CARTESIAN_POINT('Ctrl Pts',(1.6128423401575,-1.,1.32683074483356));
#25814=CARTESIAN_POINT('Ctrl Pts',(1.60677758290954,-1.,1.32534250785782));
#25815=CARTESIAN_POINT('Ctrl Pts',(1.60073511858687,-1.,1.32381550858256));
#25816=CARTESIAN_POINT('Ctrl Pts',(1.59471591079403,-1.,1.32224985747682));
#25817=CARTESIAN_POINT('Ctrl Pts',(1.58872057258245,-1.,1.32064537110892));
#25818=CARTESIAN_POINT('Ctrl Pts',(1.58274907898834,-1.,1.31900135021432));
#25819=CARTESIAN_POINT('Ctrl Pts',(1.5768005650559,-1.,1.31731642317187));
#25820=CARTESIAN_POINT('Ctrl Pts',(1.57087397835723,-1.,1.31558903860016));
#25821=CARTESIAN_POINT('Ctrl Pts',(1.56496872402353,-1.,1.31381795281002));
#25822=CARTESIAN_POINT('Ctrl Pts',(1.55908521254821,-1.,1.31200264341696));
#25823=CARTESIAN_POINT('Ctrl Pts',(1.55322568759481,-1.,1.31014393684222));
#25824=CARTESIAN_POINT('Ctrl Pts',(1.54739413957185,-1.,1.30824393907473));
#25825=CARTESIAN_POINT('Ctrl Pts',(1.54159462645432,-1.,1.30630475189556));
#25826=CARTESIAN_POINT('Ctrl Pts',(1.53582981268977,-1.,1.30432735639489));
#25827=CARTESIAN_POINT('Ctrl Pts',(1.53009970283891,-1.,1.30231064395568));
#25828=CARTESIAN_POINT('Ctrl Pts',(1.52439957861062,-1.,1.30024984366328));
#25829=CARTESIAN_POINT('Ctrl Pts',(1.51872184912724,-1.,1.29813791800747));
#25830=CARTESIAN_POINT('Ctrl Pts',(1.51305994241402,-1.,1.29596850710509));
#25831=CARTESIAN_POINT('Ctrl Pts',(1.50741159078365,-1.,1.29373841372842));
#25832=CARTESIAN_POINT('Ctrl Pts',(1.50178230149776,-1.,1.29145022885181));
#25833=CARTESIAN_POINT('Ctrl Pts',(1.49618896881754,-1.,1.28911506584254));
#25834=CARTESIAN_POINT('Ctrl Pts',(1.4906522831278,-1.,1.2867467611644));
#25835=CARTESIAN_POINT('Ctrl Pts',(1.4851881711891,-1.,1.28435533880201));
#25836=CARTESIAN_POINT('Ctrl Pts',(1.47980070347095,-1.,1.28194158939517));
#25837=CARTESIAN_POINT('Ctrl Pts',(1.4744717526707,-1.,1.2794891824849));
#25838=CARTESIAN_POINT('Ctrl Pts',(1.46916035917133,-1.,1.2769641483109));
#25839=CARTESIAN_POINT('Ctrl Pts',(1.46382431332476,-1.,1.27433119897822));
#25840=CARTESIAN_POINT('Ctrl Pts',(1.45843906294697,-1.,1.27156805265289));
#25841=CARTESIAN_POINT('Ctrl Pts',(1.45301422764247,-1.,1.2686778680489));
#25842=CARTESIAN_POINT('Ctrl Pts',(1.44761985001662,-1.,1.26570925118868));
#25843=CARTESIAN_POINT('Ctrl Pts',(1.44236470511303,-1.,1.26273903323859));
#25844=CARTESIAN_POINT('Ctrl Pts',(1.43734919180847,-1.,1.25983531012005));
#25845=CARTESIAN_POINT('Ctrl Pts',(1.43262645609691,-1.,1.25702687965755));
#25846=CARTESIAN_POINT('Ctrl Pts',(1.42815938799387,-1.,1.25426945222639));
#25847=CARTESIAN_POINT('Ctrl Pts',(1.42378102115575,-1.,1.2514145557001));
#25848=CARTESIAN_POINT('Ctrl Pts',(1.41923722596025,-1.,1.24824430986571));
#25849=CARTESIAN_POINT('Ctrl Pts',(1.41422913175179,-1.,1.24450600513056));
#25850=CARTESIAN_POINT('Ctrl Pts',(1.40845295531283,-1.,1.23994455029534));
#25851=CARTESIAN_POINT('Ctrl Pts',(1.40164708206106,-1.,1.23434087290423));
#25852=CARTESIAN_POINT('Ctrl Pts',(1.39361389568796,-1.,1.22752961899387));
#25853=CARTESIAN_POINT('Ctrl Pts',(1.38420564527715,-1.,1.21938737280852));
#25854=CARTESIAN_POINT('Ctrl Pts',(1.37331915607905,-1.,1.20982812925645));
#25855=CARTESIAN_POINT('Ctrl Pts',(1.36088705043885,-1.,1.1987959077932));
#25856=CARTESIAN_POINT('Ctrl Pts',(1.34687054001093,-1.,1.18625865667441));
#25857=CARTESIAN_POINT('Ctrl Pts',(1.33437539347008,-1.,1.17501305789857));
#25858=CARTESIAN_POINT('Ctrl Pts',(1.32428080721772,-1.,1.16589330093588));
#25859=CARTESIAN_POINT('Ctrl Pts',(1.31722977216397,-1.,1.15950888730809));
#25860=CARTESIAN_POINT('Ctrl Pts',(1.31362392696032,-1.,1.15624053661742));
#25861=CARTESIAN_POINT('',(1.15624053661742,-1.,1.31362392696033));
#25862=CARTESIAN_POINT('Origin',(0.,-1.,0.));
#25863=CARTESIAN_POINT('',(1.34869019493419,-1.,1.73811241238545));
#25864=CARTESIAN_POINT('Ctrl Pts',(1.15624053661742,-1.,1.31362392696033));
#25865=CARTESIAN_POINT('Ctrl Pts',(1.15950888730433,-1.,1.3172297721596));
#25866=CARTESIAN_POINT('Ctrl Pts',(1.16589330092532,-1.,1.32428080720544));
#25867=CARTESIAN_POINT('Ctrl Pts',(1.17501305787994,-1.,1.33437539344842));
#25868=CARTESIAN_POINT('Ctrl Pts',(1.18625865664915,-1.,1.34687053998157));
#25869=CARTESIAN_POINT('Ctrl Pts',(1.1987959077656,-1.,1.36088705040677));
#25870=CARTESIAN_POINT('Ctrl Pts',(1.20982812923113,-1.,1.37331915604962));
#25871=CARTESIAN_POINT('Ctrl Pts',(1.21938737278853,-1.,1.38420564525391));
#25872=CARTESIAN_POINT('Ctrl Pts',(1.22752961898063,-1.,1.39361389567257));
#25873=CARTESIAN_POINT('Ctrl Pts',(1.23434087289768,-1.,1.40164708205345));
#25874=CARTESIAN_POINT('Ctrl Pts',(1.23994455029421,-1.,1.40845295531151));
#25875=CARTESIAN_POINT('Ctrl Pts',(1.24450600513278,-1.,1.41422913175437));
#25876=CARTESIAN_POINT('Ctrl Pts',(1.24824430986911,-1.,1.41923722596421));
#25877=CARTESIAN_POINT('Ctrl Pts',(1.25141455570299,-1.,1.42378102115911));
#25878=CARTESIAN_POINT('Ctrl Pts',(1.25426945222783,-1.,1.42815938799555));
#25879=CARTESIAN_POINT('Ctrl Pts',(1.25702687965744,-1.,1.43262645609679));
#25880=CARTESIAN_POINT('Ctrl Pts',(1.25983531011894,-1.,1.43734919180719));
#25881=CARTESIAN_POINT('Ctrl Pts',(1.26273903323723,-1.,1.44236470511145));
#25882=CARTESIAN_POINT('Ctrl Pts',(1.26570925118767,-1.,1.44761985001544));
#25883=CARTESIAN_POINT('Ctrl Pts',(1.26867786804854,-1.,1.45301422764205));
#25884=CARTESIAN_POINT('Ctrl Pts',(1.27156805265312,-1.,1.45843906294725));
#25885=CARTESIAN_POINT('Ctrl Pts',(1.27433119897877,-1.,1.4638243133254));
#25886=CARTESIAN_POINT('Ctrl Pts',(1.27696414831144,-1.,1.46916035917197));
#25887=CARTESIAN_POINT('Ctrl Pts',(1.27948918248524,-1.,1.4744717526711));
#25888=CARTESIAN_POINT('Ctrl Pts',(1.28194158939522,-1.,1.47980070347102));
#25889=CARTESIAN_POINT('Ctrl Pts',(1.28435533880184,-1.,1.48518817118891));
#25890=CARTESIAN_POINT('Ctrl Pts',(1.28674676116415,-1.,1.4906522831275));
#25891=CARTESIAN_POINT('Ctrl Pts',(1.28911506584232,-1.,1.49618896881729));
#25892=CARTESIAN_POINT('Ctrl Pts',(1.29145022885171,-1.,1.50178230149764));
#25893=CARTESIAN_POINT('Ctrl Pts',(1.29373841372843,-1.,1.50741159078367));
#25894=CARTESIAN_POINT('Ctrl Pts',(1.29596850710518,-1.,1.51305994241412));
#25895=CARTESIAN_POINT('Ctrl Pts',(1.29813791800757,-1.,1.51872184912735));
#25896=CARTESIAN_POINT('Ctrl Pts',(1.30024984366334,-1.,1.5243995786107));
#25897=CARTESIAN_POINT('Ctrl Pts',(1.3023106439557,-1.,1.53009970283893));
#25898=CARTESIAN_POINT('Ctrl Pts',(1.30432735639487,-1.,1.53582981268976));
#25899=CARTESIAN_POINT('Ctrl Pts',(1.30630475189553,-1.,1.54159462645428));
#25900=CARTESIAN_POINT('Ctrl Pts',(1.30824393907471,-1.,1.54739413957183));
#25901=CARTESIAN_POINT('Ctrl Pts',(1.31014393684221,-1.,1.55322568759481));
#25902=CARTESIAN_POINT('Ctrl Pts',(1.31200264341696,-1.,1.55908521254822));
#25903=CARTESIAN_POINT('Ctrl Pts',(1.31381795281002,-1.,1.56496872402352));
#25904=CARTESIAN_POINT('Ctrl Pts',(1.31558903860015,-1.,1.57087397835721));
#25905=CARTESIAN_POINT('Ctrl Pts',(1.31731642317183,-1.,1.57680056505585));
#25906=CARTESIAN_POINT('Ctrl Pts',(1.31900135021428,-1.,1.58274907898829));
#25907=CARTESIAN_POINT('Ctrl Pts',(1.32064537110891,-1.,1.58872057258244));
#25908=CARTESIAN_POINT('Ctrl Pts',(1.32224985747686,-1.,1.59471591079408));
#25909=CARTESIAN_POINT('Ctrl Pts',(1.32381550858266,-1.,1.600735118587));
#25910=CARTESIAN_POINT('Ctrl Pts',(1.32534250785794,-1.,1.6067775829097));
#25911=CARTESIAN_POINT('Ctrl Pts',(1.32683074483365,-1.,1.61284234015762));
#25912=CARTESIAN_POINT('Ctrl Pts',(1.32828000610448,-1.,1.61892832270723));
#25913=CARTESIAN_POINT('Ctrl Pts',(1.32969019505665,-1.,1.62503464209777));
#25914=CARTESIAN_POINT('Ctrl Pts',(1.33106149345618,-1.,1.63116079730887));
#25915=CARTESIAN_POINT('Ctrl Pts',(1.33239425103694,-1.,1.6373065347505));
#25916=CARTESIAN_POINT('Ctrl Pts',(1.33368890676554,-1.,1.64347174856007));
#25917=CARTESIAN_POINT('Ctrl Pts',(1.33494590468003,-1.,1.64965637286843));
#25918=CARTESIAN_POINT('Ctrl Pts',(1.33616559745217,-1.,1.65586025952651));
#25919=CARTESIAN_POINT('Ctrl Pts',(1.33734820885331,-1.,1.66208312542073));
#25920=CARTESIAN_POINT('Ctrl Pts',(1.33849388654458,-1.,1.66832460784078));
#25921=CARTESIAN_POINT('Ctrl Pts',(1.33960273470372,-1.,1.67458429426126));
#25922=CARTESIAN_POINT('Ctrl Pts',(1.3406748518516,-1.,1.68086176030308));
#25923=CARTESIAN_POINT('Ctrl Pts',(1.34171037484673,-1.,1.68715660868602));
#25924=CARTESIAN_POINT('Ctrl Pts',(1.34270948206139,-1.,1.6934684849664));
#25925=CARTESIAN_POINT('Ctrl Pts',(1.34367237124322,-1.,1.69979707754221));
#25926=CARTESIAN_POINT('Ctrl Pts',(1.34459924533783,-1.,1.70614212266676));
#25927=CARTESIAN_POINT('Ctrl Pts',(1.34549029589563,-1.,1.71250340687011));
#25928=CARTESIAN_POINT('Ctrl Pts',(1.34634568653586,-1.,1.7188807715095));
#25929=CARTESIAN_POINT('Ctrl Pts',(1.34716554820013,-1.,1.72527410681298));
#25930=CARTESIAN_POINT('Ctrl Pts',(1.3477930915247,-1.,1.73040149654497));
#25931=CARTESIAN_POINT('Ctrl Pts',(1.34824783113158,-1.,1.73425417886255));
#25932=CARTESIAN_POINT('Ctrl Pts',(1.34854391898145,-1.,1.73682580585819));
#25933=CARTESIAN_POINT('Ctrl Pts',(1.34869019493419,-1.,1.73811241238545));
#25934=CARTESIAN_POINT('',(1.23627494547115,-1.,1.81978687191668));
#25935=CARTESIAN_POINT('',(1.34869019493419,-1.,1.73811241238545));
#25936=CARTESIAN_POINT('',(0.892032620296855,-1.,1.5055822144029));
#25937=CARTESIAN_POINT('Ctrl Pts',(1.23627494547115,-1.,1.81978687191668));
#25938=CARTESIAN_POINT('Ctrl Pts',(1.23509651170384,-1.,1.81925017193531));
#25939=CARTESIAN_POINT('Ctrl Pts',(1.23274224526804,-1.,1.81817389920914));
#25940=CARTESIAN_POINT('Ctrl Pts',(1.22921864890975,-1.,1.81655087183054));
#25941=CARTESIAN_POINT('Ctrl Pts',(1.22453613304507,-1.,1.81436959209778));
#25942=CARTESIAN_POINT('Ctrl Pts',(1.2187090610323,-1.,1.81161420806172));
#25943=CARTESIAN_POINT('Ctrl Pts',(1.2129081570818,-1.,1.80882996916931));
#25944=CARTESIAN_POINT('Ctrl Pts',(1.20713356605519,-1.,1.80601678480772));
#25945=CARTESIAN_POINT('Ctrl Pts',(1.2013854893912,-1.,1.8031745483882));
#25946=CARTESIAN_POINT('Ctrl Pts',(1.19566418930405,-1.,1.80030314370121));
#25947=CARTESIAN_POINT('Ctrl Pts',(1.1899699793456,-1.,1.79740245923649));
#25948=CARTESIAN_POINT('Ctrl Pts',(1.18430321697471,-1.,1.79447240321572));
#25949=CARTESIAN_POINT('Ctrl Pts',(1.17866429440781,-1.,1.79151291552646));
#25950=CARTESIAN_POINT('Ctrl Pts',(1.17305363177265,-1.,1.78852398877523));
#25951=CARTESIAN_POINT('Ctrl Pts',(1.16747166312239,-1.,1.78550566040349));
#25952=CARTESIAN_POINT('Ctrl Pts',(1.16191881298458,-1.,1.78245795880949));
#25953=CARTESIAN_POINT('Ctrl Pts',(1.15639547194689,-1.,1.77938085564261));
#25954=CARTESIAN_POINT('Ctrl Pts',(1.15090197841531,-1.,1.77627422557034));
#25955=CARTESIAN_POINT('Ctrl Pts',(1.14543858226948,-1.,1.77313777896234));
#25956=CARTESIAN_POINT('Ctrl Pts',(1.14000548337,-1.,1.76997111386806));
#25957=CARTESIAN_POINT('Ctrl Pts',(1.13460291804634,-1.,1.76677384551883));
#25958=CARTESIAN_POINT('Ctrl Pts',(1.12923123555076,-1.,1.76354571966171));
#25959=CARTESIAN_POINT('Ctrl Pts',(1.12389096855078,-1.,1.76028671825084));
#25960=CARTESIAN_POINT('Ctrl Pts',(1.11858293216752,-1.,1.75699720772089));
#25961=CARTESIAN_POINT('Ctrl Pts',(1.11330807582542,-1.,1.75367772094617));
#25962=CARTESIAN_POINT('Ctrl Pts',(1.10806728183003,-1.,1.75032866075914));
#25963=CARTESIAN_POINT('Ctrl Pts',(1.10286118991144,-1.,1.74695004214924));
#25964=CARTESIAN_POINT('Ctrl Pts',(1.09768999241229,-1.,1.74354119236212));
#25965=CARTESIAN_POINT('Ctrl Pts',(1.09255329056496,-1.,1.74010053962252));
#25966=CARTESIAN_POINT('Ctrl Pts',(1.08745056285429,-1.,1.73662628326093));
#25967=CARTESIAN_POINT('Ctrl Pts',(1.08238162784749,-1.,1.73311705663407));
#25968=CARTESIAN_POINT('Ctrl Pts',(1.0773470373727,-1.,1.72957248977424));
#25969=CARTESIAN_POINT('Ctrl Pts',(1.07234866990252,-1.,1.72599406198489));
#25970=CARTESIAN_POINT('Ctrl Pts',(1.06738966975463,-1.,1.72238500928456));
#25971=CARTESIAN_POINT('Ctrl Pts',(1.06247324680649,-1.,1.71874858456908));
#25972=CARTESIAN_POINT('Ctrl Pts',(1.05760163192481,-1.,1.71508654427022));
#25973=CARTESIAN_POINT('Ctrl Pts',(1.05277517202853,-1.,1.71139783543986));
#25974=CARTESIAN_POINT('Ctrl Pts',(1.0479908540499,-1.,1.70767646263641));
#25975=CARTESIAN_POINT('Ctrl Pts',(1.04324363334546,-1.,1.70391338707969));
#25976=CARTESIAN_POINT('Ctrl Pts',(1.03852922490782,-1.,1.70010052930951));
#25977=CARTESIAN_POINT('Ctrl Pts',(1.03384646003587,-1.,1.69623414782769));
#25978=CARTESIAN_POINT('Ctrl Pts',(1.02919977579155,-1.,1.69231840863471));
#25979=CARTESIAN_POINT('Ctrl Pts',(1.02460180535272,-1.,1.68836910178475));
#25980=CARTESIAN_POINT('Ctrl Pts',(1.02006795074222,-1.,1.68440578021739));
#25981=CARTESIAN_POINT('Ctrl Pts',(1.01561026162786,-1.,1.6804428989482));
#25982=CARTESIAN_POINT('Ctrl Pts',(1.01123236493507,-1.,1.67648246776457));
#25983=CARTESIAN_POINT('Ctrl Pts',(1.00692206696387,-1.,1.67250335383248));
#25984=CARTESIAN_POINT('Ctrl Pts',(1.00265091003682,-1.,1.66846059277231));
#25985=CARTESIAN_POINT('Ctrl Pts',(0.998389654952317,-1.,1.66430758030304));
#25986=CARTESIAN_POINT('Ctrl Pts',(0.994121836661115,-1.,1.66001553809916));
#25987=CARTESIAN_POINT('Ctrl Pts',(0.98985562785445,-1.,1.65559044289746));
#25988=CARTESIAN_POINT('Ctrl Pts',(0.985642622921626,-1.,1.6511001661277));
#25989=CARTESIAN_POINT('Ctrl Pts',(0.981562530940574,-1.,1.64665139190834));
#25990=CARTESIAN_POINT('Ctrl Pts',(0.977689794120296,-1.,1.64233990826831));
#25991=CARTESIAN_POINT('Ctrl Pts',(0.974066058287501,-1.,1.63820952658157));
#25992=CARTESIAN_POINT('Ctrl Pts',(0.970669715996356,-1.,1.63420665729609));
#25993=CARTESIAN_POINT('Ctrl Pts',(0.967387853228041,-1.,1.63013849959083));
#25994=CARTESIAN_POINT('Ctrl Pts',(0.964046107037821,-1.,1.6257193066974));
#25995=CARTESIAN_POINT('Ctrl Pts',(0.960438326099958,-1.,1.62061638139929));
#25996=CARTESIAN_POINT('Ctrl Pts',(0.956354422921572,-1.,1.61449324337233));
#25997=CARTESIAN_POINT('Ctrl Pts',(0.951613284361247,-1.,1.60706069897794));
#25998=CARTESIAN_POINT('Ctrl Pts',(0.946078063325795,-1.,1.59810042045408));
#25999=CARTESIAN_POINT('Ctrl Pts',(0.939646377909319,-1.,1.58744937489796));
#26000=CARTESIAN_POINT('Ctrl Pts',(0.932246680128848,-1.,1.57499388385561));
#26001=CARTESIAN_POINT('Ctrl Pts',(0.923832188966322,-1.,1.56065988582509));
#26002=CARTESIAN_POINT('Ctrl Pts',(0.914375919046579,-1.,1.54440491152808));
#26003=CARTESIAN_POINT('Ctrl Pts',(0.905967409640498,-1.,1.52984849890434));
#26004=CARTESIAN_POINT('Ctrl Pts',(0.89918504749193,-1.,1.51805569591479));
#26005=CARTESIAN_POINT('Ctrl Pts',(0.894452006967538,-1.,1.50980486807181));
#26006=CARTESIAN_POINT('Ctrl Pts',(0.892032620296855,-1.,1.5055822144029));
#26007=CARTESIAN_POINT('',(0.693717979106305,-1.,1.60662857109684));
#26008=CARTESIAN_POINT('Origin',(0.,-1.,0.));
#26009=CARTESIAN_POINT('',(0.7455743247944,-1.,2.0698113262342));
#26010=CARTESIAN_POINT('Ctrl Pts',(0.693717979106305,-1.,1.60662857109684));
#26011=CARTESIAN_POINT('Ctrl Pts',(0.69571209787897,-1.,1.61106790957619));
#26012=CARTESIAN_POINT('Ctrl Pts',(0.699605146398836,-1.,1.61974673471117));
#26013=CARTESIAN_POINT('Ctrl Pts',(0.705159151977294,-1.,1.6321654166204));
#26014=CARTESIAN_POINT('Ctrl Pts',(0.711993139340447,-1.,1.64752408828442));
#26015=CARTESIAN_POINT('Ctrl Pts',(0.719585433787949,-1.,1.66472880551777));
#26016=CARTESIAN_POINT('Ctrl Pts',(0.726235967982445,-1.,1.67996158451922));
#26017=CARTESIAN_POINT('Ctrl Pts',(0.731963238685357,-1.,1.69326921972915));
#26018=CARTESIAN_POINT('Ctrl Pts',(0.736799665716932,-1.,1.70473309004249));
#26019=CARTESIAN_POINT('Ctrl Pts',(0.74079516202821,-1.,1.71447789751001));
#26020=CARTESIAN_POINT('Ctrl Pts',(0.744021445433093,-1.,1.72268229916769));
#26021=CARTESIAN_POINT('Ctrl Pts',(0.746574710097752,-1.,1.72958533647714));
#26022=CARTESIAN_POINT('Ctrl Pts',(0.74858246295687,-1.,1.7355035168033));
#26023=CARTESIAN_POINT('Ctrl Pts',(0.750193435981249,-1.,1.74080458267114));
#26024=CARTESIAN_POINT('Ctrl Pts',(0.751555614164482,-1.,1.74585086852502));
#26025=CARTESIAN_POINT('Ctrl Pts',(0.752797683531314,-1.,1.75095139468794));
#26026=CARTESIAN_POINT('Ctrl Pts',(0.754009254027828,-1.,1.75631083600019));
#26027=CARTESIAN_POINT('Ctrl Pts',(0.755220979974461,-1.,1.76197817240128));
#26028=CARTESIAN_POINT('Ctrl Pts',(0.75642189602781,-1.,1.76789396002998));
#26029=CARTESIAN_POINT('Ctrl Pts',(0.757578264077028,-1.,1.77394167108292));
#26030=CARTESIAN_POINT('Ctrl Pts',(0.758650626677518,-1.,1.77999411220945));
#26031=CARTESIAN_POINT('Ctrl Pts',(0.759614401110189,-1.,1.78596964884604));
#26032=CARTESIAN_POINT('Ctrl Pts',(0.760469555880749,-1.,1.7918581561088));
#26033=CARTESIAN_POINT('Ctrl Pts',(0.761229695230558,-1.,1.79768986997783));
#26034=CARTESIAN_POINT('Ctrl Pts',(0.761915336443547,-1.,1.80351583877342));
#26035=CARTESIAN_POINT('Ctrl Pts',(0.762546129463938,-1.,1.80938551463965));
#26036=CARTESIAN_POINT('Ctrl Pts',(0.763132003836634,-1.,1.8153211840553));
#26037=CARTESIAN_POINT('Ctrl Pts',(0.763673465462726,-1.,1.82131873145266));
#26038=CARTESIAN_POINT('Ctrl Pts',(0.764165902605995,-1.,1.82735991200065));
#26039=CARTESIAN_POINT('Ctrl Pts',(0.764602549687853,-1.,1.83342077227142));
#26040=CARTESIAN_POINT('Ctrl Pts',(0.764978057881737,-1.,1.83948181064835));
#26041=CARTESIAN_POINT('Ctrl Pts',(0.765291664862029,-1.,1.84553698875924));
#26042=CARTESIAN_POINT('Ctrl Pts',(0.765545710619062,-1.,1.85158945130063));
#26043=CARTESIAN_POINT('Ctrl Pts',(0.765744212909318,-1.,1.85764741390394));
#26044=CARTESIAN_POINT('Ctrl Pts',(0.765891519092547,-1.,1.86372027063312));
#26045=CARTESIAN_POINT('Ctrl Pts',(0.765990708546091,-1.,1.86981398314341));
#26046=CARTESIAN_POINT('Ctrl Pts',(0.766042837036744,-1.,1.87592888967883));
#26047=CARTESIAN_POINT('Ctrl Pts',(0.766047794851864,-1.,1.88206215302561));
#26048=CARTESIAN_POINT('Ctrl Pts',(0.766004837062091,-1.,1.88820926433409));
#26049=CARTESIAN_POINT('Ctrl Pts',(0.765913193856978,-1.,1.89436577771388));
#26050=CARTESIAN_POINT('Ctrl Pts',(0.765772772593386,-1.,1.90052930393596));
#26051=CARTESIAN_POINT('Ctrl Pts',(0.765584196937919,-1.,1.90669961402356));
#26052=CARTESIAN_POINT('Ctrl Pts',(0.765348465884722,-1.,1.91287765805169));
#26053=CARTESIAN_POINT('Ctrl Pts',(0.765066729667088,-1.,1.91906491634196));
#26054=CARTESIAN_POINT('Ctrl Pts',(0.764740025488211,-1.,1.92526263537048));
#26055=CARTESIAN_POINT('Ctrl Pts',(0.76436901067394,-1.,1.93147105496382));
#26056=CARTESIAN_POINT('Ctrl Pts',(0.763954049121458,-1.,1.93768964875886));
#26057=CARTESIAN_POINT('Ctrl Pts',(0.763495333538629,-1.,1.9439174661764));
#26058=CARTESIAN_POINT('Ctrl Pts',(0.762992990878769,-1.,1.95015342590024));
#26059=CARTESIAN_POINT('Ctrl Pts',(0.762447203806178,-1.,1.95639665309869));
#26060=CARTESIAN_POINT('Ctrl Pts',(0.761858300014423,-1.,1.96264672744186));
#26061=CARTESIAN_POINT('Ctrl Pts',(0.76122669048382,-1.,1.96890351582499));
#26062=CARTESIAN_POINT('Ctrl Pts',(0.760552825409757,-1.,1.97516705321494));
#26063=CARTESIAN_POINT('Ctrl Pts',(0.75983714745219,-1.,1.98143741418172));
#26064=CARTESIAN_POINT('Ctrl Pts',(0.759080037802488,-1.,1.98771456680874));
#26065=CARTESIAN_POINT('Ctrl Pts',(0.758281796766761,-1.,1.99399831098817));
#26066=CARTESIAN_POINT('Ctrl Pts',(0.757442676862724,-1.,2.00028834739178));
#26067=CARTESIAN_POINT('Ctrl Pts',(0.75656290464667,-1.,2.0065843158773));
#26068=CARTESIAN_POINT('Ctrl Pts',(0.755642704957865,-1.,2.01288584328084));
#26069=CARTESIAN_POINT('Ctrl Pts',(0.754682330722816,-1.,2.01919259405809));
#26070=CARTESIAN_POINT('Ctrl Pts',(0.753682061112768,-1.,2.02550428623313));
#26071=CARTESIAN_POINT('Ctrl Pts',(0.75264218048721,-1.,2.03182068456221));
#26072=CARTESIAN_POINT('Ctrl Pts',(0.751562963361115,-1.,2.03814160092099));
#26073=CARTESIAN_POINT('Ctrl Pts',(0.750444657875575,-1.,2.04446689147979));
#26074=CARTESIAN_POINT('Ctrl Pts',(0.749287468665046,-1.,2.05079645592154));
#26075=CARTESIAN_POINT('Ctrl Pts',(0.748091554183802,-1.,2.05713023031007));
#26076=CARTESIAN_POINT('Ctrl Pts',(0.747103932787919,-1.,2.06220058927826));
#26077=CARTESIAN_POINT('Ctrl Pts',(0.7463458715442,-1.,2.06600523016815));
#26078=CARTESIAN_POINT('Ctrl Pts',(0.745832791378367,-1.,2.06854248895728));
#26079=CARTESIAN_POINT('Ctrl Pts',(0.7455743247944,-1.,2.0698113262342));
#26080=CARTESIAN_POINT('',(0.61342227326009,-1.,2.11275013067528));
#26081=CARTESIAN_POINT('',(0.7455743247944,-1.,2.0698113262342));
#26082=CARTESIAN_POINT('',(0.383122945602004,-1.,1.7075470150345));
#26083=CARTESIAN_POINT('Ctrl Pts',(0.61342227326009,-1.,2.11275013067528));
#26084=CARTESIAN_POINT('Ctrl Pts',(0.6124673655618,-1.,2.11187554259986));
#26085=CARTESIAN_POINT('Ctrl Pts',(0.610560911689898,-1.,2.11012443807238));
#26086=CARTESIAN_POINT('Ctrl Pts',(0.607711315454876,-1.,2.1074919961518));
#26087=CARTESIAN_POINT('Ctrl Pts',(0.60393203073603,-1.,2.10397049886949));
#26088=CARTESIAN_POINT('Ctrl Pts',(0.599241616420533,-1.,2.0995493086477));
#26089=CARTESIAN_POINT('Ctrl Pts',(0.594585006052162,-1.,2.0951087622027));
#26090=CARTESIAN_POINT('Ctrl Pts',(0.589962365403406,-1.,2.09064881812129));
#26091=CARTESIAN_POINT('Ctrl Pts',(0.585373918991617,-1.,2.08616943727951));
#26092=CARTESIAN_POINT('Ctrl Pts',(0.580819952108063,-1.,2.08167059018418));
#26093=CARTESIAN_POINT('Ctrl Pts',(0.576300797416844,-1.,2.07715226767559));
#26094=CARTESIAN_POINT('Ctrl Pts',(0.571816823242602,-1.,2.07261449292824));
#26095=CARTESIAN_POINT('Ctrl Pts',(0.567368421181087,-1.,2.06805732997334));
#26096=CARTESIAN_POINT('Ctrl Pts',(0.562955993082261,-1.,2.06348090160589));
#26097=CARTESIAN_POINT('Ctrl Pts',(0.558579940185151,-1.,2.05888537756462));
#26098=CARTESIAN_POINT('Ctrl Pts',(0.554240657463906,-1.,2.05427091604413));
#26099=CARTESIAN_POINT('Ctrl Pts',(0.549938525150295,-1.,2.04963761077958));
#26100=CARTESIAN_POINT('Ctrl Pts',(0.54567390381743,-1.,2.04498544714588));
#26101=CARTESIAN_POINT('Ctrl Pts',(0.541447120615659,-1.,2.04031422690527));
#26102=CARTESIAN_POINT('Ctrl Pts',(0.537258489833262,-1.,2.03562362954037));
#26103=CARTESIAN_POINT('Ctrl Pts',(0.533108355132976,-1.,2.03091336214426));
#26104=CARTESIAN_POINT('Ctrl Pts',(0.528997127241914,-1.,2.0261832908329));
#26105=CARTESIAN_POINT('Ctrl Pts',(0.524925318333476,-1.,2.02143356304698));
#26106=CARTESIAN_POINT('Ctrl Pts',(0.52089359039937,-1.,2.01666477917286));
#26107=CARTESIAN_POINT('Ctrl Pts',(0.516902681728687,-1.,2.01187773939242));
#26108=CARTESIAN_POINT('Ctrl Pts',(0.512953306961792,-1.,2.00707309946949));
#26109=CARTESIAN_POINT('Ctrl Pts',(0.509046069886157,-1.,2.00225107134734));
#26110=CARTESIAN_POINT('Ctrl Pts',(0.505181361323026,-1.,1.99741107463572));
#26111=CARTESIAN_POINT('Ctrl Pts',(0.501359287727146,-1.,1.99255149126155));
#26112=CARTESIAN_POINT('Ctrl Pts',(0.497579909545574,-1.,1.98767044752932));
#26113=CARTESIAN_POINT('Ctrl Pts',(0.493843476541494,-1.,1.98276658761821));
#26114=CARTESIAN_POINT('Ctrl Pts',(0.490150627860952,-1.,1.97783973019229));
#26115=CARTESIAN_POINT('Ctrl Pts',(0.486502692907658,-1.,1.97289186263272));
#26116=CARTESIAN_POINT('Ctrl Pts',(0.48290166212069,-1.,1.96792703422362));
#26117=CARTESIAN_POINT('Ctrl Pts',(0.479349583074855,-1.,1.96294933055943));
#26118=CARTESIAN_POINT('Ctrl Pts',(0.475848034683176,-1.,1.95796111148177));
#26119=CARTESIAN_POINT('Ctrl Pts',(0.472397672264072,-1.,1.95296148278133));
#26120=CARTESIAN_POINT('Ctrl Pts',(0.468997482913135,-1.,1.94794381136514));
#26121=CARTESIAN_POINT('Ctrl Pts',(0.46564546202603,-1.,1.9428979419619));
#26122=CARTESIAN_POINT('Ctrl Pts',(0.462340031009056,-1.,1.93781486640821));
#26123=CARTESIAN_POINT('Ctrl Pts',(0.459081234547926,-1.,1.93269066517934));
#26124=CARTESIAN_POINT('Ctrl Pts',(0.45587200517437,-1.,1.92753067150476));
#26125=CARTESIAN_POINT('Ctrl Pts',(0.452719478359432,-1.,1.92235380648502));
#26126=CARTESIAN_POINT('Ctrl Pts',(0.449632260106662,-1.,1.91718342555755));
#26127=CARTESIAN_POINT('Ctrl Pts',(0.446617343485711,-1.,1.9120369998112));
#26128=CARTESIAN_POINT('Ctrl Pts',(0.44367755684915,-1.,1.90691756144898));
#26129=CARTESIAN_POINT('Ctrl Pts',(0.440807833704038,-1.,1.90180124389086));
#26130=CARTESIAN_POINT('Ctrl Pts',(0.437995003948244,-1.,1.89663648956466));
#26131=CARTESIAN_POINT('Ctrl Pts',(0.435225660963383,-1.,1.89136993975504));
#26132=CARTESIAN_POINT('Ctrl Pts',(0.432493038548748,-1.,1.88596913666793));
#26133=CARTESIAN_POINT('Ctrl Pts',(0.429803062482344,-1.,1.88044229001832));
#26134=CARTESIAN_POINT('Ctrl Pts',(0.427183828519102,-1.,1.87486989291484));
#26135=CARTESIAN_POINT('Ctrl Pts',(0.424678177291358,-1.,1.86937803944323));
#26136=CARTESIAN_POINT('Ctrl Pts',(0.422327307418275,-1.,1.86408083334028));
#26137=CARTESIAN_POINT('Ctrl Pts',(0.420157287975619,-1.,1.85903281096686));
#26138=CARTESIAN_POINT('Ctrl Pts',(0.418164129143534,-1.,1.85417632856234));
#26139=CARTESIAN_POINT('Ctrl Pts',(0.416300022038864,-1.,1.84929312929882));
#26140=CARTESIAN_POINT('Ctrl Pts',(0.41448743825434,-1.,1.8440575707371));
#26141=CARTESIAN_POINT('Ctrl Pts',(0.412633125322161,-1.,1.83808953475839));
#26142=CARTESIAN_POINT('Ctrl Pts',(0.410641256301674,-1.,1.83100408895216));
#26143=CARTESIAN_POINT('Ctrl Pts',(0.408428948108533,-1.,1.8224702267854));
#26144=CARTESIAN_POINT('Ctrl Pts',(0.405933518411838,-1.,1.81223801813988));
#26145=CARTESIAN_POINT('Ctrl Pts',(0.403107976170441,-1.,1.80012077176221));
#26146=CARTESIAN_POINT('Ctrl Pts',(0.39991940378308,-1.,1.78598826347533));
#26147=CARTESIAN_POINT('Ctrl Pts',(0.39634619612042,-1.,1.7697556004756));
#26148=CARTESIAN_POINT('Ctrl Pts',(0.392375812294307,-1.,1.75137405313962));
#26149=CARTESIAN_POINT('Ctrl Pts',(0.388877023509191,-1.,1.7349317097561));
#26150=CARTESIAN_POINT('Ctrl Pts',(0.38607079032701,-1.,1.72162022246158));
#26151=CARTESIAN_POINT('Ctrl Pts',(0.384119047315541,-1.,1.71231062891958));
#26152=CARTESIAN_POINT('Ctrl Pts',(0.383122945602004,-1.,1.7075470150345));
#26153=CARTESIAN_POINT('',(0.163289472382896,-1.,1.74236521665491));
#26154=CARTESIAN_POINT('Origin',(0.,-1.,0.));
#26155=CARTESIAN_POINT('',(0.0694764450219578,-1.,2.19890268624765));
#26156=CARTESIAN_POINT('Ctrl Pts',(0.163289472382896,-1.,1.74236521665491));
#26157=CARTESIAN_POINT('Ctrl Pts',(0.163814161002002,-1.,1.7472034950333));
#26158=CARTESIAN_POINT('Ctrl Pts',(0.164834765707158,-1.,1.75666056638427));
#26159=CARTESIAN_POINT('Ctrl Pts',(0.1662793551464,-1.,1.77018771684844));
#26160=CARTESIAN_POINT('Ctrl Pts',(0.168032772805197,-1.,1.7869064998507));
#26161=CARTESIAN_POINT('Ctrl Pts',(0.169936923904608,-1.,1.80561530629706));
#26162=CARTESIAN_POINT('Ctrl Pts',(0.171554770204119,-1.,1.82215766811545));
#26163=CARTESIAN_POINT('Ctrl Pts',(0.1728894428919,-1.,1.83658380527692));
#26164=CARTESIAN_POINT('Ctrl Pts',(0.173946627587731,-1.,1.8489811319852));
#26165=CARTESIAN_POINT('Ctrl Pts',(0.17473525927603,-1.,1.85948367088837));
#26166=CARTESIAN_POINT('Ctrl Pts',(0.175268337590757,-1.,1.86828349694799));
#26167=CARTESIAN_POINT('Ctrl Pts',(0.175563480746485,-1.,1.87563767773588));
#26168=CARTESIAN_POINT('Ctrl Pts',(0.175644148889698,-1.,1.88188663145367));
#26169=CARTESIAN_POINT('Ctrl Pts',(0.175538155840648,-1.,1.88742606273259));
#26170=CARTESIAN_POINT('Ctrl Pts',(0.175274276190844,-1.,1.892646301985));
#26171=CARTESIAN_POINT('Ctrl Pts',(0.174879405091263,-1.,1.89788101117132));
#26172=CARTESIAN_POINT('Ctrl Pts',(0.174375518661085,-1.,1.90335253862834));
#26173=CARTESIAN_POINT('Ctrl Pts',(0.173776635257816,-1.,1.90911693975267));
#26174=CARTESIAN_POINT('Ctrl Pts',(0.173090695383496,-1.,1.91511429159527));
#26175=CARTESIAN_POINT('Ctrl Pts',(0.172321621259513,-1.,1.9212233439798));
#26176=CARTESIAN_POINT('Ctrl Pts',(0.171471191532988,-1.,1.92731093582036));
#26177=CARTESIAN_POINT('Ctrl Pts',(0.170541253116201,-1.,1.93329183155539));
#26178=CARTESIAN_POINT('Ctrl Pts',(0.16953490481749,-1.,1.93915639211581));
#26179=CARTESIAN_POINT('Ctrl Pts',(0.168455741607556,-1.,1.94493757756931));
#26180=CARTESIAN_POINT('Ctrl Pts',(0.167307501784475,-1.,1.95069027794294));
#26181=CARTESIAN_POINT('Ctrl Pts',(0.166093592002812,-1.,1.9564675971873));
#26182=CARTESIAN_POINT('Ctrl Pts',(0.164816568920269,-1.,1.96229379940136));
#26183=CARTESIAN_POINT('Ctrl Pts',(0.163478185457734,-1.,1.96816512677967));
#26184=CARTESIAN_POINT('Ctrl Pts',(0.162079693556288,-1.,1.97406280235188));
#26185=CARTESIAN_POINT('Ctrl Pts',(0.160622060784611,-1.,1.97996195437559));
#26186=CARTESIAN_POINT('Ctrl Pts',(0.159106226437299,-1.,1.98584238283292));
#26187=CARTESIAN_POINT('Ctrl Pts',(0.157533331459227,-1.,1.99169810931908));
#26188=CARTESIAN_POINT('Ctrl Pts',(0.155904629548783,-1.,1.99753284771497));
#26189=CARTESIAN_POINT('Ctrl Pts',(0.154221403049722,-1.,2.00335565310543));
#26190=CARTESIAN_POINT('Ctrl Pts',(0.152484883621449,-1.,2.00917680318424));
#26191=CARTESIAN_POINT('Ctrl Pts',(0.150696157673078,-1.,2.01500291940238));
#26192=CARTESIAN_POINT('Ctrl Pts',(0.148856124775337,-1.,2.02083464969894));
#26193=CARTESIAN_POINT('Ctrl Pts',(0.146965557332583,-1.,2.02666926182017));
#26194=CARTESIAN_POINT('Ctrl Pts',(0.145025140186057,-1.,2.03250223739942));
#26195=CARTESIAN_POINT('Ctrl Pts',(0.143035515058208,-1.,2.03832911025912));
#26196=CARTESIAN_POINT('Ctrl Pts',(0.140997332152546,-1.,2.04414757947916));
#26197=CARTESIAN_POINT('Ctrl Pts',(0.138911255368966,-1.,2.04995762001328));
#26198=CARTESIAN_POINT('Ctrl Pts',(0.136777941218043,-1.,2.05576044414264));
#26199=CARTESIAN_POINT('Ctrl Pts',(0.134598026192106,-1.,2.06155781517842));
#26200=CARTESIAN_POINT('Ctrl Pts',(0.13237211154771,-1.,2.06735123910326));
#26201=CARTESIAN_POINT('Ctrl Pts',(0.130100748328403,-1.,2.07314114713063));
#26202=CARTESIAN_POINT('Ctrl Pts',(0.12778444527612,-1.,2.07892715110987));
#26203=CARTESIAN_POINT('Ctrl Pts',(0.125423679412061,-1.,2.08470840653643));
#26204=CARTESIAN_POINT('Ctrl Pts',(0.123018905621083,-1.,2.09048392424825));
#26205=CARTESIAN_POINT('Ctrl Pts',(0.120570567965122,-1.,2.0962529286773));
#26206=CARTESIAN_POINT('Ctrl Pts',(0.118079107988355,-1.,2.102015121329));
#26207=CARTESIAN_POINT('Ctrl Pts',(0.115544957687926,-1.,2.10777050261309));
#26208=CARTESIAN_POINT('Ctrl Pts',(0.112968534419737,-1.,2.11351924490306));
#26209=CARTESIAN_POINT('Ctrl Pts',(0.110350236135025,-1.,2.11926155590865));
#26210=CARTESIAN_POINT('Ctrl Pts',(0.10769043523109,-1.,2.12499752307));
#26211=CARTESIAN_POINT('Ctrl Pts',(0.104989479152739,-1.,2.13072704887293));
#26212=CARTESIAN_POINT('Ctrl Pts',(0.1022477005561,-1.,2.13644992667165));
#26213=CARTESIAN_POINT('Ctrl Pts',(0.0994654261990913,-1.,2.14216588396025));
#26214=CARTESIAN_POINT('Ctrl Pts',(0.0966429852305456,-1.,2.14787463531795));
#26215=CARTESIAN_POINT('Ctrl Pts',(0.0937807218867641,-1.,2.1535759397817));
#26216=CARTESIAN_POINT('Ctrl Pts',(0.0908789888107263,-1.,2.15926961544516));
#26217=CARTESIAN_POINT('Ctrl Pts',(0.087938129138692,-1.,2.16495552645014));
#26218=CARTESIAN_POINT('Ctrl Pts',(0.084958462083537,-1.,2.17063357870952));
#26219=CARTESIAN_POINT('Ctrl Pts',(0.0819402680872763,-1.,2.176303712113));
#26220=CARTESIAN_POINT('Ctrl Pts',(0.078883772768524,-1.,2.18196589448887));
#26221=CARTESIAN_POINT('Ctrl Pts',(0.0757891465836145,-1.,2.1876201139953));
#26222=CARTESIAN_POINT('Ctrl Pts',(0.0732830357306722,-1.,2.19213712013662));
#26223=CARTESIAN_POINT('Ctrl Pts',(0.0713863779526151,-1.,2.19552129484002));
#26224=CARTESIAN_POINT('Ctrl Pts',(0.0701143536325487,-1.,2.19777582085423));
#26225=CARTESIAN_POINT('Ctrl Pts',(0.0694764450219578,-1.,2.19890268624765));
#26226=CARTESIAN_POINT('',(-0.0694764450219586,-1.,2.19890268624765));
#26227=CARTESIAN_POINT('',(0.0694764450219578,-1.,2.19890268624765));
#26228=CARTESIAN_POINT('',(-0.163289472382896,-1.,1.74236521665491));
#26229=CARTESIAN_POINT('Ctrl Pts',(-0.0694764450219586,-1.,2.19890268624765));
#26230=CARTESIAN_POINT('Ctrl Pts',(-0.0701143536324929,-1.,2.19777582085261));
#26231=CARTESIAN_POINT('Ctrl Pts',(-0.071386377952463,-1.,2.19552129483562));
#26232=CARTESIAN_POINT('Ctrl Pts',(-0.0732830357304279,-1.,2.19213712012956));
#26233=CARTESIAN_POINT('Ctrl Pts',(-0.0757891465833414,-1.,2.1876201139874));
#26234=CARTESIAN_POINT('Ctrl Pts',(-0.078883772768323,-1.,2.18196589448304));
#26235=CARTESIAN_POINT('Ctrl Pts',(-0.0819402680871942,-1.,2.1763037121106));
#26236=CARTESIAN_POINT('Ctrl Pts',(-0.0849584620835646,-1.,2.17063357871031));
#26237=CARTESIAN_POINT('Ctrl Pts',(-0.0879381291387825,-1.,2.16495552645275));
#26238=CARTESIAN_POINT('Ctrl Pts',(-0.0908789888108269,-1.,2.15926961544808));
#26239=CARTESIAN_POINT('Ctrl Pts',(-0.0937807218868348,-1.,2.15357593978377));
#26240=CARTESIAN_POINT('Ctrl Pts',(-0.0966429852305691,-1.,2.14787463531864));
#26241=CARTESIAN_POINT('Ctrl Pts',(-0.0994654261990745,-1.,2.14216588395974));
#26242=CARTESIAN_POINT('Ctrl Pts',(-0.102247700556064,-1.,2.13644992667052));
#26243=CARTESIAN_POINT('Ctrl Pts',(-0.104989479152703,-1.,2.1307270488718));
#26244=CARTESIAN_POINT('Ctrl Pts',(-0.107690435231068,-1.,2.12499752306927));
#26245=CARTESIAN_POINT('Ctrl Pts',(-0.11035023613502,-1.,2.11926155590849));
#26246=CARTESIAN_POINT('Ctrl Pts',(-0.112968534419746,-1.,2.11351924490335));
#26247=CARTESIAN_POINT('Ctrl Pts',(-0.115544957687941,-1.,2.10777050261359));
#26248=CARTESIAN_POINT('Ctrl Pts',(-0.118079107988368,-1.,2.10201512132945));
#26249=CARTESIAN_POINT('Ctrl Pts',(-0.120570567965129,-1.,2.09625292867756));
#26250=CARTESIAN_POINT('Ctrl Pts',(-0.123018905621083,-1.,2.09048392424826));
#26251=CARTESIAN_POINT('Ctrl Pts',(-0.125423679412058,-1.,2.08470840653628));
#26252=CARTESIAN_POINT('Ctrl Pts',(-0.127784445276116,-1.,2.07892715110967));
#26253=CARTESIAN_POINT('Ctrl Pts',(-0.130100748328401,-1.,2.07314114713047));
#26254=CARTESIAN_POINT('Ctrl Pts',(-0.13237211154771,-1.,2.06735123910319));
#26255=CARTESIAN_POINT('Ctrl Pts',(-0.134598026192107,-1.,2.06155781517844));
#26256=CARTESIAN_POINT('Ctrl Pts',(-0.136777941218044,-1.,2.0557604441427));
#26257=CARTESIAN_POINT('Ctrl Pts',(-0.138911255368966,-1.,2.04995762001333));
#26258=CARTESIAN_POINT('Ctrl Pts',(-0.140997332152546,-1.,2.04414757947919));
#26259=CARTESIAN_POINT('Ctrl Pts',(-0.143035515058208,-1.,2.03832911025913));
#26260=CARTESIAN_POINT('Ctrl Pts',(-0.145025140186058,-1.,2.03250223739941));
#26261=CARTESIAN_POINT('Ctrl Pts',(-0.146965557332586,-1.,2.02666926182017));
#26262=CARTESIAN_POINT('Ctrl Pts',(-0.148856124775343,-1.,2.02083464969897));
#26263=CARTESIAN_POINT('Ctrl Pts',(-0.150696157673084,-1.,2.01500291940243));
#26264=CARTESIAN_POINT('Ctrl Pts',(-0.152484883621452,-1.,2.00917680318426));
#26265=CARTESIAN_POINT('Ctrl Pts',(-0.154221403049719,-1.,2.00335565310539));
#26266=CARTESIAN_POINT('Ctrl Pts',(-0.155904629548775,-1.,1.99753284771487));
#26267=CARTESIAN_POINT('Ctrl Pts',(-0.157533331459215,-1.,1.99169810931893));
#26268=CARTESIAN_POINT('Ctrl Pts',(-0.159106226437289,-1.,1.98584238283279));
#26269=CARTESIAN_POINT('Ctrl Pts',(-0.16062206078461,-1.,1.97996195437557));
#26270=CARTESIAN_POINT('Ctrl Pts',(-0.162079693556302,-1.,1.97406280235204));
#26271=CARTESIAN_POINT('Ctrl Pts',(-0.16347818545776,-1.,1.96816512678));
#26272=CARTESIAN_POINT('Ctrl Pts',(-0.1648165689203,-1.,1.96229379940174));
#26273=CARTESIAN_POINT('Ctrl Pts',(-0.166093592002833,-1.,1.95646759718755));
#26274=CARTESIAN_POINT('Ctrl Pts',(-0.167307501784469,-1.,1.95069027794286));
#26275=CARTESIAN_POINT('Ctrl Pts',(-0.168455741607516,-1.,1.94493757756879));
#26276=CARTESIAN_POINT('Ctrl Pts',(-0.169534904817425,-1.,1.93915639211497));
#26277=CARTESIAN_POINT('Ctrl Pts',(-0.170541253116136,-1.,1.93329183155455));
#26278=CARTESIAN_POINT('Ctrl Pts',(-0.17147119153296,-1.,1.92731093582));
#26279=CARTESIAN_POINT('Ctrl Pts',(-0.172321621259557,-1.,1.92122334398034));
#26280=CARTESIAN_POINT('Ctrl Pts',(-0.173090695383619,-1.,1.91511429159681));
#26281=CARTESIAN_POINT('Ctrl Pts',(-0.173776635257984,-1.,1.90911693975475));
#26282=CARTESIAN_POINT('Ctrl Pts',(-0.174375518661222,-1.,1.90335253863003));
#26283=CARTESIAN_POINT('Ctrl Pts',(-0.174879405091277,-1.,1.89788101117148));
#26284=CARTESIAN_POINT('Ctrl Pts',(-0.175274276190664,-1.,1.89264630198279));
#26285=CARTESIAN_POINT('Ctrl Pts',(-0.175538155840286,-1.,1.88742606272818));
#26286=CARTESIAN_POINT('Ctrl Pts',(-0.175644148889271,-1.,1.88188663144846));
#26287=CARTESIAN_POINT('Ctrl Pts',(-0.175563480746206,-1.,1.87563767773249));
#26288=CARTESIAN_POINT('Ctrl Pts',(-0.175268337590901,-1.,1.86828349694972));
#26289=CARTESIAN_POINT('Ctrl Pts',(-0.174735259276856,-1.,1.85948367089838));
#26290=CARTESIAN_POINT('Ctrl Pts',(-0.173946627589401,-1.,1.84898113200543));
#26291=CARTESIAN_POINT('Ctrl Pts',(-0.17288944289442,-1.,1.83658380530747));
#26292=CARTESIAN_POINT('Ctrl Pts',(-0.171554770207306,-1.,1.82215766815414));
#26293=CARTESIAN_POINT('Ctrl Pts',(-0.169936923908078,-1.,1.80561530633924));
#26294=CARTESIAN_POINT('Ctrl Pts',(-0.16803277280837,-1.,1.78690649988931));
#26295=CARTESIAN_POINT('Ctrl Pts',(-0.166279355148738,-1.,1.77018771687692));
#26296=CARTESIAN_POINT('Ctrl Pts',(-0.164834765708484,-1.,1.75666056640041));
#26297=CARTESIAN_POINT('Ctrl Pts',(-0.163814161002474,-1.,1.74720349503904));
#26298=CARTESIAN_POINT('Ctrl Pts',(-0.163289472382896,-1.,1.74236521665491));
#26299=CARTESIAN_POINT('',(-0.383122945602004,-1.,1.7075470150345));
#26300=CARTESIAN_POINT('Origin',(0.,-1.,0.));
#26301=CARTESIAN_POINT('',(-0.61342227326009,-1.,2.11275013067528));
#26302=CARTESIAN_POINT('Ctrl Pts',(-0.383122945602004,-1.,1.7075470150345));
#26303=CARTESIAN_POINT('Ctrl Pts',(-0.384119047314215,-1.,1.71231062891398));
#26304=CARTESIAN_POINT('Ctrl Pts',(-0.386070790323281,-1.,1.72162022244582));
#26305=CARTESIAN_POINT('Ctrl Pts',(-0.388877023502615,-1.,1.73493170972829));
#26306=CARTESIAN_POINT('Ctrl Pts',(-0.392375812285395,-1.,1.75137405310193));
#26307=CARTESIAN_POINT('Ctrl Pts',(-0.396346196110688,-1.,1.76975560043442));
#26308=CARTESIAN_POINT('Ctrl Pts',(-0.399919403774155,-1.,1.78598826343754));
#26309=CARTESIAN_POINT('Ctrl Pts',(-0.403107976163396,-1.,1.80012077173238));
#26310=CARTESIAN_POINT('Ctrl Pts',(-0.405933518407175,-1.,1.81223801812013));
#26311=CARTESIAN_POINT('Ctrl Pts',(-0.408428948106227,-1.,1.82247022677562));
#26312=CARTESIAN_POINT('Ctrl Pts',(-0.410641256301276,-1.,1.83100408895047));
#26313=CARTESIAN_POINT('Ctrl Pts',(-0.412633125322945,-1.,1.8380895347617));
#26314=CARTESIAN_POINT('Ctrl Pts',(-0.414487438255542,-1.,1.84405757074218));
#26315=CARTESIAN_POINT('Ctrl Pts',(-0.416300022039885,-1.,1.84929312930314));
#26316=CARTESIAN_POINT('Ctrl Pts',(-0.418164129144045,-1.,1.8541763285645));
#26317=CARTESIAN_POINT('Ctrl Pts',(-0.420157287975583,-1.,1.8590328109667));
#26318=CARTESIAN_POINT('Ctrl Pts',(-0.422327307417885,-1.,1.86408083333863));
#26319=CARTESIAN_POINT('Ctrl Pts',(-0.424678177290876,-1.,1.8693780394412));
#26320=CARTESIAN_POINT('Ctrl Pts',(-0.427183828518743,-1.,1.87486989291333));
#26321=CARTESIAN_POINT('Ctrl Pts',(-0.429803062482217,-1.,1.88044229001778));
#26322=CARTESIAN_POINT('Ctrl Pts',(-0.432493038548833,-1.,1.88596913666828));
#26323=CARTESIAN_POINT('Ctrl Pts',(-0.43522566096358,-1.,1.89136993975585));
#26324=CARTESIAN_POINT('Ctrl Pts',(-0.437995003948443,-1.,1.89663648956549));
#26325=CARTESIAN_POINT('Ctrl Pts',(-0.440807833704161,-1.,1.90180124389137));
#26326=CARTESIAN_POINT('Ctrl Pts',(-0.44367755684917,-1.,1.90691756144906));
#26327=CARTESIAN_POINT('Ctrl Pts',(-0.446617343485651,-1.,1.91203699981095));
#26328=CARTESIAN_POINT('Ctrl Pts',(-0.449632260106572,-1.,1.91718342555717));
#26329=CARTESIAN_POINT('Ctrl Pts',(-0.452719478359356,-1.,1.9223538064847));
#26330=CARTESIAN_POINT('Ctrl Pts',(-0.455872005174335,-1.,1.92753067150461));
#26331=CARTESIAN_POINT('Ctrl Pts',(-0.459081234547931,-1.,1.93269066517936));
#26332=CARTESIAN_POINT('Ctrl Pts',(-0.462340031009087,-1.,1.93781486640834));
#26333=CARTESIAN_POINT('Ctrl Pts',(-0.465645462026065,-1.,1.94289794196205));
#26334=CARTESIAN_POINT('Ctrl Pts',(-0.468997482913158,-1.,1.94794381136524));
#26335=CARTESIAN_POINT('Ctrl Pts',(-0.47239767226408,-1.,1.95296148278136));
#26336=CARTESIAN_POINT('Ctrl Pts',(-0.475848034683172,-1.,1.95796111148175));
#26337=CARTESIAN_POINT('Ctrl Pts',(-0.479349583074846,-1.,1.96294933055938));
#26338=CARTESIAN_POINT('Ctrl Pts',(-0.482901662120687,-1.,1.96792703422358));
#26339=CARTESIAN_POINT('Ctrl Pts',(-0.486502692907661,-1.,1.97289186263272));
#26340=CARTESIAN_POINT('Ctrl Pts',(-0.490150627860955,-1.,1.97783973019229));
#26341=CARTESIAN_POINT('Ctrl Pts',(-0.493843476541492,-1.,1.9827665876182));
#26342=CARTESIAN_POINT('Ctrl Pts',(-0.497579909545564,-1.,1.98767044752929));
#26343=CARTESIAN_POINT('Ctrl Pts',(-0.501359287727129,-1.,1.9925514912615));
#26344=CARTESIAN_POINT('Ctrl Pts',(-0.505181361323011,-1.,1.99741107463567));
#26345=CARTESIAN_POINT('Ctrl Pts',(-0.509046069886152,-1.,2.00225107134733));
#26346=CARTESIAN_POINT('Ctrl Pts',(-0.512953306961814,-1.,2.00707309946955));
#26347=CARTESIAN_POINT('Ctrl Pts',(-0.516902681728733,-1.,2.01187773939257));
#26348=CARTESIAN_POINT('Ctrl Pts',(-0.520893590399428,-1.,2.01666477917305));
#26349=CARTESIAN_POINT('Ctrl Pts',(-0.524925318333518,-1.,2.02143356304712));
#26350=CARTESIAN_POINT('Ctrl Pts',(-0.528997127241911,-1.,2.02618329083289));
#26351=CARTESIAN_POINT('Ctrl Pts',(-0.533108355132905,-1.,2.03091336214401));
#26352=CARTESIAN_POINT('Ctrl Pts',(-0.537258489833134,-1.,2.03562362953993));
#26353=CARTESIAN_POINT('Ctrl Pts',(-0.54144712061552,-1.,2.0403142269048));
#26354=CARTESIAN_POINT('Ctrl Pts',(-0.545673903817348,-1.,2.0449854471456));
#26355=CARTESIAN_POINT('Ctrl Pts',(-0.549938525150342,-1.,2.04963761077974));
#26356=CARTESIAN_POINT('Ctrl Pts',(-0.55424065746411,-1.,2.05427091604482));
#26357=CARTESIAN_POINT('Ctrl Pts',(-0.558579940185467,-1.,2.05888537756571));
#26358=CARTESIAN_POINT('Ctrl Pts',(-0.562955993082574,-1.,2.06348090160697));
#26359=CARTESIAN_POINT('Ctrl Pts',(-0.567368421181229,-1.,2.06805732997383));
#26360=CARTESIAN_POINT('Ctrl Pts',(-0.571816823242411,-1.,2.07261449292757));
#26361=CARTESIAN_POINT('Ctrl Pts',(-0.576300797416275,-1.,2.07715226767361));
#26362=CARTESIAN_POINT('Ctrl Pts',(-0.580819952107257,-1.,2.08167059018138));
#26363=CARTESIAN_POINT('Ctrl Pts',(-0.585373918990895,-1.,2.086169437277));
#26364=CARTESIAN_POINT('Ctrl Pts',(-0.589962365403189,-1.,2.09064881812053));
#26365=CARTESIAN_POINT('Ctrl Pts',(-0.594585006052824,-1.,2.09510876220501));
#26366=CARTESIAN_POINT('Ctrl Pts',(-0.599241616422144,-1.,2.09954930865331));
#26367=CARTESIAN_POINT('Ctrl Pts',(-0.603932030738212,-1.,2.10397049887709));
#26368=CARTESIAN_POINT('Ctrl Pts',(-0.607711315456826,-1.,2.10749199615859));
#26369=CARTESIAN_POINT('Ctrl Pts',(-0.610560911691113,-1.,2.11012443807661));
#26370=CARTESIAN_POINT('Ctrl Pts',(-0.61246736556225,-1.,2.11187554260142));
#26371=CARTESIAN_POINT('Ctrl Pts',(-0.61342227326009,-1.,2.11275013067528));
#26372=CARTESIAN_POINT('',(-0.745574324794401,-1.,2.0698113262342));
#26373=CARTESIAN_POINT('',(-0.61342227326009,-1.,2.11275013067528));
#26374=CARTESIAN_POINT('',(-0.693717979106306,-1.,1.60662857109684));
#26375=CARTESIAN_POINT('Ctrl Pts',(-0.745574324794401,-1.,2.0698113262342));
#26376=CARTESIAN_POINT('Ctrl Pts',(-0.74583279137781,-1.,2.06854248895575));
#26377=CARTESIAN_POINT('Ctrl Pts',(-0.746345871542696,-1.,2.06600523016401));
#26378=CARTESIAN_POINT('Ctrl Pts',(-0.747103932785504,-1.,2.06220058927162));
#26379=CARTESIAN_POINT('Ctrl Pts',(-0.748091554181101,-1.,2.05713023030263));
#26380=CARTESIAN_POINT('Ctrl Pts',(-0.749287468663053,-1.,2.05079645591606));
#26381=CARTESIAN_POINT('Ctrl Pts',(-0.750444657874758,-1.,2.04446689147754));
#26382=CARTESIAN_POINT('Ctrl Pts',(-0.751562963361384,-1.,2.03814160092173));
#26383=CARTESIAN_POINT('Ctrl Pts',(-0.752642180488104,-1.,2.03182068456467));
#26384=CARTESIAN_POINT('Ctrl Pts',(-0.753682061113766,-1.,2.02550428623587));
#26385=CARTESIAN_POINT('Ctrl Pts',(-0.75468233072352,-1.,2.01919259406003));
#26386=CARTESIAN_POINT('Ctrl Pts',(-0.7556427049581,-1.,2.01288584328149));
#26387=CARTESIAN_POINT('Ctrl Pts',(-0.756562904646496,-1.,2.00658431587682));
#26388=CARTESIAN_POINT('Ctrl Pts',(-0.757442676862341,-1.,2.00028834739072));
#26389=CARTESIAN_POINT('Ctrl Pts',(-0.758281796766377,-1.,1.9939983109871));
#26390=CARTESIAN_POINT('Ctrl Pts',(-0.759080037802243,-1.,1.98771456680806));
#26391=CARTESIAN_POINT('Ctrl Pts',(-0.759837147452135,-1.,1.98143741418156));
#26392=CARTESIAN_POINT('Ctrl Pts',(-0.760552825409855,-1.,1.97516705321521));
#26393=CARTESIAN_POINT('Ctrl Pts',(-0.761226690483986,-1.,1.96890351582545));
#26394=CARTESIAN_POINT('Ctrl Pts',(-0.761858300014575,-1.,1.96264672744229));
#26395=CARTESIAN_POINT('Ctrl Pts',(-0.762447203806263,-1.,1.95639665309893));
#26396=CARTESIAN_POINT('Ctrl Pts',(-0.762992990878774,-1.,1.95015342590025));
#26397=CARTESIAN_POINT('Ctrl Pts',(-0.76349533353858,-1.,1.94391746617626));
#26398=CARTESIAN_POINT('Ctrl Pts',(-0.763954049121393,-1.,1.93768964875867));
#26399=CARTESIAN_POINT('Ctrl Pts',(-0.764369010673889,-1.,1.93147105496367));
#26400=CARTESIAN_POINT('Ctrl Pts',(-0.764740025488189,-1.,1.92526263537041));
#26401=CARTESIAN_POINT('Ctrl Pts',(-0.765066729667095,-1.,1.91906491634197));
#26402=CARTESIAN_POINT('Ctrl Pts',(-0.765348465884739,-1.,1.91287765805174));
#26403=CARTESIAN_POINT('Ctrl Pts',(-0.765584196937936,-1.,1.90669961402362));
#26404=CARTESIAN_POINT('Ctrl Pts',(-0.765772772593395,-1.,1.90052930393599));
#26405=CARTESIAN_POINT('Ctrl Pts',(-0.765913193856979,-1.,1.89436577771389));
#26406=CARTESIAN_POINT('Ctrl Pts',(-0.76600483706209,-1.,1.88820926433409));
#26407=CARTESIAN_POINT('Ctrl Pts',(-0.766047794851869,-1.,1.88206215302561));
#26408=CARTESIAN_POINT('Ctrl Pts',(-0.766042837036759,-1.,1.87592888967886));
#26409=CARTESIAN_POINT('Ctrl Pts',(-0.765990708546111,-1.,1.86981398314345));
#26410=CARTESIAN_POINT('Ctrl Pts',(-0.765891519092557,-1.,1.86372027063314));
#26411=CARTESIAN_POINT('Ctrl Pts',(-0.765744212909305,-1.,1.85764741390391));
#26412=CARTESIAN_POINT('Ctrl Pts',(-0.765545710619023,-1.,1.85158945130054));
#26413=CARTESIAN_POINT('Ctrl Pts',(-0.765291664861971,-1.,1.8455369887591));
#26414=CARTESIAN_POINT('Ctrl Pts',(-0.764978057881687,-1.,1.83948181064823));
#26415=CARTESIAN_POINT('Ctrl Pts',(-0.764602549687845,-1.,1.8334207722714));
#26416=CARTESIAN_POINT('Ctrl Pts',(-0.764165902606055,-1.,1.8273599120008));
#26417=CARTESIAN_POINT('Ctrl Pts',(-0.763673465462854,-1.,1.82131873145297));
#26418=CARTESIAN_POINT('Ctrl Pts',(-0.763132003836783,-1.,1.81532118405566));
#26419=CARTESIAN_POINT('Ctrl Pts',(-0.762546129464036,-1.,1.80938551463989));
#26420=CARTESIAN_POINT('Ctrl Pts',(-0.761915336443516,-1.,1.80351583877334));
#26421=CARTESIAN_POINT('Ctrl Pts',(-0.761229695230359,-1.,1.79768986997735));
#26422=CARTESIAN_POINT('Ctrl Pts',(-0.760469555880425,-1.,1.79185815610802));
#26423=CARTESIAN_POINT('Ctrl Pts',(-0.759614401109868,-1.,1.78596964884526));
#26424=CARTESIAN_POINT('Ctrl Pts',(-0.75865062667738,-1.,1.77999411220912));
#26425=CARTESIAN_POINT('Ctrl Pts',(-0.757578264077238,-1.,1.77394167108342));
#26426=CARTESIAN_POINT('Ctrl Pts',(-0.756421896028403,-1.,1.76789396003141));
#26427=CARTESIAN_POINT('Ctrl Pts',(-0.755220979975262,-1.,1.7619781724032));
#26428=CARTESIAN_POINT('Ctrl Pts',(-0.75400925402848,-1.,1.75631083600175));
#26429=CARTESIAN_POINT('Ctrl Pts',(-0.752797683531377,-1.,1.75095139468809));
#26430=CARTESIAN_POINT('Ctrl Pts',(-0.751555614163629,-1.,1.74585086852298));
#26431=CARTESIAN_POINT('Ctrl Pts',(-0.75019343597954,-1.,1.74080458266705));
#26432=CARTESIAN_POINT('Ctrl Pts',(-0.748582462954855,-1.,1.73550351679848));
#26433=CARTESIAN_POINT('Ctrl Pts',(-0.746574710096436,-1.,1.72958533647399));
#26434=CARTESIAN_POINT('Ctrl Pts',(-0.744021445433764,-1.,1.7226822991693));
#26435=CARTESIAN_POINT('Ctrl Pts',(-0.740795162032088,-1.,1.71447789751927));
#26436=CARTESIAN_POINT('Ctrl Pts',(-0.736799665724771,-1.,1.70473309006121));
#26437=CARTESIAN_POINT('Ctrl Pts',(-0.731963238697195,-1.,1.69326921975743));
#26438=CARTESIAN_POINT('Ctrl Pts',(-0.726235967997433,-1.,1.67996158455503));
#26439=CARTESIAN_POINT('Ctrl Pts',(-0.719585433804282,-1.,1.6647288055568));
#26440=CARTESIAN_POINT('Ctrl Pts',(-0.711993139355394,-1.,1.64752408832016));
#26441=CARTESIAN_POINT('Ctrl Pts',(-0.705159151988319,-1.,1.63216541664676));
#26442=CARTESIAN_POINT('Ctrl Pts',(-0.699605146405088,-1.,1.61974673472612));
#26443=CARTESIAN_POINT('Ctrl Pts',(-0.695712097881194,-1.,1.61106790958151));
#26444=CARTESIAN_POINT('Ctrl Pts',(-0.693717979106306,-1.,1.60662857109684));
#26445=CARTESIAN_POINT('',(-0.892032620296855,-1.,1.5055822144029));
#26446=CARTESIAN_POINT('Origin',(0.,-1.,0.));
#26447=CARTESIAN_POINT('',(-1.23627494547115,-1.,1.81978687191668));
#26448=CARTESIAN_POINT('Ctrl Pts',(-0.892032620296855,-1.,1.5055822144029));
#26449=CARTESIAN_POINT('Ctrl Pts',(-0.894452006964543,-1.,1.50980486806688));
#26450=CARTESIAN_POINT('Ctrl Pts',(-0.899185047483511,-1.,1.51805569590094));
#26451=CARTESIAN_POINT('Ctrl Pts',(-0.905967409625651,-1.,1.52984849887993));
#26452=CARTESIAN_POINT('Ctrl Pts',(-0.914375919026456,-1.,1.54440491149498));
#26453=CARTESIAN_POINT('Ctrl Pts',(-0.923832188944341,-1.,1.56065988578893));
#26454=CARTESIAN_POINT('Ctrl Pts',(-0.932246680108685,-1.,1.57499388382243));
#26455=CARTESIAN_POINT('Ctrl Pts',(-0.939646377893399,-1.,1.58744937487176));
#26456=CARTESIAN_POINT('Ctrl Pts',(-0.946078063315257,-1.,1.59810042043673));
#26457=CARTESIAN_POINT('Ctrl Pts',(-0.951613284356035,-1.,1.60706069896936));
#26458=CARTESIAN_POINT('Ctrl Pts',(-0.956354422920671,-1.,1.61449324337085));
#26459=CARTESIAN_POINT('Ctrl Pts',(-0.960438326101729,-1.,1.62061638140221));
#26460=CARTESIAN_POINT('Ctrl Pts',(-0.964046107040536,-1.,1.62571930670187));
#26461=CARTESIAN_POINT('Ctrl Pts',(-0.967387853230345,-1.,1.63013849959461));
#26462=CARTESIAN_POINT('Ctrl Pts',(-0.970669715997509,-1.,1.63420665729798));
#26463=CARTESIAN_POINT('Ctrl Pts',(-0.974066058287418,-1.,1.63820952658144));
#26464=CARTESIAN_POINT('Ctrl Pts',(-0.977689794119416,-1.,1.64233990826687));
#26465=CARTESIAN_POINT('Ctrl Pts',(-0.981562530939489,-1.,1.64665139190656));
#26466=CARTESIAN_POINT('Ctrl Pts',(-0.985642622920821,-1.,1.65110016612638));
#26467=CARTESIAN_POINT('Ctrl Pts',(-0.989855627854165,-1.,1.65559044289699));
#26468=CARTESIAN_POINT('Ctrl Pts',(-0.994121836661306,-1.,1.66001553809947));
#26469=CARTESIAN_POINT('Ctrl Pts',(-0.998389654952758,-1.,1.66430758030376));
#26470=CARTESIAN_POINT('Ctrl Pts',(-1.00265091003727,-1.,1.66846059277303));
#26471=CARTESIAN_POINT('Ctrl Pts',(-1.00692206696414,-1.,1.67250335383293));
#26472=CARTESIAN_POINT('Ctrl Pts',(-1.01123236493511,-1.,1.67648246776464));
#26473=CARTESIAN_POINT('Ctrl Pts',(-1.01561026162773,-1.,1.68044289894798));
#26474=CARTESIAN_POINT('Ctrl Pts',(-1.02006795074201,-1.,1.68440578021706));
#26475=CARTESIAN_POINT('Ctrl Pts',(-1.02460180535255,-1.,1.68836910178447));
#26476=CARTESIAN_POINT('Ctrl Pts',(-1.02919977579147,-1.,1.69231840863458));
#26477=CARTESIAN_POINT('Ctrl Pts',(-1.03384646003588,-1.,1.69623414782771));
#26478=CARTESIAN_POINT('Ctrl Pts',(-1.03852922490789,-1.,1.70010052930962));
#26479=CARTESIAN_POINT('Ctrl Pts',(-1.04324363334554,-1.,1.70391338707982));
#26480=CARTESIAN_POINT('Ctrl Pts',(-1.04799085404995,-1.,1.70767646263649));
#26481=CARTESIAN_POINT('Ctrl Pts',(-1.05277517202855,-1.,1.71139783543989));
#26482=CARTESIAN_POINT('Ctrl Pts',(-1.05760163192479,-1.,1.7150865442702));
#26483=CARTESIAN_POINT('Ctrl Pts',(-1.06247324680647,-1.,1.71874858456904));
#26484=CARTESIAN_POINT('Ctrl Pts',(-1.06738966975462,-1.,1.72238500928453));
#26485=CARTESIAN_POINT('Ctrl Pts',(-1.07234866990252,-1.,1.72599406198488));
#26486=CARTESIAN_POINT('Ctrl Pts',(-1.0773470373727,-1.,1.72957248977424));
#26487=CARTESIAN_POINT('Ctrl Pts',(-1.08238162784749,-1.,1.73311705663407));
#26488=CARTESIAN_POINT('Ctrl Pts',(-1.08745056285427,-1.,1.73662628326091));
#26489=CARTESIAN_POINT('Ctrl Pts',(-1.09255329056493,-1.,1.74010053962247));
#26490=CARTESIAN_POINT('Ctrl Pts',(-1.09768999241225,-1.,1.74354119236208));
#26491=CARTESIAN_POINT('Ctrl Pts',(-1.10286118991143,-1.,1.74695004214923));
#26492=CARTESIAN_POINT('Ctrl Pts',(-1.10806728183007,-1.,1.7503286607592));
#26493=CARTESIAN_POINT('Ctrl Pts',(-1.11330807582551,-1.,1.7536777209463));
#26494=CARTESIAN_POINT('Ctrl Pts',(-1.11858293216763,-1.,1.75699720772105));
#26495=CARTESIAN_POINT('Ctrl Pts',(-1.12389096855086,-1.,1.76028671825096));
#26496=CARTESIAN_POINT('Ctrl Pts',(-1.12923123555075,-1.,1.7635457196617));
#26497=CARTESIAN_POINT('Ctrl Pts',(-1.1346029180462,-1.,1.76677384551862));
#26498=CARTESIAN_POINT('Ctrl Pts',(-1.14000548336975,-1.,1.76997111386769));
#26499=CARTESIAN_POINT('Ctrl Pts',(-1.1454385822692,-1.,1.77313777896194));
#26500=CARTESIAN_POINT('Ctrl Pts',(-1.15090197841515,-1.,1.7762742255701));
#26501=CARTESIAN_POINT('Ctrl Pts',(-1.15639547194698,-1.,1.77938085564275));
#26502=CARTESIAN_POINT('Ctrl Pts',(-1.16191881298499,-1.,1.78245795881009));
#26503=CARTESIAN_POINT('Ctrl Pts',(-1.16747166312303,-1.,1.78550566040443));
#26504=CARTESIAN_POINT('Ctrl Pts',(-1.17305363177328,-1.,1.78852398877616));
#26505=CARTESIAN_POINT('Ctrl Pts',(-1.17866429440809,-1.,1.79151291552689));
#26506=CARTESIAN_POINT('Ctrl Pts',(-1.18430321697432,-1.,1.79447240321515));
#26507=CARTESIAN_POINT('Ctrl Pts',(-1.18996997934445,-1.,1.79740245923478));
#26508=CARTESIAN_POINT('Ctrl Pts',(-1.19566418930242,-1.,1.80030314369879));
#26509=CARTESIAN_POINT('Ctrl Pts',(-1.20138548938974,-1.,1.80317454838603));
#26510=CARTESIAN_POINT('Ctrl Pts',(-1.20713356605475,-1.,1.80601678480707));
#26511=CARTESIAN_POINT('Ctrl Pts',(-1.21290815708314,-1.,1.80882996917129));
#26512=CARTESIAN_POINT('Ctrl Pts',(-1.21870906103557,-1.,1.81161420806656));
#26513=CARTESIAN_POINT('Ctrl Pts',(-1.2245361330495,-1.,1.81436959210434));
#26514=CARTESIAN_POINT('Ctrl Pts',(-1.2292186489137,-1.,1.8165508718364));
#26515=CARTESIAN_POINT('Ctrl Pts',(-1.2327422452705,-1.,1.81817389921279));
#26516=CARTESIAN_POINT('Ctrl Pts',(-1.23509651170476,-1.,1.81925017193666));
#26517=CARTESIAN_POINT('Ctrl Pts',(-1.23627494547115,-1.,1.81978687191668));
#26518=CARTESIAN_POINT('',(-1.34869019493419,-1.,1.73811241238545));
#26519=CARTESIAN_POINT('',(-1.23627494547115,-1.,1.81978687191668));
#26520=CARTESIAN_POINT('',(-1.15624053661742,-1.,1.31362392696032));
#26521=CARTESIAN_POINT('Ctrl Pts',(-1.34869019493419,-1.,1.73811241238545));
#26522=CARTESIAN_POINT('Ctrl Pts',(-1.34854391898045,-1.,1.73682580585691));
#26523=CARTESIAN_POINT('Ctrl Pts',(-1.34824783112887,-1.,1.73425417885907));
#26524=CARTESIAN_POINT('Ctrl Pts',(-1.34779309152035,-1.,1.7304014965394));
#26525=CARTESIAN_POINT('Ctrl Pts',(-1.34716554819527,-1.,1.72527410680674));
#26526=CARTESIAN_POINT('Ctrl Pts',(-1.34634568653227,-1.,1.7188807715049));
#26527=CARTESIAN_POINT('Ctrl Pts',(-1.34549029589416,-1.,1.71250340686822));
#26528=CARTESIAN_POINT('Ctrl Pts',(-1.34459924533831,-1.,1.70614212266738));
#26529=CARTESIAN_POINT('Ctrl Pts',(-1.34367237124483,-1.,1.69979707754427));
#26530=CARTESIAN_POINT('Ctrl Pts',(-1.34270948206319,-1.,1.6934684849687));
#26531=CARTESIAN_POINT('Ctrl Pts',(-1.341710374848,-1.,1.68715660868764));
#26532=CARTESIAN_POINT('Ctrl Pts',(-1.34067485185203,-1.,1.68086176030362));
#26533=CARTESIAN_POINT('Ctrl Pts',(-1.3396027347034,-1.,1.67458429426086));
#26534=CARTESIAN_POINT('Ctrl Pts',(-1.33849388654388,-1.,1.66832460783989));
#26535=CARTESIAN_POINT('Ctrl Pts',(-1.33734820885262,-1.,1.66208312541983));
#26536=CARTESIAN_POINT('Ctrl Pts',(-1.33616559745172,-1.,1.65586025952593));
#26537=CARTESIAN_POINT('Ctrl Pts',(-1.33494590467993,-1.,1.6496563728683));
#26538=CARTESIAN_POINT('Ctrl Pts',(-1.33368890676572,-1.,1.6434717485603));
#26539=CARTESIAN_POINT('Ctrl Pts',(-1.33239425103724,-1.,1.63730653475089));
#26540=CARTESIAN_POINT('Ctrl Pts',(-1.33106149345645,-1.,1.63116079730923));
#26541=CARTESIAN_POINT('Ctrl Pts',(-1.3296901950568,-1.,1.62503464209797));
#26542=CARTESIAN_POINT('Ctrl Pts',(-1.32828000610449,-1.,1.61892832270724));
#26543=CARTESIAN_POINT('Ctrl Pts',(-1.32683074483356,-1.,1.6128423401575));
#26544=CARTESIAN_POINT('Ctrl Pts',(-1.32534250785782,-1.,1.60677758290954));
#26545=CARTESIAN_POINT('Ctrl Pts',(-1.32381550858256,-1.,1.60073511858687));
#26546=CARTESIAN_POINT('Ctrl Pts',(-1.32224985747682,-1.,1.59471591079403));
#26547=CARTESIAN_POINT('Ctrl Pts',(-1.32064537110892,-1.,1.58872057258245));
#26548=CARTESIAN_POINT('Ctrl Pts',(-1.31900135021432,-1.,1.58274907898834));
#26549=CARTESIAN_POINT('Ctrl Pts',(-1.31731642317187,-1.,1.5768005650559));
#26550=CARTESIAN_POINT('Ctrl Pts',(-1.31558903860016,-1.,1.57087397835723));
#26551=CARTESIAN_POINT('Ctrl Pts',(-1.31381795281002,-1.,1.56496872402353));
#26552=CARTESIAN_POINT('Ctrl Pts',(-1.31200264341696,-1.,1.55908521254821));
#26553=CARTESIAN_POINT('Ctrl Pts',(-1.31014393684222,-1.,1.55322568759481));
#26554=CARTESIAN_POINT('Ctrl Pts',(-1.30824393907473,-1.,1.54739413957185));
#26555=CARTESIAN_POINT('Ctrl Pts',(-1.30630475189556,-1.,1.54159462645432));
#26556=CARTESIAN_POINT('Ctrl Pts',(-1.30432735639489,-1.,1.53582981268977));
#26557=CARTESIAN_POINT('Ctrl Pts',(-1.30231064395568,-1.,1.53009970283891));
#26558=CARTESIAN_POINT('Ctrl Pts',(-1.30024984366328,-1.,1.52439957861062));
#26559=CARTESIAN_POINT('Ctrl Pts',(-1.29813791800747,-1.,1.51872184912724));
#26560=CARTESIAN_POINT('Ctrl Pts',(-1.29596850710509,-1.,1.51305994241402));
#26561=CARTESIAN_POINT('Ctrl Pts',(-1.29373841372842,-1.,1.50741159078365));
#26562=CARTESIAN_POINT('Ctrl Pts',(-1.29145022885181,-1.,1.50178230149776));
#26563=CARTESIAN_POINT('Ctrl Pts',(-1.28911506584254,-1.,1.49618896881754));
#26564=CARTESIAN_POINT('Ctrl Pts',(-1.2867467611644,-1.,1.4906522831278));
#26565=CARTESIAN_POINT('Ctrl Pts',(-1.28435533880201,-1.,1.4851881711891));
#26566=CARTESIAN_POINT('Ctrl Pts',(-1.28194158939517,-1.,1.47980070347095));
#26567=CARTESIAN_POINT('Ctrl Pts',(-1.2794891824849,-1.,1.4744717526707));
#26568=CARTESIAN_POINT('Ctrl Pts',(-1.27696414831089,-1.,1.46916035917133));
#26569=CARTESIAN_POINT('Ctrl Pts',(-1.27433119897822,-1.,1.46382431332476));
#26570=CARTESIAN_POINT('Ctrl Pts',(-1.27156805265289,-1.,1.45843906294697));
#26571=CARTESIAN_POINT('Ctrl Pts',(-1.2686778680489,-1.,1.45301422764247));
#26572=CARTESIAN_POINT('Ctrl Pts',(-1.26570925118868,-1.,1.44761985001662));
#26573=CARTESIAN_POINT('Ctrl Pts',(-1.26273903323859,-1.,1.44236470511303));
#26574=CARTESIAN_POINT('Ctrl Pts',(-1.25983531012005,-1.,1.43734919180848));
#26575=CARTESIAN_POINT('Ctrl Pts',(-1.25702687965755,-1.,1.43262645609691));
#26576=CARTESIAN_POINT('Ctrl Pts',(-1.25426945222639,-1.,1.42815938799387));
#26577=CARTESIAN_POINT('Ctrl Pts',(-1.2514145557001,-1.,1.42378102115575));
#26578=CARTESIAN_POINT('Ctrl Pts',(-1.24824430986571,-1.,1.41923722596025));
#26579=CARTESIAN_POINT('Ctrl Pts',(-1.24450600513056,-1.,1.41422913175179));
#26580=CARTESIAN_POINT('Ctrl Pts',(-1.23994455029534,-1.,1.40845295531283));
#26581=CARTESIAN_POINT('Ctrl Pts',(-1.23434087290423,-1.,1.40164708206106));
#26582=CARTESIAN_POINT('Ctrl Pts',(-1.22752961899387,-1.,1.39361389568796));
#26583=CARTESIAN_POINT('Ctrl Pts',(-1.21938737280852,-1.,1.38420564527715));
#26584=CARTESIAN_POINT('Ctrl Pts',(-1.20982812925645,-1.,1.37331915607905));
#26585=CARTESIAN_POINT('Ctrl Pts',(-1.1987959077932,-1.,1.36088705043885));
#26586=CARTESIAN_POINT('Ctrl Pts',(-1.18625865667441,-1.,1.34687054001093));
#26587=CARTESIAN_POINT('Ctrl Pts',(-1.17501305789857,-1.,1.33437539347008));
#26588=CARTESIAN_POINT('Ctrl Pts',(-1.16589330093588,-1.,1.32428080721772));
#26589=CARTESIAN_POINT('Ctrl Pts',(-1.15950888730809,-1.,1.31722977216397));
#26590=CARTESIAN_POINT('Ctrl Pts',(-1.15624053661742,-1.,1.31362392696032));
#26591=CARTESIAN_POINT('',(-1.31362392696033,-1.,1.15624053661742));
#26592=CARTESIAN_POINT('Origin',(0.,-1.,0.));
#26593=CARTESIAN_POINT('',(-1.73811241238545,-1.,1.34869019493419));
#26594=CARTESIAN_POINT('Ctrl Pts',(-1.31362392696033,-1.,1.15624053661742));
#26595=CARTESIAN_POINT('Ctrl Pts',(-1.3172297721596,-1.,1.15950888730433));
#26596=CARTESIAN_POINT('Ctrl Pts',(-1.32428080720544,-1.,1.16589330092532));
#26597=CARTESIAN_POINT('Ctrl Pts',(-1.33437539344842,-1.,1.17501305787994));
#26598=CARTESIAN_POINT('Ctrl Pts',(-1.34687053998157,-1.,1.18625865664915));
#26599=CARTESIAN_POINT('Ctrl Pts',(-1.36088705040677,-1.,1.1987959077656));
#26600=CARTESIAN_POINT('Ctrl Pts',(-1.37331915604962,-1.,1.20982812923113));
#26601=CARTESIAN_POINT('Ctrl Pts',(-1.38420564525391,-1.,1.21938737278853));
#26602=CARTESIAN_POINT('Ctrl Pts',(-1.39361389567257,-1.,1.22752961898063));
#26603=CARTESIAN_POINT('Ctrl Pts',(-1.40164708205345,-1.,1.23434087289768));
#26604=CARTESIAN_POINT('Ctrl Pts',(-1.40845295531151,-1.,1.23994455029421));
#26605=CARTESIAN_POINT('Ctrl Pts',(-1.41422913175437,-1.,1.24450600513278));
#26606=CARTESIAN_POINT('Ctrl Pts',(-1.41923722596421,-1.,1.24824430986911));
#26607=CARTESIAN_POINT('Ctrl Pts',(-1.42378102115911,-1.,1.25141455570299));
#26608=CARTESIAN_POINT('Ctrl Pts',(-1.42815938799555,-1.,1.25426945222783));
#26609=CARTESIAN_POINT('Ctrl Pts',(-1.43262645609679,-1.,1.25702687965744));
#26610=CARTESIAN_POINT('Ctrl Pts',(-1.43734919180719,-1.,1.25983531011894));
#26611=CARTESIAN_POINT('Ctrl Pts',(-1.44236470511145,-1.,1.26273903323723));
#26612=CARTESIAN_POINT('Ctrl Pts',(-1.44761985001544,-1.,1.26570925118767));
#26613=CARTESIAN_POINT('Ctrl Pts',(-1.45301422764205,-1.,1.26867786804854));
#26614=CARTESIAN_POINT('Ctrl Pts',(-1.45843906294725,-1.,1.27156805265312));
#26615=CARTESIAN_POINT('Ctrl Pts',(-1.4638243133254,-1.,1.27433119897877));
#26616=CARTESIAN_POINT('Ctrl Pts',(-1.46916035917197,-1.,1.27696414831144));
#26617=CARTESIAN_POINT('Ctrl Pts',(-1.4744717526711,-1.,1.27948918248524));
#26618=CARTESIAN_POINT('Ctrl Pts',(-1.47980070347102,-1.,1.28194158939522));
#26619=CARTESIAN_POINT('Ctrl Pts',(-1.48518817118891,-1.,1.28435533880184));
#26620=CARTESIAN_POINT('Ctrl Pts',(-1.4906522831275,-1.,1.28674676116415));
#26621=CARTESIAN_POINT('Ctrl Pts',(-1.49618896881729,-1.,1.28911506584232));
#26622=CARTESIAN_POINT('Ctrl Pts',(-1.50178230149764,-1.,1.29145022885171));
#26623=CARTESIAN_POINT('Ctrl Pts',(-1.50741159078367,-1.,1.29373841372843));
#26624=CARTESIAN_POINT('Ctrl Pts',(-1.51305994241412,-1.,1.29596850710518));
#26625=CARTESIAN_POINT('Ctrl Pts',(-1.51872184912735,-1.,1.29813791800757));
#26626=CARTESIAN_POINT('Ctrl Pts',(-1.5243995786107,-1.,1.30024984366334));
#26627=CARTESIAN_POINT('Ctrl Pts',(-1.53009970283893,-1.,1.3023106439557));
#26628=CARTESIAN_POINT('Ctrl Pts',(-1.53582981268976,-1.,1.30432735639487));
#26629=CARTESIAN_POINT('Ctrl Pts',(-1.54159462645428,-1.,1.30630475189553));
#26630=CARTESIAN_POINT('Ctrl Pts',(-1.54739413957183,-1.,1.30824393907471));
#26631=CARTESIAN_POINT('Ctrl Pts',(-1.55322568759481,-1.,1.31014393684221));
#26632=CARTESIAN_POINT('Ctrl Pts',(-1.55908521254822,-1.,1.31200264341696));
#26633=CARTESIAN_POINT('Ctrl Pts',(-1.56496872402352,-1.,1.31381795281002));
#26634=CARTESIAN_POINT('Ctrl Pts',(-1.57087397835721,-1.,1.31558903860015));
#26635=CARTESIAN_POINT('Ctrl Pts',(-1.57680056505585,-1.,1.31731642317183));
#26636=CARTESIAN_POINT('Ctrl Pts',(-1.58274907898829,-1.,1.31900135021428));
#26637=CARTESIAN_POINT('Ctrl Pts',(-1.58872057258244,-1.,1.32064537110891));
#26638=CARTESIAN_POINT('Ctrl Pts',(-1.59471591079408,-1.,1.32224985747686));
#26639=CARTESIAN_POINT('Ctrl Pts',(-1.600735118587,-1.,1.32381550858266));
#26640=CARTESIAN_POINT('Ctrl Pts',(-1.6067775829097,-1.,1.32534250785794));
#26641=CARTESIAN_POINT('Ctrl Pts',(-1.61284234015762,-1.,1.32683074483365));
#26642=CARTESIAN_POINT('Ctrl Pts',(-1.61892832270723,-1.,1.32828000610448));
#26643=CARTESIAN_POINT('Ctrl Pts',(-1.62503464209777,-1.,1.32969019505665));
#26644=CARTESIAN_POINT('Ctrl Pts',(-1.63116079730887,-1.,1.33106149345618));
#26645=CARTESIAN_POINT('Ctrl Pts',(-1.6373065347505,-1.,1.33239425103694));
#26646=CARTESIAN_POINT('Ctrl Pts',(-1.64347174856007,-1.,1.33368890676554));
#26647=CARTESIAN_POINT('Ctrl Pts',(-1.64965637286843,-1.,1.33494590468003));
#26648=CARTESIAN_POINT('Ctrl Pts',(-1.65586025952651,-1.,1.33616559745217));
#26649=CARTESIAN_POINT('Ctrl Pts',(-1.66208312542073,-1.,1.33734820885331));
#26650=CARTESIAN_POINT('Ctrl Pts',(-1.66832460784078,-1.,1.33849388654458));
#26651=CARTESIAN_POINT('Ctrl Pts',(-1.67458429426126,-1.,1.33960273470372));
#26652=CARTESIAN_POINT('Ctrl Pts',(-1.68086176030308,-1.,1.3406748518516));
#26653=CARTESIAN_POINT('Ctrl Pts',(-1.68715660868602,-1.,1.34171037484673));
#26654=CARTESIAN_POINT('Ctrl Pts',(-1.6934684849664,-1.,1.34270948206139));
#26655=CARTESIAN_POINT('Ctrl Pts',(-1.69979707754221,-1.,1.34367237124322));
#26656=CARTESIAN_POINT('Ctrl Pts',(-1.70614212266676,-1.,1.34459924533783));
#26657=CARTESIAN_POINT('Ctrl Pts',(-1.71250340687011,-1.,1.34549029589563));
#26658=CARTESIAN_POINT('Ctrl Pts',(-1.7188807715095,-1.,1.34634568653586));
#26659=CARTESIAN_POINT('Ctrl Pts',(-1.72527410681298,-1.,1.34716554820013));
#26660=CARTESIAN_POINT('Ctrl Pts',(-1.73040149654497,-1.,1.3477930915247));
#26661=CARTESIAN_POINT('Ctrl Pts',(-1.73425417886255,-1.,1.34824783113158));
#26662=CARTESIAN_POINT('Ctrl Pts',(-1.73682580585819,-1.,1.34854391898145));
#26663=CARTESIAN_POINT('Ctrl Pts',(-1.73811241238545,-1.,1.34869019493419));
#26664=CARTESIAN_POINT('',(-1.81978687191668,-1.,1.23627494547115));
#26665=CARTESIAN_POINT('',(-1.73811241238545,-1.,1.34869019493419));
#26666=CARTESIAN_POINT('',(-1.5055822144029,-1.,0.892032620296855));
#26667=CARTESIAN_POINT('Ctrl Pts',(-1.81978687191668,-1.,1.23627494547115));
#26668=CARTESIAN_POINT('Ctrl Pts',(-1.81925017193531,-1.,1.23509651170384));
#26669=CARTESIAN_POINT('Ctrl Pts',(-1.81817389920914,-1.,1.23274224526804));
#26670=CARTESIAN_POINT('Ctrl Pts',(-1.81655087183054,-1.,1.22921864890975));
#26671=CARTESIAN_POINT('Ctrl Pts',(-1.81436959209778,-1.,1.22453613304507));
#26672=CARTESIAN_POINT('Ctrl Pts',(-1.81161420806172,-1.,1.2187090610323));
#26673=CARTESIAN_POINT('Ctrl Pts',(-1.80882996916931,-1.,1.2129081570818));
#26674=CARTESIAN_POINT('Ctrl Pts',(-1.80601678480772,-1.,1.20713356605519));
#26675=CARTESIAN_POINT('Ctrl Pts',(-1.8031745483882,-1.,1.2013854893912));
#26676=CARTESIAN_POINT('Ctrl Pts',(-1.80030314370121,-1.,1.19566418930405));
#26677=CARTESIAN_POINT('Ctrl Pts',(-1.79740245923649,-1.,1.1899699793456));
#26678=CARTESIAN_POINT('Ctrl Pts',(-1.79447240321572,-1.,1.18430321697471));
#26679=CARTESIAN_POINT('Ctrl Pts',(-1.79151291552646,-1.,1.17866429440781));
#26680=CARTESIAN_POINT('Ctrl Pts',(-1.78852398877523,-1.,1.17305363177265));
#26681=CARTESIAN_POINT('Ctrl Pts',(-1.78550566040349,-1.,1.16747166312239));
#26682=CARTESIAN_POINT('Ctrl Pts',(-1.78245795880949,-1.,1.16191881298458));
#26683=CARTESIAN_POINT('Ctrl Pts',(-1.77938085564261,-1.,1.15639547194689));
#26684=CARTESIAN_POINT('Ctrl Pts',(-1.77627422557034,-1.,1.15090197841531));
#26685=CARTESIAN_POINT('Ctrl Pts',(-1.77313777896234,-1.,1.14543858226948));
#26686=CARTESIAN_POINT('Ctrl Pts',(-1.76997111386806,-1.,1.14000548337));
#26687=CARTESIAN_POINT('Ctrl Pts',(-1.76677384551883,-1.,1.13460291804635));
#26688=CARTESIAN_POINT('Ctrl Pts',(-1.76354571966171,-1.,1.12923123555076));
#26689=CARTESIAN_POINT('Ctrl Pts',(-1.76028671825084,-1.,1.12389096855078));
#26690=CARTESIAN_POINT('Ctrl Pts',(-1.75699720772089,-1.,1.11858293216752));
#26691=CARTESIAN_POINT('Ctrl Pts',(-1.75367772094617,-1.,1.11330807582542));
#26692=CARTESIAN_POINT('Ctrl Pts',(-1.75032866075914,-1.,1.10806728183003));
#26693=CARTESIAN_POINT('Ctrl Pts',(-1.74695004214924,-1.,1.10286118991144));
#26694=CARTESIAN_POINT('Ctrl Pts',(-1.74354119236212,-1.,1.09768999241229));
#26695=CARTESIAN_POINT('Ctrl Pts',(-1.74010053962252,-1.,1.09255329056496));
#26696=CARTESIAN_POINT('Ctrl Pts',(-1.73662628326093,-1.,1.08745056285429));
#26697=CARTESIAN_POINT('Ctrl Pts',(-1.73311705663407,-1.,1.08238162784749));
#26698=CARTESIAN_POINT('Ctrl Pts',(-1.72957248977424,-1.,1.0773470373727));
#26699=CARTESIAN_POINT('Ctrl Pts',(-1.72599406198489,-1.,1.07234866990252));
#26700=CARTESIAN_POINT('Ctrl Pts',(-1.72238500928456,-1.,1.06738966975463));
#26701=CARTESIAN_POINT('Ctrl Pts',(-1.71874858456908,-1.,1.0624732468065));
#26702=CARTESIAN_POINT('Ctrl Pts',(-1.71508654427022,-1.,1.05760163192481));
#26703=CARTESIAN_POINT('Ctrl Pts',(-1.71139783543986,-1.,1.05277517202854));
#26704=CARTESIAN_POINT('Ctrl Pts',(-1.70767646263641,-1.,1.0479908540499));
#26705=CARTESIAN_POINT('Ctrl Pts',(-1.70391338707969,-1.,1.04324363334546));
#26706=CARTESIAN_POINT('Ctrl Pts',(-1.70010052930951,-1.,1.03852922490782));
#26707=CARTESIAN_POINT('Ctrl Pts',(-1.69623414782769,-1.,1.03384646003587));
#26708=CARTESIAN_POINT('Ctrl Pts',(-1.69231840863471,-1.,1.02919977579155));
#26709=CARTESIAN_POINT('Ctrl Pts',(-1.68836910178475,-1.,1.02460180535272));
#26710=CARTESIAN_POINT('Ctrl Pts',(-1.68440578021739,-1.,1.02006795074222));
#26711=CARTESIAN_POINT('Ctrl Pts',(-1.6804428989482,-1.,1.01561026162787));
#26712=CARTESIAN_POINT('Ctrl Pts',(-1.67648246776457,-1.,1.01123236493507));
#26713=CARTESIAN_POINT('Ctrl Pts',(-1.67250335383248,-1.,1.00692206696387));
#26714=CARTESIAN_POINT('Ctrl Pts',(-1.66846059277231,-1.,1.00265091003682));
#26715=CARTESIAN_POINT('Ctrl Pts',(-1.66430758030304,-1.,0.998389654952317));
#26716=CARTESIAN_POINT('Ctrl Pts',(-1.66001553809916,-1.,0.994121836661116));
#26717=CARTESIAN_POINT('Ctrl Pts',(-1.65559044289746,-1.,0.98985562785445));
#26718=CARTESIAN_POINT('Ctrl Pts',(-1.6511001661277,-1.,0.985642622921626));
#26719=CARTESIAN_POINT('Ctrl Pts',(-1.64665139190834,-1.,0.981562530940574));
#26720=CARTESIAN_POINT('Ctrl Pts',(-1.64233990826831,-1.,0.977689794120297));
#26721=CARTESIAN_POINT('Ctrl Pts',(-1.63820952658157,-1.,0.974066058287501));
#26722=CARTESIAN_POINT('Ctrl Pts',(-1.63420665729609,-1.,0.970669715996356));
#26723=CARTESIAN_POINT('Ctrl Pts',(-1.63013849959083,-1.,0.967387853228041));
#26724=CARTESIAN_POINT('Ctrl Pts',(-1.6257193066974,-1.,0.964046107037821));
#26725=CARTESIAN_POINT('Ctrl Pts',(-1.62061638139929,-1.,0.960438326099958));
#26726=CARTESIAN_POINT('Ctrl Pts',(-1.61449324337233,-1.,0.956354422921573));
#26727=CARTESIAN_POINT('Ctrl Pts',(-1.60706069897794,-1.,0.951613284361248));
#26728=CARTESIAN_POINT('Ctrl Pts',(-1.59810042045408,-1.,0.946078063325796));
#26729=CARTESIAN_POINT('Ctrl Pts',(-1.58744937489796,-1.,0.939646377909319));
#26730=CARTESIAN_POINT('Ctrl Pts',(-1.57499388385561,-1.,0.932246680128849));
#26731=CARTESIAN_POINT('Ctrl Pts',(-1.56065988582509,-1.,0.923832188966322));
#26732=CARTESIAN_POINT('Ctrl Pts',(-1.54440491152808,-1.,0.91437591904658));
#26733=CARTESIAN_POINT('Ctrl Pts',(-1.52984849890434,-1.,0.905967409640499));
#26734=CARTESIAN_POINT('Ctrl Pts',(-1.51805569591479,-1.,0.89918504749193));
#26735=CARTESIAN_POINT('Ctrl Pts',(-1.50980486807181,-1.,0.894452006967538));
#26736=CARTESIAN_POINT('Ctrl Pts',(-1.5055822144029,-1.,0.892032620296855));
#26737=CARTESIAN_POINT('',(-1.60662857109684,-1.,0.693717979106305));
#26738=CARTESIAN_POINT('Origin',(0.,-1.,0.));
#26739=CARTESIAN_POINT('',(-2.0698113262342,-1.,0.7455743247944));
#26740=CARTESIAN_POINT('Ctrl Pts',(-1.60662857109684,-1.,0.693717979106305));
#26741=CARTESIAN_POINT('Ctrl Pts',(-1.61106790957619,-1.,0.69571209787897));
#26742=CARTESIAN_POINT('Ctrl Pts',(-1.61974673471117,-1.,0.699605146398837));
#26743=CARTESIAN_POINT('Ctrl Pts',(-1.6321654166204,-1.,0.705159151977294));
#26744=CARTESIAN_POINT('Ctrl Pts',(-1.64752408828442,-1.,0.711993139340447));
#26745=CARTESIAN_POINT('Ctrl Pts',(-1.66472880551777,-1.,0.71958543378795));
#26746=CARTESIAN_POINT('Ctrl Pts',(-1.67996158451922,-1.,0.726235967982445));
#26747=CARTESIAN_POINT('Ctrl Pts',(-1.69326921972915,-1.,0.731963238685357));
#26748=CARTESIAN_POINT('Ctrl Pts',(-1.70473309004249,-1.,0.736799665716932));
#26749=CARTESIAN_POINT('Ctrl Pts',(-1.71447789751001,-1.,0.74079516202821));
#26750=CARTESIAN_POINT('Ctrl Pts',(-1.72268229916769,-1.,0.744021445433093));
#26751=CARTESIAN_POINT('Ctrl Pts',(-1.72958533647714,-1.,0.746574710097752));
#26752=CARTESIAN_POINT('Ctrl Pts',(-1.7355035168033,-1.,0.74858246295687));
#26753=CARTESIAN_POINT('Ctrl Pts',(-1.74080458267114,-1.,0.750193435981249));
#26754=CARTESIAN_POINT('Ctrl Pts',(-1.74585086852502,-1.,0.751555614164482));
#26755=CARTESIAN_POINT('Ctrl Pts',(-1.75095139468794,-1.,0.752797683531314));
#26756=CARTESIAN_POINT('Ctrl Pts',(-1.75631083600019,-1.,0.754009254027829));
#26757=CARTESIAN_POINT('Ctrl Pts',(-1.76197817240128,-1.,0.755220979974461));
#26758=CARTESIAN_POINT('Ctrl Pts',(-1.76789396002998,-1.,0.75642189602781));
#26759=CARTESIAN_POINT('Ctrl Pts',(-1.77394167108292,-1.,0.757578264077029));
#26760=CARTESIAN_POINT('Ctrl Pts',(-1.77999411220945,-1.,0.758650626677518));
#26761=CARTESIAN_POINT('Ctrl Pts',(-1.78596964884604,-1.,0.759614401110189));
#26762=CARTESIAN_POINT('Ctrl Pts',(-1.7918581561088,-1.,0.760469555880749));
#26763=CARTESIAN_POINT('Ctrl Pts',(-1.79768986997783,-1.,0.761229695230558));
#26764=CARTESIAN_POINT('Ctrl Pts',(-1.80351583877342,-1.,0.761915336443547));
#26765=CARTESIAN_POINT('Ctrl Pts',(-1.80938551463965,-1.,0.762546129463938));
#26766=CARTESIAN_POINT('Ctrl Pts',(-1.8153211840553,-1.,0.763132003836634));
#26767=CARTESIAN_POINT('Ctrl Pts',(-1.82131873145266,-1.,0.763673465462726));
#26768=CARTESIAN_POINT('Ctrl Pts',(-1.82735991200065,-1.,0.764165902605995));
#26769=CARTESIAN_POINT('Ctrl Pts',(-1.83342077227142,-1.,0.764602549687853));
#26770=CARTESIAN_POINT('Ctrl Pts',(-1.83948181064835,-1.,0.764978057881737));
#26771=CARTESIAN_POINT('Ctrl Pts',(-1.84553698875924,-1.,0.765291664862029));
#26772=CARTESIAN_POINT('Ctrl Pts',(-1.85158945130063,-1.,0.765545710619062));
#26773=CARTESIAN_POINT('Ctrl Pts',(-1.85764741390394,-1.,0.765744212909318));
#26774=CARTESIAN_POINT('Ctrl Pts',(-1.86372027063312,-1.,0.765891519092547));
#26775=CARTESIAN_POINT('Ctrl Pts',(-1.86981398314341,-1.,0.765990708546091));
#26776=CARTESIAN_POINT('Ctrl Pts',(-1.87592888967883,-1.,0.766042837036744));
#26777=CARTESIAN_POINT('Ctrl Pts',(-1.88206215302561,-1.,0.766047794851864));
#26778=CARTESIAN_POINT('Ctrl Pts',(-1.88820926433409,-1.,0.766004837062091));
#26779=CARTESIAN_POINT('Ctrl Pts',(-1.89436577771388,-1.,0.765913193856978));
#26780=CARTESIAN_POINT('Ctrl Pts',(-1.90052930393596,-1.,0.765772772593386));
#26781=CARTESIAN_POINT('Ctrl Pts',(-1.90669961402356,-1.,0.765584196937919));
#26782=CARTESIAN_POINT('Ctrl Pts',(-1.91287765805169,-1.,0.765348465884722));
#26783=CARTESIAN_POINT('Ctrl Pts',(-1.91906491634196,-1.,0.765066729667088));
#26784=CARTESIAN_POINT('Ctrl Pts',(-1.92526263537048,-1.,0.764740025488211));
#26785=CARTESIAN_POINT('Ctrl Pts',(-1.93147105496382,-1.,0.76436901067394));
#26786=CARTESIAN_POINT('Ctrl Pts',(-1.93768964875886,-1.,0.763954049121458));
#26787=CARTESIAN_POINT('Ctrl Pts',(-1.9439174661764,-1.,0.763495333538629));
#26788=CARTESIAN_POINT('Ctrl Pts',(-1.95015342590024,-1.,0.762992990878769));
#26789=CARTESIAN_POINT('Ctrl Pts',(-1.95639665309869,-1.,0.762447203806179));
#26790=CARTESIAN_POINT('Ctrl Pts',(-1.96264672744186,-1.,0.761858300014423));
#26791=CARTESIAN_POINT('Ctrl Pts',(-1.96890351582499,-1.,0.76122669048382));
#26792=CARTESIAN_POINT('Ctrl Pts',(-1.97516705321494,-1.,0.760552825409757));
#26793=CARTESIAN_POINT('Ctrl Pts',(-1.98143741418172,-1.,0.75983714745219));
#26794=CARTESIAN_POINT('Ctrl Pts',(-1.98771456680874,-1.,0.759080037802488));
#26795=CARTESIAN_POINT('Ctrl Pts',(-1.99399831098817,-1.,0.758281796766761));
#26796=CARTESIAN_POINT('Ctrl Pts',(-2.00028834739178,-1.,0.757442676862724));
#26797=CARTESIAN_POINT('Ctrl Pts',(-2.0065843158773,-1.,0.75656290464667));
#26798=CARTESIAN_POINT('Ctrl Pts',(-2.01288584328084,-1.,0.755642704957865));
#26799=CARTESIAN_POINT('Ctrl Pts',(-2.01919259405809,-1.,0.754682330722816));
#26800=CARTESIAN_POINT('Ctrl Pts',(-2.02550428623313,-1.,0.753682061112768));
#26801=CARTESIAN_POINT('Ctrl Pts',(-2.03182068456221,-1.,0.752642180487211));
#26802=CARTESIAN_POINT('Ctrl Pts',(-2.03814160092099,-1.,0.751562963361115));
#26803=CARTESIAN_POINT('Ctrl Pts',(-2.04446689147979,-1.,0.750444657875576));
#26804=CARTESIAN_POINT('Ctrl Pts',(-2.05079645592154,-1.,0.749287468665046));
#26805=CARTESIAN_POINT('Ctrl Pts',(-2.05713023031006,-1.,0.748091554183802));
#26806=CARTESIAN_POINT('Ctrl Pts',(-2.06220058927826,-1.,0.747103932787919));
#26807=CARTESIAN_POINT('Ctrl Pts',(-2.06600523016815,-1.,0.7463458715442));
#26808=CARTESIAN_POINT('Ctrl Pts',(-2.06854248895728,-1.,0.745832791378367));
#26809=CARTESIAN_POINT('Ctrl Pts',(-2.0698113262342,-1.,0.7455743247944));
#26810=CARTESIAN_POINT('',(-2.11275013067528,-1.,0.61342227326009));
#26811=CARTESIAN_POINT('',(-2.0698113262342,-1.,0.7455743247944));
#26812=CARTESIAN_POINT('',(-1.7075470150345,-1.,0.383122945602004));
#26813=CARTESIAN_POINT('Ctrl Pts',(-2.11275013067528,-1.,0.61342227326009));
#26814=CARTESIAN_POINT('Ctrl Pts',(-2.11187554259986,-1.,0.6124673655618));
#26815=CARTESIAN_POINT('Ctrl Pts',(-2.11012443807238,-1.,0.610560911689899));
#26816=CARTESIAN_POINT('Ctrl Pts',(-2.1074919961518,-1.,0.607711315454876));
#26817=CARTESIAN_POINT('Ctrl Pts',(-2.10397049886949,-1.,0.60393203073603));
#26818=CARTESIAN_POINT('Ctrl Pts',(-2.0995493086477,-1.,0.599241616420533));
#26819=CARTESIAN_POINT('Ctrl Pts',(-2.0951087622027,-1.,0.594585006052162));
#26820=CARTESIAN_POINT('Ctrl Pts',(-2.09064881812129,-1.,0.589962365403406));
#26821=CARTESIAN_POINT('Ctrl Pts',(-2.08616943727951,-1.,0.585373918991617));
#26822=CARTESIAN_POINT('Ctrl Pts',(-2.08167059018418,-1.,0.580819952108063));
#26823=CARTESIAN_POINT('Ctrl Pts',(-2.07715226767559,-1.,0.576300797416844));
#26824=CARTESIAN_POINT('Ctrl Pts',(-2.07261449292824,-1.,0.571816823242603));
#26825=CARTESIAN_POINT('Ctrl Pts',(-2.06805732997334,-1.,0.567368421181087));
#26826=CARTESIAN_POINT('Ctrl Pts',(-2.06348090160589,-1.,0.562955993082261));
#26827=CARTESIAN_POINT('Ctrl Pts',(-2.05888537756462,-1.,0.558579940185151));
#26828=CARTESIAN_POINT('Ctrl Pts',(-2.05427091604413,-1.,0.554240657463906));
#26829=CARTESIAN_POINT('Ctrl Pts',(-2.04963761077958,-1.,0.549938525150295));
#26830=CARTESIAN_POINT('Ctrl Pts',(-2.04498544714588,-1.,0.54567390381743));
#26831=CARTESIAN_POINT('Ctrl Pts',(-2.04031422690527,-1.,0.541447120615659));
#26832=CARTESIAN_POINT('Ctrl Pts',(-2.03562362954037,-1.,0.537258489833262));
#26833=CARTESIAN_POINT('Ctrl Pts',(-2.03091336214426,-1.,0.533108355132976));
#26834=CARTESIAN_POINT('Ctrl Pts',(-2.0261832908329,-1.,0.528997127241914));
#26835=CARTESIAN_POINT('Ctrl Pts',(-2.02143356304698,-1.,0.524925318333476));
#26836=CARTESIAN_POINT('Ctrl Pts',(-2.01666477917286,-1.,0.52089359039937));
#26837=CARTESIAN_POINT('Ctrl Pts',(-2.01187773939242,-1.,0.516902681728687));
#26838=CARTESIAN_POINT('Ctrl Pts',(-2.00707309946949,-1.,0.512953306961792));
#26839=CARTESIAN_POINT('Ctrl Pts',(-2.00225107134734,-1.,0.509046069886157));
#26840=CARTESIAN_POINT('Ctrl Pts',(-1.99741107463572,-1.,0.505181361323026));
#26841=CARTESIAN_POINT('Ctrl Pts',(-1.99255149126155,-1.,0.501359287727146));
#26842=CARTESIAN_POINT('Ctrl Pts',(-1.98767044752932,-1.,0.497579909545574));
#26843=CARTESIAN_POINT('Ctrl Pts',(-1.98276658761821,-1.,0.493843476541494));
#26844=CARTESIAN_POINT('Ctrl Pts',(-1.97783973019229,-1.,0.490150627860952));
#26845=CARTESIAN_POINT('Ctrl Pts',(-1.97289186263272,-1.,0.486502692907659));
#26846=CARTESIAN_POINT('Ctrl Pts',(-1.96792703422362,-1.,0.48290166212069));
#26847=CARTESIAN_POINT('Ctrl Pts',(-1.96294933055943,-1.,0.479349583074855));
#26848=CARTESIAN_POINT('Ctrl Pts',(-1.95796111148177,-1.,0.475848034683176));
#26849=CARTESIAN_POINT('Ctrl Pts',(-1.95296148278133,-1.,0.472397672264072));
#26850=CARTESIAN_POINT('Ctrl Pts',(-1.94794381136514,-1.,0.468997482913135));
#26851=CARTESIAN_POINT('Ctrl Pts',(-1.9428979419619,-1.,0.46564546202603));
#26852=CARTESIAN_POINT('Ctrl Pts',(-1.93781486640821,-1.,0.462340031009056));
#26853=CARTESIAN_POINT('Ctrl Pts',(-1.93269066517934,-1.,0.459081234547926));
#26854=CARTESIAN_POINT('Ctrl Pts',(-1.92753067150476,-1.,0.455872005174371));
#26855=CARTESIAN_POINT('Ctrl Pts',(-1.92235380648502,-1.,0.452719478359432));
#26856=CARTESIAN_POINT('Ctrl Pts',(-1.91718342555755,-1.,0.449632260106662));
#26857=CARTESIAN_POINT('Ctrl Pts',(-1.9120369998112,-1.,0.446617343485711));
#26858=CARTESIAN_POINT('Ctrl Pts',(-1.90691756144898,-1.,0.44367755684915));
#26859=CARTESIAN_POINT('Ctrl Pts',(-1.90180124389086,-1.,0.440807833704038));
#26860=CARTESIAN_POINT('Ctrl Pts',(-1.89663648956466,-1.,0.437995003948244));
#26861=CARTESIAN_POINT('Ctrl Pts',(-1.89136993975504,-1.,0.435225660963383));
#26862=CARTESIAN_POINT('Ctrl Pts',(-1.88596913666793,-1.,0.432493038548748));
#26863=CARTESIAN_POINT('Ctrl Pts',(-1.88044229001832,-1.,0.429803062482344));
#26864=CARTESIAN_POINT('Ctrl Pts',(-1.87486989291484,-1.,0.427183828519102));
#26865=CARTESIAN_POINT('Ctrl Pts',(-1.86937803944323,-1.,0.424678177291359));
#26866=CARTESIAN_POINT('Ctrl Pts',(-1.86408083334028,-1.,0.422327307418275));
#26867=CARTESIAN_POINT('Ctrl Pts',(-1.85903281096686,-1.,0.420157287975619));
#26868=CARTESIAN_POINT('Ctrl Pts',(-1.85417632856234,-1.,0.418164129143534));
#26869=CARTESIAN_POINT('Ctrl Pts',(-1.84929312929882,-1.,0.416300022038864));
#26870=CARTESIAN_POINT('Ctrl Pts',(-1.8440575707371,-1.,0.41448743825434));
#26871=CARTESIAN_POINT('Ctrl Pts',(-1.83808953475839,-1.,0.412633125322161));
#26872=CARTESIAN_POINT('Ctrl Pts',(-1.83100408895216,-1.,0.410641256301675));
#26873=CARTESIAN_POINT('Ctrl Pts',(-1.8224702267854,-1.,0.408428948108533));
#26874=CARTESIAN_POINT('Ctrl Pts',(-1.81223801813988,-1.,0.405933518411838));
#26875=CARTESIAN_POINT('Ctrl Pts',(-1.80012077176221,-1.,0.403107976170441));
#26876=CARTESIAN_POINT('Ctrl Pts',(-1.78598826347533,-1.,0.39991940378308));
#26877=CARTESIAN_POINT('Ctrl Pts',(-1.7697556004756,-1.,0.39634619612042));
#26878=CARTESIAN_POINT('Ctrl Pts',(-1.75137405313962,-1.,0.392375812294307));
#26879=CARTESIAN_POINT('Ctrl Pts',(-1.7349317097561,-1.,0.388877023509191));
#26880=CARTESIAN_POINT('Ctrl Pts',(-1.72162022246158,-1.,0.38607079032701));
#26881=CARTESIAN_POINT('Ctrl Pts',(-1.71231062891958,-1.,0.384119047315542));
#26882=CARTESIAN_POINT('Ctrl Pts',(-1.7075470150345,-1.,0.383122945602004));
#26883=CARTESIAN_POINT('',(-1.74236521665491,-1.,0.163289472382896));
#26884=CARTESIAN_POINT('Origin',(0.,-1.,0.));
#26885=CARTESIAN_POINT('',(-2.19890268624765,-1.,0.069476445021958));
#26886=CARTESIAN_POINT('Ctrl Pts',(-1.74236521665491,-1.,0.163289472382896));
#26887=CARTESIAN_POINT('Ctrl Pts',(-1.7472034950333,-1.,0.163814161002002));
#26888=CARTESIAN_POINT('Ctrl Pts',(-1.75666056638427,-1.,0.164834765707158));
#26889=CARTESIAN_POINT('Ctrl Pts',(-1.77018771684844,-1.,0.1662793551464));
#26890=CARTESIAN_POINT('Ctrl Pts',(-1.7869064998507,-1.,0.168032772805197));
#26891=CARTESIAN_POINT('Ctrl Pts',(-1.80561530629706,-1.,0.169936923904608));
#26892=CARTESIAN_POINT('Ctrl Pts',(-1.82215766811545,-1.,0.171554770204119));
#26893=CARTESIAN_POINT('Ctrl Pts',(-1.83658380527692,-1.,0.1728894428919));
#26894=CARTESIAN_POINT('Ctrl Pts',(-1.8489811319852,-1.,0.173946627587731));
#26895=CARTESIAN_POINT('Ctrl Pts',(-1.85948367088837,-1.,0.17473525927603));
#26896=CARTESIAN_POINT('Ctrl Pts',(-1.86828349694799,-1.,0.175268337590758));
#26897=CARTESIAN_POINT('Ctrl Pts',(-1.87563767773588,-1.,0.175563480746485));
#26898=CARTESIAN_POINT('Ctrl Pts',(-1.88188663145367,-1.,0.175644148889698));
#26899=CARTESIAN_POINT('Ctrl Pts',(-1.88742606273259,-1.,0.175538155840648));
#26900=CARTESIAN_POINT('Ctrl Pts',(-1.892646301985,-1.,0.175274276190844));
#26901=CARTESIAN_POINT('Ctrl Pts',(-1.89788101117132,-1.,0.174879405091263));
#26902=CARTESIAN_POINT('Ctrl Pts',(-1.90335253862834,-1.,0.174375518661085));
#26903=CARTESIAN_POINT('Ctrl Pts',(-1.90911693975267,-1.,0.173776635257817));
#26904=CARTESIAN_POINT('Ctrl Pts',(-1.91511429159527,-1.,0.173090695383496));
#26905=CARTESIAN_POINT('Ctrl Pts',(-1.9212233439798,-1.,0.172321621259514));
#26906=CARTESIAN_POINT('Ctrl Pts',(-1.92731093582036,-1.,0.171471191532988));
#26907=CARTESIAN_POINT('Ctrl Pts',(-1.93329183155539,-1.,0.170541253116201));
#26908=CARTESIAN_POINT('Ctrl Pts',(-1.93915639211581,-1.,0.169534904817491));
#26909=CARTESIAN_POINT('Ctrl Pts',(-1.94493757756931,-1.,0.168455741607556));
#26910=CARTESIAN_POINT('Ctrl Pts',(-1.95069027794294,-1.,0.167307501784475));
#26911=CARTESIAN_POINT('Ctrl Pts',(-1.9564675971873,-1.,0.166093592002812));
#26912=CARTESIAN_POINT('Ctrl Pts',(-1.96229379940136,-1.,0.164816568920269));
#26913=CARTESIAN_POINT('Ctrl Pts',(-1.96816512677967,-1.,0.163478185457734));
#26914=CARTESIAN_POINT('Ctrl Pts',(-1.97406280235188,-1.,0.162079693556288));
#26915=CARTESIAN_POINT('Ctrl Pts',(-1.97996195437559,-1.,0.160622060784611));
#26916=CARTESIAN_POINT('Ctrl Pts',(-1.98584238283292,-1.,0.159106226437299));
#26917=CARTESIAN_POINT('Ctrl Pts',(-1.99169810931908,-1.,0.157533331459227));
#26918=CARTESIAN_POINT('Ctrl Pts',(-1.99753284771497,-1.,0.155904629548783));
#26919=CARTESIAN_POINT('Ctrl Pts',(-2.00335565310543,-1.,0.154221403049722));
#26920=CARTESIAN_POINT('Ctrl Pts',(-2.00917680318424,-1.,0.15248488362145));
#26921=CARTESIAN_POINT('Ctrl Pts',(-2.01500291940238,-1.,0.150696157673078));
#26922=CARTESIAN_POINT('Ctrl Pts',(-2.02083464969894,-1.,0.148856124775337));
#26923=CARTESIAN_POINT('Ctrl Pts',(-2.02666926182017,-1.,0.146965557332583));
#26924=CARTESIAN_POINT('Ctrl Pts',(-2.03250223739942,-1.,0.145025140186057));
#26925=CARTESIAN_POINT('Ctrl Pts',(-2.03832911025912,-1.,0.143035515058209));
#26926=CARTESIAN_POINT('Ctrl Pts',(-2.04414757947916,-1.,0.140997332152546));
#26927=CARTESIAN_POINT('Ctrl Pts',(-2.04995762001328,-1.,0.138911255368966));
#26928=CARTESIAN_POINT('Ctrl Pts',(-2.05576044414264,-1.,0.136777941218043));
#26929=CARTESIAN_POINT('Ctrl Pts',(-2.06155781517842,-1.,0.134598026192106));
#26930=CARTESIAN_POINT('Ctrl Pts',(-2.06735123910326,-1.,0.13237211154771));
#26931=CARTESIAN_POINT('Ctrl Pts',(-2.07314114713063,-1.,0.130100748328403));
#26932=CARTESIAN_POINT('Ctrl Pts',(-2.07892715110987,-1.,0.12778444527612));
#26933=CARTESIAN_POINT('Ctrl Pts',(-2.08470840653643,-1.,0.125423679412061));
#26934=CARTESIAN_POINT('Ctrl Pts',(-2.09048392424825,-1.,0.123018905621083));
#26935=CARTESIAN_POINT('Ctrl Pts',(-2.0962529286773,-1.,0.120570567965122));
#26936=CARTESIAN_POINT('Ctrl Pts',(-2.102015121329,-1.,0.118079107988355));
#26937=CARTESIAN_POINT('Ctrl Pts',(-2.10777050261309,-1.,0.115544957687926));
#26938=CARTESIAN_POINT('Ctrl Pts',(-2.11351924490306,-1.,0.112968534419737));
#26939=CARTESIAN_POINT('Ctrl Pts',(-2.11926155590865,-1.,0.110350236135025));
#26940=CARTESIAN_POINT('Ctrl Pts',(-2.12499752307,-1.,0.10769043523109));
#26941=CARTESIAN_POINT('Ctrl Pts',(-2.13072704887293,-1.,0.104989479152739));
#26942=CARTESIAN_POINT('Ctrl Pts',(-2.13644992667165,-1.,0.1022477005561));
#26943=CARTESIAN_POINT('Ctrl Pts',(-2.14216588396025,-1.,0.0994654261990914));
#26944=CARTESIAN_POINT('Ctrl Pts',(-2.14787463531795,-1.,0.0966429852305457));
#26945=CARTESIAN_POINT('Ctrl Pts',(-2.1535759397817,-1.,0.0937807218867642));
#26946=CARTESIAN_POINT('Ctrl Pts',(-2.15926961544516,-1.,0.0908789888107264));
#26947=CARTESIAN_POINT('Ctrl Pts',(-2.16495552645014,-1.,0.0879381291386921));
#26948=CARTESIAN_POINT('Ctrl Pts',(-2.17063357870952,-1.,0.0849584620835371));
#26949=CARTESIAN_POINT('Ctrl Pts',(-2.176303712113,-1.,0.0819402680872764));
#26950=CARTESIAN_POINT('Ctrl Pts',(-2.18196589448887,-1.,0.0788837727685241));
#26951=CARTESIAN_POINT('Ctrl Pts',(-2.1876201139953,-1.,0.0757891465836146));
#26952=CARTESIAN_POINT('Ctrl Pts',(-2.19213712013662,-1.,0.0732830357306724));
#26953=CARTESIAN_POINT('Ctrl Pts',(-2.19552129484002,-1.,0.0713863779526153));
#26954=CARTESIAN_POINT('Ctrl Pts',(-2.19777582085423,-1.,0.0701143536325489));
#26955=CARTESIAN_POINT('Ctrl Pts',(-2.19890268624765,-1.,0.069476445021958));
#26956=CARTESIAN_POINT('',(-2.19890268624765,-1.,-0.0694764450219585));
#26957=CARTESIAN_POINT('',(-2.19890268624765,-1.,0.069476445021958));
#26958=CARTESIAN_POINT('',(-1.74236521665491,-1.,-0.163289472382896));
#26959=CARTESIAN_POINT('Ctrl Pts',(-2.19890268624765,-1.,-0.0694764450219585));
#26960=CARTESIAN_POINT('Ctrl Pts',(-2.19777582085261,-1.,-0.0701143536324927));
#26961=CARTESIAN_POINT('Ctrl Pts',(-2.19552129483562,-1.,-0.0713863779524629));
#26962=CARTESIAN_POINT('Ctrl Pts',(-2.19213712012956,-1.,-0.0732830357304277));
#26963=CARTESIAN_POINT('Ctrl Pts',(-2.1876201139874,-1.,-0.0757891465833413));
#26964=CARTESIAN_POINT('Ctrl Pts',(-2.18196589448304,-1.,-0.0788837727683229));
#26965=CARTESIAN_POINT('Ctrl Pts',(-2.1763037121106,-1.,-0.0819402680871941));
#26966=CARTESIAN_POINT('Ctrl Pts',(-2.17063357871031,-1.,-0.0849584620835644));
#26967=CARTESIAN_POINT('Ctrl Pts',(-2.16495552645275,-1.,-0.0879381291387824));
#26968=CARTESIAN_POINT('Ctrl Pts',(-2.15926961544808,-1.,-0.0908789888108267));
#26969=CARTESIAN_POINT('Ctrl Pts',(-2.15357593978377,-1.,-0.0937807218868346));
#26970=CARTESIAN_POINT('Ctrl Pts',(-2.14787463531864,-1.,-0.096642985230569));
#26971=CARTESIAN_POINT('Ctrl Pts',(-2.14216588395974,-1.,-0.0994654261990744));
#26972=CARTESIAN_POINT('Ctrl Pts',(-2.13644992667052,-1.,-0.102247700556064));
#26973=CARTESIAN_POINT('Ctrl Pts',(-2.1307270488718,-1.,-0.104989479152703));
#26974=CARTESIAN_POINT('Ctrl Pts',(-2.12499752306927,-1.,-0.107690435231068));
#26975=CARTESIAN_POINT('Ctrl Pts',(-2.11926155590849,-1.,-0.11035023613502));
#26976=CARTESIAN_POINT('Ctrl Pts',(-2.11351924490335,-1.,-0.112968534419746));
#26977=CARTESIAN_POINT('Ctrl Pts',(-2.10777050261359,-1.,-0.11554495768794));
#26978=CARTESIAN_POINT('Ctrl Pts',(-2.10201512132945,-1.,-0.118079107988368));
#26979=CARTESIAN_POINT('Ctrl Pts',(-2.09625292867756,-1.,-0.120570567965129));
#26980=CARTESIAN_POINT('Ctrl Pts',(-2.09048392424826,-1.,-0.123018905621083));
#26981=CARTESIAN_POINT('Ctrl Pts',(-2.08470840653628,-1.,-0.125423679412058));
#26982=CARTESIAN_POINT('Ctrl Pts',(-2.07892715110967,-1.,-0.127784445276116));
#26983=CARTESIAN_POINT('Ctrl Pts',(-2.07314114713047,-1.,-0.130100748328401));
#26984=CARTESIAN_POINT('Ctrl Pts',(-2.06735123910319,-1.,-0.13237211154771));
#26985=CARTESIAN_POINT('Ctrl Pts',(-2.06155781517844,-1.,-0.134598026192107));
#26986=CARTESIAN_POINT('Ctrl Pts',(-2.0557604441427,-1.,-0.136777941218044));
#26987=CARTESIAN_POINT('Ctrl Pts',(-2.04995762001333,-1.,-0.138911255368966));
#26988=CARTESIAN_POINT('Ctrl Pts',(-2.04414757947919,-1.,-0.140997332152545));
#26989=CARTESIAN_POINT('Ctrl Pts',(-2.03832911025913,-1.,-0.143035515058208));
#26990=CARTESIAN_POINT('Ctrl Pts',(-2.03250223739941,-1.,-0.145025140186058));
#26991=CARTESIAN_POINT('Ctrl Pts',(-2.02666926182017,-1.,-0.146965557332586));
#26992=CARTESIAN_POINT('Ctrl Pts',(-2.02083464969897,-1.,-0.148856124775343));
#26993=CARTESIAN_POINT('Ctrl Pts',(-2.01500291940243,-1.,-0.150696157673084));
#26994=CARTESIAN_POINT('Ctrl Pts',(-2.00917680318426,-1.,-0.152484883621452));
#26995=CARTESIAN_POINT('Ctrl Pts',(-2.00335565310539,-1.,-0.154221403049719));
#26996=CARTESIAN_POINT('Ctrl Pts',(-1.99753284771487,-1.,-0.155904629548775));
#26997=CARTESIAN_POINT('Ctrl Pts',(-1.99169810931893,-1.,-0.157533331459215));
#26998=CARTESIAN_POINT('Ctrl Pts',(-1.98584238283279,-1.,-0.159106226437289));
#26999=CARTESIAN_POINT('Ctrl Pts',(-1.97996195437557,-1.,-0.16062206078461));
#27000=CARTESIAN_POINT('Ctrl Pts',(-1.97406280235204,-1.,-0.162079693556302));
#27001=CARTESIAN_POINT('Ctrl Pts',(-1.96816512678,-1.,-0.16347818545776));
#27002=CARTESIAN_POINT('Ctrl Pts',(-1.96229379940174,-1.,-0.1648165689203));
#27003=CARTESIAN_POINT('Ctrl Pts',(-1.95646759718755,-1.,-0.166093592002833));
#27004=CARTESIAN_POINT('Ctrl Pts',(-1.95069027794286,-1.,-0.167307501784469));
#27005=CARTESIAN_POINT('Ctrl Pts',(-1.94493757756879,-1.,-0.168455741607516));
#27006=CARTESIAN_POINT('Ctrl Pts',(-1.93915639211497,-1.,-0.169534904817425));
#27007=CARTESIAN_POINT('Ctrl Pts',(-1.93329183155455,-1.,-0.170541253116136));
#27008=CARTESIAN_POINT('Ctrl Pts',(-1.92731093582,-1.,-0.17147119153296));
#27009=CARTESIAN_POINT('Ctrl Pts',(-1.92122334398034,-1.,-0.172321621259557));
#27010=CARTESIAN_POINT('Ctrl Pts',(-1.91511429159681,-1.,-0.173090695383619));
#27011=CARTESIAN_POINT('Ctrl Pts',(-1.90911693975475,-1.,-0.173776635257984));
#27012=CARTESIAN_POINT('Ctrl Pts',(-1.90335253863003,-1.,-0.174375518661222));
#27013=CARTESIAN_POINT('Ctrl Pts',(-1.89788101117148,-1.,-0.174879405091277));
#27014=CARTESIAN_POINT('Ctrl Pts',(-1.89264630198279,-1.,-0.175274276190664));
#27015=CARTESIAN_POINT('Ctrl Pts',(-1.88742606272818,-1.,-0.175538155840286));
#27016=CARTESIAN_POINT('Ctrl Pts',(-1.88188663144846,-1.,-0.175644148889271));
#27017=CARTESIAN_POINT('Ctrl Pts',(-1.87563767773249,-1.,-0.175563480746205));
#27018=CARTESIAN_POINT('Ctrl Pts',(-1.86828349694972,-1.,-0.175268337590901));
#27019=CARTESIAN_POINT('Ctrl Pts',(-1.85948367089838,-1.,-0.174735259276856));
#27020=CARTESIAN_POINT('Ctrl Pts',(-1.84898113200543,-1.,-0.173946627589401));
#27021=CARTESIAN_POINT('Ctrl Pts',(-1.83658380530747,-1.,-0.17288944289442));
#27022=CARTESIAN_POINT('Ctrl Pts',(-1.82215766815414,-1.,-0.171554770207306));
#27023=CARTESIAN_POINT('Ctrl Pts',(-1.80561530633924,-1.,-0.169936923908078));
#27024=CARTESIAN_POINT('Ctrl Pts',(-1.78690649988931,-1.,-0.16803277280837));
#27025=CARTESIAN_POINT('Ctrl Pts',(-1.77018771687692,-1.,-0.166279355148738));
#27026=CARTESIAN_POINT('Ctrl Pts',(-1.75666056640041,-1.,-0.164834765708484));
#27027=CARTESIAN_POINT('Ctrl Pts',(-1.74720349503904,-1.,-0.163814161002474));
#27028=CARTESIAN_POINT('Ctrl Pts',(-1.74236521665491,-1.,-0.163289472382896));
#27029=CARTESIAN_POINT('',(-1.7075470150345,-1.,-0.383122945602004));
#27030=CARTESIAN_POINT('Origin',(0.,-1.,0.));
#27031=CARTESIAN_POINT('',(-2.11275013067528,-1.,-0.61342227326009));
#27032=CARTESIAN_POINT('Ctrl Pts',(-1.7075470150345,-1.,-0.383122945602004));
#27033=CARTESIAN_POINT('Ctrl Pts',(-1.71231062891398,-1.,-0.384119047314215));
#27034=CARTESIAN_POINT('Ctrl Pts',(-1.72162022244582,-1.,-0.386070790323281));
#27035=CARTESIAN_POINT('Ctrl Pts',(-1.73493170972829,-1.,-0.388877023502615));
#27036=CARTESIAN_POINT('Ctrl Pts',(-1.75137405310193,-1.,-0.392375812285395));
#27037=CARTESIAN_POINT('Ctrl Pts',(-1.76975560043442,-1.,-0.396346196110688));
#27038=CARTESIAN_POINT('Ctrl Pts',(-1.78598826343754,-1.,-0.399919403774155));
#27039=CARTESIAN_POINT('Ctrl Pts',(-1.80012077173238,-1.,-0.403107976163396));
#27040=CARTESIAN_POINT('Ctrl Pts',(-1.81223801812013,-1.,-0.405933518407175));
#27041=CARTESIAN_POINT('Ctrl Pts',(-1.82247022677562,-1.,-0.408428948106227));
#27042=CARTESIAN_POINT('Ctrl Pts',(-1.83100408895047,-1.,-0.410641256301276));
#27043=CARTESIAN_POINT('Ctrl Pts',(-1.8380895347617,-1.,-0.412633125322945));
#27044=CARTESIAN_POINT('Ctrl Pts',(-1.84405757074218,-1.,-0.414487438255542));
#27045=CARTESIAN_POINT('Ctrl Pts',(-1.84929312930314,-1.,-0.416300022039885));
#27046=CARTESIAN_POINT('Ctrl Pts',(-1.8541763285645,-1.,-0.418164129144045));
#27047=CARTESIAN_POINT('Ctrl Pts',(-1.8590328109667,-1.,-0.420157287975583));
#27048=CARTESIAN_POINT('Ctrl Pts',(-1.86408083333863,-1.,-0.422327307417884));
#27049=CARTESIAN_POINT('Ctrl Pts',(-1.8693780394412,-1.,-0.424678177290876));
#27050=CARTESIAN_POINT('Ctrl Pts',(-1.87486989291333,-1.,-0.427183828518743));
#27051=CARTESIAN_POINT('Ctrl Pts',(-1.88044229001778,-1.,-0.429803062482217));
#27052=CARTESIAN_POINT('Ctrl Pts',(-1.88596913666828,-1.,-0.432493038548833));
#27053=CARTESIAN_POINT('Ctrl Pts',(-1.89136993975585,-1.,-0.43522566096358));
#27054=CARTESIAN_POINT('Ctrl Pts',(-1.89663648956549,-1.,-0.437995003948443));
#27055=CARTESIAN_POINT('Ctrl Pts',(-1.90180124389137,-1.,-0.44080783370416));
#27056=CARTESIAN_POINT('Ctrl Pts',(-1.90691756144906,-1.,-0.44367755684917));
#27057=CARTESIAN_POINT('Ctrl Pts',(-1.91203699981095,-1.,-0.446617343485651));
#27058=CARTESIAN_POINT('Ctrl Pts',(-1.91718342555717,-1.,-0.449632260106572));
#27059=CARTESIAN_POINT('Ctrl Pts',(-1.9223538064847,-1.,-0.452719478359356));
#27060=CARTESIAN_POINT('Ctrl Pts',(-1.92753067150461,-1.,-0.455872005174335));
#27061=CARTESIAN_POINT('Ctrl Pts',(-1.93269066517936,-1.,-0.459081234547931));
#27062=CARTESIAN_POINT('Ctrl Pts',(-1.93781486640834,-1.,-0.462340031009087));
#27063=CARTESIAN_POINT('Ctrl Pts',(-1.94289794196205,-1.,-0.465645462026064));
#27064=CARTESIAN_POINT('Ctrl Pts',(-1.94794381136524,-1.,-0.468997482913158));
#27065=CARTESIAN_POINT('Ctrl Pts',(-1.95296148278136,-1.,-0.472397672264079));
#27066=CARTESIAN_POINT('Ctrl Pts',(-1.95796111148175,-1.,-0.475848034683171));
#27067=CARTESIAN_POINT('Ctrl Pts',(-1.96294933055938,-1.,-0.479349583074846));
#27068=CARTESIAN_POINT('Ctrl Pts',(-1.96792703422358,-1.,-0.482901662120686));
#27069=CARTESIAN_POINT('Ctrl Pts',(-1.97289186263272,-1.,-0.486502692907661));
#27070=CARTESIAN_POINT('Ctrl Pts',(-1.97783973019229,-1.,-0.490150627860955));
#27071=CARTESIAN_POINT('Ctrl Pts',(-1.9827665876182,-1.,-0.493843476541492));
#27072=CARTESIAN_POINT('Ctrl Pts',(-1.98767044752929,-1.,-0.497579909545564));
#27073=CARTESIAN_POINT('Ctrl Pts',(-1.9925514912615,-1.,-0.501359287727129));
#27074=CARTESIAN_POINT('Ctrl Pts',(-1.99741107463567,-1.,-0.505181361323011));
#27075=CARTESIAN_POINT('Ctrl Pts',(-2.00225107134733,-1.,-0.509046069886152));
#27076=CARTESIAN_POINT('Ctrl Pts',(-2.00707309946955,-1.,-0.512953306961813));
#27077=CARTESIAN_POINT('Ctrl Pts',(-2.01187773939257,-1.,-0.516902681728733));
#27078=CARTESIAN_POINT('Ctrl Pts',(-2.01666477917305,-1.,-0.520893590399428));
#27079=CARTESIAN_POINT('Ctrl Pts',(-2.02143356304712,-1.,-0.524925318333518));
#27080=CARTESIAN_POINT('Ctrl Pts',(-2.02618329083289,-1.,-0.52899712724191));
#27081=CARTESIAN_POINT('Ctrl Pts',(-2.03091336214401,-1.,-0.533108355132905));
#27082=CARTESIAN_POINT('Ctrl Pts',(-2.03562362953993,-1.,-0.537258489833134));
#27083=CARTESIAN_POINT('Ctrl Pts',(-2.0403142269048,-1.,-0.54144712061552));
#27084=CARTESIAN_POINT('Ctrl Pts',(-2.0449854471456,-1.,-0.545673903817348));
#27085=CARTESIAN_POINT('Ctrl Pts',(-2.04963761077974,-1.,-0.549938525150342));
#27086=CARTESIAN_POINT('Ctrl Pts',(-2.05427091604482,-1.,-0.554240657464109));
#27087=CARTESIAN_POINT('Ctrl Pts',(-2.05888537756571,-1.,-0.558579940185467));
#27088=CARTESIAN_POINT('Ctrl Pts',(-2.06348090160697,-1.,-0.562955993082574));
#27089=CARTESIAN_POINT('Ctrl Pts',(-2.06805732997383,-1.,-0.567368421181229));
#27090=CARTESIAN_POINT('Ctrl Pts',(-2.07261449292757,-1.,-0.571816823242411));
#27091=CARTESIAN_POINT('Ctrl Pts',(-2.07715226767361,-1.,-0.576300797416274));
#27092=CARTESIAN_POINT('Ctrl Pts',(-2.08167059018138,-1.,-0.580819952107257));
#27093=CARTESIAN_POINT('Ctrl Pts',(-2.086169437277,-1.,-0.585373918990895));
#27094=CARTESIAN_POINT('Ctrl Pts',(-2.09064881812053,-1.,-0.589962365403189));
#27095=CARTESIAN_POINT('Ctrl Pts',(-2.09510876220501,-1.,-0.594585006052823));
#27096=CARTESIAN_POINT('Ctrl Pts',(-2.09954930865331,-1.,-0.599241616422144));
#27097=CARTESIAN_POINT('Ctrl Pts',(-2.10397049887709,-1.,-0.603932030738212));
#27098=CARTESIAN_POINT('Ctrl Pts',(-2.10749199615859,-1.,-0.607711315456826));
#27099=CARTESIAN_POINT('Ctrl Pts',(-2.11012443807661,-1.,-0.610560911691113));
#27100=CARTESIAN_POINT('Ctrl Pts',(-2.11187554260142,-1.,-0.61246736556225));
#27101=CARTESIAN_POINT('Ctrl Pts',(-2.11275013067528,-1.,-0.61342227326009));
#27102=CARTESIAN_POINT('',(-2.0698113262342,-1.,-0.745574324794401));
#27103=CARTESIAN_POINT('',(-2.11275013067528,-1.,-0.61342227326009));
#27104=CARTESIAN_POINT('',(-1.60662857109684,-1.,-0.693717979106306));
#27105=CARTESIAN_POINT('Ctrl Pts',(-2.0698113262342,-1.,-0.745574324794401));
#27106=CARTESIAN_POINT('Ctrl Pts',(-2.06854248895575,-1.,-0.74583279137781));
#27107=CARTESIAN_POINT('Ctrl Pts',(-2.06600523016401,-1.,-0.746345871542695));
#27108=CARTESIAN_POINT('Ctrl Pts',(-2.06220058927162,-1.,-0.747103932785504));
#27109=CARTESIAN_POINT('Ctrl Pts',(-2.05713023030263,-1.,-0.748091554181101));
#27110=CARTESIAN_POINT('Ctrl Pts',(-2.05079645591606,-1.,-0.749287468663053));
#27111=CARTESIAN_POINT('Ctrl Pts',(-2.04446689147754,-1.,-0.750444657874758));
#27112=CARTESIAN_POINT('Ctrl Pts',(-2.03814160092173,-1.,-0.751562963361383));
#27113=CARTESIAN_POINT('Ctrl Pts',(-2.03182068456467,-1.,-0.752642180488104));
#27114=CARTESIAN_POINT('Ctrl Pts',(-2.02550428623587,-1.,-0.753682061113765));
#27115=CARTESIAN_POINT('Ctrl Pts',(-2.01919259406003,-1.,-0.75468233072352));
#27116=CARTESIAN_POINT('Ctrl Pts',(-2.01288584328149,-1.,-0.7556427049581));
#27117=CARTESIAN_POINT('Ctrl Pts',(-2.00658431587682,-1.,-0.756562904646496));
#27118=CARTESIAN_POINT('Ctrl Pts',(-2.00028834739072,-1.,-0.757442676862341));
#27119=CARTESIAN_POINT('Ctrl Pts',(-1.9939983109871,-1.,-0.758281796766377));
#27120=CARTESIAN_POINT('Ctrl Pts',(-1.98771456680806,-1.,-0.759080037802242));
#27121=CARTESIAN_POINT('Ctrl Pts',(-1.98143741418156,-1.,-0.759837147452135));
#27122=CARTESIAN_POINT('Ctrl Pts',(-1.97516705321521,-1.,-0.760552825409855));
#27123=CARTESIAN_POINT('Ctrl Pts',(-1.96890351582545,-1.,-0.761226690483986));
#27124=CARTESIAN_POINT('Ctrl Pts',(-1.96264672744229,-1.,-0.761858300014575));
#27125=CARTESIAN_POINT('Ctrl Pts',(-1.95639665309893,-1.,-0.762447203806263));
#27126=CARTESIAN_POINT('Ctrl Pts',(-1.95015342590025,-1.,-0.762992990878774));
#27127=CARTESIAN_POINT('Ctrl Pts',(-1.94391746617626,-1.,-0.76349533353858));
#27128=CARTESIAN_POINT('Ctrl Pts',(-1.93768964875867,-1.,-0.763954049121393));
#27129=CARTESIAN_POINT('Ctrl Pts',(-1.93147105496367,-1.,-0.764369010673889));
#27130=CARTESIAN_POINT('Ctrl Pts',(-1.92526263537041,-1.,-0.764740025488189));
#27131=CARTESIAN_POINT('Ctrl Pts',(-1.91906491634197,-1.,-0.765066729667095));
#27132=CARTESIAN_POINT('Ctrl Pts',(-1.91287765805174,-1.,-0.765348465884739));
#27133=CARTESIAN_POINT('Ctrl Pts',(-1.90669961402362,-1.,-0.765584196937936));
#27134=CARTESIAN_POINT('Ctrl Pts',(-1.90052930393599,-1.,-0.765772772593395));
#27135=CARTESIAN_POINT('Ctrl Pts',(-1.89436577771389,-1.,-0.765913193856979));
#27136=CARTESIAN_POINT('Ctrl Pts',(-1.88820926433409,-1.,-0.76600483706209));
#27137=CARTESIAN_POINT('Ctrl Pts',(-1.88206215302561,-1.,-0.766047794851868));
#27138=CARTESIAN_POINT('Ctrl Pts',(-1.87592888967886,-1.,-0.766042837036759));
#27139=CARTESIAN_POINT('Ctrl Pts',(-1.86981398314345,-1.,-0.765990708546111));
#27140=CARTESIAN_POINT('Ctrl Pts',(-1.86372027063314,-1.,-0.765891519092557));
#27141=CARTESIAN_POINT('Ctrl Pts',(-1.85764741390391,-1.,-0.765744212909305));
#27142=CARTESIAN_POINT('Ctrl Pts',(-1.85158945130054,-1.,-0.765545710619023));
#27143=CARTESIAN_POINT('Ctrl Pts',(-1.8455369887591,-1.,-0.765291664861971));
#27144=CARTESIAN_POINT('Ctrl Pts',(-1.83948181064823,-1.,-0.764978057881687));
#27145=CARTESIAN_POINT('Ctrl Pts',(-1.8334207722714,-1.,-0.764602549687845));
#27146=CARTESIAN_POINT('Ctrl Pts',(-1.8273599120008,-1.,-0.764165902606055));
#27147=CARTESIAN_POINT('Ctrl Pts',(-1.82131873145297,-1.,-0.763673465462854));
#27148=CARTESIAN_POINT('Ctrl Pts',(-1.81532118405566,-1.,-0.763132003836783));
#27149=CARTESIAN_POINT('Ctrl Pts',(-1.80938551463989,-1.,-0.762546129464036));
#27150=CARTESIAN_POINT('Ctrl Pts',(-1.80351583877334,-1.,-0.761915336443515));
#27151=CARTESIAN_POINT('Ctrl Pts',(-1.79768986997735,-1.,-0.761229695230359));
#27152=CARTESIAN_POINT('Ctrl Pts',(-1.79185815610802,-1.,-0.760469555880425));
#27153=CARTESIAN_POINT('Ctrl Pts',(-1.78596964884526,-1.,-0.759614401109868));
#27154=CARTESIAN_POINT('Ctrl Pts',(-1.77999411220912,-1.,-0.75865062667738));
#27155=CARTESIAN_POINT('Ctrl Pts',(-1.77394167108342,-1.,-0.757578264077238));
#27156=CARTESIAN_POINT('Ctrl Pts',(-1.76789396003141,-1.,-0.756421896028403));
#27157=CARTESIAN_POINT('Ctrl Pts',(-1.7619781724032,-1.,-0.755220979975262));
#27158=CARTESIAN_POINT('Ctrl Pts',(-1.75631083600175,-1.,-0.75400925402848));
#27159=CARTESIAN_POINT('Ctrl Pts',(-1.75095139468809,-1.,-0.752797683531377));
#27160=CARTESIAN_POINT('Ctrl Pts',(-1.74585086852298,-1.,-0.751555614163629));
#27161=CARTESIAN_POINT('Ctrl Pts',(-1.74080458266705,-1.,-0.75019343597954));
#27162=CARTESIAN_POINT('Ctrl Pts',(-1.73550351679848,-1.,-0.748582462954854));
#27163=CARTESIAN_POINT('Ctrl Pts',(-1.72958533647399,-1.,-0.746574710096436));
#27164=CARTESIAN_POINT('Ctrl Pts',(-1.7226822991693,-1.,-0.744021445433764));
#27165=CARTESIAN_POINT('Ctrl Pts',(-1.71447789751927,-1.,-0.740795162032087));
#27166=CARTESIAN_POINT('Ctrl Pts',(-1.70473309006121,-1.,-0.736799665724771));
#27167=CARTESIAN_POINT('Ctrl Pts',(-1.69326921975743,-1.,-0.731963238697195));
#27168=CARTESIAN_POINT('Ctrl Pts',(-1.67996158455503,-1.,-0.726235967997433));
#27169=CARTESIAN_POINT('Ctrl Pts',(-1.6647288055568,-1.,-0.719585433804282));
#27170=CARTESIAN_POINT('Ctrl Pts',(-1.64752408832016,-1.,-0.711993139355394));
#27171=CARTESIAN_POINT('Ctrl Pts',(-1.63216541664676,-1.,-0.705159151988319));
#27172=CARTESIAN_POINT('Ctrl Pts',(-1.61974673472612,-1.,-0.699605146405088));
#27173=CARTESIAN_POINT('Ctrl Pts',(-1.61106790958151,-1.,-0.695712097881194));
#27174=CARTESIAN_POINT('Ctrl Pts',(-1.60662857109684,-1.,-0.693717979106306));
#27175=CARTESIAN_POINT('',(-1.5055822144029,-1.,-0.892032620296855));
#27176=CARTESIAN_POINT('Origin',(0.,-1.,0.));
#27177=CARTESIAN_POINT('',(-1.81978687191668,-1.,-1.23627494547115));
#27178=CARTESIAN_POINT('Ctrl Pts',(-1.5055822144029,-1.,-0.892032620296855));
#27179=CARTESIAN_POINT('Ctrl Pts',(-1.50980486806688,-1.,-0.894452006964543));
#27180=CARTESIAN_POINT('Ctrl Pts',(-1.51805569590094,-1.,-0.899185047483511));
#27181=CARTESIAN_POINT('Ctrl Pts',(-1.52984849887993,-1.,-0.905967409625651));
#27182=CARTESIAN_POINT('Ctrl Pts',(-1.54440491149498,-1.,-0.914375919026456));
#27183=CARTESIAN_POINT('Ctrl Pts',(-1.56065988578893,-1.,-0.923832188944341));
#27184=CARTESIAN_POINT('Ctrl Pts',(-1.57499388382243,-1.,-0.932246680108685));
#27185=CARTESIAN_POINT('Ctrl Pts',(-1.58744937487176,-1.,-0.939646377893399));
#27186=CARTESIAN_POINT('Ctrl Pts',(-1.59810042043673,-1.,-0.946078063315257));
#27187=CARTESIAN_POINT('Ctrl Pts',(-1.60706069896936,-1.,-0.951613284356035));
#27188=CARTESIAN_POINT('Ctrl Pts',(-1.61449324337085,-1.,-0.956354422920671));
#27189=CARTESIAN_POINT('Ctrl Pts',(-1.62061638140221,-1.,-0.960438326101729));
#27190=CARTESIAN_POINT('Ctrl Pts',(-1.62571930670187,-1.,-0.964046107040536));
#27191=CARTESIAN_POINT('Ctrl Pts',(-1.63013849959461,-1.,-0.967387853230345));
#27192=CARTESIAN_POINT('Ctrl Pts',(-1.63420665729798,-1.,-0.970669715997509));
#27193=CARTESIAN_POINT('Ctrl Pts',(-1.63820952658144,-1.,-0.974066058287418));
#27194=CARTESIAN_POINT('Ctrl Pts',(-1.64233990826687,-1.,-0.977689794119416));
#27195=CARTESIAN_POINT('Ctrl Pts',(-1.64665139190656,-1.,-0.981562530939489));
#27196=CARTESIAN_POINT('Ctrl Pts',(-1.65110016612638,-1.,-0.985642622920821));
#27197=CARTESIAN_POINT('Ctrl Pts',(-1.65559044289699,-1.,-0.989855627854165));
#27198=CARTESIAN_POINT('Ctrl Pts',(-1.66001553809947,-1.,-0.994121836661306));
#27199=CARTESIAN_POINT('Ctrl Pts',(-1.66430758030376,-1.,-0.998389654952758));
#27200=CARTESIAN_POINT('Ctrl Pts',(-1.66846059277303,-1.,-1.00265091003727));
#27201=CARTESIAN_POINT('Ctrl Pts',(-1.67250335383293,-1.,-1.00692206696414));
#27202=CARTESIAN_POINT('Ctrl Pts',(-1.67648246776464,-1.,-1.01123236493511));
#27203=CARTESIAN_POINT('Ctrl Pts',(-1.68044289894798,-1.,-1.01561026162773));
#27204=CARTESIAN_POINT('Ctrl Pts',(-1.68440578021706,-1.,-1.02006795074201));
#27205=CARTESIAN_POINT('Ctrl Pts',(-1.68836910178447,-1.,-1.02460180535255));
#27206=CARTESIAN_POINT('Ctrl Pts',(-1.69231840863458,-1.,-1.02919977579147));
#27207=CARTESIAN_POINT('Ctrl Pts',(-1.69623414782771,-1.,-1.03384646003588));
#27208=CARTESIAN_POINT('Ctrl Pts',(-1.70010052930962,-1.,-1.03852922490789));
#27209=CARTESIAN_POINT('Ctrl Pts',(-1.70391338707982,-1.,-1.04324363334554));
#27210=CARTESIAN_POINT('Ctrl Pts',(-1.70767646263649,-1.,-1.04799085404995));
#27211=CARTESIAN_POINT('Ctrl Pts',(-1.71139783543989,-1.,-1.05277517202855));
#27212=CARTESIAN_POINT('Ctrl Pts',(-1.7150865442702,-1.,-1.05760163192479));
#27213=CARTESIAN_POINT('Ctrl Pts',(-1.71874858456904,-1.,-1.06247324680647));
#27214=CARTESIAN_POINT('Ctrl Pts',(-1.72238500928453,-1.,-1.06738966975462));
#27215=CARTESIAN_POINT('Ctrl Pts',(-1.72599406198488,-1.,-1.07234866990252));
#27216=CARTESIAN_POINT('Ctrl Pts',(-1.72957248977424,-1.,-1.0773470373727));
#27217=CARTESIAN_POINT('Ctrl Pts',(-1.73311705663407,-1.,-1.08238162784749));
#27218=CARTESIAN_POINT('Ctrl Pts',(-1.73662628326091,-1.,-1.08745056285427));
#27219=CARTESIAN_POINT('Ctrl Pts',(-1.74010053962247,-1.,-1.09255329056493));
#27220=CARTESIAN_POINT('Ctrl Pts',(-1.74354119236208,-1.,-1.09768999241225));
#27221=CARTESIAN_POINT('Ctrl Pts',(-1.74695004214923,-1.,-1.10286118991143));
#27222=CARTESIAN_POINT('Ctrl Pts',(-1.7503286607592,-1.,-1.10806728183007));
#27223=CARTESIAN_POINT('Ctrl Pts',(-1.7536777209463,-1.,-1.11330807582551));
#27224=CARTESIAN_POINT('Ctrl Pts',(-1.75699720772105,-1.,-1.11858293216763));
#27225=CARTESIAN_POINT('Ctrl Pts',(-1.76028671825096,-1.,-1.12389096855086));
#27226=CARTESIAN_POINT('Ctrl Pts',(-1.7635457196617,-1.,-1.12923123555075));
#27227=CARTESIAN_POINT('Ctrl Pts',(-1.76677384551862,-1.,-1.1346029180462));
#27228=CARTESIAN_POINT('Ctrl Pts',(-1.76997111386769,-1.,-1.14000548336975));
#27229=CARTESIAN_POINT('Ctrl Pts',(-1.77313777896194,-1.,-1.1454385822692));
#27230=CARTESIAN_POINT('Ctrl Pts',(-1.7762742255701,-1.,-1.15090197841515));
#27231=CARTESIAN_POINT('Ctrl Pts',(-1.77938085564275,-1.,-1.15639547194698));
#27232=CARTESIAN_POINT('Ctrl Pts',(-1.78245795881009,-1.,-1.16191881298499));
#27233=CARTESIAN_POINT('Ctrl Pts',(-1.78550566040443,-1.,-1.16747166312303));
#27234=CARTESIAN_POINT('Ctrl Pts',(-1.78852398877616,-1.,-1.17305363177328));
#27235=CARTESIAN_POINT('Ctrl Pts',(-1.79151291552689,-1.,-1.17866429440809));
#27236=CARTESIAN_POINT('Ctrl Pts',(-1.79447240321515,-1.,-1.18430321697432));
#27237=CARTESIAN_POINT('Ctrl Pts',(-1.79740245923478,-1.,-1.18996997934445));
#27238=CARTESIAN_POINT('Ctrl Pts',(-1.80030314369879,-1.,-1.19566418930242));
#27239=CARTESIAN_POINT('Ctrl Pts',(-1.80317454838603,-1.,-1.20138548938974));
#27240=CARTESIAN_POINT('Ctrl Pts',(-1.80601678480707,-1.,-1.20713356605475));
#27241=CARTESIAN_POINT('Ctrl Pts',(-1.80882996917129,-1.,-1.21290815708314));
#27242=CARTESIAN_POINT('Ctrl Pts',(-1.81161420806656,-1.,-1.21870906103557));
#27243=CARTESIAN_POINT('Ctrl Pts',(-1.81436959210434,-1.,-1.2245361330495));
#27244=CARTESIAN_POINT('Ctrl Pts',(-1.8165508718364,-1.,-1.2292186489137));
#27245=CARTESIAN_POINT('Ctrl Pts',(-1.81817389921279,-1.,-1.2327422452705));
#27246=CARTESIAN_POINT('Ctrl Pts',(-1.81925017193666,-1.,-1.23509651170476));
#27247=CARTESIAN_POINT('Ctrl Pts',(-1.81978687191668,-1.,-1.23627494547115));
#27248=CARTESIAN_POINT('',(-1.73811241238545,-1.,-1.34869019493419));
#27249=CARTESIAN_POINT('',(-1.81978687191668,-1.,-1.23627494547115));
#27250=CARTESIAN_POINT('',(-1.31362392696032,-1.,-1.15624053661742));
#27251=CARTESIAN_POINT('Ctrl Pts',(-1.73811241238545,-1.,-1.34869019493419));
#27252=CARTESIAN_POINT('Ctrl Pts',(-1.73682580585691,-1.,-1.34854391898045));
#27253=CARTESIAN_POINT('Ctrl Pts',(-1.73425417885907,-1.,-1.34824783112887));
#27254=CARTESIAN_POINT('Ctrl Pts',(-1.7304014965394,-1.,-1.34779309152035));
#27255=CARTESIAN_POINT('Ctrl Pts',(-1.72527410680674,-1.,-1.34716554819527));
#27256=CARTESIAN_POINT('Ctrl Pts',(-1.7188807715049,-1.,-1.34634568653227));
#27257=CARTESIAN_POINT('Ctrl Pts',(-1.71250340686822,-1.,-1.34549029589416));
#27258=CARTESIAN_POINT('Ctrl Pts',(-1.70614212266738,-1.,-1.34459924533831));
#27259=CARTESIAN_POINT('Ctrl Pts',(-1.69979707754427,-1.,-1.34367237124483));
#27260=CARTESIAN_POINT('Ctrl Pts',(-1.6934684849687,-1.,-1.34270948206319));
#27261=CARTESIAN_POINT('Ctrl Pts',(-1.68715660868764,-1.,-1.341710374848));
#27262=CARTESIAN_POINT('Ctrl Pts',(-1.68086176030362,-1.,-1.34067485185203));
#27263=CARTESIAN_POINT('Ctrl Pts',(-1.67458429426086,-1.,-1.3396027347034));
#27264=CARTESIAN_POINT('Ctrl Pts',(-1.66832460783989,-1.,-1.33849388654388));
#27265=CARTESIAN_POINT('Ctrl Pts',(-1.66208312541983,-1.,-1.33734820885262));
#27266=CARTESIAN_POINT('Ctrl Pts',(-1.65586025952593,-1.,-1.33616559745172));
#27267=CARTESIAN_POINT('Ctrl Pts',(-1.6496563728683,-1.,-1.33494590467993));
#27268=CARTESIAN_POINT('Ctrl Pts',(-1.6434717485603,-1.,-1.33368890676572));
#27269=CARTESIAN_POINT('Ctrl Pts',(-1.63730653475089,-1.,-1.33239425103724));
#27270=CARTESIAN_POINT('Ctrl Pts',(-1.63116079730923,-1.,-1.33106149345645));
#27271=CARTESIAN_POINT('Ctrl Pts',(-1.62503464209797,-1.,-1.3296901950568));
#27272=CARTESIAN_POINT('Ctrl Pts',(-1.61892832270724,-1.,-1.32828000610449));
#27273=CARTESIAN_POINT('Ctrl Pts',(-1.6128423401575,-1.,-1.32683074483356));
#27274=CARTESIAN_POINT('Ctrl Pts',(-1.60677758290954,-1.,-1.32534250785782));
#27275=CARTESIAN_POINT('Ctrl Pts',(-1.60073511858687,-1.,-1.32381550858256));
#27276=CARTESIAN_POINT('Ctrl Pts',(-1.59471591079403,-1.,-1.32224985747682));
#27277=CARTESIAN_POINT('Ctrl Pts',(-1.58872057258245,-1.,-1.32064537110892));
#27278=CARTESIAN_POINT('Ctrl Pts',(-1.58274907898834,-1.,-1.31900135021432));
#27279=CARTESIAN_POINT('Ctrl Pts',(-1.5768005650559,-1.,-1.31731642317187));
#27280=CARTESIAN_POINT('Ctrl Pts',(-1.57087397835723,-1.,-1.31558903860016));
#27281=CARTESIAN_POINT('Ctrl Pts',(-1.56496872402353,-1.,-1.31381795281002));
#27282=CARTESIAN_POINT('Ctrl Pts',(-1.55908521254821,-1.,-1.31200264341696));
#27283=CARTESIAN_POINT('Ctrl Pts',(-1.55322568759481,-1.,-1.31014393684222));
#27284=CARTESIAN_POINT('Ctrl Pts',(-1.54739413957185,-1.,-1.30824393907473));
#27285=CARTESIAN_POINT('Ctrl Pts',(-1.54159462645432,-1.,-1.30630475189556));
#27286=CARTESIAN_POINT('Ctrl Pts',(-1.53582981268977,-1.,-1.30432735639489));
#27287=CARTESIAN_POINT('Ctrl Pts',(-1.53009970283891,-1.,-1.30231064395568));
#27288=CARTESIAN_POINT('Ctrl Pts',(-1.52439957861062,-1.,-1.30024984366328));
#27289=CARTESIAN_POINT('Ctrl Pts',(-1.51872184912724,-1.,-1.29813791800747));
#27290=CARTESIAN_POINT('Ctrl Pts',(-1.51305994241402,-1.,-1.29596850710509));
#27291=CARTESIAN_POINT('Ctrl Pts',(-1.50741159078365,-1.,-1.29373841372842));
#27292=CARTESIAN_POINT('Ctrl Pts',(-1.50178230149776,-1.,-1.29145022885181));
#27293=CARTESIAN_POINT('Ctrl Pts',(-1.49618896881754,-1.,-1.28911506584254));
#27294=CARTESIAN_POINT('Ctrl Pts',(-1.4906522831278,-1.,-1.2867467611644));
#27295=CARTESIAN_POINT('Ctrl Pts',(-1.4851881711891,-1.,-1.28435533880201));
#27296=CARTESIAN_POINT('Ctrl Pts',(-1.47980070347095,-1.,-1.28194158939517));
#27297=CARTESIAN_POINT('Ctrl Pts',(-1.4744717526707,-1.,-1.2794891824849));
#27298=CARTESIAN_POINT('Ctrl Pts',(-1.46916035917133,-1.,-1.27696414831089));
#27299=CARTESIAN_POINT('Ctrl Pts',(-1.46382431332476,-1.,-1.27433119897822));
#27300=CARTESIAN_POINT('Ctrl Pts',(-1.45843906294697,-1.,-1.27156805265289));
#27301=CARTESIAN_POINT('Ctrl Pts',(-1.45301422764247,-1.,-1.2686778680489));
#27302=CARTESIAN_POINT('Ctrl Pts',(-1.44761985001662,-1.,-1.26570925118868));
#27303=CARTESIAN_POINT('Ctrl Pts',(-1.44236470511303,-1.,-1.26273903323859));
#27304=CARTESIAN_POINT('Ctrl Pts',(-1.43734919180848,-1.,-1.25983531012005));
#27305=CARTESIAN_POINT('Ctrl Pts',(-1.43262645609691,-1.,-1.25702687965755));
#27306=CARTESIAN_POINT('Ctrl Pts',(-1.42815938799387,-1.,-1.25426945222639));
#27307=CARTESIAN_POINT('Ctrl Pts',(-1.42378102115575,-1.,-1.2514145557001));
#27308=CARTESIAN_POINT('Ctrl Pts',(-1.41923722596025,-1.,-1.24824430986571));
#27309=CARTESIAN_POINT('Ctrl Pts',(-1.41422913175179,-1.,-1.24450600513056));
#27310=CARTESIAN_POINT('Ctrl Pts',(-1.40845295531283,-1.,-1.23994455029534));
#27311=CARTESIAN_POINT('Ctrl Pts',(-1.40164708206106,-1.,-1.23434087290423));
#27312=CARTESIAN_POINT('Ctrl Pts',(-1.39361389568796,-1.,-1.22752961899387));
#27313=CARTESIAN_POINT('Ctrl Pts',(-1.38420564527715,-1.,-1.21938737280852));
#27314=CARTESIAN_POINT('Ctrl Pts',(-1.37331915607905,-1.,-1.20982812925645));
#27315=CARTESIAN_POINT('Ctrl Pts',(-1.36088705043885,-1.,-1.1987959077932));
#27316=CARTESIAN_POINT('Ctrl Pts',(-1.34687054001093,-1.,-1.18625865667441));
#27317=CARTESIAN_POINT('Ctrl Pts',(-1.33437539347008,-1.,-1.17501305789857));
#27318=CARTESIAN_POINT('Ctrl Pts',(-1.32428080721772,-1.,-1.16589330093588));
#27319=CARTESIAN_POINT('Ctrl Pts',(-1.31722977216397,-1.,-1.15950888730809));
#27320=CARTESIAN_POINT('Ctrl Pts',(-1.31362392696032,-1.,-1.15624053661742));
#27321=CARTESIAN_POINT('',(-1.15624053661742,-1.,-1.31362392696033));
#27322=CARTESIAN_POINT('Origin',(0.,-1.,0.));
#27323=CARTESIAN_POINT('',(-1.34869019493419,-1.,-1.73811241238545));
#27324=CARTESIAN_POINT('Ctrl Pts',(-1.15624053661742,-1.,-1.31362392696033));
#27325=CARTESIAN_POINT('Ctrl Pts',(-1.15950888730433,-1.,-1.3172297721596));
#27326=CARTESIAN_POINT('Ctrl Pts',(-1.16589330092532,-1.,-1.32428080720544));
#27327=CARTESIAN_POINT('Ctrl Pts',(-1.17501305787994,-1.,-1.33437539344842));
#27328=CARTESIAN_POINT('Ctrl Pts',(-1.18625865664915,-1.,-1.34687053998157));
#27329=CARTESIAN_POINT('Ctrl Pts',(-1.1987959077656,-1.,-1.36088705040677));
#27330=CARTESIAN_POINT('Ctrl Pts',(-1.20982812923113,-1.,-1.37331915604962));
#27331=CARTESIAN_POINT('Ctrl Pts',(-1.21938737278853,-1.,-1.38420564525391));
#27332=CARTESIAN_POINT('Ctrl Pts',(-1.22752961898063,-1.,-1.39361389567257));
#27333=CARTESIAN_POINT('Ctrl Pts',(-1.23434087289768,-1.,-1.40164708205345));
#27334=CARTESIAN_POINT('Ctrl Pts',(-1.23994455029421,-1.,-1.40845295531151));
#27335=CARTESIAN_POINT('Ctrl Pts',(-1.24450600513278,-1.,-1.41422913175437));
#27336=CARTESIAN_POINT('Ctrl Pts',(-1.24824430986911,-1.,-1.41923722596421));
#27337=CARTESIAN_POINT('Ctrl Pts',(-1.25141455570299,-1.,-1.42378102115911));
#27338=CARTESIAN_POINT('Ctrl Pts',(-1.25426945222783,-1.,-1.42815938799555));
#27339=CARTESIAN_POINT('Ctrl Pts',(-1.25702687965744,-1.,-1.43262645609679));
#27340=CARTESIAN_POINT('Ctrl Pts',(-1.25983531011894,-1.,-1.43734919180719));
#27341=CARTESIAN_POINT('Ctrl Pts',(-1.26273903323723,-1.,-1.44236470511145));
#27342=CARTESIAN_POINT('Ctrl Pts',(-1.26570925118767,-1.,-1.44761985001544));
#27343=CARTESIAN_POINT('Ctrl Pts',(-1.26867786804854,-1.,-1.45301422764205));
#27344=CARTESIAN_POINT('Ctrl Pts',(-1.27156805265312,-1.,-1.45843906294725));
#27345=CARTESIAN_POINT('Ctrl Pts',(-1.27433119897877,-1.,-1.4638243133254));
#27346=CARTESIAN_POINT('Ctrl Pts',(-1.27696414831144,-1.,-1.46916035917197));
#27347=CARTESIAN_POINT('Ctrl Pts',(-1.27948918248524,-1.,-1.4744717526711));
#27348=CARTESIAN_POINT('Ctrl Pts',(-1.28194158939522,-1.,-1.47980070347102));
#27349=CARTESIAN_POINT('Ctrl Pts',(-1.28435533880184,-1.,-1.48518817118891));
#27350=CARTESIAN_POINT('Ctrl Pts',(-1.28674676116415,-1.,-1.4906522831275));
#27351=CARTESIAN_POINT('Ctrl Pts',(-1.28911506584232,-1.,-1.49618896881729));
#27352=CARTESIAN_POINT('Ctrl Pts',(-1.29145022885171,-1.,-1.50178230149764));
#27353=CARTESIAN_POINT('Ctrl Pts',(-1.29373841372843,-1.,-1.50741159078367));
#27354=CARTESIAN_POINT('Ctrl Pts',(-1.29596850710518,-1.,-1.51305994241412));
#27355=CARTESIAN_POINT('Ctrl Pts',(-1.29813791800757,-1.,-1.51872184912735));
#27356=CARTESIAN_POINT('Ctrl Pts',(-1.30024984366334,-1.,-1.5243995786107));
#27357=CARTESIAN_POINT('Ctrl Pts',(-1.3023106439557,-1.,-1.53009970283893));
#27358=CARTESIAN_POINT('Ctrl Pts',(-1.30432735639487,-1.,-1.53582981268976));
#27359=CARTESIAN_POINT('Ctrl Pts',(-1.30630475189553,-1.,-1.54159462645428));
#27360=CARTESIAN_POINT('Ctrl Pts',(-1.30824393907471,-1.,-1.54739413957183));
#27361=CARTESIAN_POINT('Ctrl Pts',(-1.31014393684221,-1.,-1.55322568759481));
#27362=CARTESIAN_POINT('Ctrl Pts',(-1.31200264341696,-1.,-1.55908521254822));
#27363=CARTESIAN_POINT('Ctrl Pts',(-1.31381795281002,-1.,-1.56496872402352));
#27364=CARTESIAN_POINT('Ctrl Pts',(-1.31558903860015,-1.,-1.57087397835721));
#27365=CARTESIAN_POINT('Ctrl Pts',(-1.31731642317183,-1.,-1.57680056505585));
#27366=CARTESIAN_POINT('Ctrl Pts',(-1.31900135021428,-1.,-1.58274907898829));
#27367=CARTESIAN_POINT('Ctrl Pts',(-1.32064537110891,-1.,-1.58872057258244));
#27368=CARTESIAN_POINT('Ctrl Pts',(-1.32224985747686,-1.,-1.59471591079408));
#27369=CARTESIAN_POINT('Ctrl Pts',(-1.32381550858266,-1.,-1.600735118587));
#27370=CARTESIAN_POINT('Ctrl Pts',(-1.32534250785794,-1.,-1.6067775829097));
#27371=CARTESIAN_POINT('Ctrl Pts',(-1.32683074483365,-1.,-1.61284234015762));
#27372=CARTESIAN_POINT('Ctrl Pts',(-1.32828000610448,-1.,-1.61892832270723));
#27373=CARTESIAN_POINT('Ctrl Pts',(-1.32969019505665,-1.,-1.62503464209777));
#27374=CARTESIAN_POINT('Ctrl Pts',(-1.33106149345618,-1.,-1.63116079730887));
#27375=CARTESIAN_POINT('Ctrl Pts',(-1.33239425103694,-1.,-1.6373065347505));
#27376=CARTESIAN_POINT('Ctrl Pts',(-1.33368890676554,-1.,-1.64347174856007));
#27377=CARTESIAN_POINT('Ctrl Pts',(-1.33494590468003,-1.,-1.64965637286843));
#27378=CARTESIAN_POINT('Ctrl Pts',(-1.33616559745217,-1.,-1.65586025952651));
#27379=CARTESIAN_POINT('Ctrl Pts',(-1.33734820885331,-1.,-1.66208312542073));
#27380=CARTESIAN_POINT('Ctrl Pts',(-1.33849388654458,-1.,-1.66832460784078));
#27381=CARTESIAN_POINT('Ctrl Pts',(-1.33960273470372,-1.,-1.67458429426126));
#27382=CARTESIAN_POINT('Ctrl Pts',(-1.3406748518516,-1.,-1.68086176030308));
#27383=CARTESIAN_POINT('Ctrl Pts',(-1.34171037484673,-1.,-1.68715660868602));
#27384=CARTESIAN_POINT('Ctrl Pts',(-1.34270948206139,-1.,-1.6934684849664));
#27385=CARTESIAN_POINT('Ctrl Pts',(-1.34367237124322,-1.,-1.69979707754221));
#27386=CARTESIAN_POINT('Ctrl Pts',(-1.34459924533783,-1.,-1.70614212266676));
#27387=CARTESIAN_POINT('Ctrl Pts',(-1.34549029589563,-1.,-1.71250340687011));
#27388=CARTESIAN_POINT('Ctrl Pts',(-1.34634568653586,-1.,-1.7188807715095));
#27389=CARTESIAN_POINT('Ctrl Pts',(-1.34716554820013,-1.,-1.72527410681298));
#27390=CARTESIAN_POINT('Ctrl Pts',(-1.3477930915247,-1.,-1.73040149654497));
#27391=CARTESIAN_POINT('Ctrl Pts',(-1.34824783113158,-1.,-1.73425417886255));
#27392=CARTESIAN_POINT('Ctrl Pts',(-1.34854391898145,-1.,-1.73682580585819));
#27393=CARTESIAN_POINT('Ctrl Pts',(-1.34869019493419,-1.,-1.73811241238545));
#27394=CARTESIAN_POINT('',(-1.23627494547115,-1.,-1.81978687191668));
#27395=CARTESIAN_POINT('',(-1.34869019493419,-1.,-1.73811241238545));
#27396=CARTESIAN_POINT('',(-0.892032620296855,-1.,-1.5055822144029));
#27397=CARTESIAN_POINT('Ctrl Pts',(-1.23627494547115,-1.,-1.81978687191668));
#27398=CARTESIAN_POINT('Ctrl Pts',(-1.23509651170384,-1.,-1.81925017193531));
#27399=CARTESIAN_POINT('Ctrl Pts',(-1.23274224526804,-1.,-1.81817389920914));
#27400=CARTESIAN_POINT('Ctrl Pts',(-1.22921864890975,-1.,-1.81655087183054));
#27401=CARTESIAN_POINT('Ctrl Pts',(-1.22453613304507,-1.,-1.81436959209778));
#27402=CARTESIAN_POINT('Ctrl Pts',(-1.2187090610323,-1.,-1.81161420806172));
#27403=CARTESIAN_POINT('Ctrl Pts',(-1.2129081570818,-1.,-1.80882996916931));
#27404=CARTESIAN_POINT('Ctrl Pts',(-1.20713356605519,-1.,-1.80601678480772));
#27405=CARTESIAN_POINT('Ctrl Pts',(-1.2013854893912,-1.,-1.8031745483882));
#27406=CARTESIAN_POINT('Ctrl Pts',(-1.19566418930405,-1.,-1.80030314370121));
#27407=CARTESIAN_POINT('Ctrl Pts',(-1.1899699793456,-1.,-1.79740245923649));
#27408=CARTESIAN_POINT('Ctrl Pts',(-1.18430321697471,-1.,-1.79447240321572));
#27409=CARTESIAN_POINT('Ctrl Pts',(-1.17866429440781,-1.,-1.79151291552646));
#27410=CARTESIAN_POINT('Ctrl Pts',(-1.17305363177265,-1.,-1.78852398877523));
#27411=CARTESIAN_POINT('Ctrl Pts',(-1.16747166312239,-1.,-1.78550566040349));
#27412=CARTESIAN_POINT('Ctrl Pts',(-1.16191881298458,-1.,-1.78245795880949));
#27413=CARTESIAN_POINT('Ctrl Pts',(-1.15639547194689,-1.,-1.77938085564261));
#27414=CARTESIAN_POINT('Ctrl Pts',(-1.15090197841531,-1.,-1.77627422557034));
#27415=CARTESIAN_POINT('Ctrl Pts',(-1.14543858226948,-1.,-1.77313777896234));
#27416=CARTESIAN_POINT('Ctrl Pts',(-1.14000548337,-1.,-1.76997111386806));
#27417=CARTESIAN_POINT('Ctrl Pts',(-1.13460291804635,-1.,-1.76677384551883));
#27418=CARTESIAN_POINT('Ctrl Pts',(-1.12923123555076,-1.,-1.76354571966171));
#27419=CARTESIAN_POINT('Ctrl Pts',(-1.12389096855078,-1.,-1.76028671825084));
#27420=CARTESIAN_POINT('Ctrl Pts',(-1.11858293216752,-1.,-1.75699720772089));
#27421=CARTESIAN_POINT('Ctrl Pts',(-1.11330807582542,-1.,-1.75367772094617));
#27422=CARTESIAN_POINT('Ctrl Pts',(-1.10806728183003,-1.,-1.75032866075914));
#27423=CARTESIAN_POINT('Ctrl Pts',(-1.10286118991144,-1.,-1.74695004214924));
#27424=CARTESIAN_POINT('Ctrl Pts',(-1.09768999241229,-1.,-1.74354119236212));
#27425=CARTESIAN_POINT('Ctrl Pts',(-1.09255329056496,-1.,-1.74010053962252));
#27426=CARTESIAN_POINT('Ctrl Pts',(-1.08745056285429,-1.,-1.73662628326093));
#27427=CARTESIAN_POINT('Ctrl Pts',(-1.08238162784749,-1.,-1.73311705663407));
#27428=CARTESIAN_POINT('Ctrl Pts',(-1.0773470373727,-1.,-1.72957248977424));
#27429=CARTESIAN_POINT('Ctrl Pts',(-1.07234866990252,-1.,-1.72599406198489));
#27430=CARTESIAN_POINT('Ctrl Pts',(-1.06738966975463,-1.,-1.72238500928456));
#27431=CARTESIAN_POINT('Ctrl Pts',(-1.0624732468065,-1.,-1.71874858456908));
#27432=CARTESIAN_POINT('Ctrl Pts',(-1.05760163192481,-1.,-1.71508654427022));
#27433=CARTESIAN_POINT('Ctrl Pts',(-1.05277517202854,-1.,-1.71139783543986));
#27434=CARTESIAN_POINT('Ctrl Pts',(-1.0479908540499,-1.,-1.70767646263641));
#27435=CARTESIAN_POINT('Ctrl Pts',(-1.04324363334546,-1.,-1.70391338707969));
#27436=CARTESIAN_POINT('Ctrl Pts',(-1.03852922490782,-1.,-1.70010052930951));
#27437=CARTESIAN_POINT('Ctrl Pts',(-1.03384646003587,-1.,-1.69623414782769));
#27438=CARTESIAN_POINT('Ctrl Pts',(-1.02919977579155,-1.,-1.69231840863471));
#27439=CARTESIAN_POINT('Ctrl Pts',(-1.02460180535272,-1.,-1.68836910178475));
#27440=CARTESIAN_POINT('Ctrl Pts',(-1.02006795074222,-1.,-1.68440578021739));
#27441=CARTESIAN_POINT('Ctrl Pts',(-1.01561026162787,-1.,-1.6804428989482));
#27442=CARTESIAN_POINT('Ctrl Pts',(-1.01123236493507,-1.,-1.67648246776457));
#27443=CARTESIAN_POINT('Ctrl Pts',(-1.00692206696387,-1.,-1.67250335383248));
#27444=CARTESIAN_POINT('Ctrl Pts',(-1.00265091003682,-1.,-1.66846059277231));
#27445=CARTESIAN_POINT('Ctrl Pts',(-0.998389654952317,-1.,-1.66430758030304));
#27446=CARTESIAN_POINT('Ctrl Pts',(-0.994121836661116,-1.,-1.66001553809916));
#27447=CARTESIAN_POINT('Ctrl Pts',(-0.98985562785445,-1.,-1.65559044289746));
#27448=CARTESIAN_POINT('Ctrl Pts',(-0.985642622921626,-1.,-1.6511001661277));
#27449=CARTESIAN_POINT('Ctrl Pts',(-0.981562530940574,-1.,-1.64665139190834));
#27450=CARTESIAN_POINT('Ctrl Pts',(-0.977689794120297,-1.,-1.64233990826831));
#27451=CARTESIAN_POINT('Ctrl Pts',(-0.974066058287501,-1.,-1.63820952658157));
#27452=CARTESIAN_POINT('Ctrl Pts',(-0.970669715996356,-1.,-1.63420665729609));
#27453=CARTESIAN_POINT('Ctrl Pts',(-0.967387853228041,-1.,-1.63013849959083));
#27454=CARTESIAN_POINT('Ctrl Pts',(-0.964046107037821,-1.,-1.6257193066974));
#27455=CARTESIAN_POINT('Ctrl Pts',(-0.960438326099958,-1.,-1.62061638139929));
#27456=CARTESIAN_POINT('Ctrl Pts',(-0.956354422921573,-1.,-1.61449324337233));
#27457=CARTESIAN_POINT('Ctrl Pts',(-0.951613284361248,-1.,-1.60706069897794));
#27458=CARTESIAN_POINT('Ctrl Pts',(-0.946078063325796,-1.,-1.59810042045408));
#27459=CARTESIAN_POINT('Ctrl Pts',(-0.939646377909319,-1.,-1.58744937489796));
#27460=CARTESIAN_POINT('Ctrl Pts',(-0.932246680128849,-1.,-1.57499388385561));
#27461=CARTESIAN_POINT('Ctrl Pts',(-0.923832188966322,-1.,-1.56065988582509));
#27462=CARTESIAN_POINT('Ctrl Pts',(-0.91437591904658,-1.,-1.54440491152808));
#27463=CARTESIAN_POINT('Ctrl Pts',(-0.905967409640499,-1.,-1.52984849890434));
#27464=CARTESIAN_POINT('Ctrl Pts',(-0.89918504749193,-1.,-1.51805569591479));
#27465=CARTESIAN_POINT('Ctrl Pts',(-0.894452006967538,-1.,-1.50980486807181));
#27466=CARTESIAN_POINT('Ctrl Pts',(-0.892032620296855,-1.,-1.5055822144029));
#27467=CARTESIAN_POINT('',(-0.693717979106305,-1.,-1.60662857109684));
#27468=CARTESIAN_POINT('Origin',(0.,-1.,0.));
#27469=CARTESIAN_POINT('',(-0.745574324794401,-1.,-2.0698113262342));
#27470=CARTESIAN_POINT('Ctrl Pts',(-0.693717979106305,-1.,-1.60662857109684));
#27471=CARTESIAN_POINT('Ctrl Pts',(-0.69571209787897,-1.,-1.61106790957619));
#27472=CARTESIAN_POINT('Ctrl Pts',(-0.699605146398837,-1.,-1.61974673471117));
#27473=CARTESIAN_POINT('Ctrl Pts',(-0.705159151977294,-1.,-1.6321654166204));
#27474=CARTESIAN_POINT('Ctrl Pts',(-0.711993139340447,-1.,-1.64752408828442));
#27475=CARTESIAN_POINT('Ctrl Pts',(-0.71958543378795,-1.,-1.66472880551777));
#27476=CARTESIAN_POINT('Ctrl Pts',(-0.726235967982445,-1.,-1.67996158451922));
#27477=CARTESIAN_POINT('Ctrl Pts',(-0.731963238685357,-1.,-1.69326921972915));
#27478=CARTESIAN_POINT('Ctrl Pts',(-0.736799665716932,-1.,-1.70473309004249));
#27479=CARTESIAN_POINT('Ctrl Pts',(-0.74079516202821,-1.,-1.71447789751001));
#27480=CARTESIAN_POINT('Ctrl Pts',(-0.744021445433093,-1.,-1.72268229916769));
#27481=CARTESIAN_POINT('Ctrl Pts',(-0.746574710097752,-1.,-1.72958533647714));
#27482=CARTESIAN_POINT('Ctrl Pts',(-0.74858246295687,-1.,-1.7355035168033));
#27483=CARTESIAN_POINT('Ctrl Pts',(-0.750193435981249,-1.,-1.74080458267114));
#27484=CARTESIAN_POINT('Ctrl Pts',(-0.751555614164482,-1.,-1.74585086852502));
#27485=CARTESIAN_POINT('Ctrl Pts',(-0.752797683531314,-1.,-1.75095139468794));
#27486=CARTESIAN_POINT('Ctrl Pts',(-0.754009254027829,-1.,-1.75631083600019));
#27487=CARTESIAN_POINT('Ctrl Pts',(-0.755220979974461,-1.,-1.76197817240128));
#27488=CARTESIAN_POINT('Ctrl Pts',(-0.75642189602781,-1.,-1.76789396002998));
#27489=CARTESIAN_POINT('Ctrl Pts',(-0.757578264077029,-1.,-1.77394167108292));
#27490=CARTESIAN_POINT('Ctrl Pts',(-0.758650626677518,-1.,-1.77999411220945));
#27491=CARTESIAN_POINT('Ctrl Pts',(-0.759614401110189,-1.,-1.78596964884604));
#27492=CARTESIAN_POINT('Ctrl Pts',(-0.760469555880749,-1.,-1.7918581561088));
#27493=CARTESIAN_POINT('Ctrl Pts',(-0.761229695230558,-1.,-1.79768986997783));
#27494=CARTESIAN_POINT('Ctrl Pts',(-0.761915336443547,-1.,-1.80351583877342));
#27495=CARTESIAN_POINT('Ctrl Pts',(-0.762546129463938,-1.,-1.80938551463965));
#27496=CARTESIAN_POINT('Ctrl Pts',(-0.763132003836634,-1.,-1.8153211840553));
#27497=CARTESIAN_POINT('Ctrl Pts',(-0.763673465462726,-1.,-1.82131873145266));
#27498=CARTESIAN_POINT('Ctrl Pts',(-0.764165902605995,-1.,-1.82735991200065));
#27499=CARTESIAN_POINT('Ctrl Pts',(-0.764602549687853,-1.,-1.83342077227142));
#27500=CARTESIAN_POINT('Ctrl Pts',(-0.764978057881737,-1.,-1.83948181064835));
#27501=CARTESIAN_POINT('Ctrl Pts',(-0.765291664862029,-1.,-1.84553698875924));
#27502=CARTESIAN_POINT('Ctrl Pts',(-0.765545710619062,-1.,-1.85158945130063));
#27503=CARTESIAN_POINT('Ctrl Pts',(-0.765744212909318,-1.,-1.85764741390394));
#27504=CARTESIAN_POINT('Ctrl Pts',(-0.765891519092547,-1.,-1.86372027063312));
#27505=CARTESIAN_POINT('Ctrl Pts',(-0.765990708546091,-1.,-1.86981398314341));
#27506=CARTESIAN_POINT('Ctrl Pts',(-0.766042837036744,-1.,-1.87592888967883));
#27507=CARTESIAN_POINT('Ctrl Pts',(-0.766047794851865,-1.,-1.88206215302561));
#27508=CARTESIAN_POINT('Ctrl Pts',(-0.766004837062091,-1.,-1.88820926433409));
#27509=CARTESIAN_POINT('Ctrl Pts',(-0.765913193856978,-1.,-1.89436577771388));
#27510=CARTESIAN_POINT('Ctrl Pts',(-0.765772772593386,-1.,-1.90052930393596));
#27511=CARTESIAN_POINT('Ctrl Pts',(-0.765584196937919,-1.,-1.90669961402356));
#27512=CARTESIAN_POINT('Ctrl Pts',(-0.765348465884722,-1.,-1.91287765805169));
#27513=CARTESIAN_POINT('Ctrl Pts',(-0.765066729667088,-1.,-1.91906491634196));
#27514=CARTESIAN_POINT('Ctrl Pts',(-0.764740025488211,-1.,-1.92526263537048));
#27515=CARTESIAN_POINT('Ctrl Pts',(-0.764369010673941,-1.,-1.93147105496382));
#27516=CARTESIAN_POINT('Ctrl Pts',(-0.763954049121458,-1.,-1.93768964875886));
#27517=CARTESIAN_POINT('Ctrl Pts',(-0.763495333538629,-1.,-1.9439174661764));
#27518=CARTESIAN_POINT('Ctrl Pts',(-0.762992990878769,-1.,-1.95015342590024));
#27519=CARTESIAN_POINT('Ctrl Pts',(-0.762447203806179,-1.,-1.95639665309869));
#27520=CARTESIAN_POINT('Ctrl Pts',(-0.761858300014423,-1.,-1.96264672744186));
#27521=CARTESIAN_POINT('Ctrl Pts',(-0.76122669048382,-1.,-1.96890351582499));
#27522=CARTESIAN_POINT('Ctrl Pts',(-0.760552825409757,-1.,-1.97516705321494));
#27523=CARTESIAN_POINT('Ctrl Pts',(-0.75983714745219,-1.,-1.98143741418172));
#27524=CARTESIAN_POINT('Ctrl Pts',(-0.759080037802488,-1.,-1.98771456680874));
#27525=CARTESIAN_POINT('Ctrl Pts',(-0.758281796766761,-1.,-1.99399831098817));
#27526=CARTESIAN_POINT('Ctrl Pts',(-0.757442676862724,-1.,-2.00028834739178));
#27527=CARTESIAN_POINT('Ctrl Pts',(-0.75656290464667,-1.,-2.0065843158773));
#27528=CARTESIAN_POINT('Ctrl Pts',(-0.755642704957865,-1.,-2.01288584328084));
#27529=CARTESIAN_POINT('Ctrl Pts',(-0.754682330722816,-1.,-2.01919259405809));
#27530=CARTESIAN_POINT('Ctrl Pts',(-0.753682061112768,-1.,-2.02550428623313));
#27531=CARTESIAN_POINT('Ctrl Pts',(-0.752642180487211,-1.,-2.03182068456221));
#27532=CARTESIAN_POINT('Ctrl Pts',(-0.751562963361115,-1.,-2.03814160092099));
#27533=CARTESIAN_POINT('Ctrl Pts',(-0.750444657875576,-1.,-2.04446689147979));
#27534=CARTESIAN_POINT('Ctrl Pts',(-0.749287468665046,-1.,-2.05079645592154));
#27535=CARTESIAN_POINT('Ctrl Pts',(-0.748091554183802,-1.,-2.05713023031006));
#27536=CARTESIAN_POINT('Ctrl Pts',(-0.747103932787919,-1.,-2.06220058927826));
#27537=CARTESIAN_POINT('Ctrl Pts',(-0.7463458715442,-1.,-2.06600523016815));
#27538=CARTESIAN_POINT('Ctrl Pts',(-0.745832791378367,-1.,-2.06854248895728));
#27539=CARTESIAN_POINT('Ctrl Pts',(-0.745574324794401,-1.,-2.0698113262342));
#27540=CARTESIAN_POINT('',(-0.61342227326009,-1.,-2.11275013067528));
#27541=CARTESIAN_POINT('',(-0.745574324794401,-1.,-2.0698113262342));
#27542=CARTESIAN_POINT('',(-0.383122945602004,-1.,-1.7075470150345));
#27543=CARTESIAN_POINT('Ctrl Pts',(-0.61342227326009,-1.,-2.11275013067528));
#27544=CARTESIAN_POINT('Ctrl Pts',(-0.6124673655618,-1.,-2.11187554259986));
#27545=CARTESIAN_POINT('Ctrl Pts',(-0.610560911689899,-1.,-2.11012443807238));
#27546=CARTESIAN_POINT('Ctrl Pts',(-0.607711315454876,-1.,-2.1074919961518));
#27547=CARTESIAN_POINT('Ctrl Pts',(-0.60393203073603,-1.,-2.10397049886949));
#27548=CARTESIAN_POINT('Ctrl Pts',(-0.599241616420533,-1.,-2.0995493086477));
#27549=CARTESIAN_POINT('Ctrl Pts',(-0.594585006052162,-1.,-2.0951087622027));
#27550=CARTESIAN_POINT('Ctrl Pts',(-0.589962365403406,-1.,-2.09064881812129));
#27551=CARTESIAN_POINT('Ctrl Pts',(-0.585373918991617,-1.,-2.08616943727951));
#27552=CARTESIAN_POINT('Ctrl Pts',(-0.580819952108063,-1.,-2.08167059018418));
#27553=CARTESIAN_POINT('Ctrl Pts',(-0.576300797416844,-1.,-2.07715226767559));
#27554=CARTESIAN_POINT('Ctrl Pts',(-0.571816823242603,-1.,-2.07261449292824));
#27555=CARTESIAN_POINT('Ctrl Pts',(-0.567368421181087,-1.,-2.06805732997334));
#27556=CARTESIAN_POINT('Ctrl Pts',(-0.562955993082261,-1.,-2.06348090160589));
#27557=CARTESIAN_POINT('Ctrl Pts',(-0.558579940185151,-1.,-2.05888537756462));
#27558=CARTESIAN_POINT('Ctrl Pts',(-0.554240657463906,-1.,-2.05427091604413));
#27559=CARTESIAN_POINT('Ctrl Pts',(-0.549938525150295,-1.,-2.04963761077958));
#27560=CARTESIAN_POINT('Ctrl Pts',(-0.54567390381743,-1.,-2.04498544714588));
#27561=CARTESIAN_POINT('Ctrl Pts',(-0.541447120615659,-1.,-2.04031422690527));
#27562=CARTESIAN_POINT('Ctrl Pts',(-0.537258489833262,-1.,-2.03562362954037));
#27563=CARTESIAN_POINT('Ctrl Pts',(-0.533108355132977,-1.,-2.03091336214426));
#27564=CARTESIAN_POINT('Ctrl Pts',(-0.528997127241914,-1.,-2.0261832908329));
#27565=CARTESIAN_POINT('Ctrl Pts',(-0.524925318333476,-1.,-2.02143356304698));
#27566=CARTESIAN_POINT('Ctrl Pts',(-0.52089359039937,-1.,-2.01666477917286));
#27567=CARTESIAN_POINT('Ctrl Pts',(-0.516902681728687,-1.,-2.01187773939242));
#27568=CARTESIAN_POINT('Ctrl Pts',(-0.512953306961792,-1.,-2.00707309946949));
#27569=CARTESIAN_POINT('Ctrl Pts',(-0.509046069886157,-1.,-2.00225107134734));
#27570=CARTESIAN_POINT('Ctrl Pts',(-0.505181361323026,-1.,-1.99741107463572));
#27571=CARTESIAN_POINT('Ctrl Pts',(-0.501359287727146,-1.,-1.99255149126155));
#27572=CARTESIAN_POINT('Ctrl Pts',(-0.497579909545574,-1.,-1.98767044752932));
#27573=CARTESIAN_POINT('Ctrl Pts',(-0.493843476541495,-1.,-1.98276658761821));
#27574=CARTESIAN_POINT('Ctrl Pts',(-0.490150627860952,-1.,-1.97783973019229));
#27575=CARTESIAN_POINT('Ctrl Pts',(-0.486502692907659,-1.,-1.97289186263272));
#27576=CARTESIAN_POINT('Ctrl Pts',(-0.482901662120691,-1.,-1.96792703422362));
#27577=CARTESIAN_POINT('Ctrl Pts',(-0.479349583074855,-1.,-1.96294933055943));
#27578=CARTESIAN_POINT('Ctrl Pts',(-0.475848034683176,-1.,-1.95796111148177));
#27579=CARTESIAN_POINT('Ctrl Pts',(-0.472397672264072,-1.,-1.95296148278133));
#27580=CARTESIAN_POINT('Ctrl Pts',(-0.468997482913135,-1.,-1.94794381136514));
#27581=CARTESIAN_POINT('Ctrl Pts',(-0.46564546202603,-1.,-1.9428979419619));
#27582=CARTESIAN_POINT('Ctrl Pts',(-0.462340031009056,-1.,-1.93781486640821));
#27583=CARTESIAN_POINT('Ctrl Pts',(-0.459081234547926,-1.,-1.93269066517934));
#27584=CARTESIAN_POINT('Ctrl Pts',(-0.455872005174371,-1.,-1.92753067150476));
#27585=CARTESIAN_POINT('Ctrl Pts',(-0.452719478359432,-1.,-1.92235380648502));
#27586=CARTESIAN_POINT('Ctrl Pts',(-0.449632260106662,-1.,-1.91718342555755));
#27587=CARTESIAN_POINT('Ctrl Pts',(-0.446617343485711,-1.,-1.9120369998112));
#27588=CARTESIAN_POINT('Ctrl Pts',(-0.443677556849151,-1.,-1.90691756144898));
#27589=CARTESIAN_POINT('Ctrl Pts',(-0.440807833704038,-1.,-1.90180124389086));
#27590=CARTESIAN_POINT('Ctrl Pts',(-0.437995003948244,-1.,-1.89663648956466));
#27591=CARTESIAN_POINT('Ctrl Pts',(-0.435225660963383,-1.,-1.89136993975504));
#27592=CARTESIAN_POINT('Ctrl Pts',(-0.432493038548748,-1.,-1.88596913666793));
#27593=CARTESIAN_POINT('Ctrl Pts',(-0.429803062482344,-1.,-1.88044229001832));
#27594=CARTESIAN_POINT('Ctrl Pts',(-0.427183828519102,-1.,-1.87486989291484));
#27595=CARTESIAN_POINT('Ctrl Pts',(-0.424678177291359,-1.,-1.86937803944323));
#27596=CARTESIAN_POINT('Ctrl Pts',(-0.422327307418275,-1.,-1.86408083334028));
#27597=CARTESIAN_POINT('Ctrl Pts',(-0.420157287975619,-1.,-1.85903281096686));
#27598=CARTESIAN_POINT('Ctrl Pts',(-0.418164129143534,-1.,-1.85417632856234));
#27599=CARTESIAN_POINT('Ctrl Pts',(-0.416300022038864,-1.,-1.84929312929882));
#27600=CARTESIAN_POINT('Ctrl Pts',(-0.41448743825434,-1.,-1.8440575707371));
#27601=CARTESIAN_POINT('Ctrl Pts',(-0.412633125322162,-1.,-1.83808953475839));
#27602=CARTESIAN_POINT('Ctrl Pts',(-0.410641256301675,-1.,-1.83100408895216));
#27603=CARTESIAN_POINT('Ctrl Pts',(-0.408428948108533,-1.,-1.8224702267854));
#27604=CARTESIAN_POINT('Ctrl Pts',(-0.405933518411838,-1.,-1.81223801813988));
#27605=CARTESIAN_POINT('Ctrl Pts',(-0.403107976170441,-1.,-1.80012077176221));
#27606=CARTESIAN_POINT('Ctrl Pts',(-0.39991940378308,-1.,-1.78598826347533));
#27607=CARTESIAN_POINT('Ctrl Pts',(-0.39634619612042,-1.,-1.7697556004756));
#27608=CARTESIAN_POINT('Ctrl Pts',(-0.392375812294307,-1.,-1.75137405313962));
#27609=CARTESIAN_POINT('Ctrl Pts',(-0.388877023509191,-1.,-1.7349317097561));
#27610=CARTESIAN_POINT('Ctrl Pts',(-0.38607079032701,-1.,-1.72162022246158));
#27611=CARTESIAN_POINT('Ctrl Pts',(-0.384119047315542,-1.,-1.71231062891958));
#27612=CARTESIAN_POINT('Ctrl Pts',(-0.383122945602004,-1.,-1.7075470150345));
#27613=CARTESIAN_POINT('',(-0.163289472382896,-1.,-1.74236521665491));
#27614=CARTESIAN_POINT('Origin',(0.,-1.,0.));
#27615=CARTESIAN_POINT('',(-0.0694764450219581,-1.,-2.19890268624765));
#27616=CARTESIAN_POINT('Ctrl Pts',(-0.163289472382896,-1.,-1.74236521665491));
#27617=CARTESIAN_POINT('Ctrl Pts',(-0.163814161002002,-1.,-1.7472034950333));
#27618=CARTESIAN_POINT('Ctrl Pts',(-0.164834765707158,-1.,-1.75666056638427));
#27619=CARTESIAN_POINT('Ctrl Pts',(-0.1662793551464,-1.,-1.77018771684844));
#27620=CARTESIAN_POINT('Ctrl Pts',(-0.168032772805197,-1.,-1.7869064998507));
#27621=CARTESIAN_POINT('Ctrl Pts',(-0.169936923904608,-1.,-1.80561530629706));
#27622=CARTESIAN_POINT('Ctrl Pts',(-0.171554770204119,-1.,-1.82215766811545));
#27623=CARTESIAN_POINT('Ctrl Pts',(-0.1728894428919,-1.,-1.83658380527692));
#27624=CARTESIAN_POINT('Ctrl Pts',(-0.173946627587731,-1.,-1.8489811319852));
#27625=CARTESIAN_POINT('Ctrl Pts',(-0.17473525927603,-1.,-1.85948367088837));
#27626=CARTESIAN_POINT('Ctrl Pts',(-0.175268337590758,-1.,-1.86828349694799));
#27627=CARTESIAN_POINT('Ctrl Pts',(-0.175563480746485,-1.,-1.87563767773588));
#27628=CARTESIAN_POINT('Ctrl Pts',(-0.175644148889699,-1.,-1.88188663145367));
#27629=CARTESIAN_POINT('Ctrl Pts',(-0.175538155840648,-1.,-1.88742606273259));
#27630=CARTESIAN_POINT('Ctrl Pts',(-0.175274276190844,-1.,-1.892646301985));
#27631=CARTESIAN_POINT('Ctrl Pts',(-0.174879405091263,-1.,-1.89788101117132));
#27632=CARTESIAN_POINT('Ctrl Pts',(-0.174375518661085,-1.,-1.90335253862834));
#27633=CARTESIAN_POINT('Ctrl Pts',(-0.173776635257817,-1.,-1.90911693975267));
#27634=CARTESIAN_POINT('Ctrl Pts',(-0.173090695383496,-1.,-1.91511429159527));
#27635=CARTESIAN_POINT('Ctrl Pts',(-0.172321621259514,-1.,-1.9212233439798));
#27636=CARTESIAN_POINT('Ctrl Pts',(-0.171471191532988,-1.,-1.92731093582036));
#27637=CARTESIAN_POINT('Ctrl Pts',(-0.170541253116202,-1.,-1.93329183155539));
#27638=CARTESIAN_POINT('Ctrl Pts',(-0.169534904817491,-1.,-1.93915639211581));
#27639=CARTESIAN_POINT('Ctrl Pts',(-0.168455741607556,-1.,-1.94493757756931));
#27640=CARTESIAN_POINT('Ctrl Pts',(-0.167307501784475,-1.,-1.95069027794294));
#27641=CARTESIAN_POINT('Ctrl Pts',(-0.166093592002812,-1.,-1.9564675971873));
#27642=CARTESIAN_POINT('Ctrl Pts',(-0.164816568920269,-1.,-1.96229379940136));
#27643=CARTESIAN_POINT('Ctrl Pts',(-0.163478185457734,-1.,-1.96816512677967));
#27644=CARTESIAN_POINT('Ctrl Pts',(-0.162079693556289,-1.,-1.97406280235188));
#27645=CARTESIAN_POINT('Ctrl Pts',(-0.160622060784611,-1.,-1.97996195437559));
#27646=CARTESIAN_POINT('Ctrl Pts',(-0.159106226437299,-1.,-1.98584238283292));
#27647=CARTESIAN_POINT('Ctrl Pts',(-0.157533331459227,-1.,-1.99169810931908));
#27648=CARTESIAN_POINT('Ctrl Pts',(-0.155904629548783,-1.,-1.99753284771497));
#27649=CARTESIAN_POINT('Ctrl Pts',(-0.154221403049722,-1.,-2.00335565310543));
#27650=CARTESIAN_POINT('Ctrl Pts',(-0.15248488362145,-1.,-2.00917680318424));
#27651=CARTESIAN_POINT('Ctrl Pts',(-0.150696157673078,-1.,-2.01500291940238));
#27652=CARTESIAN_POINT('Ctrl Pts',(-0.148856124775337,-1.,-2.02083464969894));
#27653=CARTESIAN_POINT('Ctrl Pts',(-0.146965557332583,-1.,-2.02666926182017));
#27654=CARTESIAN_POINT('Ctrl Pts',(-0.145025140186057,-1.,-2.03250223739942));
#27655=CARTESIAN_POINT('Ctrl Pts',(-0.143035515058209,-1.,-2.03832911025912));
#27656=CARTESIAN_POINT('Ctrl Pts',(-0.140997332152546,-1.,-2.04414757947916));
#27657=CARTESIAN_POINT('Ctrl Pts',(-0.138911255368966,-1.,-2.04995762001328));
#27658=CARTESIAN_POINT('Ctrl Pts',(-0.136777941218044,-1.,-2.05576044414264));
#27659=CARTESIAN_POINT('Ctrl Pts',(-0.134598026192106,-1.,-2.06155781517842));
#27660=CARTESIAN_POINT('Ctrl Pts',(-0.13237211154771,-1.,-2.06735123910326));
#27661=CARTESIAN_POINT('Ctrl Pts',(-0.130100748328403,-1.,-2.07314114713063));
#27662=CARTESIAN_POINT('Ctrl Pts',(-0.12778444527612,-1.,-2.07892715110987));
#27663=CARTESIAN_POINT('Ctrl Pts',(-0.125423679412061,-1.,-2.08470840653643));
#27664=CARTESIAN_POINT('Ctrl Pts',(-0.123018905621083,-1.,-2.09048392424825));
#27665=CARTESIAN_POINT('Ctrl Pts',(-0.120570567965122,-1.,-2.0962529286773));
#27666=CARTESIAN_POINT('Ctrl Pts',(-0.118079107988355,-1.,-2.102015121329));
#27667=CARTESIAN_POINT('Ctrl Pts',(-0.115544957687926,-1.,-2.10777050261309));
#27668=CARTESIAN_POINT('Ctrl Pts',(-0.112968534419737,-1.,-2.11351924490306));
#27669=CARTESIAN_POINT('Ctrl Pts',(-0.110350236135025,-1.,-2.11926155590865));
#27670=CARTESIAN_POINT('Ctrl Pts',(-0.10769043523109,-1.,-2.12499752307));
#27671=CARTESIAN_POINT('Ctrl Pts',(-0.104989479152739,-1.,-2.13072704887293));
#27672=CARTESIAN_POINT('Ctrl Pts',(-0.1022477005561,-1.,-2.13644992667165));
#27673=CARTESIAN_POINT('Ctrl Pts',(-0.0994654261990915,-1.,-2.14216588396025));
#27674=CARTESIAN_POINT('Ctrl Pts',(-0.0966429852305459,-1.,-2.14787463531795));
#27675=CARTESIAN_POINT('Ctrl Pts',(-0.0937807218867643,-1.,-2.1535759397817));
#27676=CARTESIAN_POINT('Ctrl Pts',(-0.0908789888107265,-1.,-2.15926961544516));
#27677=CARTESIAN_POINT('Ctrl Pts',(-0.0879381291386923,-1.,-2.16495552645014));
#27678=CARTESIAN_POINT('Ctrl Pts',(-0.0849584620835372,-1.,-2.17063357870952));
#27679=CARTESIAN_POINT('Ctrl Pts',(-0.0819402680872765,-1.,-2.176303712113));
#27680=CARTESIAN_POINT('Ctrl Pts',(-0.0788837727685243,-1.,-2.18196589448887));
#27681=CARTESIAN_POINT('Ctrl Pts',(-0.0757891465836148,-1.,-2.1876201139953));
#27682=CARTESIAN_POINT('Ctrl Pts',(-0.0732830357306725,-1.,-2.19213712013662));
#27683=CARTESIAN_POINT('Ctrl Pts',(-0.0713863779526154,-1.,-2.19552129484002));
#27684=CARTESIAN_POINT('Ctrl Pts',(-0.070114353632549,-1.,-2.19777582085423));
#27685=CARTESIAN_POINT('Ctrl Pts',(-0.0694764450219581,-1.,-2.19890268624765));
#27686=CARTESIAN_POINT('',(0.0694764450219584,-1.,-2.19890268624765));
#27687=CARTESIAN_POINT('',(-0.0694764450219581,-1.,-2.19890268624765));
#27688=CARTESIAN_POINT('',(0.163289472382896,-1.,-1.74236521665491));
#27689=CARTESIAN_POINT('Ctrl Pts',(0.0694764450219584,-1.,-2.19890268624765));
#27690=CARTESIAN_POINT('Ctrl Pts',(0.0701143536324926,-1.,-2.19777582085261));
#27691=CARTESIAN_POINT('Ctrl Pts',(0.0713863779524627,-1.,-2.19552129483562));
#27692=CARTESIAN_POINT('Ctrl Pts',(0.0732830357304276,-1.,-2.19213712012956));
#27693=CARTESIAN_POINT('Ctrl Pts',(0.0757891465833411,-1.,-2.1876201139874));
#27694=CARTESIAN_POINT('Ctrl Pts',(0.0788837727683228,-1.,-2.18196589448304));
#27695=CARTESIAN_POINT('Ctrl Pts',(0.0819402680871939,-1.,-2.1763037121106));
#27696=CARTESIAN_POINT('Ctrl Pts',(0.0849584620835643,-1.,-2.17063357871031));
#27697=CARTESIAN_POINT('Ctrl Pts',(0.0879381291387823,-1.,-2.16495552645275));
#27698=CARTESIAN_POINT('Ctrl Pts',(0.0908789888108266,-1.,-2.15926961544808));
#27699=CARTESIAN_POINT('Ctrl Pts',(0.0937807218868345,-1.,-2.15357593978377));
#27700=CARTESIAN_POINT('Ctrl Pts',(0.0966429852305689,-1.,-2.14787463531864));
#27701=CARTESIAN_POINT('Ctrl Pts',(0.0994654261990743,-1.,-2.14216588395974));
#27702=CARTESIAN_POINT('Ctrl Pts',(0.102247700556064,-1.,-2.13644992667052));
#27703=CARTESIAN_POINT('Ctrl Pts',(0.104989479152703,-1.,-2.1307270488718));
#27704=CARTESIAN_POINT('Ctrl Pts',(0.107690435231068,-1.,-2.12499752306927));
#27705=CARTESIAN_POINT('Ctrl Pts',(0.11035023613502,-1.,-2.11926155590849));
#27706=CARTESIAN_POINT('Ctrl Pts',(0.112968534419746,-1.,-2.11351924490335));
#27707=CARTESIAN_POINT('Ctrl Pts',(0.11554495768794,-1.,-2.10777050261359));
#27708=CARTESIAN_POINT('Ctrl Pts',(0.118079107988368,-1.,-2.10201512132945));
#27709=CARTESIAN_POINT('Ctrl Pts',(0.120570567965129,-1.,-2.09625292867756));
#27710=CARTESIAN_POINT('Ctrl Pts',(0.123018905621083,-1.,-2.09048392424826));
#27711=CARTESIAN_POINT('Ctrl Pts',(0.125423679412058,-1.,-2.08470840653628));
#27712=CARTESIAN_POINT('Ctrl Pts',(0.127784445276116,-1.,-2.07892715110967));
#27713=CARTESIAN_POINT('Ctrl Pts',(0.1301007483284,-1.,-2.07314114713047));
#27714=CARTESIAN_POINT('Ctrl Pts',(0.13237211154771,-1.,-2.06735123910319));
#27715=CARTESIAN_POINT('Ctrl Pts',(0.134598026192107,-1.,-2.06155781517844));
#27716=CARTESIAN_POINT('Ctrl Pts',(0.136777941218044,-1.,-2.0557604441427));
#27717=CARTESIAN_POINT('Ctrl Pts',(0.138911255368966,-1.,-2.04995762001333));
#27718=CARTESIAN_POINT('Ctrl Pts',(0.140997332152545,-1.,-2.04414757947919));
#27719=CARTESIAN_POINT('Ctrl Pts',(0.143035515058208,-1.,-2.03832911025913));
#27720=CARTESIAN_POINT('Ctrl Pts',(0.145025140186058,-1.,-2.03250223739941));
#27721=CARTESIAN_POINT('Ctrl Pts',(0.146965557332586,-1.,-2.02666926182017));
#27722=CARTESIAN_POINT('Ctrl Pts',(0.148856124775343,-1.,-2.02083464969897));
#27723=CARTESIAN_POINT('Ctrl Pts',(0.150696157673084,-1.,-2.01500291940243));
#27724=CARTESIAN_POINT('Ctrl Pts',(0.152484883621452,-1.,-2.00917680318426));
#27725=CARTESIAN_POINT('Ctrl Pts',(0.154221403049719,-1.,-2.00335565310539));
#27726=CARTESIAN_POINT('Ctrl Pts',(0.155904629548774,-1.,-1.99753284771487));
#27727=CARTESIAN_POINT('Ctrl Pts',(0.157533331459215,-1.,-1.99169810931893));
#27728=CARTESIAN_POINT('Ctrl Pts',(0.159106226437288,-1.,-1.98584238283279));
#27729=CARTESIAN_POINT('Ctrl Pts',(0.16062206078461,-1.,-1.97996195437557));
#27730=CARTESIAN_POINT('Ctrl Pts',(0.162079693556302,-1.,-1.97406280235204));
#27731=CARTESIAN_POINT('Ctrl Pts',(0.16347818545776,-1.,-1.96816512678));
#27732=CARTESIAN_POINT('Ctrl Pts',(0.1648165689203,-1.,-1.96229379940174));
#27733=CARTESIAN_POINT('Ctrl Pts',(0.166093592002833,-1.,-1.95646759718755));
#27734=CARTESIAN_POINT('Ctrl Pts',(0.167307501784469,-1.,-1.95069027794286));
#27735=CARTESIAN_POINT('Ctrl Pts',(0.168455741607516,-1.,-1.94493757756879));
#27736=CARTESIAN_POINT('Ctrl Pts',(0.169534904817425,-1.,-1.93915639211497));
#27737=CARTESIAN_POINT('Ctrl Pts',(0.170541253116136,-1.,-1.93329183155455));
#27738=CARTESIAN_POINT('Ctrl Pts',(0.17147119153296,-1.,-1.92731093582));
#27739=CARTESIAN_POINT('Ctrl Pts',(0.172321621259557,-1.,-1.92122334398034));
#27740=CARTESIAN_POINT('Ctrl Pts',(0.173090695383619,-1.,-1.91511429159681));
#27741=CARTESIAN_POINT('Ctrl Pts',(0.173776635257984,-1.,-1.90911693975475));
#27742=CARTESIAN_POINT('Ctrl Pts',(0.174375518661222,-1.,-1.90335253863003));
#27743=CARTESIAN_POINT('Ctrl Pts',(0.174879405091277,-1.,-1.89788101117148));
#27744=CARTESIAN_POINT('Ctrl Pts',(0.175274276190664,-1.,-1.89264630198279));
#27745=CARTESIAN_POINT('Ctrl Pts',(0.175538155840286,-1.,-1.88742606272818));
#27746=CARTESIAN_POINT('Ctrl Pts',(0.175644148889271,-1.,-1.88188663144846));
#27747=CARTESIAN_POINT('Ctrl Pts',(0.175563480746205,-1.,-1.87563767773249));
#27748=CARTESIAN_POINT('Ctrl Pts',(0.175268337590901,-1.,-1.86828349694972));
#27749=CARTESIAN_POINT('Ctrl Pts',(0.174735259276856,-1.,-1.85948367089838));
#27750=CARTESIAN_POINT('Ctrl Pts',(0.173946627589401,-1.,-1.84898113200543));
#27751=CARTESIAN_POINT('Ctrl Pts',(0.17288944289442,-1.,-1.83658380530747));
#27752=CARTESIAN_POINT('Ctrl Pts',(0.171554770207306,-1.,-1.82215766815414));
#27753=CARTESIAN_POINT('Ctrl Pts',(0.169936923908078,-1.,-1.80561530633924));
#27754=CARTESIAN_POINT('Ctrl Pts',(0.16803277280837,-1.,-1.78690649988931));
#27755=CARTESIAN_POINT('Ctrl Pts',(0.166279355148738,-1.,-1.77018771687692));
#27756=CARTESIAN_POINT('Ctrl Pts',(0.164834765708484,-1.,-1.75666056640041));
#27757=CARTESIAN_POINT('Ctrl Pts',(0.163814161002474,-1.,-1.74720349503904));
#27758=CARTESIAN_POINT('Ctrl Pts',(0.163289472382896,-1.,-1.74236521665491));
#27759=CARTESIAN_POINT('',(0.383122945602004,-1.,-1.7075470150345));
#27760=CARTESIAN_POINT('Origin',(0.,-1.,0.));
#27761=CARTESIAN_POINT('',(0.61342227326009,-1.,-2.11275013067528));
#27762=CARTESIAN_POINT('Ctrl Pts',(0.383122945602004,-1.,-1.7075470150345));
#27763=CARTESIAN_POINT('Ctrl Pts',(0.384119047314215,-1.,-1.71231062891398));
#27764=CARTESIAN_POINT('Ctrl Pts',(0.386070790323281,-1.,-1.72162022244582));
#27765=CARTESIAN_POINT('Ctrl Pts',(0.388877023502615,-1.,-1.73493170972829));
#27766=CARTESIAN_POINT('Ctrl Pts',(0.392375812285395,-1.,-1.75137405310193));
#27767=CARTESIAN_POINT('Ctrl Pts',(0.396346196110688,-1.,-1.76975560043442));
#27768=CARTESIAN_POINT('Ctrl Pts',(0.399919403774155,-1.,-1.78598826343754));
#27769=CARTESIAN_POINT('Ctrl Pts',(0.403107976163396,-1.,-1.80012077173238));
#27770=CARTESIAN_POINT('Ctrl Pts',(0.405933518407175,-1.,-1.81223801812013));
#27771=CARTESIAN_POINT('Ctrl Pts',(0.408428948106227,-1.,-1.82247022677562));
#27772=CARTESIAN_POINT('Ctrl Pts',(0.410641256301276,-1.,-1.83100408895047));
#27773=CARTESIAN_POINT('Ctrl Pts',(0.412633125322945,-1.,-1.8380895347617));
#27774=CARTESIAN_POINT('Ctrl Pts',(0.414487438255542,-1.,-1.84405757074218));
#27775=CARTESIAN_POINT('Ctrl Pts',(0.416300022039885,-1.,-1.84929312930314));
#27776=CARTESIAN_POINT('Ctrl Pts',(0.418164129144045,-1.,-1.8541763285645));
#27777=CARTESIAN_POINT('Ctrl Pts',(0.420157287975583,-1.,-1.8590328109667));
#27778=CARTESIAN_POINT('Ctrl Pts',(0.422327307417884,-1.,-1.86408083333863));
#27779=CARTESIAN_POINT('Ctrl Pts',(0.424678177290876,-1.,-1.8693780394412));
#27780=CARTESIAN_POINT('Ctrl Pts',(0.427183828518743,-1.,-1.87486989291334));
#27781=CARTESIAN_POINT('Ctrl Pts',(0.429803062482217,-1.,-1.88044229001779));
#27782=CARTESIAN_POINT('Ctrl Pts',(0.432493038548833,-1.,-1.88596913666828));
#27783=CARTESIAN_POINT('Ctrl Pts',(0.43522566096358,-1.,-1.89136993975585));
#27784=CARTESIAN_POINT('Ctrl Pts',(0.437995003948443,-1.,-1.89663648956549));
#27785=CARTESIAN_POINT('Ctrl Pts',(0.44080783370416,-1.,-1.90180124389137));
#27786=CARTESIAN_POINT('Ctrl Pts',(0.44367755684917,-1.,-1.90691756144906));
#27787=CARTESIAN_POINT('Ctrl Pts',(0.446617343485651,-1.,-1.91203699981095));
#27788=CARTESIAN_POINT('Ctrl Pts',(0.449632260106572,-1.,-1.91718342555717));
#27789=CARTESIAN_POINT('Ctrl Pts',(0.452719478359356,-1.,-1.9223538064847));
#27790=CARTESIAN_POINT('Ctrl Pts',(0.455872005174335,-1.,-1.92753067150461));
#27791=CARTESIAN_POINT('Ctrl Pts',(0.459081234547931,-1.,-1.93269066517936));
#27792=CARTESIAN_POINT('Ctrl Pts',(0.462340031009087,-1.,-1.93781486640834));
#27793=CARTESIAN_POINT('Ctrl Pts',(0.465645462026064,-1.,-1.94289794196205));
#27794=CARTESIAN_POINT('Ctrl Pts',(0.468997482913158,-1.,-1.94794381136524));
#27795=CARTESIAN_POINT('Ctrl Pts',(0.472397672264079,-1.,-1.95296148278136));
#27796=CARTESIAN_POINT('Ctrl Pts',(0.475848034683171,-1.,-1.95796111148175));
#27797=CARTESIAN_POINT('Ctrl Pts',(0.479349583074846,-1.,-1.96294933055938));
#27798=CARTESIAN_POINT('Ctrl Pts',(0.482901662120686,-1.,-1.96792703422358));
#27799=CARTESIAN_POINT('Ctrl Pts',(0.486502692907661,-1.,-1.97289186263272));
#27800=CARTESIAN_POINT('Ctrl Pts',(0.490150627860955,-1.,-1.97783973019229));
#27801=CARTESIAN_POINT('Ctrl Pts',(0.493843476541492,-1.,-1.9827665876182));
#27802=CARTESIAN_POINT('Ctrl Pts',(0.497579909545564,-1.,-1.98767044752929));
#27803=CARTESIAN_POINT('Ctrl Pts',(0.501359287727129,-1.,-1.9925514912615));
#27804=CARTESIAN_POINT('Ctrl Pts',(0.505181361323011,-1.,-1.99741107463567));
#27805=CARTESIAN_POINT('Ctrl Pts',(0.509046069886152,-1.,-2.00225107134733));
#27806=CARTESIAN_POINT('Ctrl Pts',(0.512953306961813,-1.,-2.00707309946955));
#27807=CARTESIAN_POINT('Ctrl Pts',(0.516902681728733,-1.,-2.01187773939257));
#27808=CARTESIAN_POINT('Ctrl Pts',(0.520893590399428,-1.,-2.01666477917306));
#27809=CARTESIAN_POINT('Ctrl Pts',(0.524925318333518,-1.,-2.02143356304712));
#27810=CARTESIAN_POINT('Ctrl Pts',(0.52899712724191,-1.,-2.02618329083289));
#27811=CARTESIAN_POINT('Ctrl Pts',(0.533108355132905,-1.,-2.03091336214401));
#27812=CARTESIAN_POINT('Ctrl Pts',(0.537258489833134,-1.,-2.03562362953993));
#27813=CARTESIAN_POINT('Ctrl Pts',(0.54144712061552,-1.,-2.0403142269048));
#27814=CARTESIAN_POINT('Ctrl Pts',(0.545673903817348,-1.,-2.0449854471456));
#27815=CARTESIAN_POINT('Ctrl Pts',(0.549938525150342,-1.,-2.04963761077974));
#27816=CARTESIAN_POINT('Ctrl Pts',(0.554240657464109,-1.,-2.05427091604482));
#27817=CARTESIAN_POINT('Ctrl Pts',(0.558579940185467,-1.,-2.05888537756571));
#27818=CARTESIAN_POINT('Ctrl Pts',(0.562955993082574,-1.,-2.06348090160697));
#27819=CARTESIAN_POINT('Ctrl Pts',(0.567368421181229,-1.,-2.06805732997383));
#27820=CARTESIAN_POINT('Ctrl Pts',(0.571816823242411,-1.,-2.07261449292758));
#27821=CARTESIAN_POINT('Ctrl Pts',(0.576300797416274,-1.,-2.07715226767361));
#27822=CARTESIAN_POINT('Ctrl Pts',(0.580819952107256,-1.,-2.08167059018138));
#27823=CARTESIAN_POINT('Ctrl Pts',(0.585373918990895,-1.,-2.086169437277));
#27824=CARTESIAN_POINT('Ctrl Pts',(0.589962365403189,-1.,-2.09064881812053));
#27825=CARTESIAN_POINT('Ctrl Pts',(0.594585006052823,-1.,-2.09510876220501));
#27826=CARTESIAN_POINT('Ctrl Pts',(0.599241616422144,-1.,-2.09954930865331));
#27827=CARTESIAN_POINT('Ctrl Pts',(0.603932030738212,-1.,-2.10397049887709));
#27828=CARTESIAN_POINT('Ctrl Pts',(0.607711315456826,-1.,-2.10749199615859));
#27829=CARTESIAN_POINT('Ctrl Pts',(0.610560911691113,-1.,-2.11012443807661));
#27830=CARTESIAN_POINT('Ctrl Pts',(0.61246736556225,-1.,-2.11187554260142));
#27831=CARTESIAN_POINT('Ctrl Pts',(0.61342227326009,-1.,-2.11275013067528));
#27832=CARTESIAN_POINT('',(0.745574324794401,-1.,-2.0698113262342));
#27833=CARTESIAN_POINT('',(0.61342227326009,-1.,-2.11275013067528));
#27834=CARTESIAN_POINT('',(0.693717979106306,-1.,-1.60662857109684));
#27835=CARTESIAN_POINT('Ctrl Pts',(0.745574324794401,-1.,-2.0698113262342));
#27836=CARTESIAN_POINT('Ctrl Pts',(0.74583279137781,-1.,-2.06854248895575));
#27837=CARTESIAN_POINT('Ctrl Pts',(0.746345871542695,-1.,-2.06600523016401));
#27838=CARTESIAN_POINT('Ctrl Pts',(0.747103932785504,-1.,-2.06220058927162));
#27839=CARTESIAN_POINT('Ctrl Pts',(0.748091554181101,-1.,-2.05713023030263));
#27840=CARTESIAN_POINT('Ctrl Pts',(0.749287468663053,-1.,-2.05079645591606));
#27841=CARTESIAN_POINT('Ctrl Pts',(0.750444657874758,-1.,-2.04446689147754));
#27842=CARTESIAN_POINT('Ctrl Pts',(0.751562963361383,-1.,-2.03814160092173));
#27843=CARTESIAN_POINT('Ctrl Pts',(0.752642180488104,-1.,-2.03182068456467));
#27844=CARTESIAN_POINT('Ctrl Pts',(0.753682061113765,-1.,-2.02550428623587));
#27845=CARTESIAN_POINT('Ctrl Pts',(0.75468233072352,-1.,-2.01919259406003));
#27846=CARTESIAN_POINT('Ctrl Pts',(0.7556427049581,-1.,-2.01288584328149));
#27847=CARTESIAN_POINT('Ctrl Pts',(0.756562904646496,-1.,-2.00658431587682));
#27848=CARTESIAN_POINT('Ctrl Pts',(0.757442676862341,-1.,-2.00028834739072));
#27849=CARTESIAN_POINT('Ctrl Pts',(0.758281796766377,-1.,-1.9939983109871));
#27850=CARTESIAN_POINT('Ctrl Pts',(0.759080037802242,-1.,-1.98771456680806));
#27851=CARTESIAN_POINT('Ctrl Pts',(0.759837147452135,-1.,-1.98143741418156));
#27852=CARTESIAN_POINT('Ctrl Pts',(0.760552825409855,-1.,-1.97516705321521));
#27853=CARTESIAN_POINT('Ctrl Pts',(0.761226690483986,-1.,-1.96890351582545));
#27854=CARTESIAN_POINT('Ctrl Pts',(0.761858300014575,-1.,-1.96264672744229));
#27855=CARTESIAN_POINT('Ctrl Pts',(0.762447203806263,-1.,-1.95639665309893));
#27856=CARTESIAN_POINT('Ctrl Pts',(0.762992990878774,-1.,-1.95015342590025));
#27857=CARTESIAN_POINT('Ctrl Pts',(0.76349533353858,-1.,-1.94391746617626));
#27858=CARTESIAN_POINT('Ctrl Pts',(0.763954049121393,-1.,-1.93768964875867));
#27859=CARTESIAN_POINT('Ctrl Pts',(0.764369010673889,-1.,-1.93147105496367));
#27860=CARTESIAN_POINT('Ctrl Pts',(0.764740025488189,-1.,-1.92526263537041));
#27861=CARTESIAN_POINT('Ctrl Pts',(0.765066729667095,-1.,-1.91906491634197));
#27862=CARTESIAN_POINT('Ctrl Pts',(0.765348465884739,-1.,-1.91287765805174));
#27863=CARTESIAN_POINT('Ctrl Pts',(0.765584196937936,-1.,-1.90669961402362));
#27864=CARTESIAN_POINT('Ctrl Pts',(0.765772772593395,-1.,-1.90052930393599));
#27865=CARTESIAN_POINT('Ctrl Pts',(0.765913193856979,-1.,-1.89436577771389));
#27866=CARTESIAN_POINT('Ctrl Pts',(0.76600483706209,-1.,-1.88820926433409));
#27867=CARTESIAN_POINT('Ctrl Pts',(0.766047794851868,-1.,-1.88206215302561));
#27868=CARTESIAN_POINT('Ctrl Pts',(0.766042837036759,-1.,-1.87592888967886));
#27869=CARTESIAN_POINT('Ctrl Pts',(0.765990708546111,-1.,-1.86981398314345));
#27870=CARTESIAN_POINT('Ctrl Pts',(0.765891519092557,-1.,-1.86372027063315));
#27871=CARTESIAN_POINT('Ctrl Pts',(0.765744212909305,-1.,-1.85764741390391));
#27872=CARTESIAN_POINT('Ctrl Pts',(0.765545710619023,-1.,-1.85158945130054));
#27873=CARTESIAN_POINT('Ctrl Pts',(0.765291664861971,-1.,-1.84553698875911));
#27874=CARTESIAN_POINT('Ctrl Pts',(0.764978057881687,-1.,-1.83948181064823));
#27875=CARTESIAN_POINT('Ctrl Pts',(0.764602549687845,-1.,-1.8334207722714));
#27876=CARTESIAN_POINT('Ctrl Pts',(0.764165902606055,-1.,-1.8273599120008));
#27877=CARTESIAN_POINT('Ctrl Pts',(0.763673465462854,-1.,-1.82131873145297));
#27878=CARTESIAN_POINT('Ctrl Pts',(0.763132003836783,-1.,-1.81532118405566));
#27879=CARTESIAN_POINT('Ctrl Pts',(0.762546129464036,-1.,-1.80938551463989));
#27880=CARTESIAN_POINT('Ctrl Pts',(0.761915336443515,-1.,-1.80351583877334));
#27881=CARTESIAN_POINT('Ctrl Pts',(0.761229695230359,-1.,-1.79768986997735));
#27882=CARTESIAN_POINT('Ctrl Pts',(0.760469555880425,-1.,-1.79185815610802));
#27883=CARTESIAN_POINT('Ctrl Pts',(0.759614401109868,-1.,-1.78596964884527));
#27884=CARTESIAN_POINT('Ctrl Pts',(0.75865062667738,-1.,-1.77999411220912));
#27885=CARTESIAN_POINT('Ctrl Pts',(0.757578264077238,-1.,-1.77394167108342));
#27886=CARTESIAN_POINT('Ctrl Pts',(0.756421896028403,-1.,-1.76789396003141));
#27887=CARTESIAN_POINT('Ctrl Pts',(0.755220979975262,-1.,-1.7619781724032));
#27888=CARTESIAN_POINT('Ctrl Pts',(0.75400925402848,-1.,-1.75631083600175));
#27889=CARTESIAN_POINT('Ctrl Pts',(0.752797683531377,-1.,-1.75095139468809));
#27890=CARTESIAN_POINT('Ctrl Pts',(0.751555614163629,-1.,-1.74585086852298));
#27891=CARTESIAN_POINT('Ctrl Pts',(0.75019343597954,-1.,-1.74080458266705));
#27892=CARTESIAN_POINT('Ctrl Pts',(0.748582462954854,-1.,-1.73550351679848));
#27893=CARTESIAN_POINT('Ctrl Pts',(0.746574710096436,-1.,-1.72958533647399));
#27894=CARTESIAN_POINT('Ctrl Pts',(0.744021445433764,-1.,-1.7226822991693));
#27895=CARTESIAN_POINT('Ctrl Pts',(0.740795162032087,-1.,-1.71447789751927));
#27896=CARTESIAN_POINT('Ctrl Pts',(0.736799665724771,-1.,-1.70473309006121));
#27897=CARTESIAN_POINT('Ctrl Pts',(0.731963238697195,-1.,-1.69326921975743));
#27898=CARTESIAN_POINT('Ctrl Pts',(0.726235967997433,-1.,-1.67996158455503));
#27899=CARTESIAN_POINT('Ctrl Pts',(0.719585433804282,-1.,-1.6647288055568));
#27900=CARTESIAN_POINT('Ctrl Pts',(0.711993139355394,-1.,-1.64752408832016));
#27901=CARTESIAN_POINT('Ctrl Pts',(0.705159151988319,-1.,-1.63216541664676));
#27902=CARTESIAN_POINT('Ctrl Pts',(0.699605146405088,-1.,-1.61974673472612));
#27903=CARTESIAN_POINT('Ctrl Pts',(0.695712097881194,-1.,-1.61106790958151));
#27904=CARTESIAN_POINT('Ctrl Pts',(0.693717979106306,-1.,-1.60662857109684));
#27905=CARTESIAN_POINT('',(0.892032620296855,-1.,-1.5055822144029));
#27906=CARTESIAN_POINT('Origin',(0.,-1.,0.));
#27907=CARTESIAN_POINT('',(1.23627494547115,-1.,-1.81978687191668));
#27908=CARTESIAN_POINT('Ctrl Pts',(0.892032620296855,-1.,-1.5055822144029));
#27909=CARTESIAN_POINT('Ctrl Pts',(0.894452006964543,-1.,-1.50980486806688));
#27910=CARTESIAN_POINT('Ctrl Pts',(0.89918504748351,-1.,-1.51805569590094));
#27911=CARTESIAN_POINT('Ctrl Pts',(0.905967409625651,-1.,-1.52984849887993));
#27912=CARTESIAN_POINT('Ctrl Pts',(0.914375919026456,-1.,-1.54440491149498));
#27913=CARTESIAN_POINT('Ctrl Pts',(0.923832188944341,-1.,-1.56065988578893));
#27914=CARTESIAN_POINT('Ctrl Pts',(0.932246680108685,-1.,-1.57499388382243));
#27915=CARTESIAN_POINT('Ctrl Pts',(0.939646377893399,-1.,-1.58744937487176));
#27916=CARTESIAN_POINT('Ctrl Pts',(0.946078063315257,-1.,-1.59810042043673));
#27917=CARTESIAN_POINT('Ctrl Pts',(0.951613284356035,-1.,-1.60706069896936));
#27918=CARTESIAN_POINT('Ctrl Pts',(0.95635442292067,-1.,-1.61449324337085));
#27919=CARTESIAN_POINT('Ctrl Pts',(0.960438326101728,-1.,-1.62061638140221));
#27920=CARTESIAN_POINT('Ctrl Pts',(0.964046107040535,-1.,-1.62571930670187));
#27921=CARTESIAN_POINT('Ctrl Pts',(0.967387853230345,-1.,-1.63013849959462));
#27922=CARTESIAN_POINT('Ctrl Pts',(0.970669715997509,-1.,-1.63420665729798));
#27923=CARTESIAN_POINT('Ctrl Pts',(0.974066058287418,-1.,-1.63820952658144));
#27924=CARTESIAN_POINT('Ctrl Pts',(0.977689794119416,-1.,-1.64233990826687));
#27925=CARTESIAN_POINT('Ctrl Pts',(0.981562530939489,-1.,-1.64665139190656));
#27926=CARTESIAN_POINT('Ctrl Pts',(0.98564262292082,-1.,-1.65110016612638));
#27927=CARTESIAN_POINT('Ctrl Pts',(0.989855627854164,-1.,-1.65559044289699));
#27928=CARTESIAN_POINT('Ctrl Pts',(0.994121836661305,-1.,-1.66001553809947));
#27929=CARTESIAN_POINT('Ctrl Pts',(0.998389654952757,-1.,-1.66430758030376));
#27930=CARTESIAN_POINT('Ctrl Pts',(1.00265091003727,-1.,-1.66846059277303));
#27931=CARTESIAN_POINT('Ctrl Pts',(1.00692206696414,-1.,-1.67250335383293));
#27932=CARTESIAN_POINT('Ctrl Pts',(1.01123236493511,-1.,-1.67648246776464));
#27933=CARTESIAN_POINT('Ctrl Pts',(1.01561026162773,-1.,-1.68044289894798));
#27934=CARTESIAN_POINT('Ctrl Pts',(1.02006795074201,-1.,-1.68440578021706));
#27935=CARTESIAN_POINT('Ctrl Pts',(1.02460180535255,-1.,-1.68836910178447));
#27936=CARTESIAN_POINT('Ctrl Pts',(1.02919977579147,-1.,-1.69231840863458));
#27937=CARTESIAN_POINT('Ctrl Pts',(1.03384646003588,-1.,-1.69623414782771));
#27938=CARTESIAN_POINT('Ctrl Pts',(1.03852922490789,-1.,-1.70010052930962));
#27939=CARTESIAN_POINT('Ctrl Pts',(1.04324363334554,-1.,-1.70391338707982));
#27940=CARTESIAN_POINT('Ctrl Pts',(1.04799085404995,-1.,-1.70767646263649));
#27941=CARTESIAN_POINT('Ctrl Pts',(1.05277517202855,-1.,-1.71139783543989));
#27942=CARTESIAN_POINT('Ctrl Pts',(1.05760163192479,-1.,-1.7150865442702));
#27943=CARTESIAN_POINT('Ctrl Pts',(1.06247324680647,-1.,-1.71874858456904));
#27944=CARTESIAN_POINT('Ctrl Pts',(1.06738966975462,-1.,-1.72238500928453));
#27945=CARTESIAN_POINT('Ctrl Pts',(1.07234866990252,-1.,-1.72599406198488));
#27946=CARTESIAN_POINT('Ctrl Pts',(1.0773470373727,-1.,-1.72957248977424));
#27947=CARTESIAN_POINT('Ctrl Pts',(1.08238162784749,-1.,-1.73311705663407));
#27948=CARTESIAN_POINT('Ctrl Pts',(1.08745056285427,-1.,-1.73662628326091));
#27949=CARTESIAN_POINT('Ctrl Pts',(1.09255329056493,-1.,-1.74010053962247));
#27950=CARTESIAN_POINT('Ctrl Pts',(1.09768999241225,-1.,-1.74354119236208));
#27951=CARTESIAN_POINT('Ctrl Pts',(1.10286118991143,-1.,-1.74695004214923));
#27952=CARTESIAN_POINT('Ctrl Pts',(1.10806728183007,-1.,-1.7503286607592));
#27953=CARTESIAN_POINT('Ctrl Pts',(1.11330807582551,-1.,-1.7536777209463));
#27954=CARTESIAN_POINT('Ctrl Pts',(1.11858293216763,-1.,-1.75699720772105));
#27955=CARTESIAN_POINT('Ctrl Pts',(1.12389096855086,-1.,-1.76028671825096));
#27956=CARTESIAN_POINT('Ctrl Pts',(1.12923123555075,-1.,-1.7635457196617));
#27957=CARTESIAN_POINT('Ctrl Pts',(1.1346029180462,-1.,-1.76677384551862));
#27958=CARTESIAN_POINT('Ctrl Pts',(1.14000548336975,-1.,-1.76997111386769));
#27959=CARTESIAN_POINT('Ctrl Pts',(1.1454385822692,-1.,-1.77313777896194));
#27960=CARTESIAN_POINT('Ctrl Pts',(1.15090197841514,-1.,-1.7762742255701));
#27961=CARTESIAN_POINT('Ctrl Pts',(1.15639547194698,-1.,-1.77938085564275));
#27962=CARTESIAN_POINT('Ctrl Pts',(1.16191881298499,-1.,-1.78245795881009));
#27963=CARTESIAN_POINT('Ctrl Pts',(1.16747166312303,-1.,-1.78550566040443));
#27964=CARTESIAN_POINT('Ctrl Pts',(1.17305363177328,-1.,-1.78852398877617));
#27965=CARTESIAN_POINT('Ctrl Pts',(1.17866429440809,-1.,-1.79151291552689));
#27966=CARTESIAN_POINT('Ctrl Pts',(1.18430321697432,-1.,-1.79447240321515));
#27967=CARTESIAN_POINT('Ctrl Pts',(1.18996997934445,-1.,-1.79740245923478));
#27968=CARTESIAN_POINT('Ctrl Pts',(1.19566418930242,-1.,-1.80030314369879));
#27969=CARTESIAN_POINT('Ctrl Pts',(1.20138548938974,-1.,-1.80317454838603));
#27970=CARTESIAN_POINT('Ctrl Pts',(1.20713356605475,-1.,-1.80601678480707));
#27971=CARTESIAN_POINT('Ctrl Pts',(1.21290815708314,-1.,-1.80882996917129));
#27972=CARTESIAN_POINT('Ctrl Pts',(1.21870906103557,-1.,-1.81161420806656));
#27973=CARTESIAN_POINT('Ctrl Pts',(1.2245361330495,-1.,-1.81436959210434));
#27974=CARTESIAN_POINT('Ctrl Pts',(1.2292186489137,-1.,-1.8165508718364));
#27975=CARTESIAN_POINT('Ctrl Pts',(1.2327422452705,-1.,-1.81817389921279));
#27976=CARTESIAN_POINT('Ctrl Pts',(1.23509651170476,-1.,-1.81925017193666));
#27977=CARTESIAN_POINT('Ctrl Pts',(1.23627494547115,-1.,-1.81978687191668));
#27978=CARTESIAN_POINT('',(1.34869019493419,-1.,-1.73811241238545));
#27979=CARTESIAN_POINT('',(1.23627494547115,-1.,-1.81978687191668));
#27980=CARTESIAN_POINT('',(1.15624053661742,-1.,-1.31362392696032));
#27981=CARTESIAN_POINT('Ctrl Pts',(1.34869019493419,-1.,-1.73811241238545));
#27982=CARTESIAN_POINT('Ctrl Pts',(1.34854391898045,-1.,-1.73682580585691));
#27983=CARTESIAN_POINT('Ctrl Pts',(1.34824783112887,-1.,-1.73425417885907));
#27984=CARTESIAN_POINT('Ctrl Pts',(1.34779309152035,-1.,-1.7304014965394));
#27985=CARTESIAN_POINT('Ctrl Pts',(1.34716554819527,-1.,-1.72527410680674));
#27986=CARTESIAN_POINT('Ctrl Pts',(1.34634568653227,-1.,-1.7188807715049));
#27987=CARTESIAN_POINT('Ctrl Pts',(1.34549029589416,-1.,-1.71250340686822));
#27988=CARTESIAN_POINT('Ctrl Pts',(1.34459924533831,-1.,-1.70614212266738));
#27989=CARTESIAN_POINT('Ctrl Pts',(1.34367237124483,-1.,-1.69979707754427));
#27990=CARTESIAN_POINT('Ctrl Pts',(1.34270948206319,-1.,-1.6934684849687));
#27991=CARTESIAN_POINT('Ctrl Pts',(1.341710374848,-1.,-1.68715660868764));
#27992=CARTESIAN_POINT('Ctrl Pts',(1.34067485185203,-1.,-1.68086176030362));
#27993=CARTESIAN_POINT('Ctrl Pts',(1.3396027347034,-1.,-1.67458429426086));
#27994=CARTESIAN_POINT('Ctrl Pts',(1.33849388654388,-1.,-1.66832460783989));
#27995=CARTESIAN_POINT('Ctrl Pts',(1.33734820885262,-1.,-1.66208312541983));
#27996=CARTESIAN_POINT('Ctrl Pts',(1.33616559745172,-1.,-1.65586025952593));
#27997=CARTESIAN_POINT('Ctrl Pts',(1.33494590467993,-1.,-1.6496563728683));
#27998=CARTESIAN_POINT('Ctrl Pts',(1.33368890676572,-1.,-1.6434717485603));
#27999=CARTESIAN_POINT('Ctrl Pts',(1.33239425103724,-1.,-1.63730653475089));
#28000=CARTESIAN_POINT('Ctrl Pts',(1.33106149345645,-1.,-1.63116079730923));
#28001=CARTESIAN_POINT('Ctrl Pts',(1.3296901950568,-1.,-1.62503464209797));
#28002=CARTESIAN_POINT('Ctrl Pts',(1.32828000610449,-1.,-1.61892832270724));
#28003=CARTESIAN_POINT('Ctrl Pts',(1.32683074483356,-1.,-1.6128423401575));
#28004=CARTESIAN_POINT('Ctrl Pts',(1.32534250785782,-1.,-1.60677758290954));
#28005=CARTESIAN_POINT('Ctrl Pts',(1.32381550858256,-1.,-1.60073511858687));
#28006=CARTESIAN_POINT('Ctrl Pts',(1.32224985747682,-1.,-1.59471591079403));
#28007=CARTESIAN_POINT('Ctrl Pts',(1.32064537110892,-1.,-1.58872057258245));
#28008=CARTESIAN_POINT('Ctrl Pts',(1.31900135021432,-1.,-1.58274907898834));
#28009=CARTESIAN_POINT('Ctrl Pts',(1.31731642317187,-1.,-1.5768005650559));
#28010=CARTESIAN_POINT('Ctrl Pts',(1.31558903860016,-1.,-1.57087397835723));
#28011=CARTESIAN_POINT('Ctrl Pts',(1.31381795281002,-1.,-1.56496872402353));
#28012=CARTESIAN_POINT('Ctrl Pts',(1.31200264341696,-1.,-1.55908521254821));
#28013=CARTESIAN_POINT('Ctrl Pts',(1.31014393684222,-1.,-1.55322568759481));
#28014=CARTESIAN_POINT('Ctrl Pts',(1.30824393907473,-1.,-1.54739413957185));
#28015=CARTESIAN_POINT('Ctrl Pts',(1.30630475189556,-1.,-1.54159462645432));
#28016=CARTESIAN_POINT('Ctrl Pts',(1.30432735639489,-1.,-1.53582981268977));
#28017=CARTESIAN_POINT('Ctrl Pts',(1.30231064395568,-1.,-1.53009970283891));
#28018=CARTESIAN_POINT('Ctrl Pts',(1.30024984366328,-1.,-1.52439957861062));
#28019=CARTESIAN_POINT('Ctrl Pts',(1.29813791800747,-1.,-1.51872184912724));
#28020=CARTESIAN_POINT('Ctrl Pts',(1.29596850710509,-1.,-1.51305994241402));
#28021=CARTESIAN_POINT('Ctrl Pts',(1.29373841372842,-1.,-1.50741159078365));
#28022=CARTESIAN_POINT('Ctrl Pts',(1.29145022885181,-1.,-1.50178230149776));
#28023=CARTESIAN_POINT('Ctrl Pts',(1.28911506584254,-1.,-1.49618896881754));
#28024=CARTESIAN_POINT('Ctrl Pts',(1.2867467611644,-1.,-1.4906522831278));
#28025=CARTESIAN_POINT('Ctrl Pts',(1.28435533880201,-1.,-1.4851881711891));
#28026=CARTESIAN_POINT('Ctrl Pts',(1.28194158939517,-1.,-1.47980070347096));
#28027=CARTESIAN_POINT('Ctrl Pts',(1.2794891824849,-1.,-1.4744717526707));
#28028=CARTESIAN_POINT('Ctrl Pts',(1.27696414831089,-1.,-1.46916035917133));
#28029=CARTESIAN_POINT('Ctrl Pts',(1.27433119897822,-1.,-1.46382431332476));
#28030=CARTESIAN_POINT('Ctrl Pts',(1.27156805265289,-1.,-1.45843906294697));
#28031=CARTESIAN_POINT('Ctrl Pts',(1.2686778680489,-1.,-1.45301422764247));
#28032=CARTESIAN_POINT('Ctrl Pts',(1.26570925118868,-1.,-1.44761985001662));
#28033=CARTESIAN_POINT('Ctrl Pts',(1.26273903323858,-1.,-1.44236470511303));
#28034=CARTESIAN_POINT('Ctrl Pts',(1.25983531012005,-1.,-1.43734919180848));
#28035=CARTESIAN_POINT('Ctrl Pts',(1.25702687965755,-1.,-1.43262645609691));
#28036=CARTESIAN_POINT('Ctrl Pts',(1.25426945222639,-1.,-1.42815938799387));
#28037=CARTESIAN_POINT('Ctrl Pts',(1.2514145557001,-1.,-1.42378102115575));
#28038=CARTESIAN_POINT('Ctrl Pts',(1.24824430986571,-1.,-1.41923722596025));
#28039=CARTESIAN_POINT('Ctrl Pts',(1.24450600513056,-1.,-1.41422913175179));
#28040=CARTESIAN_POINT('Ctrl Pts',(1.23994455029534,-1.,-1.40845295531283));
#28041=CARTESIAN_POINT('Ctrl Pts',(1.23434087290423,-1.,-1.40164708206106));
#28042=CARTESIAN_POINT('Ctrl Pts',(1.22752961899387,-1.,-1.39361389568796));
#28043=CARTESIAN_POINT('Ctrl Pts',(1.21938737280852,-1.,-1.38420564527715));
#28044=CARTESIAN_POINT('Ctrl Pts',(1.20982812925645,-1.,-1.37331915607905));
#28045=CARTESIAN_POINT('Ctrl Pts',(1.1987959077932,-1.,-1.36088705043885));
#28046=CARTESIAN_POINT('Ctrl Pts',(1.18625865667441,-1.,-1.34687054001093));
#28047=CARTESIAN_POINT('Ctrl Pts',(1.17501305789857,-1.,-1.33437539347008));
#28048=CARTESIAN_POINT('Ctrl Pts',(1.16589330093588,-1.,-1.32428080721772));
#28049=CARTESIAN_POINT('Ctrl Pts',(1.15950888730809,-1.,-1.31722977216397));
#28050=CARTESIAN_POINT('Ctrl Pts',(1.15624053661742,-1.,-1.31362392696032));
#28051=CARTESIAN_POINT('',(1.31362392696032,-1.,-1.15624053661742));
#28052=CARTESIAN_POINT('Origin',(0.,-1.,0.));
#28053=CARTESIAN_POINT('',(1.73811241238545,-1.,-1.34869019493419));
#28054=CARTESIAN_POINT('Ctrl Pts',(1.31362392696032,-1.,-1.15624053661742));
#28055=CARTESIAN_POINT('Ctrl Pts',(1.3172297721596,-1.,-1.15950888730433));
#28056=CARTESIAN_POINT('Ctrl Pts',(1.32428080720544,-1.,-1.16589330092532));
#28057=CARTESIAN_POINT('Ctrl Pts',(1.33437539344842,-1.,-1.17501305787994));
#28058=CARTESIAN_POINT('Ctrl Pts',(1.34687053998157,-1.,-1.18625865664915));
#28059=CARTESIAN_POINT('Ctrl Pts',(1.36088705040677,-1.,-1.1987959077656));
#28060=CARTESIAN_POINT('Ctrl Pts',(1.37331915604962,-1.,-1.20982812923113));
#28061=CARTESIAN_POINT('Ctrl Pts',(1.38420564525391,-1.,-1.21938737278853));
#28062=CARTESIAN_POINT('Ctrl Pts',(1.39361389567257,-1.,-1.22752961898063));
#28063=CARTESIAN_POINT('Ctrl Pts',(1.40164708205345,-1.,-1.23434087289768));
#28064=CARTESIAN_POINT('Ctrl Pts',(1.40845295531151,-1.,-1.23994455029421));
#28065=CARTESIAN_POINT('Ctrl Pts',(1.41422913175437,-1.,-1.24450600513278));
#28066=CARTESIAN_POINT('Ctrl Pts',(1.41923722596421,-1.,-1.24824430986911));
#28067=CARTESIAN_POINT('Ctrl Pts',(1.42378102115911,-1.,-1.25141455570299));
#28068=CARTESIAN_POINT('Ctrl Pts',(1.42815938799555,-1.,-1.25426945222783));
#28069=CARTESIAN_POINT('Ctrl Pts',(1.43262645609679,-1.,-1.25702687965744));
#28070=CARTESIAN_POINT('Ctrl Pts',(1.43734919180719,-1.,-1.25983531011894));
#28071=CARTESIAN_POINT('Ctrl Pts',(1.44236470511145,-1.,-1.26273903323723));
#28072=CARTESIAN_POINT('Ctrl Pts',(1.44761985001544,-1.,-1.26570925118767));
#28073=CARTESIAN_POINT('Ctrl Pts',(1.45301422764205,-1.,-1.26867786804854));
#28074=CARTESIAN_POINT('Ctrl Pts',(1.45843906294725,-1.,-1.27156805265312));
#28075=CARTESIAN_POINT('Ctrl Pts',(1.4638243133254,-1.,-1.27433119897877));
#28076=CARTESIAN_POINT('Ctrl Pts',(1.46916035917197,-1.,-1.27696414831144));
#28077=CARTESIAN_POINT('Ctrl Pts',(1.4744717526711,-1.,-1.27948918248524));
#28078=CARTESIAN_POINT('Ctrl Pts',(1.47980070347102,-1.,-1.28194158939522));
#28079=CARTESIAN_POINT('Ctrl Pts',(1.48518817118891,-1.,-1.28435533880184));
#28080=CARTESIAN_POINT('Ctrl Pts',(1.4906522831275,-1.,-1.28674676116415));
#28081=CARTESIAN_POINT('Ctrl Pts',(1.49618896881729,-1.,-1.28911506584232));
#28082=CARTESIAN_POINT('Ctrl Pts',(1.50178230149764,-1.,-1.29145022885171));
#28083=CARTESIAN_POINT('Ctrl Pts',(1.50741159078367,-1.,-1.29373841372843));
#28084=CARTESIAN_POINT('Ctrl Pts',(1.51305994241412,-1.,-1.29596850710518));
#28085=CARTESIAN_POINT('Ctrl Pts',(1.51872184912735,-1.,-1.29813791800757));
#28086=CARTESIAN_POINT('Ctrl Pts',(1.5243995786107,-1.,-1.30024984366334));
#28087=CARTESIAN_POINT('Ctrl Pts',(1.53009970283893,-1.,-1.3023106439557));
#28088=CARTESIAN_POINT('Ctrl Pts',(1.53582981268976,-1.,-1.30432735639487));
#28089=CARTESIAN_POINT('Ctrl Pts',(1.54159462645428,-1.,-1.30630475189553));
#28090=CARTESIAN_POINT('Ctrl Pts',(1.54739413957183,-1.,-1.30824393907471));
#28091=CARTESIAN_POINT('Ctrl Pts',(1.55322568759481,-1.,-1.31014393684221));
#28092=CARTESIAN_POINT('Ctrl Pts',(1.55908521254822,-1.,-1.31200264341696));
#28093=CARTESIAN_POINT('Ctrl Pts',(1.56496872402352,-1.,-1.31381795281002));
#28094=CARTESIAN_POINT('Ctrl Pts',(1.57087397835721,-1.,-1.31558903860015));
#28095=CARTESIAN_POINT('Ctrl Pts',(1.57680056505585,-1.,-1.31731642317183));
#28096=CARTESIAN_POINT('Ctrl Pts',(1.58274907898829,-1.,-1.31900135021428));
#28097=CARTESIAN_POINT('Ctrl Pts',(1.58872057258244,-1.,-1.32064537110891));
#28098=CARTESIAN_POINT('Ctrl Pts',(1.59471591079408,-1.,-1.32224985747686));
#28099=CARTESIAN_POINT('Ctrl Pts',(1.600735118587,-1.,-1.32381550858266));
#28100=CARTESIAN_POINT('Ctrl Pts',(1.6067775829097,-1.,-1.32534250785794));
#28101=CARTESIAN_POINT('Ctrl Pts',(1.61284234015762,-1.,-1.32683074483365));
#28102=CARTESIAN_POINT('Ctrl Pts',(1.61892832270723,-1.,-1.32828000610448));
#28103=CARTESIAN_POINT('Ctrl Pts',(1.62503464209777,-1.,-1.32969019505665));
#28104=CARTESIAN_POINT('Ctrl Pts',(1.63116079730887,-1.,-1.33106149345618));
#28105=CARTESIAN_POINT('Ctrl Pts',(1.63730653475049,-1.,-1.33239425103694));
#28106=CARTESIAN_POINT('Ctrl Pts',(1.64347174856007,-1.,-1.33368890676554));
#28107=CARTESIAN_POINT('Ctrl Pts',(1.64965637286843,-1.,-1.33494590468003));
#28108=CARTESIAN_POINT('Ctrl Pts',(1.65586025952651,-1.,-1.33616559745217));
#28109=CARTESIAN_POINT('Ctrl Pts',(1.66208312542073,-1.,-1.33734820885331));
#28110=CARTESIAN_POINT('Ctrl Pts',(1.66832460784078,-1.,-1.33849388654458));
#28111=CARTESIAN_POINT('Ctrl Pts',(1.67458429426126,-1.,-1.33960273470372));
#28112=CARTESIAN_POINT('Ctrl Pts',(1.68086176030308,-1.,-1.3406748518516));
#28113=CARTESIAN_POINT('Ctrl Pts',(1.68715660868602,-1.,-1.34171037484673));
#28114=CARTESIAN_POINT('Ctrl Pts',(1.6934684849664,-1.,-1.34270948206139));
#28115=CARTESIAN_POINT('Ctrl Pts',(1.69979707754221,-1.,-1.34367237124322));
#28116=CARTESIAN_POINT('Ctrl Pts',(1.70614212266676,-1.,-1.34459924533783));
#28117=CARTESIAN_POINT('Ctrl Pts',(1.71250340687011,-1.,-1.34549029589563));
#28118=CARTESIAN_POINT('Ctrl Pts',(1.7188807715095,-1.,-1.34634568653586));
#28119=CARTESIAN_POINT('Ctrl Pts',(1.72527410681298,-1.,-1.34716554820013));
#28120=CARTESIAN_POINT('Ctrl Pts',(1.73040149654497,-1.,-1.3477930915247));
#28121=CARTESIAN_POINT('Ctrl Pts',(1.73425417886254,-1.,-1.34824783113158));
#28122=CARTESIAN_POINT('Ctrl Pts',(1.73682580585819,-1.,-1.34854391898145));
#28123=CARTESIAN_POINT('Ctrl Pts',(1.73811241238545,-1.,-1.34869019493419));
#28124=CARTESIAN_POINT('',(1.81978687191668,-1.,-1.23627494547115));
#28125=CARTESIAN_POINT('',(1.73811241238545,-1.,-1.34869019493419));
#28126=CARTESIAN_POINT('',(1.5055822144029,-1.,-0.892032620296855));
#28127=CARTESIAN_POINT('Ctrl Pts',(1.81978687191668,-1.,-1.23627494547115));
#28128=CARTESIAN_POINT('Ctrl Pts',(1.81925017193531,-1.,-1.23509651170384));
#28129=CARTESIAN_POINT('Ctrl Pts',(1.81817389920914,-1.,-1.23274224526804));
#28130=CARTESIAN_POINT('Ctrl Pts',(1.81655087183054,-1.,-1.22921864890975));
#28131=CARTESIAN_POINT('Ctrl Pts',(1.81436959209778,-1.,-1.22453613304507));
#28132=CARTESIAN_POINT('Ctrl Pts',(1.81161420806172,-1.,-1.2187090610323));
#28133=CARTESIAN_POINT('Ctrl Pts',(1.80882996916931,-1.,-1.2129081570818));
#28134=CARTESIAN_POINT('Ctrl Pts',(1.80601678480772,-1.,-1.20713356605519));
#28135=CARTESIAN_POINT('Ctrl Pts',(1.8031745483882,-1.,-1.2013854893912));
#28136=CARTESIAN_POINT('Ctrl Pts',(1.80030314370121,-1.,-1.19566418930405));
#28137=CARTESIAN_POINT('Ctrl Pts',(1.79740245923649,-1.,-1.1899699793456));
#28138=CARTESIAN_POINT('Ctrl Pts',(1.79447240321572,-1.,-1.18430321697471));
#28139=CARTESIAN_POINT('Ctrl Pts',(1.79151291552646,-1.,-1.17866429440781));
#28140=CARTESIAN_POINT('Ctrl Pts',(1.78852398877523,-1.,-1.17305363177265));
#28141=CARTESIAN_POINT('Ctrl Pts',(1.78550566040349,-1.,-1.16747166312239));
#28142=CARTESIAN_POINT('Ctrl Pts',(1.78245795880949,-1.,-1.16191881298458));
#28143=CARTESIAN_POINT('Ctrl Pts',(1.77938085564261,-1.,-1.15639547194689));
#28144=CARTESIAN_POINT('Ctrl Pts',(1.77627422557034,-1.,-1.15090197841531));
#28145=CARTESIAN_POINT('Ctrl Pts',(1.77313777896234,-1.,-1.14543858226948));
#28146=CARTESIAN_POINT('Ctrl Pts',(1.76997111386806,-1.,-1.14000548337));
#28147=CARTESIAN_POINT('Ctrl Pts',(1.76677384551883,-1.,-1.13460291804635));
#28148=CARTESIAN_POINT('Ctrl Pts',(1.76354571966171,-1.,-1.12923123555076));
#28149=CARTESIAN_POINT('Ctrl Pts',(1.76028671825084,-1.,-1.12389096855078));
#28150=CARTESIAN_POINT('Ctrl Pts',(1.75699720772089,-1.,-1.11858293216752));
#28151=CARTESIAN_POINT('Ctrl Pts',(1.75367772094617,-1.,-1.11330807582542));
#28152=CARTESIAN_POINT('Ctrl Pts',(1.75032866075914,-1.,-1.10806728183003));
#28153=CARTESIAN_POINT('Ctrl Pts',(1.74695004214924,-1.,-1.10286118991144));
#28154=CARTESIAN_POINT('Ctrl Pts',(1.74354119236212,-1.,-1.09768999241229));
#28155=CARTESIAN_POINT('Ctrl Pts',(1.74010053962252,-1.,-1.09255329056496));
#28156=CARTESIAN_POINT('Ctrl Pts',(1.73662628326093,-1.,-1.08745056285429));
#28157=CARTESIAN_POINT('Ctrl Pts',(1.73311705663407,-1.,-1.08238162784749));
#28158=CARTESIAN_POINT('Ctrl Pts',(1.72957248977424,-1.,-1.0773470373727));
#28159=CARTESIAN_POINT('Ctrl Pts',(1.72599406198489,-1.,-1.07234866990252));
#28160=CARTESIAN_POINT('Ctrl Pts',(1.72238500928456,-1.,-1.06738966975463));
#28161=CARTESIAN_POINT('Ctrl Pts',(1.71874858456908,-1.,-1.0624732468065));
#28162=CARTESIAN_POINT('Ctrl Pts',(1.71508654427022,-1.,-1.05760163192481));
#28163=CARTESIAN_POINT('Ctrl Pts',(1.71139783543986,-1.,-1.05277517202854));
#28164=CARTESIAN_POINT('Ctrl Pts',(1.70767646263641,-1.,-1.0479908540499));
#28165=CARTESIAN_POINT('Ctrl Pts',(1.70391338707969,-1.,-1.04324363334546));
#28166=CARTESIAN_POINT('Ctrl Pts',(1.70010052930951,-1.,-1.03852922490782));
#28167=CARTESIAN_POINT('Ctrl Pts',(1.69623414782769,-1.,-1.03384646003587));
#28168=CARTESIAN_POINT('Ctrl Pts',(1.69231840863471,-1.,-1.02919977579155));
#28169=CARTESIAN_POINT('Ctrl Pts',(1.68836910178475,-1.,-1.02460180535272));
#28170=CARTESIAN_POINT('Ctrl Pts',(1.68440578021739,-1.,-1.02006795074222));
#28171=CARTESIAN_POINT('Ctrl Pts',(1.6804428989482,-1.,-1.01561026162787));
#28172=CARTESIAN_POINT('Ctrl Pts',(1.67648246776457,-1.,-1.01123236493507));
#28173=CARTESIAN_POINT('Ctrl Pts',(1.67250335383248,-1.,-1.00692206696387));
#28174=CARTESIAN_POINT('Ctrl Pts',(1.66846059277231,-1.,-1.00265091003682));
#28175=CARTESIAN_POINT('Ctrl Pts',(1.66430758030304,-1.,-0.998389654952317));
#28176=CARTESIAN_POINT('Ctrl Pts',(1.66001553809916,-1.,-0.994121836661116));
#28177=CARTESIAN_POINT('Ctrl Pts',(1.65559044289746,-1.,-0.98985562785445));
#28178=CARTESIAN_POINT('Ctrl Pts',(1.6511001661277,-1.,-0.985642622921626));
#28179=CARTESIAN_POINT('Ctrl Pts',(1.64665139190834,-1.,-0.981562530940574));
#28180=CARTESIAN_POINT('Ctrl Pts',(1.64233990826831,-1.,-0.977689794120297));
#28181=CARTESIAN_POINT('Ctrl Pts',(1.63820952658157,-1.,-0.974066058287501));
#28182=CARTESIAN_POINT('Ctrl Pts',(1.63420665729609,-1.,-0.970669715996356));
#28183=CARTESIAN_POINT('Ctrl Pts',(1.63013849959083,-1.,-0.967387853228041));
#28184=CARTESIAN_POINT('Ctrl Pts',(1.6257193066974,-1.,-0.964046107037821));
#28185=CARTESIAN_POINT('Ctrl Pts',(1.62061638139929,-1.,-0.960438326099958));
#28186=CARTESIAN_POINT('Ctrl Pts',(1.61449324337233,-1.,-0.956354422921573));
#28187=CARTESIAN_POINT('Ctrl Pts',(1.60706069897794,-1.,-0.951613284361248));
#28188=CARTESIAN_POINT('Ctrl Pts',(1.59810042045408,-1.,-0.946078063325796));
#28189=CARTESIAN_POINT('Ctrl Pts',(1.58744937489796,-1.,-0.939646377909319));
#28190=CARTESIAN_POINT('Ctrl Pts',(1.57499388385561,-1.,-0.932246680128849));
#28191=CARTESIAN_POINT('Ctrl Pts',(1.56065988582509,-1.,-0.923832188966322));
#28192=CARTESIAN_POINT('Ctrl Pts',(1.54440491152807,-1.,-0.91437591904658));
#28193=CARTESIAN_POINT('Ctrl Pts',(1.52984849890434,-1.,-0.905967409640499));
#28194=CARTESIAN_POINT('Ctrl Pts',(1.51805569591479,-1.,-0.89918504749193));
#28195=CARTESIAN_POINT('Ctrl Pts',(1.50980486807181,-1.,-0.894452006967538));
#28196=CARTESIAN_POINT('Ctrl Pts',(1.5055822144029,-1.,-0.892032620296855));
#28197=CARTESIAN_POINT('',(1.60662857109684,-1.,-0.693717979106306));
#28198=CARTESIAN_POINT('Origin',(0.,-1.,0.));
#28199=CARTESIAN_POINT('',(2.0698113262342,-1.,-0.745574324794401));
#28200=CARTESIAN_POINT('Ctrl Pts',(1.60662857109684,-1.,-0.693717979106306));
#28201=CARTESIAN_POINT('Ctrl Pts',(1.61106790957619,-1.,-0.69571209787897));
#28202=CARTESIAN_POINT('Ctrl Pts',(1.61974673471117,-1.,-0.699605146398837));
#28203=CARTESIAN_POINT('Ctrl Pts',(1.6321654166204,-1.,-0.705159151977294));
#28204=CARTESIAN_POINT('Ctrl Pts',(1.64752408828442,-1.,-0.711993139340448));
#28205=CARTESIAN_POINT('Ctrl Pts',(1.66472880551777,-1.,-0.71958543378795));
#28206=CARTESIAN_POINT('Ctrl Pts',(1.67996158451922,-1.,-0.726235967982445));
#28207=CARTESIAN_POINT('Ctrl Pts',(1.69326921972915,-1.,-0.731963238685357));
#28208=CARTESIAN_POINT('Ctrl Pts',(1.70473309004249,-1.,-0.736799665716932));
#28209=CARTESIAN_POINT('Ctrl Pts',(1.71447789751001,-1.,-0.74079516202821));
#28210=CARTESIAN_POINT('Ctrl Pts',(1.72268229916769,-1.,-0.744021445433094));
#28211=CARTESIAN_POINT('Ctrl Pts',(1.72958533647714,-1.,-0.746574710097752));
#28212=CARTESIAN_POINT('Ctrl Pts',(1.7355035168033,-1.,-0.74858246295687));
#28213=CARTESIAN_POINT('Ctrl Pts',(1.74080458267114,-1.,-0.75019343598125));
#28214=CARTESIAN_POINT('Ctrl Pts',(1.74585086852502,-1.,-0.751555614164483));
#28215=CARTESIAN_POINT('Ctrl Pts',(1.75095139468794,-1.,-0.752797683531314));
#28216=CARTESIAN_POINT('Ctrl Pts',(1.75631083600019,-1.,-0.754009254027829));
#28217=CARTESIAN_POINT('Ctrl Pts',(1.76197817240128,-1.,-0.755220979974462));
#28218=CARTESIAN_POINT('Ctrl Pts',(1.76789396002998,-1.,-0.75642189602781));
#28219=CARTESIAN_POINT('Ctrl Pts',(1.77394167108292,-1.,-0.757578264077029));
#28220=CARTESIAN_POINT('Ctrl Pts',(1.77999411220945,-1.,-0.758650626677519));
#28221=CARTESIAN_POINT('Ctrl Pts',(1.78596964884604,-1.,-0.75961440111019));
#28222=CARTESIAN_POINT('Ctrl Pts',(1.7918581561088,-1.,-0.760469555880749));
#28223=CARTESIAN_POINT('Ctrl Pts',(1.79768986997783,-1.,-0.761229695230558));
#28224=CARTESIAN_POINT('Ctrl Pts',(1.80351583877342,-1.,-0.761915336443547));
#28225=CARTESIAN_POINT('Ctrl Pts',(1.80938551463965,-1.,-0.762546129463938));
#28226=CARTESIAN_POINT('Ctrl Pts',(1.8153211840553,-1.,-0.763132003836634));
#28227=CARTESIAN_POINT('Ctrl Pts',(1.82131873145266,-1.,-0.763673465462727));
#28228=CARTESIAN_POINT('Ctrl Pts',(1.82735991200065,-1.,-0.764165902605995));
#28229=CARTESIAN_POINT('Ctrl Pts',(1.83342077227142,-1.,-0.764602549687853));
#28230=CARTESIAN_POINT('Ctrl Pts',(1.83948181064835,-1.,-0.764978057881738));
#28231=CARTESIAN_POINT('Ctrl Pts',(1.84553698875924,-1.,-0.765291664862029));
#28232=CARTESIAN_POINT('Ctrl Pts',(1.85158945130063,-1.,-0.765545710619063));
#28233=CARTESIAN_POINT('Ctrl Pts',(1.85764741390394,-1.,-0.765744212909319));
#28234=CARTESIAN_POINT('Ctrl Pts',(1.86372027063312,-1.,-0.765891519092547));
#28235=CARTESIAN_POINT('Ctrl Pts',(1.86981398314341,-1.,-0.765990708546091));
#28236=CARTESIAN_POINT('Ctrl Pts',(1.87592888967883,-1.,-0.766042837036744));
#28237=CARTESIAN_POINT('Ctrl Pts',(1.88206215302561,-1.,-0.766047794851865));
#28238=CARTESIAN_POINT('Ctrl Pts',(1.88820926433409,-1.,-0.766004837062091));
#28239=CARTESIAN_POINT('Ctrl Pts',(1.89436577771388,-1.,-0.765913193856978));
#28240=CARTESIAN_POINT('Ctrl Pts',(1.90052930393596,-1.,-0.765772772593386));
#28241=CARTESIAN_POINT('Ctrl Pts',(1.90669961402356,-1.,-0.765584196937919));
#28242=CARTESIAN_POINT('Ctrl Pts',(1.91287765805169,-1.,-0.765348465884722));
#28243=CARTESIAN_POINT('Ctrl Pts',(1.91906491634196,-1.,-0.765066729667089));
#28244=CARTESIAN_POINT('Ctrl Pts',(1.92526263537048,-1.,-0.764740025488212));
#28245=CARTESIAN_POINT('Ctrl Pts',(1.93147105496382,-1.,-0.764369010673941));
#28246=CARTESIAN_POINT('Ctrl Pts',(1.93768964875886,-1.,-0.763954049121459));
#28247=CARTESIAN_POINT('Ctrl Pts',(1.9439174661764,-1.,-0.763495333538629));
#28248=CARTESIAN_POINT('Ctrl Pts',(1.95015342590024,-1.,-0.762992990878769));
#28249=CARTESIAN_POINT('Ctrl Pts',(1.95639665309869,-1.,-0.762447203806179));
#28250=CARTESIAN_POINT('Ctrl Pts',(1.96264672744186,-1.,-0.761858300014424));
#28251=CARTESIAN_POINT('Ctrl Pts',(1.96890351582499,-1.,-0.761226690483821));
#28252=CARTESIAN_POINT('Ctrl Pts',(1.97516705321494,-1.,-0.760552825409757));
#28253=CARTESIAN_POINT('Ctrl Pts',(1.98143741418172,-1.,-0.75983714745219));
#28254=CARTESIAN_POINT('Ctrl Pts',(1.98771456680874,-1.,-0.759080037802488));
#28255=CARTESIAN_POINT('Ctrl Pts',(1.99399831098817,-1.,-0.758281796766761));
#28256=CARTESIAN_POINT('Ctrl Pts',(2.00028834739178,-1.,-0.757442676862724));
#28257=CARTESIAN_POINT('Ctrl Pts',(2.0065843158773,-1.,-0.756562904646671));
#28258=CARTESIAN_POINT('Ctrl Pts',(2.01288584328084,-1.,-0.755642704957865));
#28259=CARTESIAN_POINT('Ctrl Pts',(2.01919259405809,-1.,-0.754682330722816));
#28260=CARTESIAN_POINT('Ctrl Pts',(2.02550428623313,-1.,-0.753682061112768));
#28261=CARTESIAN_POINT('Ctrl Pts',(2.03182068456221,-1.,-0.752642180487211));
#28262=CARTESIAN_POINT('Ctrl Pts',(2.03814160092099,-1.,-0.751562963361115));
#28263=CARTESIAN_POINT('Ctrl Pts',(2.04446689147979,-1.,-0.750444657875576));
#28264=CARTESIAN_POINT('Ctrl Pts',(2.05079645592154,-1.,-0.749287468665046));
#28265=CARTESIAN_POINT('Ctrl Pts',(2.05713023031006,-1.,-0.748091554183803));
#28266=CARTESIAN_POINT('Ctrl Pts',(2.06220058927826,-1.,-0.74710393278792));
#28267=CARTESIAN_POINT('Ctrl Pts',(2.06600523016815,-1.,-0.746345871544201));
#28268=CARTESIAN_POINT('Ctrl Pts',(2.06854248895728,-1.,-0.745832791378367));
#28269=CARTESIAN_POINT('Ctrl Pts',(2.0698113262342,-1.,-0.745574324794401));
#28270=CARTESIAN_POINT('',(2.11275013067528,-1.,-0.61342227326009));
#28271=CARTESIAN_POINT('',(2.0698113262342,-1.,-0.745574324794401));
#28272=CARTESIAN_POINT('',(1.7075470150345,-1.,-0.383122945602004));
#28273=CARTESIAN_POINT('Ctrl Pts',(2.11275013067528,-1.,-0.61342227326009));
#28274=CARTESIAN_POINT('Ctrl Pts',(2.11187554259986,-1.,-0.6124673655618));
#28275=CARTESIAN_POINT('Ctrl Pts',(2.11012443807238,-1.,-0.610560911689899));
#28276=CARTESIAN_POINT('Ctrl Pts',(2.1074919961518,-1.,-0.607711315454876));
#28277=CARTESIAN_POINT('Ctrl Pts',(2.10397049886949,-1.,-0.60393203073603));
#28278=CARTESIAN_POINT('Ctrl Pts',(2.0995493086477,-1.,-0.599241616420534));
#28279=CARTESIAN_POINT('Ctrl Pts',(2.0951087622027,-1.,-0.594585006052162));
#28280=CARTESIAN_POINT('Ctrl Pts',(2.09064881812129,-1.,-0.589962365403406));
#28281=CARTESIAN_POINT('Ctrl Pts',(2.08616943727951,-1.,-0.585373918991617));
#28282=CARTESIAN_POINT('Ctrl Pts',(2.08167059018418,-1.,-0.580819952108064));
#28283=CARTESIAN_POINT('Ctrl Pts',(2.07715226767559,-1.,-0.576300797416845));
#28284=CARTESIAN_POINT('Ctrl Pts',(2.07261449292824,-1.,-0.571816823242603));
#28285=CARTESIAN_POINT('Ctrl Pts',(2.06805732997334,-1.,-0.567368421181087));
#28286=CARTESIAN_POINT('Ctrl Pts',(2.06348090160589,-1.,-0.562955993082262));
#28287=CARTESIAN_POINT('Ctrl Pts',(2.05888537756462,-1.,-0.558579940185152));
#28288=CARTESIAN_POINT('Ctrl Pts',(2.05427091604413,-1.,-0.554240657463906));
#28289=CARTESIAN_POINT('Ctrl Pts',(2.04963761077958,-1.,-0.549938525150295));
#28290=CARTESIAN_POINT('Ctrl Pts',(2.04498544714588,-1.,-0.54567390381743));
#28291=CARTESIAN_POINT('Ctrl Pts',(2.04031422690527,-1.,-0.541447120615659));
#28292=CARTESIAN_POINT('Ctrl Pts',(2.03562362954037,-1.,-0.537258489833262));
#28293=CARTESIAN_POINT('Ctrl Pts',(2.03091336214426,-1.,-0.533108355132977));
#28294=CARTESIAN_POINT('Ctrl Pts',(2.0261832908329,-1.,-0.528997127241914));
#28295=CARTESIAN_POINT('Ctrl Pts',(2.02143356304698,-1.,-0.524925318333476));
#28296=CARTESIAN_POINT('Ctrl Pts',(2.01666477917286,-1.,-0.520893590399371));
#28297=CARTESIAN_POINT('Ctrl Pts',(2.01187773939242,-1.,-0.516902681728687));
#28298=CARTESIAN_POINT('Ctrl Pts',(2.00707309946949,-1.,-0.512953306961793));
#28299=CARTESIAN_POINT('Ctrl Pts',(2.00225107134734,-1.,-0.509046069886157));
#28300=CARTESIAN_POINT('Ctrl Pts',(1.99741107463572,-1.,-0.505181361323026));
#28301=CARTESIAN_POINT('Ctrl Pts',(1.99255149126155,-1.,-0.501359287727146));
#28302=CARTESIAN_POINT('Ctrl Pts',(1.98767044752932,-1.,-0.497579909545574));
#28303=CARTESIAN_POINT('Ctrl Pts',(1.98276658761821,-1.,-0.493843476541495));
#28304=CARTESIAN_POINT('Ctrl Pts',(1.97783973019229,-1.,-0.490150627860953));
#28305=CARTESIAN_POINT('Ctrl Pts',(1.97289186263272,-1.,-0.486502692907659));
#28306=CARTESIAN_POINT('Ctrl Pts',(1.96792703422362,-1.,-0.482901662120691));
#28307=CARTESIAN_POINT('Ctrl Pts',(1.96294933055943,-1.,-0.479349583074855));
#28308=CARTESIAN_POINT('Ctrl Pts',(1.95796111148177,-1.,-0.475848034683176));
#28309=CARTESIAN_POINT('Ctrl Pts',(1.95296148278133,-1.,-0.472397672264072));
#28310=CARTESIAN_POINT('Ctrl Pts',(1.94794381136514,-1.,-0.468997482913135));
#28311=CARTESIAN_POINT('Ctrl Pts',(1.9428979419619,-1.,-0.46564546202603));
#28312=CARTESIAN_POINT('Ctrl Pts',(1.93781486640821,-1.,-0.462340031009057));
#28313=CARTESIAN_POINT('Ctrl Pts',(1.93269066517934,-1.,-0.459081234547926));
#28314=CARTESIAN_POINT('Ctrl Pts',(1.92753067150476,-1.,-0.455872005174371));
#28315=CARTESIAN_POINT('Ctrl Pts',(1.92235380648502,-1.,-0.452719478359433));
#28316=CARTESIAN_POINT('Ctrl Pts',(1.91718342555755,-1.,-0.449632260106662));
#28317=CARTESIAN_POINT('Ctrl Pts',(1.9120369998112,-1.,-0.446617343485711));
#28318=CARTESIAN_POINT('Ctrl Pts',(1.90691756144898,-1.,-0.443677556849151));
#28319=CARTESIAN_POINT('Ctrl Pts',(1.90180124389086,-1.,-0.440807833704038));
#28320=CARTESIAN_POINT('Ctrl Pts',(1.89663648956466,-1.,-0.437995003948244));
#28321=CARTESIAN_POINT('Ctrl Pts',(1.89136993975504,-1.,-0.435225660963383));
#28322=CARTESIAN_POINT('Ctrl Pts',(1.88596913666793,-1.,-0.432493038548748));
#28323=CARTESIAN_POINT('Ctrl Pts',(1.88044229001832,-1.,-0.429803062482345));
#28324=CARTESIAN_POINT('Ctrl Pts',(1.87486989291484,-1.,-0.427183828519102));
#28325=CARTESIAN_POINT('Ctrl Pts',(1.86937803944323,-1.,-0.424678177291359));
#28326=CARTESIAN_POINT('Ctrl Pts',(1.86408083334028,-1.,-0.422327307418275));
#28327=CARTESIAN_POINT('Ctrl Pts',(1.85903281096686,-1.,-0.42015728797562));
#28328=CARTESIAN_POINT('Ctrl Pts',(1.85417632856234,-1.,-0.418164129143534));
#28329=CARTESIAN_POINT('Ctrl Pts',(1.84929312929882,-1.,-0.416300022038864));
#28330=CARTESIAN_POINT('Ctrl Pts',(1.8440575707371,-1.,-0.41448743825434));
#28331=CARTESIAN_POINT('Ctrl Pts',(1.83808953475839,-1.,-0.412633125322162));
#28332=CARTESIAN_POINT('Ctrl Pts',(1.83100408895216,-1.,-0.410641256301675));
#28333=CARTESIAN_POINT('Ctrl Pts',(1.8224702267854,-1.,-0.408428948108534));
#28334=CARTESIAN_POINT('Ctrl Pts',(1.81223801813988,-1.,-0.405933518411838));
#28335=CARTESIAN_POINT('Ctrl Pts',(1.80012077176221,-1.,-0.403107976170441));
#28336=CARTESIAN_POINT('Ctrl Pts',(1.78598826347533,-1.,-0.399919403783081));
#28337=CARTESIAN_POINT('Ctrl Pts',(1.7697556004756,-1.,-0.39634619612042));
#28338=CARTESIAN_POINT('Ctrl Pts',(1.75137405313962,-1.,-0.392375812294307));
#28339=CARTESIAN_POINT('Ctrl Pts',(1.7349317097561,-1.,-0.388877023509192));
#28340=CARTESIAN_POINT('Ctrl Pts',(1.72162022246158,-1.,-0.38607079032701));
#28341=CARTESIAN_POINT('Ctrl Pts',(1.71231062891958,-1.,-0.384119047315542));
#28342=CARTESIAN_POINT('Ctrl Pts',(1.7075470150345,-1.,-0.383122945602004));
#28343=CARTESIAN_POINT('',(1.74236521665491,-1.,-0.163289472382896));
#28344=CARTESIAN_POINT('Origin',(0.,-1.,0.));
#28345=CARTESIAN_POINT('',(2.19890268624765,-1.,-0.0694764450219582));
#28346=CARTESIAN_POINT('Ctrl Pts',(1.74236521665491,-1.,-0.163289472382896));
#28347=CARTESIAN_POINT('Ctrl Pts',(1.7472034950333,-1.,-0.163814161002002));
#28348=CARTESIAN_POINT('Ctrl Pts',(1.75666056638427,-1.,-0.164834765707159));
#28349=CARTESIAN_POINT('Ctrl Pts',(1.77018771684844,-1.,-0.1662793551464));
#28350=CARTESIAN_POINT('Ctrl Pts',(1.7869064998507,-1.,-0.168032772805197));
#28351=CARTESIAN_POINT('Ctrl Pts',(1.80561530629706,-1.,-0.169936923904608));
#28352=CARTESIAN_POINT('Ctrl Pts',(1.82215766811545,-1.,-0.171554770204119));
#28353=CARTESIAN_POINT('Ctrl Pts',(1.83658380527692,-1.,-0.1728894428919));
#28354=CARTESIAN_POINT('Ctrl Pts',(1.8489811319852,-1.,-0.173946627587732));
#28355=CARTESIAN_POINT('Ctrl Pts',(1.85948367088837,-1.,-0.17473525927603));
#28356=CARTESIAN_POINT('Ctrl Pts',(1.86828349694799,-1.,-0.175268337590758));
#28357=CARTESIAN_POINT('Ctrl Pts',(1.87563767773588,-1.,-0.175563480746485));
#28358=CARTESIAN_POINT('Ctrl Pts',(1.88188663145367,-1.,-0.175644148889699));
#28359=CARTESIAN_POINT('Ctrl Pts',(1.88742606273259,-1.,-0.175538155840648));
#28360=CARTESIAN_POINT('Ctrl Pts',(1.892646301985,-1.,-0.175274276190844));
#28361=CARTESIAN_POINT('Ctrl Pts',(1.89788101117132,-1.,-0.174879405091263));
#28362=CARTESIAN_POINT('Ctrl Pts',(1.90335253862834,-1.,-0.174375518661085));
#28363=CARTESIAN_POINT('Ctrl Pts',(1.90911693975267,-1.,-0.173776635257817));
#28364=CARTESIAN_POINT('Ctrl Pts',(1.91511429159527,-1.,-0.173090695383496));
#28365=CARTESIAN_POINT('Ctrl Pts',(1.9212233439798,-1.,-0.172321621259514));
#28366=CARTESIAN_POINT('Ctrl Pts',(1.92731093582036,-1.,-0.171471191532988));
#28367=CARTESIAN_POINT('Ctrl Pts',(1.93329183155539,-1.,-0.170541253116202));
#28368=CARTESIAN_POINT('Ctrl Pts',(1.93915639211581,-1.,-0.169534904817491));
#28369=CARTESIAN_POINT('Ctrl Pts',(1.94493757756931,-1.,-0.168455741607556));
#28370=CARTESIAN_POINT('Ctrl Pts',(1.95069027794294,-1.,-0.167307501784476));
#28371=CARTESIAN_POINT('Ctrl Pts',(1.9564675971873,-1.,-0.166093592002813));
#28372=CARTESIAN_POINT('Ctrl Pts',(1.96229379940136,-1.,-0.164816568920269));
#28373=CARTESIAN_POINT('Ctrl Pts',(1.96816512677967,-1.,-0.163478185457734));
#28374=CARTESIAN_POINT('Ctrl Pts',(1.97406280235188,-1.,-0.162079693556289));
#28375=CARTESIAN_POINT('Ctrl Pts',(1.97996195437559,-1.,-0.160622060784611));
#28376=CARTESIAN_POINT('Ctrl Pts',(1.98584238283292,-1.,-0.159106226437299));
#28377=CARTESIAN_POINT('Ctrl Pts',(1.99169810931908,-1.,-0.157533331459227));
#28378=CARTESIAN_POINT('Ctrl Pts',(1.99753284771497,-1.,-0.155904629548784));
#28379=CARTESIAN_POINT('Ctrl Pts',(2.00335565310543,-1.,-0.154221403049722));
#28380=CARTESIAN_POINT('Ctrl Pts',(2.00917680318424,-1.,-0.15248488362145));
#28381=CARTESIAN_POINT('Ctrl Pts',(2.01500291940238,-1.,-0.150696157673078));
#28382=CARTESIAN_POINT('Ctrl Pts',(2.02083464969894,-1.,-0.148856124775337));
#28383=CARTESIAN_POINT('Ctrl Pts',(2.02666926182017,-1.,-0.146965557332583));
#28384=CARTESIAN_POINT('Ctrl Pts',(2.03250223739942,-1.,-0.145025140186058));
#28385=CARTESIAN_POINT('Ctrl Pts',(2.03832911025912,-1.,-0.143035515058209));
#28386=CARTESIAN_POINT('Ctrl Pts',(2.04414757947916,-1.,-0.140997332152546));
#28387=CARTESIAN_POINT('Ctrl Pts',(2.04995762001328,-1.,-0.138911255368966));
#28388=CARTESIAN_POINT('Ctrl Pts',(2.05576044414264,-1.,-0.136777941218044));
#28389=CARTESIAN_POINT('Ctrl Pts',(2.06155781517842,-1.,-0.134598026192106));
#28390=CARTESIAN_POINT('Ctrl Pts',(2.06735123910326,-1.,-0.132372111547711));
#28391=CARTESIAN_POINT('Ctrl Pts',(2.07314114713063,-1.,-0.130100748328404));
#28392=CARTESIAN_POINT('Ctrl Pts',(2.07892715110987,-1.,-0.12778444527612));
#28393=CARTESIAN_POINT('Ctrl Pts',(2.08470840653643,-1.,-0.125423679412062));
#28394=CARTESIAN_POINT('Ctrl Pts',(2.09048392424825,-1.,-0.123018905621083));
#28395=CARTESIAN_POINT('Ctrl Pts',(2.0962529286773,-1.,-0.120570567965122));
#28396=CARTESIAN_POINT('Ctrl Pts',(2.102015121329,-1.,-0.118079107988356));
#28397=CARTESIAN_POINT('Ctrl Pts',(2.10777050261309,-1.,-0.115544957687927));
#28398=CARTESIAN_POINT('Ctrl Pts',(2.11351924490306,-1.,-0.112968534419737));
#28399=CARTESIAN_POINT('Ctrl Pts',(2.11926155590865,-1.,-0.110350236135025));
#28400=CARTESIAN_POINT('Ctrl Pts',(2.12499752307,-1.,-0.10769043523109));
#28401=CARTESIAN_POINT('Ctrl Pts',(2.13072704887293,-1.,-0.10498947915274));
#28402=CARTESIAN_POINT('Ctrl Pts',(2.13644992667165,-1.,-0.102247700556101));
#28403=CARTESIAN_POINT('Ctrl Pts',(2.14216588396025,-1.,-0.0994654261990917));
#28404=CARTESIAN_POINT('Ctrl Pts',(2.14787463531795,-1.,-0.096642985230546));
#28405=CARTESIAN_POINT('Ctrl Pts',(2.1535759397817,-1.,-0.0937807218867645));
#28406=CARTESIAN_POINT('Ctrl Pts',(2.15926961544516,-1.,-0.0908789888107267));
#28407=CARTESIAN_POINT('Ctrl Pts',(2.16495552645014,-1.,-0.0879381291386924));
#28408=CARTESIAN_POINT('Ctrl Pts',(2.17063357870952,-1.,-0.0849584620835374));
#28409=CARTESIAN_POINT('Ctrl Pts',(2.176303712113,-1.,-0.0819402680872767));
#28410=CARTESIAN_POINT('Ctrl Pts',(2.18196589448887,-1.,-0.0788837727685244));
#28411=CARTESIAN_POINT('Ctrl Pts',(2.1876201139953,-1.,-0.0757891465836149));
#28412=CARTESIAN_POINT('Ctrl Pts',(2.19213712013662,-1.,-0.0732830357306726));
#28413=CARTESIAN_POINT('Ctrl Pts',(2.19552129484002,-1.,-0.0713863779526155));
#28414=CARTESIAN_POINT('Ctrl Pts',(2.19777582085423,-1.,-0.0701143536325491));
#28415=CARTESIAN_POINT('Ctrl Pts',(2.19890268624765,-1.,-0.0694764450219582));
#28416=CARTESIAN_POINT('',(2.19890268624765,-1.,0.0694764450219582));
#28417=CARTESIAN_POINT('',(2.19890268624765,-1.,-0.0694764450219582));
#28418=CARTESIAN_POINT('',(1.74236521665491,-1.,0.163289472382896));
#28419=CARTESIAN_POINT('Ctrl Pts',(2.19890268624765,-1.,0.0694764450219582));
#28420=CARTESIAN_POINT('Ctrl Pts',(2.19777582085261,-1.,0.0701143536324925));
#28421=CARTESIAN_POINT('Ctrl Pts',(2.19552129483562,-1.,0.0713863779524626));
#28422=CARTESIAN_POINT('Ctrl Pts',(2.19213712012956,-1.,0.0732830357304275));
#28423=CARTESIAN_POINT('Ctrl Pts',(2.1876201139874,-1.,0.075789146583341));
#28424=CARTESIAN_POINT('Ctrl Pts',(2.18196589448304,-1.,0.0788837727683226));
#28425=CARTESIAN_POINT('Ctrl Pts',(2.1763037121106,-1.,0.0819402680871938));
#28426=CARTESIAN_POINT('Ctrl Pts',(2.17063357871031,-1.,0.0849584620835642));
#28427=CARTESIAN_POINT('Ctrl Pts',(2.16495552645275,-1.,0.0879381291387821));
#28428=CARTESIAN_POINT('Ctrl Pts',(2.15926961544808,-1.,0.0908789888108265));
#28429=CARTESIAN_POINT('Ctrl Pts',(2.15357593978377,-1.,0.0937807218868344));
#28430=CARTESIAN_POINT('Ctrl Pts',(2.14787463531864,-1.,0.0966429852305688));
#28431=CARTESIAN_POINT('Ctrl Pts',(2.14216588395974,-1.,0.0994654261990741));
#28432=CARTESIAN_POINT('Ctrl Pts',(2.13644992667052,-1.,0.102247700556063));
#28433=CARTESIAN_POINT('Ctrl Pts',(2.1307270488718,-1.,0.104989479152703));
#28434=CARTESIAN_POINT('Ctrl Pts',(2.12499752306927,-1.,0.107690435231068));
#28435=CARTESIAN_POINT('Ctrl Pts',(2.11926155590849,-1.,0.11035023613502));
#28436=CARTESIAN_POINT('Ctrl Pts',(2.11351924490335,-1.,0.112968534419746));
#28437=CARTESIAN_POINT('Ctrl Pts',(2.10777050261359,-1.,0.11554495768794));
#28438=CARTESIAN_POINT('Ctrl Pts',(2.10201512132945,-1.,0.118079107988368));
#28439=CARTESIAN_POINT('Ctrl Pts',(2.09625292867756,-1.,0.120570567965129));
#28440=CARTESIAN_POINT('Ctrl Pts',(2.09048392424826,-1.,0.123018905621083));
#28441=CARTESIAN_POINT('Ctrl Pts',(2.08470840653628,-1.,0.125423679412058));
#28442=CARTESIAN_POINT('Ctrl Pts',(2.07892715110967,-1.,0.127784445276116));
#28443=CARTESIAN_POINT('Ctrl Pts',(2.07314114713047,-1.,0.1301007483284));
#28444=CARTESIAN_POINT('Ctrl Pts',(2.06735123910319,-1.,0.132372111547709));
#28445=CARTESIAN_POINT('Ctrl Pts',(2.06155781517844,-1.,0.134598026192107));
#28446=CARTESIAN_POINT('Ctrl Pts',(2.0557604441427,-1.,0.136777941218044));
#28447=CARTESIAN_POINT('Ctrl Pts',(2.04995762001333,-1.,0.138911255368966));
#28448=CARTESIAN_POINT('Ctrl Pts',(2.04414757947919,-1.,0.140997332152545));
#28449=CARTESIAN_POINT('Ctrl Pts',(2.03832911025913,-1.,0.143035515058208));
#28450=CARTESIAN_POINT('Ctrl Pts',(2.03250223739941,-1.,0.145025140186058));
#28451=CARTESIAN_POINT('Ctrl Pts',(2.02666926182017,-1.,0.146965557332586));
#28452=CARTESIAN_POINT('Ctrl Pts',(2.02083464969897,-1.,0.148856124775342));
#28453=CARTESIAN_POINT('Ctrl Pts',(2.01500291940243,-1.,0.150696157673084));
#28454=CARTESIAN_POINT('Ctrl Pts',(2.00917680318426,-1.,0.152484883621452));
#28455=CARTESIAN_POINT('Ctrl Pts',(2.00335565310539,-1.,0.154221403049719));
#28456=CARTESIAN_POINT('Ctrl Pts',(1.99753284771487,-1.,0.155904629548774));
#28457=CARTESIAN_POINT('Ctrl Pts',(1.99169810931893,-1.,0.157533331459215));
#28458=CARTESIAN_POINT('Ctrl Pts',(1.98584238283279,-1.,0.159106226437288));
#28459=CARTESIAN_POINT('Ctrl Pts',(1.97996195437557,-1.,0.16062206078461));
#28460=CARTESIAN_POINT('Ctrl Pts',(1.97406280235204,-1.,0.162079693556302));
#28461=CARTESIAN_POINT('Ctrl Pts',(1.96816512678,-1.,0.16347818545776));
#28462=CARTESIAN_POINT('Ctrl Pts',(1.96229379940174,-1.,0.1648165689203));
#28463=CARTESIAN_POINT('Ctrl Pts',(1.95646759718755,-1.,0.166093592002832));
#28464=CARTESIAN_POINT('Ctrl Pts',(1.95069027794286,-1.,0.167307501784469));
#28465=CARTESIAN_POINT('Ctrl Pts',(1.94493757756879,-1.,0.168455741607515));
#28466=CARTESIAN_POINT('Ctrl Pts',(1.93915639211497,-1.,0.169534904817425));
#28467=CARTESIAN_POINT('Ctrl Pts',(1.93329183155455,-1.,0.170541253116136));
#28468=CARTESIAN_POINT('Ctrl Pts',(1.92731093582,-1.,0.17147119153296));
#28469=CARTESIAN_POINT('Ctrl Pts',(1.92122334398034,-1.,0.172321621259556));
#28470=CARTESIAN_POINT('Ctrl Pts',(1.91511429159681,-1.,0.173090695383619));
#28471=CARTESIAN_POINT('Ctrl Pts',(1.90911693975475,-1.,0.173776635257983));
#28472=CARTESIAN_POINT('Ctrl Pts',(1.90335253863003,-1.,0.174375518661222));
#28473=CARTESIAN_POINT('Ctrl Pts',(1.89788101117148,-1.,0.174879405091277));
#28474=CARTESIAN_POINT('Ctrl Pts',(1.89264630198279,-1.,0.175274276190664));
#28475=CARTESIAN_POINT('Ctrl Pts',(1.88742606272818,-1.,0.175538155840286));
#28476=CARTESIAN_POINT('Ctrl Pts',(1.88188663144846,-1.,0.175644148889271));
#28477=CARTESIAN_POINT('Ctrl Pts',(1.87563767773249,-1.,0.175563480746205));
#28478=CARTESIAN_POINT('Ctrl Pts',(1.86828349694972,-1.,0.1752683375909));
#28479=CARTESIAN_POINT('Ctrl Pts',(1.85948367089838,-1.,0.174735259276856));
#28480=CARTESIAN_POINT('Ctrl Pts',(1.84898113200543,-1.,0.173946627589401));
#28481=CARTESIAN_POINT('Ctrl Pts',(1.83658380530747,-1.,0.17288944289442));
#28482=CARTESIAN_POINT('Ctrl Pts',(1.82215766815414,-1.,0.171554770207306));
#28483=CARTESIAN_POINT('Ctrl Pts',(1.80561530633924,-1.,0.169936923908078));
#28484=CARTESIAN_POINT('Ctrl Pts',(1.78690649988931,-1.,0.16803277280837));
#28485=CARTESIAN_POINT('Ctrl Pts',(1.77018771687692,-1.,0.166279355148738));
#28486=CARTESIAN_POINT('Ctrl Pts',(1.75666056640041,-1.,0.164834765708484));
#28487=CARTESIAN_POINT('Ctrl Pts',(1.74720349503904,-1.,0.163814161002474));
#28488=CARTESIAN_POINT('Ctrl Pts',(1.74236521665491,-1.,0.163289472382896));
#28489=CARTESIAN_POINT('',(1.7075470150345,-1.,0.383122945602004));
#28490=CARTESIAN_POINT('Origin',(0.,-1.,0.));
#28491=CARTESIAN_POINT('',(2.11275013067528,-1.,0.613422273260091));
#28492=CARTESIAN_POINT('Ctrl Pts',(1.7075470150345,-1.,0.383122945602004));
#28493=CARTESIAN_POINT('Ctrl Pts',(1.71231062891398,-1.,0.384119047314215));
#28494=CARTESIAN_POINT('Ctrl Pts',(1.72162022244582,-1.,0.386070790323281));
#28495=CARTESIAN_POINT('Ctrl Pts',(1.73493170972829,-1.,0.388877023502615));
#28496=CARTESIAN_POINT('Ctrl Pts',(1.75137405310193,-1.,0.392375812285396));
#28497=CARTESIAN_POINT('Ctrl Pts',(1.76975560043442,-1.,0.396346196110688));
#28498=CARTESIAN_POINT('Ctrl Pts',(1.78598826343754,-1.,0.399919403774156));
#28499=CARTESIAN_POINT('Ctrl Pts',(1.80012077173238,-1.,0.403107976163396));
#28500=CARTESIAN_POINT('Ctrl Pts',(1.81223801812013,-1.,0.405933518407176));
#28501=CARTESIAN_POINT('Ctrl Pts',(1.82247022677562,-1.,0.408428948106228));
#28502=CARTESIAN_POINT('Ctrl Pts',(1.83100408895047,-1.,0.410641256301276));
#28503=CARTESIAN_POINT('Ctrl Pts',(1.8380895347617,-1.,0.412633125322945));
#28504=CARTESIAN_POINT('Ctrl Pts',(1.84405757074218,-1.,0.414487438255542));
#28505=CARTESIAN_POINT('Ctrl Pts',(1.84929312930314,-1.,0.416300022039885));
#28506=CARTESIAN_POINT('Ctrl Pts',(1.8541763285645,-1.,0.418164129144046));
#28507=CARTESIAN_POINT('Ctrl Pts',(1.8590328109667,-1.,0.420157287975583));
#28508=CARTESIAN_POINT('Ctrl Pts',(1.86408083333863,-1.,0.422327307417885));
#28509=CARTESIAN_POINT('Ctrl Pts',(1.8693780394412,-1.,0.424678177290876));
#28510=CARTESIAN_POINT('Ctrl Pts',(1.87486989291333,-1.,0.427183828518743));
#28511=CARTESIAN_POINT('Ctrl Pts',(1.88044229001778,-1.,0.429803062482217));
#28512=CARTESIAN_POINT('Ctrl Pts',(1.88596913666828,-1.,0.432493038548833));
#28513=CARTESIAN_POINT('Ctrl Pts',(1.89136993975585,-1.,0.43522566096358));
#28514=CARTESIAN_POINT('Ctrl Pts',(1.89663648956549,-1.,0.437995003948443));
#28515=CARTESIAN_POINT('Ctrl Pts',(1.90180124389137,-1.,0.440807833704161));
#28516=CARTESIAN_POINT('Ctrl Pts',(1.90691756144906,-1.,0.443677556849171));
#28517=CARTESIAN_POINT('Ctrl Pts',(1.91203699981095,-1.,0.446617343485651));
#28518=CARTESIAN_POINT('Ctrl Pts',(1.91718342555717,-1.,0.449632260106572));
#28519=CARTESIAN_POINT('Ctrl Pts',(1.9223538064847,-1.,0.452719478359356));
#28520=CARTESIAN_POINT('Ctrl Pts',(1.92753067150461,-1.,0.455872005174336));
#28521=CARTESIAN_POINT('Ctrl Pts',(1.93269066517936,-1.,0.459081234547932));
#28522=CARTESIAN_POINT('Ctrl Pts',(1.93781486640834,-1.,0.462340031009087));
#28523=CARTESIAN_POINT('Ctrl Pts',(1.94289794196205,-1.,0.465645462026065));
#28524=CARTESIAN_POINT('Ctrl Pts',(1.94794381136524,-1.,0.468997482913158));
#28525=CARTESIAN_POINT('Ctrl Pts',(1.95296148278136,-1.,0.47239767226408));
#28526=CARTESIAN_POINT('Ctrl Pts',(1.95796111148175,-1.,0.475848034683172));
#28527=CARTESIAN_POINT('Ctrl Pts',(1.96294933055938,-1.,0.479349583074846));
#28528=CARTESIAN_POINT('Ctrl Pts',(1.96792703422358,-1.,0.482901662120687));
#28529=CARTESIAN_POINT('Ctrl Pts',(1.97289186263272,-1.,0.486502692907661));
#28530=CARTESIAN_POINT('Ctrl Pts',(1.97783973019229,-1.,0.490150627860955));
#28531=CARTESIAN_POINT('Ctrl Pts',(1.9827665876182,-1.,0.493843476541493));
#28532=CARTESIAN_POINT('Ctrl Pts',(1.98767044752929,-1.,0.497579909545564));
#28533=CARTESIAN_POINT('Ctrl Pts',(1.9925514912615,-1.,0.501359287727129));
#28534=CARTESIAN_POINT('Ctrl Pts',(1.99741107463567,-1.,0.505181361323011));
#28535=CARTESIAN_POINT('Ctrl Pts',(2.00225107134733,-1.,0.509046069886152));
#28536=CARTESIAN_POINT('Ctrl Pts',(2.00707309946955,-1.,0.512953306961814));
#28537=CARTESIAN_POINT('Ctrl Pts',(2.01187773939257,-1.,0.516902681728733));
#28538=CARTESIAN_POINT('Ctrl Pts',(2.01666477917305,-1.,0.520893590399429));
#28539=CARTESIAN_POINT('Ctrl Pts',(2.02143356304712,-1.,0.524925318333519));
#28540=CARTESIAN_POINT('Ctrl Pts',(2.02618329083289,-1.,0.528997127241911));
#28541=CARTESIAN_POINT('Ctrl Pts',(2.03091336214401,-1.,0.533108355132905));
#28542=CARTESIAN_POINT('Ctrl Pts',(2.03562362953993,-1.,0.537258489833135));
#28543=CARTESIAN_POINT('Ctrl Pts',(2.0403142269048,-1.,0.54144712061552));
#28544=CARTESIAN_POINT('Ctrl Pts',(2.0449854471456,-1.,0.545673903817349));
#28545=CARTESIAN_POINT('Ctrl Pts',(2.04963761077974,-1.,0.549938525150342));
#28546=CARTESIAN_POINT('Ctrl Pts',(2.05427091604482,-1.,0.55424065746411));
#28547=CARTESIAN_POINT('Ctrl Pts',(2.05888537756571,-1.,0.558579940185468));
#28548=CARTESIAN_POINT('Ctrl Pts',(2.06348090160697,-1.,0.562955993082574));
#28549=CARTESIAN_POINT('Ctrl Pts',(2.06805732997383,-1.,0.56736842118123));
#28550=CARTESIAN_POINT('Ctrl Pts',(2.07261449292757,-1.,0.571816823242411));
#28551=CARTESIAN_POINT('Ctrl Pts',(2.07715226767361,-1.,0.576300797416275));
#28552=CARTESIAN_POINT('Ctrl Pts',(2.08167059018138,-1.,0.580819952107257));
#28553=CARTESIAN_POINT('Ctrl Pts',(2.086169437277,-1.,0.585373918990895));
#28554=CARTESIAN_POINT('Ctrl Pts',(2.09064881812053,-1.,0.58996236540319));
#28555=CARTESIAN_POINT('Ctrl Pts',(2.09510876220501,-1.,0.594585006052824));
#28556=CARTESIAN_POINT('Ctrl Pts',(2.09954930865331,-1.,0.599241616422144));
#28557=CARTESIAN_POINT('Ctrl Pts',(2.10397049887709,-1.,0.603932030738212));
#28558=CARTESIAN_POINT('Ctrl Pts',(2.10749199615859,-1.,0.607711315456826));
#28559=CARTESIAN_POINT('Ctrl Pts',(2.11012443807661,-1.,0.610560911691114));
#28560=CARTESIAN_POINT('Ctrl Pts',(2.11187554260142,-1.,0.61246736556225));
#28561=CARTESIAN_POINT('Ctrl Pts',(2.11275013067528,-1.,0.613422273260091));
#28562=CARTESIAN_POINT('',(2.0698113262342,-1.,0.745574324794401));
#28563=CARTESIAN_POINT('',(2.11275013067528,-1.,0.613422273260091));
#28564=CARTESIAN_POINT('Ctrl Pts',(2.0698113262342,-1.,0.745574324794401));
#28565=CARTESIAN_POINT('Ctrl Pts',(2.06854248895575,-1.,0.74583279137781));
#28566=CARTESIAN_POINT('Ctrl Pts',(2.06600523016401,-1.,0.746345871542696));
#28567=CARTESIAN_POINT('Ctrl Pts',(2.06220058927162,-1.,0.747103932785504));
#28568=CARTESIAN_POINT('Ctrl Pts',(2.05713023030263,-1.,0.748091554181101));
#28569=CARTESIAN_POINT('Ctrl Pts',(2.05079645591606,-1.,0.749287468663053));
#28570=CARTESIAN_POINT('Ctrl Pts',(2.04446689147754,-1.,0.750444657874758));
#28571=CARTESIAN_POINT('Ctrl Pts',(2.03814160092173,-1.,0.751562963361384));
#28572=CARTESIAN_POINT('Ctrl Pts',(2.03182068456467,-1.,0.752642180488104));
#28573=CARTESIAN_POINT('Ctrl Pts',(2.02550428623587,-1.,0.753682061113766));
#28574=CARTESIAN_POINT('Ctrl Pts',(2.01919259406003,-1.,0.75468233072352));
#28575=CARTESIAN_POINT('Ctrl Pts',(2.01288584328149,-1.,0.755642704958101));
#28576=CARTESIAN_POINT('Ctrl Pts',(2.00658431587682,-1.,0.756562904646496));
#28577=CARTESIAN_POINT('Ctrl Pts',(2.00028834739072,-1.,0.757442676862342));
#28578=CARTESIAN_POINT('Ctrl Pts',(1.9939983109871,-1.,0.758281796766377));
#28579=CARTESIAN_POINT('Ctrl Pts',(1.98771456680806,-1.,0.759080037802243));
#28580=CARTESIAN_POINT('Ctrl Pts',(1.98143741418156,-1.,0.759837147452135));
#28581=CARTESIAN_POINT('Ctrl Pts',(1.97516705321521,-1.,0.760552825409856));
#28582=CARTESIAN_POINT('Ctrl Pts',(1.96890351582545,-1.,0.761226690483986));
#28583=CARTESIAN_POINT('Ctrl Pts',(1.96264672744229,-1.,0.761858300014575));
#28584=CARTESIAN_POINT('Ctrl Pts',(1.95639665309893,-1.,0.762447203806264));
#28585=CARTESIAN_POINT('Ctrl Pts',(1.95015342590025,-1.,0.762992990878774));
#28586=CARTESIAN_POINT('Ctrl Pts',(1.94391746617626,-1.,0.763495333538581));
#28587=CARTESIAN_POINT('Ctrl Pts',(1.93768964875867,-1.,0.763954049121394));
#28588=CARTESIAN_POINT('Ctrl Pts',(1.93147105496367,-1.,0.76436901067389));
#28589=CARTESIAN_POINT('Ctrl Pts',(1.92526263537041,-1.,0.764740025488189));
#28590=CARTESIAN_POINT('Ctrl Pts',(1.91906491634197,-1.,0.765066729667095));
#28591=CARTESIAN_POINT('Ctrl Pts',(1.91287765805174,-1.,0.765348465884739));
#28592=CARTESIAN_POINT('Ctrl Pts',(1.90669961402362,-1.,0.765584196937937));
#28593=CARTESIAN_POINT('Ctrl Pts',(1.90052930393599,-1.,0.765772772593395));
#28594=CARTESIAN_POINT('Ctrl Pts',(1.89436577771389,-1.,0.765913193856979));
#28595=CARTESIAN_POINT('Ctrl Pts',(1.88820926433409,-1.,0.76600483706209));
#28596=CARTESIAN_POINT('Ctrl Pts',(1.88206215302561,-1.,0.766047794851869));
#28597=CARTESIAN_POINT('Ctrl Pts',(1.87592888967886,-1.,0.766042837036759));
#28598=CARTESIAN_POINT('Ctrl Pts',(1.86981398314345,-1.,0.765990708546112));
#28599=CARTESIAN_POINT('Ctrl Pts',(1.86372027063314,-1.,0.765891519092557));
#28600=CARTESIAN_POINT('Ctrl Pts',(1.85764741390391,-1.,0.765744212909305));
#28601=CARTESIAN_POINT('Ctrl Pts',(1.85158945130054,-1.,0.765545710619023));
#28602=CARTESIAN_POINT('Ctrl Pts',(1.8455369887591,-1.,0.765291664861972));
#28603=CARTESIAN_POINT('Ctrl Pts',(1.83948181064823,-1.,0.764978057881688));
#28604=CARTESIAN_POINT('Ctrl Pts',(1.8334207722714,-1.,0.764602549687846));
#28605=CARTESIAN_POINT('Ctrl Pts',(1.8273599120008,-1.,0.764165902606056));
#28606=CARTESIAN_POINT('Ctrl Pts',(1.82131873145297,-1.,0.763673465462854));
#28607=CARTESIAN_POINT('Ctrl Pts',(1.81532118405566,-1.,0.763132003836783));
#28608=CARTESIAN_POINT('Ctrl Pts',(1.80938551463989,-1.,0.762546129464036));
#28609=CARTESIAN_POINT('Ctrl Pts',(1.80351583877334,-1.,0.761915336443516));
#28610=CARTESIAN_POINT('Ctrl Pts',(1.79768986997735,-1.,0.761229695230359));
#28611=CARTESIAN_POINT('Ctrl Pts',(1.79185815610802,-1.,0.760469555880425));
#28612=CARTESIAN_POINT('Ctrl Pts',(1.78596964884526,-1.,0.759614401109868));
#28613=CARTESIAN_POINT('Ctrl Pts',(1.77999411220912,-1.,0.75865062667738));
#28614=CARTESIAN_POINT('Ctrl Pts',(1.77394167108342,-1.,0.757578264077238));
#28615=CARTESIAN_POINT('Ctrl Pts',(1.76789396003141,-1.,0.756421896028403));
#28616=CARTESIAN_POINT('Ctrl Pts',(1.7619781724032,-1.,0.755220979975262));
#28617=CARTESIAN_POINT('Ctrl Pts',(1.75631083600175,-1.,0.75400925402848));
#28618=CARTESIAN_POINT('Ctrl Pts',(1.75095139468809,-1.,0.752797683531377));
#28619=CARTESIAN_POINT('Ctrl Pts',(1.74585086852298,-1.,0.751555614163629));
#28620=CARTESIAN_POINT('Ctrl Pts',(1.74080458266705,-1.,0.750193435979541));
#28621=CARTESIAN_POINT('Ctrl Pts',(1.73550351679848,-1.,0.748582462954855));
#28622=CARTESIAN_POINT('Ctrl Pts',(1.72958533647399,-1.,0.746574710096437));
#28623=CARTESIAN_POINT('Ctrl Pts',(1.7226822991693,-1.,0.744021445433765));
#28624=CARTESIAN_POINT('Ctrl Pts',(1.71447789751927,-1.,0.740795162032088));
#28625=CARTESIAN_POINT('Ctrl Pts',(1.70473309006121,-1.,0.736799665724771));
#28626=CARTESIAN_POINT('Ctrl Pts',(1.69326921975743,-1.,0.731963238697195));
#28627=CARTESIAN_POINT('Ctrl Pts',(1.67996158455503,-1.,0.726235967997433));
#28628=CARTESIAN_POINT('Ctrl Pts',(1.6647288055568,-1.,0.719585433804282));
#28629=CARTESIAN_POINT('Ctrl Pts',(1.64752408832016,-1.,0.711993139355394));
#28630=CARTESIAN_POINT('Ctrl Pts',(1.63216541664676,-1.,0.705159151988319));
#28631=CARTESIAN_POINT('Ctrl Pts',(1.61974673472612,-1.,0.699605146405088));
#28632=CARTESIAN_POINT('Ctrl Pts',(1.61106790958151,-1.,0.695712097881194));
#28633=CARTESIAN_POINT('Ctrl Pts',(1.60662857109684,-1.,0.693717979106306));
#28634=CARTESIAN_POINT('Origin',(0.,-1.,0.));
#28635=CARTESIAN_POINT('Origin',(0.,0.,0.));
#28636=CARTESIAN_POINT('Origin',(0.,2.2,0.));
#28637=CARTESIAN_POINT('Origin',(0.,1.,0.));
#28638=CARTESIAN_POINT('',(-1.4,2.2,1.71450551880629E-16));
#28639=CARTESIAN_POINT('Origin',(0.,2.2,0.));
#28640=CARTESIAN_POINT('',(-1.4,1.,1.71450551880629E-16));
#28641=CARTESIAN_POINT('',(-1.4,1.,1.71450551880629E-16));
#28642=CARTESIAN_POINT('Origin',(0.,1.,0.));
#28643=CARTESIAN_POINT('Origin',(0.,2.2,0.));
#28644=CARTESIAN_POINT('Ctrl Pts',(2.11275013067528,-1.,0.613422273260091));
#28645=CARTESIAN_POINT('Ctrl Pts',(2.11275013067528,1.,0.613422273260091));
#28646=CARTESIAN_POINT('Ctrl Pts',(2.11187554260142,-1.,0.61246736556225));
#28647=CARTESIAN_POINT('Ctrl Pts',(2.11187554260142,1.,0.61246736556225));
#28648=CARTESIAN_POINT('Ctrl Pts',(2.11012443807661,-1.,0.610560911691114));
#28649=CARTESIAN_POINT('Ctrl Pts',(2.11012443807661,1.,0.610560911691114));
#28650=CARTESIAN_POINT('Ctrl Pts',(2.10749199615859,-1.,0.607711315456826));
#28651=CARTESIAN_POINT('Ctrl Pts',(2.10749199615859,1.,0.607711315456826));
#28652=CARTESIAN_POINT('Ctrl Pts',(2.10397049887709,-1.,0.603932030738212));
#28653=CARTESIAN_POINT('Ctrl Pts',(2.10397049887709,1.,0.603932030738212));
#28654=CARTESIAN_POINT('Ctrl Pts',(2.09954930865331,-1.,0.599241616422144));
#28655=CARTESIAN_POINT('Ctrl Pts',(2.09954930865331,1.,0.599241616422144));
#28656=CARTESIAN_POINT('Ctrl Pts',(2.09510876220501,-1.,0.594585006052824));
#28657=CARTESIAN_POINT('Ctrl Pts',(2.09510876220501,1.,0.594585006052824));
#28658=CARTESIAN_POINT('Ctrl Pts',(2.09064881812053,-1.,0.58996236540319));
#28659=CARTESIAN_POINT('Ctrl Pts',(2.09064881812053,1.,0.58996236540319));
#28660=CARTESIAN_POINT('Ctrl Pts',(2.086169437277,-1.,0.585373918990895));
#28661=CARTESIAN_POINT('Ctrl Pts',(2.086169437277,1.,0.585373918990895));
#28662=CARTESIAN_POINT('Ctrl Pts',(2.08167059018138,-1.,0.580819952107257));
#28663=CARTESIAN_POINT('Ctrl Pts',(2.08167059018138,1.,0.580819952107257));
#28664=CARTESIAN_POINT('Ctrl Pts',(2.07715226767361,-1.,0.576300797416275));
#28665=CARTESIAN_POINT('Ctrl Pts',(2.07715226767361,1.,0.576300797416275));
#28666=CARTESIAN_POINT('Ctrl Pts',(2.07261449292757,-1.,0.571816823242411));
#28667=CARTESIAN_POINT('Ctrl Pts',(2.07261449292757,1.,0.571816823242411));
#28668=CARTESIAN_POINT('Ctrl Pts',(2.06805732997383,-1.,0.56736842118123));
#28669=CARTESIAN_POINT('Ctrl Pts',(2.06805732997383,1.,0.56736842118123));
#28670=CARTESIAN_POINT('Ctrl Pts',(2.06348090160697,-1.,0.562955993082574));
#28671=CARTESIAN_POINT('Ctrl Pts',(2.06348090160697,1.,0.562955993082574));
#28672=CARTESIAN_POINT('Ctrl Pts',(2.05888537756571,-1.,0.558579940185468));
#28673=CARTESIAN_POINT('Ctrl Pts',(2.05888537756571,1.,0.558579940185468));
#28674=CARTESIAN_POINT('Ctrl Pts',(2.05427091604482,-1.,0.55424065746411));
#28675=CARTESIAN_POINT('Ctrl Pts',(2.05427091604482,1.,0.55424065746411));
#28676=CARTESIAN_POINT('Ctrl Pts',(2.04963761077974,-1.,0.549938525150342));
#28677=CARTESIAN_POINT('Ctrl Pts',(2.04963761077974,1.,0.549938525150342));
#28678=CARTESIAN_POINT('Ctrl Pts',(2.0449854471456,-1.,0.545673903817349));
#28679=CARTESIAN_POINT('Ctrl Pts',(2.0449854471456,1.,0.545673903817349));
#28680=CARTESIAN_POINT('Ctrl Pts',(2.0403142269048,-1.,0.54144712061552));
#28681=CARTESIAN_POINT('Ctrl Pts',(2.0403142269048,1.,0.54144712061552));
#28682=CARTESIAN_POINT('Ctrl Pts',(2.03562362953993,-1.,0.537258489833135));
#28683=CARTESIAN_POINT('Ctrl Pts',(2.03562362953993,1.,0.537258489833135));
#28684=CARTESIAN_POINT('Ctrl Pts',(2.03091336214401,-1.,0.533108355132905));
#28685=CARTESIAN_POINT('Ctrl Pts',(2.03091336214401,1.,0.533108355132905));
#28686=CARTESIAN_POINT('Ctrl Pts',(2.02618329083289,-1.,0.528997127241911));
#28687=CARTESIAN_POINT('Ctrl Pts',(2.02618329083289,1.,0.528997127241911));
#28688=CARTESIAN_POINT('Ctrl Pts',(2.02143356304712,-1.,0.524925318333519));
#28689=CARTESIAN_POINT('Ctrl Pts',(2.02143356304712,1.,0.524925318333519));
#28690=CARTESIAN_POINT('Ctrl Pts',(2.01666477917305,-1.,0.520893590399429));
#28691=CARTESIAN_POINT('Ctrl Pts',(2.01666477917305,1.,0.520893590399429));
#28692=CARTESIAN_POINT('Ctrl Pts',(2.01187773939257,-1.,0.516902681728733));
#28693=CARTESIAN_POINT('Ctrl Pts',(2.01187773939257,1.,0.516902681728733));
#28694=CARTESIAN_POINT('Ctrl Pts',(2.00707309946955,-1.,0.512953306961814));
#28695=CARTESIAN_POINT('Ctrl Pts',(2.00707309946955,1.,0.512953306961814));
#28696=CARTESIAN_POINT('Ctrl Pts',(2.00225107134733,-1.,0.509046069886152));
#28697=CARTESIAN_POINT('Ctrl Pts',(2.00225107134733,1.,0.509046069886152));
#28698=CARTESIAN_POINT('Ctrl Pts',(1.99741107463567,-1.,0.505181361323011));
#28699=CARTESIAN_POINT('Ctrl Pts',(1.99741107463567,1.,0.505181361323011));
#28700=CARTESIAN_POINT('Ctrl Pts',(1.9925514912615,-1.,0.501359287727129));
#28701=CARTESIAN_POINT('Ctrl Pts',(1.9925514912615,1.,0.501359287727129));
#28702=CARTESIAN_POINT('Ctrl Pts',(1.98767044752929,-1.,0.497579909545564));
#28703=CARTESIAN_POINT('Ctrl Pts',(1.98767044752929,1.,0.497579909545564));
#28704=CARTESIAN_POINT('Ctrl Pts',(1.9827665876182,-1.,0.493843476541493));
#28705=CARTESIAN_POINT('Ctrl Pts',(1.9827665876182,1.,0.493843476541493));
#28706=CARTESIAN_POINT('Ctrl Pts',(1.97783973019229,-1.,0.490150627860955));
#28707=CARTESIAN_POINT('Ctrl Pts',(1.97783973019229,1.,0.490150627860955));
#28708=CARTESIAN_POINT('Ctrl Pts',(1.97289186263272,-1.,0.486502692907661));
#28709=CARTESIAN_POINT('Ctrl Pts',(1.97289186263272,1.,0.486502692907661));
#28710=CARTESIAN_POINT('Ctrl Pts',(1.96792703422358,-1.,0.482901662120687));
#28711=CARTESIAN_POINT('Ctrl Pts',(1.96792703422358,1.,0.482901662120687));
#28712=CARTESIAN_POINT('Ctrl Pts',(1.96294933055938,-1.,0.479349583074846));
#28713=CARTESIAN_POINT('Ctrl Pts',(1.96294933055938,1.,0.479349583074846));
#28714=CARTESIAN_POINT('Ctrl Pts',(1.95796111148175,-1.,0.475848034683172));
#28715=CARTESIAN_POINT('Ctrl Pts',(1.95796111148175,1.,0.475848034683172));
#28716=CARTESIAN_POINT('Ctrl Pts',(1.95296148278136,-1.,0.47239767226408));
#28717=CARTESIAN_POINT('Ctrl Pts',(1.95296148278136,1.,0.47239767226408));
#28718=CARTESIAN_POINT('Ctrl Pts',(1.94794381136524,-1.,0.468997482913158));
#28719=CARTESIAN_POINT('Ctrl Pts',(1.94794381136524,1.,0.468997482913158));
#28720=CARTESIAN_POINT('Ctrl Pts',(1.94289794196205,-1.,0.465645462026065));
#28721=CARTESIAN_POINT('Ctrl Pts',(1.94289794196205,1.,0.465645462026065));
#28722=CARTESIAN_POINT('Ctrl Pts',(1.93781486640834,-1.,0.462340031009087));
#28723=CARTESIAN_POINT('Ctrl Pts',(1.93781486640834,1.,0.462340031009087));
#28724=CARTESIAN_POINT('Ctrl Pts',(1.93269066517936,-1.,0.459081234547932));
#28725=CARTESIAN_POINT('Ctrl Pts',(1.93269066517936,1.,0.459081234547932));
#28726=CARTESIAN_POINT('Ctrl Pts',(1.92753067150461,-1.,0.455872005174336));
#28727=CARTESIAN_POINT('Ctrl Pts',(1.92753067150461,1.,0.455872005174336));
#28728=CARTESIAN_POINT('Ctrl Pts',(1.9223538064847,-1.,0.452719478359356));
#28729=CARTESIAN_POINT('Ctrl Pts',(1.9223538064847,1.,0.452719478359356));
#28730=CARTESIAN_POINT('Ctrl Pts',(1.91718342555717,-1.,0.449632260106572));
#28731=CARTESIAN_POINT('Ctrl Pts',(1.91718342555717,1.,0.449632260106572));
#28732=CARTESIAN_POINT('Ctrl Pts',(1.91203699981095,-1.,0.446617343485651));
#28733=CARTESIAN_POINT('Ctrl Pts',(1.91203699981095,1.,0.446617343485651));
#28734=CARTESIAN_POINT('Ctrl Pts',(1.90691756144906,-1.,0.443677556849171));
#28735=CARTESIAN_POINT('Ctrl Pts',(1.90691756144906,1.,0.443677556849171));
#28736=CARTESIAN_POINT('Ctrl Pts',(1.90180124389137,-1.,0.440807833704161));
#28737=CARTESIAN_POINT('Ctrl Pts',(1.90180124389137,1.,0.440807833704161));
#28738=CARTESIAN_POINT('Ctrl Pts',(1.89663648956549,-1.,0.437995003948443));
#28739=CARTESIAN_POINT('Ctrl Pts',(1.89663648956549,1.,0.437995003948443));
#28740=CARTESIAN_POINT('Ctrl Pts',(1.89136993975585,-1.,0.43522566096358));
#28741=CARTESIAN_POINT('Ctrl Pts',(1.89136993975585,1.,0.43522566096358));
#28742=CARTESIAN_POINT('Ctrl Pts',(1.88596913666828,-1.,0.432493038548833));
#28743=CARTESIAN_POINT('Ctrl Pts',(1.88596913666828,1.,0.432493038548833));
#28744=CARTESIAN_POINT('Ctrl Pts',(1.88044229001778,-1.,0.429803062482217));
#28745=CARTESIAN_POINT('Ctrl Pts',(1.88044229001778,1.,0.429803062482217));
#28746=CARTESIAN_POINT('Ctrl Pts',(1.87486989291333,-1.,0.427183828518743));
#28747=CARTESIAN_POINT('Ctrl Pts',(1.87486989291333,1.,0.427183828518743));
#28748=CARTESIAN_POINT('Ctrl Pts',(1.8693780394412,-1.,0.424678177290876));
#28749=CARTESIAN_POINT('Ctrl Pts',(1.8693780394412,1.,0.424678177290876));
#28750=CARTESIAN_POINT('Ctrl Pts',(1.86408083333863,-1.,0.422327307417885));
#28751=CARTESIAN_POINT('Ctrl Pts',(1.86408083333863,1.,0.422327307417885));
#28752=CARTESIAN_POINT('Ctrl Pts',(1.8590328109667,-1.,0.420157287975583));
#28753=CARTESIAN_POINT('Ctrl Pts',(1.8590328109667,1.,0.420157287975583));
#28754=CARTESIAN_POINT('Ctrl Pts',(1.8541763285645,-1.,0.418164129144046));
#28755=CARTESIAN_POINT('Ctrl Pts',(1.8541763285645,1.,0.418164129144046));
#28756=CARTESIAN_POINT('Ctrl Pts',(1.84929312930314,-1.,0.416300022039885));
#28757=CARTESIAN_POINT('Ctrl Pts',(1.84929312930314,1.,0.416300022039885));
#28758=CARTESIAN_POINT('Ctrl Pts',(1.84405757074218,-1.,0.414487438255542));
#28759=CARTESIAN_POINT('Ctrl Pts',(1.84405757074218,1.,0.414487438255542));
#28760=CARTESIAN_POINT('Ctrl Pts',(1.8380895347617,-1.,0.412633125322945));
#28761=CARTESIAN_POINT('Ctrl Pts',(1.8380895347617,1.,0.412633125322945));
#28762=CARTESIAN_POINT('Ctrl Pts',(1.83100408895047,-1.,0.410641256301276));
#28763=CARTESIAN_POINT('Ctrl Pts',(1.83100408895047,1.,0.410641256301276));
#28764=CARTESIAN_POINT('Ctrl Pts',(1.82247022677562,-1.,0.408428948106228));
#28765=CARTESIAN_POINT('Ctrl Pts',(1.82247022677562,1.,0.408428948106228));
#28766=CARTESIAN_POINT('Ctrl Pts',(1.81223801812013,-1.,0.405933518407176));
#28767=CARTESIAN_POINT('Ctrl Pts',(1.81223801812013,1.,0.405933518407176));
#28768=CARTESIAN_POINT('Ctrl Pts',(1.80012077173238,-1.,0.403107976163396));
#28769=CARTESIAN_POINT('Ctrl Pts',(1.80012077173238,1.,0.403107976163396));
#28770=CARTESIAN_POINT('Ctrl Pts',(1.78598826343754,-1.,0.399919403774156));
#28771=CARTESIAN_POINT('Ctrl Pts',(1.78598826343754,1.,0.399919403774156));
#28772=CARTESIAN_POINT('Ctrl Pts',(1.76975560043442,-1.,0.396346196110688));
#28773=CARTESIAN_POINT('Ctrl Pts',(1.76975560043442,1.,0.396346196110688));
#28774=CARTESIAN_POINT('Ctrl Pts',(1.75137405310193,-1.,0.392375812285396));
#28775=CARTESIAN_POINT('Ctrl Pts',(1.75137405310193,1.,0.392375812285396));
#28776=CARTESIAN_POINT('Ctrl Pts',(1.73493170972829,-1.,0.388877023502615));
#28777=CARTESIAN_POINT('Ctrl Pts',(1.73493170972829,1.,0.388877023502615));
#28778=CARTESIAN_POINT('Ctrl Pts',(1.72162022244582,-1.,0.386070790323281));
#28779=CARTESIAN_POINT('Ctrl Pts',(1.72162022244582,1.,0.386070790323281));
#28780=CARTESIAN_POINT('Ctrl Pts',(1.71231062891398,-1.,0.384119047314215));
#28781=CARTESIAN_POINT('Ctrl Pts',(1.71231062891398,1.,0.384119047314215));
#28782=CARTESIAN_POINT('Ctrl Pts',(1.7075470150345,-1.,0.383122945602004));
#28783=CARTESIAN_POINT('Ctrl Pts',(1.7075470150345,1.,0.383122945602004));
#28784=CARTESIAN_POINT('',(1.7075470150345,1.,0.383122945602004));
#28785=CARTESIAN_POINT('',(1.7075470150345,0.,0.383122945602005));
#28786=CARTESIAN_POINT('',(2.11275013067528,1.,0.613422273260091));
#28787=CARTESIAN_POINT('Ctrl Pts',(2.11275013067528,1.,0.613422273260091));
#28788=CARTESIAN_POINT('Ctrl Pts',(2.11187554260142,1.,0.61246736556225));
#28789=CARTESIAN_POINT('Ctrl Pts',(2.11012443807661,1.,0.610560911691114));
#28790=CARTESIAN_POINT('Ctrl Pts',(2.10749199615859,1.,0.607711315456826));
#28791=CARTESIAN_POINT('Ctrl Pts',(2.10397049887709,1.,0.603932030738212));
#28792=CARTESIAN_POINT('Ctrl Pts',(2.09954930865331,1.,0.599241616422144));
#28793=CARTESIAN_POINT('Ctrl Pts',(2.09510876220501,1.,0.594585006052824));
#28794=CARTESIAN_POINT('Ctrl Pts',(2.09064881812053,1.,0.58996236540319));
#28795=CARTESIAN_POINT('Ctrl Pts',(2.086169437277,1.,0.585373918990895));
#28796=CARTESIAN_POINT('Ctrl Pts',(2.08167059018138,1.,0.580819952107257));
#28797=CARTESIAN_POINT('Ctrl Pts',(2.07715226767361,1.,0.576300797416275));
#28798=CARTESIAN_POINT('Ctrl Pts',(2.07261449292757,1.,0.571816823242411));
#28799=CARTESIAN_POINT('Ctrl Pts',(2.06805732997383,1.,0.56736842118123));
#28800=CARTESIAN_POINT('Ctrl Pts',(2.06348090160697,1.,0.562955993082574));
#28801=CARTESIAN_POINT('Ctrl Pts',(2.05888537756571,1.,0.558579940185468));
#28802=CARTESIAN_POINT('Ctrl Pts',(2.05427091604482,1.,0.55424065746411));
#28803=CARTESIAN_POINT('Ctrl Pts',(2.04963761077974,1.,0.549938525150342));
#28804=CARTESIAN_POINT('Ctrl Pts',(2.0449854471456,1.,0.545673903817349));
#28805=CARTESIAN_POINT('Ctrl Pts',(2.0403142269048,1.,0.54144712061552));
#28806=CARTESIAN_POINT('Ctrl Pts',(2.03562362953993,1.,0.537258489833135));
#28807=CARTESIAN_POINT('Ctrl Pts',(2.03091336214401,1.,0.533108355132905));
#28808=CARTESIAN_POINT('Ctrl Pts',(2.02618329083289,1.,0.528997127241911));
#28809=CARTESIAN_POINT('Ctrl Pts',(2.02143356304712,1.,0.524925318333519));
#28810=CARTESIAN_POINT('Ctrl Pts',(2.01666477917305,1.,0.520893590399429));
#28811=CARTESIAN_POINT('Ctrl Pts',(2.01187773939257,1.,0.516902681728733));
#28812=CARTESIAN_POINT('Ctrl Pts',(2.00707309946955,1.,0.512953306961814));
#28813=CARTESIAN_POINT('Ctrl Pts',(2.00225107134733,1.,0.509046069886152));
#28814=CARTESIAN_POINT('Ctrl Pts',(1.99741107463567,1.,0.505181361323011));
#28815=CARTESIAN_POINT('Ctrl Pts',(1.9925514912615,1.,0.501359287727129));
#28816=CARTESIAN_POINT('Ctrl Pts',(1.98767044752929,1.,0.497579909545564));
#28817=CARTESIAN_POINT('Ctrl Pts',(1.9827665876182,1.,0.493843476541493));
#28818=CARTESIAN_POINT('Ctrl Pts',(1.97783973019229,1.,0.490150627860955));
#28819=CARTESIAN_POINT('Ctrl Pts',(1.97289186263272,1.,0.486502692907661));
#28820=CARTESIAN_POINT('Ctrl Pts',(1.96792703422358,1.,0.482901662120687));
#28821=CARTESIAN_POINT('Ctrl Pts',(1.96294933055938,1.,0.479349583074846));
#28822=CARTESIAN_POINT('Ctrl Pts',(1.95796111148175,1.,0.475848034683172));
#28823=CARTESIAN_POINT('Ctrl Pts',(1.95296148278136,1.,0.47239767226408));
#28824=CARTESIAN_POINT('Ctrl Pts',(1.94794381136524,1.,0.468997482913158));
#28825=CARTESIAN_POINT('Ctrl Pts',(1.94289794196205,1.,0.465645462026065));
#28826=CARTESIAN_POINT('Ctrl Pts',(1.93781486640834,1.,0.462340031009087));
#28827=CARTESIAN_POINT('Ctrl Pts',(1.93269066517936,1.,0.459081234547932));
#28828=CARTESIAN_POINT('Ctrl Pts',(1.92753067150461,1.,0.455872005174336));
#28829=CARTESIAN_POINT('Ctrl Pts',(1.9223538064847,1.,0.452719478359356));
#28830=CARTESIAN_POINT('Ctrl Pts',(1.91718342555717,1.,0.449632260106572));
#28831=CARTESIAN_POINT('Ctrl Pts',(1.91203699981095,1.,0.446617343485651));
#28832=CARTESIAN_POINT('Ctrl Pts',(1.90691756144906,1.,0.443677556849171));
#28833=CARTESIAN_POINT('Ctrl Pts',(1.90180124389137,1.,0.440807833704161));
#28834=CARTESIAN_POINT('Ctrl Pts',(1.89663648956549,1.,0.437995003948443));
#28835=CARTESIAN_POINT('Ctrl Pts',(1.89136993975585,1.,0.43522566096358));
#28836=CARTESIAN_POINT('Ctrl Pts',(1.88596913666828,1.,0.432493038548833));
#28837=CARTESIAN_POINT('Ctrl Pts',(1.88044229001778,1.,0.429803062482217));
#28838=CARTESIAN_POINT('Ctrl Pts',(1.87486989291333,1.,0.427183828518743));
#28839=CARTESIAN_POINT('Ctrl Pts',(1.8693780394412,1.,0.424678177290876));
#28840=CARTESIAN_POINT('Ctrl Pts',(1.86408083333863,1.,0.422327307417885));
#28841=CARTESIAN_POINT('Ctrl Pts',(1.8590328109667,1.,0.420157287975583));
#28842=CARTESIAN_POINT('Ctrl Pts',(1.8541763285645,1.,0.418164129144046));
#28843=CARTESIAN_POINT('Ctrl Pts',(1.84929312930314,1.,0.416300022039885));
#28844=CARTESIAN_POINT('Ctrl Pts',(1.84405757074218,1.,0.414487438255542));
#28845=CARTESIAN_POINT('Ctrl Pts',(1.8380895347617,1.,0.412633125322945));
#28846=CARTESIAN_POINT('Ctrl Pts',(1.83100408895047,1.,0.410641256301276));
#28847=CARTESIAN_POINT('Ctrl Pts',(1.82247022677562,1.,0.408428948106228));
#28848=CARTESIAN_POINT('Ctrl Pts',(1.81223801812013,1.,0.405933518407176));
#28849=CARTESIAN_POINT('Ctrl Pts',(1.80012077173238,1.,0.403107976163396));
#28850=CARTESIAN_POINT('Ctrl Pts',(1.78598826343754,1.,0.399919403774156));
#28851=CARTESIAN_POINT('Ctrl Pts',(1.76975560043442,1.,0.396346196110688));
#28852=CARTESIAN_POINT('Ctrl Pts',(1.75137405310193,1.,0.392375812285396));
#28853=CARTESIAN_POINT('Ctrl Pts',(1.73493170972829,1.,0.388877023502615));
#28854=CARTESIAN_POINT('Ctrl Pts',(1.72162022244582,1.,0.386070790323281));
#28855=CARTESIAN_POINT('Ctrl Pts',(1.71231062891398,1.,0.384119047314215));
#28856=CARTESIAN_POINT('Ctrl Pts',(1.7075470150345,1.,0.383122945602004));
#28857=CARTESIAN_POINT('',(2.11275013067528,0.,0.613422273260091));
#28858=CARTESIAN_POINT('Origin',(2.0698113262342,0.,0.745574324794401));
#28859=CARTESIAN_POINT('',(2.0698113262342,1.,0.745574324794401));
#28860=CARTESIAN_POINT('',(2.11275013067528,1.,0.613422273260091));
#28861=CARTESIAN_POINT('',(2.0698113262342,0.,0.745574324794401));
#28862=CARTESIAN_POINT('Ctrl Pts',(1.60662857109684,-1.,0.693717979106306));
#28863=CARTESIAN_POINT('Ctrl Pts',(1.60662857109684,1.,0.693717979106306));
#28864=CARTESIAN_POINT('Ctrl Pts',(1.61106790958151,-1.,0.695712097881194));
#28865=CARTESIAN_POINT('Ctrl Pts',(1.61106790958151,1.,0.695712097881194));
#28866=CARTESIAN_POINT('Ctrl Pts',(1.61974673472612,-1.,0.699605146405088));
#28867=CARTESIAN_POINT('Ctrl Pts',(1.61974673472612,1.,0.699605146405088));
#28868=CARTESIAN_POINT('Ctrl Pts',(1.63216541664676,-1.,0.705159151988319));
#28869=CARTESIAN_POINT('Ctrl Pts',(1.63216541664676,1.,0.705159151988319));
#28870=CARTESIAN_POINT('Ctrl Pts',(1.64752408832016,-1.,0.711993139355394));
#28871=CARTESIAN_POINT('Ctrl Pts',(1.64752408832016,1.,0.711993139355394));
#28872=CARTESIAN_POINT('Ctrl Pts',(1.6647288055568,-1.,0.719585433804282));
#28873=CARTESIAN_POINT('Ctrl Pts',(1.6647288055568,1.,0.719585433804282));
#28874=CARTESIAN_POINT('Ctrl Pts',(1.67996158455503,-1.,0.726235967997433));
#28875=CARTESIAN_POINT('Ctrl Pts',(1.67996158455503,1.,0.726235967997433));
#28876=CARTESIAN_POINT('Ctrl Pts',(1.69326921975743,-1.,0.731963238697195));
#28877=CARTESIAN_POINT('Ctrl Pts',(1.69326921975743,1.,0.731963238697195));
#28878=CARTESIAN_POINT('Ctrl Pts',(1.70473309006121,-1.,0.736799665724771));
#28879=CARTESIAN_POINT('Ctrl Pts',(1.70473309006121,1.,0.736799665724771));
#28880=CARTESIAN_POINT('Ctrl Pts',(1.71447789751927,-1.,0.740795162032088));
#28881=CARTESIAN_POINT('Ctrl Pts',(1.71447789751927,1.,0.740795162032088));
#28882=CARTESIAN_POINT('Ctrl Pts',(1.7226822991693,-1.,0.744021445433765));
#28883=CARTESIAN_POINT('Ctrl Pts',(1.7226822991693,1.,0.744021445433765));
#28884=CARTESIAN_POINT('Ctrl Pts',(1.72958533647399,-1.,0.746574710096437));
#28885=CARTESIAN_POINT('Ctrl Pts',(1.72958533647399,1.,0.746574710096437));
#28886=CARTESIAN_POINT('Ctrl Pts',(1.73550351679848,-1.,0.748582462954855));
#28887=CARTESIAN_POINT('Ctrl Pts',(1.73550351679848,1.,0.748582462954855));
#28888=CARTESIAN_POINT('Ctrl Pts',(1.74080458266705,-1.,0.750193435979541));
#28889=CARTESIAN_POINT('Ctrl Pts',(1.74080458266705,1.,0.750193435979541));
#28890=CARTESIAN_POINT('Ctrl Pts',(1.74585086852298,-1.,0.751555614163629));
#28891=CARTESIAN_POINT('Ctrl Pts',(1.74585086852298,1.,0.751555614163629));
#28892=CARTESIAN_POINT('Ctrl Pts',(1.75095139468809,-1.,0.752797683531377));
#28893=CARTESIAN_POINT('Ctrl Pts',(1.75095139468809,1.,0.752797683531377));
#28894=CARTESIAN_POINT('Ctrl Pts',(1.75631083600175,-1.,0.75400925402848));
#28895=CARTESIAN_POINT('Ctrl Pts',(1.75631083600175,1.,0.75400925402848));
#28896=CARTESIAN_POINT('Ctrl Pts',(1.7619781724032,-1.,0.755220979975262));
#28897=CARTESIAN_POINT('Ctrl Pts',(1.7619781724032,1.,0.755220979975262));
#28898=CARTESIAN_POINT('Ctrl Pts',(1.76789396003141,-1.,0.756421896028403));
#28899=CARTESIAN_POINT('Ctrl Pts',(1.76789396003141,1.,0.756421896028403));
#28900=CARTESIAN_POINT('Ctrl Pts',(1.77394167108342,-1.,0.757578264077238));
#28901=CARTESIAN_POINT('Ctrl Pts',(1.77394167108342,1.,0.757578264077238));
#28902=CARTESIAN_POINT('Ctrl Pts',(1.77999411220912,-1.,0.75865062667738));
#28903=CARTESIAN_POINT('Ctrl Pts',(1.77999411220912,1.,0.75865062667738));
#28904=CARTESIAN_POINT('Ctrl Pts',(1.78596964884526,-1.,0.759614401109868));
#28905=CARTESIAN_POINT('Ctrl Pts',(1.78596964884526,1.,0.759614401109868));
#28906=CARTESIAN_POINT('Ctrl Pts',(1.79185815610802,-1.,0.760469555880425));
#28907=CARTESIAN_POINT('Ctrl Pts',(1.79185815610802,1.,0.760469555880425));
#28908=CARTESIAN_POINT('Ctrl Pts',(1.79768986997735,-1.,0.761229695230359));
#28909=CARTESIAN_POINT('Ctrl Pts',(1.79768986997735,1.,0.761229695230359));
#28910=CARTESIAN_POINT('Ctrl Pts',(1.80351583877334,-1.,0.761915336443516));
#28911=CARTESIAN_POINT('Ctrl Pts',(1.80351583877334,1.,0.761915336443516));
#28912=CARTESIAN_POINT('Ctrl Pts',(1.80938551463989,-1.,0.762546129464036));
#28913=CARTESIAN_POINT('Ctrl Pts',(1.80938551463989,1.,0.762546129464036));
#28914=CARTESIAN_POINT('Ctrl Pts',(1.81532118405566,-1.,0.763132003836783));
#28915=CARTESIAN_POINT('Ctrl Pts',(1.81532118405566,1.,0.763132003836783));
#28916=CARTESIAN_POINT('Ctrl Pts',(1.82131873145297,-1.,0.763673465462854));
#28917=CARTESIAN_POINT('Ctrl Pts',(1.82131873145297,1.,0.763673465462854));
#28918=CARTESIAN_POINT('Ctrl Pts',(1.8273599120008,-1.,0.764165902606056));
#28919=CARTESIAN_POINT('Ctrl Pts',(1.8273599120008,1.,0.764165902606056));
#28920=CARTESIAN_POINT('Ctrl Pts',(1.8334207722714,-1.,0.764602549687846));
#28921=CARTESIAN_POINT('Ctrl Pts',(1.8334207722714,1.,0.764602549687846));
#28922=CARTESIAN_POINT('Ctrl Pts',(1.83948181064823,-1.,0.764978057881688));
#28923=CARTESIAN_POINT('Ctrl Pts',(1.83948181064823,1.,0.764978057881688));
#28924=CARTESIAN_POINT('Ctrl Pts',(1.8455369887591,-1.,0.765291664861972));
#28925=CARTESIAN_POINT('Ctrl Pts',(1.8455369887591,1.,0.765291664861972));
#28926=CARTESIAN_POINT('Ctrl Pts',(1.85158945130054,-1.,0.765545710619023));
#28927=CARTESIAN_POINT('Ctrl Pts',(1.85158945130054,1.,0.765545710619023));
#28928=CARTESIAN_POINT('Ctrl Pts',(1.85764741390391,-1.,0.765744212909305));
#28929=CARTESIAN_POINT('Ctrl Pts',(1.85764741390391,1.,0.765744212909305));
#28930=CARTESIAN_POINT('Ctrl Pts',(1.86372027063314,-1.,0.765891519092557));
#28931=CARTESIAN_POINT('Ctrl Pts',(1.86372027063314,1.,0.765891519092557));
#28932=CARTESIAN_POINT('Ctrl Pts',(1.86981398314345,-1.,0.765990708546112));
#28933=CARTESIAN_POINT('Ctrl Pts',(1.86981398314345,1.,0.765990708546112));
#28934=CARTESIAN_POINT('Ctrl Pts',(1.87592888967886,-1.,0.766042837036759));
#28935=CARTESIAN_POINT('Ctrl Pts',(1.87592888967886,1.,0.766042837036759));
#28936=CARTESIAN_POINT('Ctrl Pts',(1.88206215302561,-1.,0.766047794851869));
#28937=CARTESIAN_POINT('Ctrl Pts',(1.88206215302561,1.,0.766047794851869));
#28938=CARTESIAN_POINT('Ctrl Pts',(1.88820926433409,-1.,0.76600483706209));
#28939=CARTESIAN_POINT('Ctrl Pts',(1.88820926433409,1.,0.76600483706209));
#28940=CARTESIAN_POINT('Ctrl Pts',(1.89436577771389,-1.,0.765913193856979));
#28941=CARTESIAN_POINT('Ctrl Pts',(1.89436577771389,1.,0.765913193856979));
#28942=CARTESIAN_POINT('Ctrl Pts',(1.90052930393599,-1.,0.765772772593395));
#28943=CARTESIAN_POINT('Ctrl Pts',(1.90052930393599,1.,0.765772772593395));
#28944=CARTESIAN_POINT('Ctrl Pts',(1.90669961402362,-1.,0.765584196937937));
#28945=CARTESIAN_POINT('Ctrl Pts',(1.90669961402362,1.,0.765584196937937));
#28946=CARTESIAN_POINT('Ctrl Pts',(1.91287765805174,-1.,0.765348465884739));
#28947=CARTESIAN_POINT('Ctrl Pts',(1.91287765805174,1.,0.765348465884739));
#28948=CARTESIAN_POINT('Ctrl Pts',(1.91906491634197,-1.,0.765066729667095));
#28949=CARTESIAN_POINT('Ctrl Pts',(1.91906491634197,1.,0.765066729667095));
#28950=CARTESIAN_POINT('Ctrl Pts',(1.92526263537041,-1.,0.764740025488189));
#28951=CARTESIAN_POINT('Ctrl Pts',(1.92526263537041,1.,0.764740025488189));
#28952=CARTESIAN_POINT('Ctrl Pts',(1.93147105496367,-1.,0.76436901067389));
#28953=CARTESIAN_POINT('Ctrl Pts',(1.93147105496367,1.,0.76436901067389));
#28954=CARTESIAN_POINT('Ctrl Pts',(1.93768964875867,-1.,0.763954049121394));
#28955=CARTESIAN_POINT('Ctrl Pts',(1.93768964875867,1.,0.763954049121394));
#28956=CARTESIAN_POINT('Ctrl Pts',(1.94391746617626,-1.,0.763495333538581));
#28957=CARTESIAN_POINT('Ctrl Pts',(1.94391746617626,1.,0.763495333538581));
#28958=CARTESIAN_POINT('Ctrl Pts',(1.95015342590025,-1.,0.762992990878774));
#28959=CARTESIAN_POINT('Ctrl Pts',(1.95015342590025,1.,0.762992990878774));
#28960=CARTESIAN_POINT('Ctrl Pts',(1.95639665309893,-1.,0.762447203806264));
#28961=CARTESIAN_POINT('Ctrl Pts',(1.95639665309893,1.,0.762447203806264));
#28962=CARTESIAN_POINT('Ctrl Pts',(1.96264672744229,-1.,0.761858300014575));
#28963=CARTESIAN_POINT('Ctrl Pts',(1.96264672744229,1.,0.761858300014575));
#28964=CARTESIAN_POINT('Ctrl Pts',(1.96890351582545,-1.,0.761226690483986));
#28965=CARTESIAN_POINT('Ctrl Pts',(1.96890351582545,1.,0.761226690483986));
#28966=CARTESIAN_POINT('Ctrl Pts',(1.97516705321521,-1.,0.760552825409856));
#28967=CARTESIAN_POINT('Ctrl Pts',(1.97516705321521,1.,0.760552825409856));
#28968=CARTESIAN_POINT('Ctrl Pts',(1.98143741418156,-1.,0.759837147452135));
#28969=CARTESIAN_POINT('Ctrl Pts',(1.98143741418156,1.,0.759837147452135));
#28970=CARTESIAN_POINT('Ctrl Pts',(1.98771456680806,-1.,0.759080037802243));
#28971=CARTESIAN_POINT('Ctrl Pts',(1.98771456680806,1.,0.759080037802243));
#28972=CARTESIAN_POINT('Ctrl Pts',(1.9939983109871,-1.,0.758281796766377));
#28973=CARTESIAN_POINT('Ctrl Pts',(1.9939983109871,1.,0.758281796766377));
#28974=CARTESIAN_POINT('Ctrl Pts',(2.00028834739072,-1.,0.757442676862342));
#28975=CARTESIAN_POINT('Ctrl Pts',(2.00028834739072,1.,0.757442676862342));
#28976=CARTESIAN_POINT('Ctrl Pts',(2.00658431587682,-1.,0.756562904646496));
#28977=CARTESIAN_POINT('Ctrl Pts',(2.00658431587682,1.,0.756562904646496));
#28978=CARTESIAN_POINT('Ctrl Pts',(2.01288584328149,-1.,0.755642704958101));
#28979=CARTESIAN_POINT('Ctrl Pts',(2.01288584328149,1.,0.755642704958101));
#28980=CARTESIAN_POINT('Ctrl Pts',(2.01919259406003,-1.,0.75468233072352));
#28981=CARTESIAN_POINT('Ctrl Pts',(2.01919259406003,1.,0.75468233072352));
#28982=CARTESIAN_POINT('Ctrl Pts',(2.02550428623587,-1.,0.753682061113766));
#28983=CARTESIAN_POINT('Ctrl Pts',(2.02550428623587,1.,0.753682061113766));
#28984=CARTESIAN_POINT('Ctrl Pts',(2.03182068456467,-1.,0.752642180488104));
#28985=CARTESIAN_POINT('Ctrl Pts',(2.03182068456467,1.,0.752642180488104));
#28986=CARTESIAN_POINT('Ctrl Pts',(2.03814160092173,-1.,0.751562963361384));
#28987=CARTESIAN_POINT('Ctrl Pts',(2.03814160092173,1.,0.751562963361384));
#28988=CARTESIAN_POINT('Ctrl Pts',(2.04446689147754,-1.,0.750444657874758));
#28989=CARTESIAN_POINT('Ctrl Pts',(2.04446689147754,1.,0.750444657874758));
#28990=CARTESIAN_POINT('Ctrl Pts',(2.05079645591606,-1.,0.749287468663053));
#28991=CARTESIAN_POINT('Ctrl Pts',(2.05079645591606,1.,0.749287468663053));
#28992=CARTESIAN_POINT('Ctrl Pts',(2.05713023030263,-1.,0.748091554181101));
#28993=CARTESIAN_POINT('Ctrl Pts',(2.05713023030263,1.,0.748091554181101));
#28994=CARTESIAN_POINT('Ctrl Pts',(2.06220058927162,-1.,0.747103932785504));
#28995=CARTESIAN_POINT('Ctrl Pts',(2.06220058927162,1.,0.747103932785504));
#28996=CARTESIAN_POINT('Ctrl Pts',(2.06600523016401,-1.,0.746345871542696));
#28997=CARTESIAN_POINT('Ctrl Pts',(2.06600523016401,1.,0.746345871542696));
#28998=CARTESIAN_POINT('Ctrl Pts',(2.06854248895575,-1.,0.74583279137781));
#28999=CARTESIAN_POINT('Ctrl Pts',(2.06854248895575,1.,0.74583279137781));
#29000=CARTESIAN_POINT('Ctrl Pts',(2.0698113262342,-1.,0.745574324794401));
#29001=CARTESIAN_POINT('Ctrl Pts',(2.0698113262342,1.,0.745574324794401));
#29002=CARTESIAN_POINT('',(1.60662857109684,1.,0.693717979106306));
#29003=CARTESIAN_POINT('Ctrl Pts',(1.60662857109684,1.,0.693717979106306));
#29004=CARTESIAN_POINT('Ctrl Pts',(1.61106790958151,1.,0.695712097881194));
#29005=CARTESIAN_POINT('Ctrl Pts',(1.61974673472612,1.,0.699605146405088));
#29006=CARTESIAN_POINT('Ctrl Pts',(1.63216541664676,1.,0.705159151988319));
#29007=CARTESIAN_POINT('Ctrl Pts',(1.64752408832016,1.,0.711993139355394));
#29008=CARTESIAN_POINT('Ctrl Pts',(1.6647288055568,1.,0.719585433804282));
#29009=CARTESIAN_POINT('Ctrl Pts',(1.67996158455503,1.,0.726235967997433));
#29010=CARTESIAN_POINT('Ctrl Pts',(1.69326921975743,1.,0.731963238697195));
#29011=CARTESIAN_POINT('Ctrl Pts',(1.70473309006121,1.,0.736799665724771));
#29012=CARTESIAN_POINT('Ctrl Pts',(1.71447789751927,1.,0.740795162032088));
#29013=CARTESIAN_POINT('Ctrl Pts',(1.7226822991693,1.,0.744021445433765));
#29014=CARTESIAN_POINT('Ctrl Pts',(1.72958533647399,1.,0.746574710096437));
#29015=CARTESIAN_POINT('Ctrl Pts',(1.73550351679848,1.,0.748582462954855));
#29016=CARTESIAN_POINT('Ctrl Pts',(1.74080458266705,1.,0.750193435979541));
#29017=CARTESIAN_POINT('Ctrl Pts',(1.74585086852298,1.,0.751555614163629));
#29018=CARTESIAN_POINT('Ctrl Pts',(1.75095139468809,1.,0.752797683531377));
#29019=CARTESIAN_POINT('Ctrl Pts',(1.75631083600175,1.,0.75400925402848));
#29020=CARTESIAN_POINT('Ctrl Pts',(1.7619781724032,1.,0.755220979975262));
#29021=CARTESIAN_POINT('Ctrl Pts',(1.76789396003141,1.,0.756421896028403));
#29022=CARTESIAN_POINT('Ctrl Pts',(1.77394167108342,1.,0.757578264077238));
#29023=CARTESIAN_POINT('Ctrl Pts',(1.77999411220912,1.,0.75865062667738));
#29024=CARTESIAN_POINT('Ctrl Pts',(1.78596964884526,1.,0.759614401109868));
#29025=CARTESIAN_POINT('Ctrl Pts',(1.79185815610802,1.,0.760469555880425));
#29026=CARTESIAN_POINT('Ctrl Pts',(1.79768986997735,1.,0.761229695230359));
#29027=CARTESIAN_POINT('Ctrl Pts',(1.80351583877334,1.,0.761915336443516));
#29028=CARTESIAN_POINT('Ctrl Pts',(1.80938551463989,1.,0.762546129464036));
#29029=CARTESIAN_POINT('Ctrl Pts',(1.81532118405566,1.,0.763132003836783));
#29030=CARTESIAN_POINT('Ctrl Pts',(1.82131873145297,1.,0.763673465462854));
#29031=CARTESIAN_POINT('Ctrl Pts',(1.8273599120008,1.,0.764165902606056));
#29032=CARTESIAN_POINT('Ctrl Pts',(1.8334207722714,1.,0.764602549687846));
#29033=CARTESIAN_POINT('Ctrl Pts',(1.83948181064823,1.,0.764978057881688));
#29034=CARTESIAN_POINT('Ctrl Pts',(1.8455369887591,1.,0.765291664861972));
#29035=CARTESIAN_POINT('Ctrl Pts',(1.85158945130054,1.,0.765545710619023));
#29036=CARTESIAN_POINT('Ctrl Pts',(1.85764741390391,1.,0.765744212909305));
#29037=CARTESIAN_POINT('Ctrl Pts',(1.86372027063314,1.,0.765891519092557));
#29038=CARTESIAN_POINT('Ctrl Pts',(1.86981398314345,1.,0.765990708546112));
#29039=CARTESIAN_POINT('Ctrl Pts',(1.87592888967886,1.,0.766042837036759));
#29040=CARTESIAN_POINT('Ctrl Pts',(1.88206215302561,1.,0.766047794851869));
#29041=CARTESIAN_POINT('Ctrl Pts',(1.88820926433409,1.,0.76600483706209));
#29042=CARTESIAN_POINT('Ctrl Pts',(1.89436577771389,1.,0.765913193856979));
#29043=CARTESIAN_POINT('Ctrl Pts',(1.90052930393599,1.,0.765772772593395));
#29044=CARTESIAN_POINT('Ctrl Pts',(1.90669961402362,1.,0.765584196937937));
#29045=CARTESIAN_POINT('Ctrl Pts',(1.91287765805174,1.,0.765348465884739));
#29046=CARTESIAN_POINT('Ctrl Pts',(1.91906491634197,1.,0.765066729667095));
#29047=CARTESIAN_POINT('Ctrl Pts',(1.92526263537041,1.,0.764740025488189));
#29048=CARTESIAN_POINT('Ctrl Pts',(1.93147105496367,1.,0.76436901067389));
#29049=CARTESIAN_POINT('Ctrl Pts',(1.93768964875867,1.,0.763954049121394));
#29050=CARTESIAN_POINT('Ctrl Pts',(1.94391746617626,1.,0.763495333538581));
#29051=CARTESIAN_POINT('Ctrl Pts',(1.95015342590025,1.,0.762992990878774));
#29052=CARTESIAN_POINT('Ctrl Pts',(1.95639665309893,1.,0.762447203806264));
#29053=CARTESIAN_POINT('Ctrl Pts',(1.96264672744229,1.,0.761858300014575));
#29054=CARTESIAN_POINT('Ctrl Pts',(1.96890351582545,1.,0.761226690483986));
#29055=CARTESIAN_POINT('Ctrl Pts',(1.97516705321521,1.,0.760552825409856));
#29056=CARTESIAN_POINT('Ctrl Pts',(1.98143741418156,1.,0.759837147452135));
#29057=CARTESIAN_POINT('Ctrl Pts',(1.98771456680806,1.,0.759080037802243));
#29058=CARTESIAN_POINT('Ctrl Pts',(1.9939983109871,1.,0.758281796766377));
#29059=CARTESIAN_POINT('Ctrl Pts',(2.00028834739072,1.,0.757442676862342));
#29060=CARTESIAN_POINT('Ctrl Pts',(2.00658431587682,1.,0.756562904646496));
#29061=CARTESIAN_POINT('Ctrl Pts',(2.01288584328149,1.,0.755642704958101));
#29062=CARTESIAN_POINT('Ctrl Pts',(2.01919259406003,1.,0.75468233072352));
#29063=CARTESIAN_POINT('Ctrl Pts',(2.02550428623587,1.,0.753682061113766));
#29064=CARTESIAN_POINT('Ctrl Pts',(2.03182068456467,1.,0.752642180488104));
#29065=CARTESIAN_POINT('Ctrl Pts',(2.03814160092173,1.,0.751562963361384));
#29066=CARTESIAN_POINT('Ctrl Pts',(2.04446689147754,1.,0.750444657874758));
#29067=CARTESIAN_POINT('Ctrl Pts',(2.05079645591606,1.,0.749287468663053));
#29068=CARTESIAN_POINT('Ctrl Pts',(2.05713023030263,1.,0.748091554181101));
#29069=CARTESIAN_POINT('Ctrl Pts',(2.06220058927162,1.,0.747103932785504));
#29070=CARTESIAN_POINT('Ctrl Pts',(2.06600523016401,1.,0.746345871542696));
#29071=CARTESIAN_POINT('Ctrl Pts',(2.06854248895575,1.,0.74583279137781));
#29072=CARTESIAN_POINT('Ctrl Pts',(2.0698113262342,1.,0.745574324794401));
#29073=CARTESIAN_POINT('',(1.60662857109684,0.,0.693717979106305));
#29074=CARTESIAN_POINT('Origin',(0.,0.,0.));
#29075=CARTESIAN_POINT('',(1.5055822144029,1.,0.892032620296856));
#29076=CARTESIAN_POINT('Origin',(0.,1.,0.));
#29077=CARTESIAN_POINT('',(1.5055822144029,0.,0.892032620296855));
#29078=CARTESIAN_POINT('Ctrl Pts',(1.81978687191668,-1.,1.23627494547115));
#29079=CARTESIAN_POINT('Ctrl Pts',(1.81978687191668,1.,1.23627494547115));
#29080=CARTESIAN_POINT('Ctrl Pts',(1.81925017193666,-1.,1.23509651170476));
#29081=CARTESIAN_POINT('Ctrl Pts',(1.81925017193666,1.,1.23509651170476));
#29082=CARTESIAN_POINT('Ctrl Pts',(1.81817389921279,-1.,1.2327422452705));
#29083=CARTESIAN_POINT('Ctrl Pts',(1.81817389921279,1.,1.2327422452705));
#29084=CARTESIAN_POINT('Ctrl Pts',(1.8165508718364,-1.,1.2292186489137));
#29085=CARTESIAN_POINT('Ctrl Pts',(1.8165508718364,1.,1.2292186489137));
#29086=CARTESIAN_POINT('Ctrl Pts',(1.81436959210434,-1.,1.2245361330495));
#29087=CARTESIAN_POINT('Ctrl Pts',(1.81436959210434,1.,1.2245361330495));
#29088=CARTESIAN_POINT('Ctrl Pts',(1.81161420806656,-1.,1.21870906103557));
#29089=CARTESIAN_POINT('Ctrl Pts',(1.81161420806656,1.,1.21870906103557));
#29090=CARTESIAN_POINT('Ctrl Pts',(1.80882996917129,-1.,1.21290815708314));
#29091=CARTESIAN_POINT('Ctrl Pts',(1.80882996917129,1.,1.21290815708314));
#29092=CARTESIAN_POINT('Ctrl Pts',(1.80601678480707,-1.,1.20713356605475));
#29093=CARTESIAN_POINT('Ctrl Pts',(1.80601678480707,1.,1.20713356605475));
#29094=CARTESIAN_POINT('Ctrl Pts',(1.80317454838603,-1.,1.20138548938974));
#29095=CARTESIAN_POINT('Ctrl Pts',(1.80317454838603,1.,1.20138548938974));
#29096=CARTESIAN_POINT('Ctrl Pts',(1.80030314369879,-1.,1.19566418930242));
#29097=CARTESIAN_POINT('Ctrl Pts',(1.80030314369879,1.,1.19566418930242));
#29098=CARTESIAN_POINT('Ctrl Pts',(1.79740245923478,-1.,1.18996997934445));
#29099=CARTESIAN_POINT('Ctrl Pts',(1.79740245923478,1.,1.18996997934445));
#29100=CARTESIAN_POINT('Ctrl Pts',(1.79447240321515,-1.,1.18430321697432));
#29101=CARTESIAN_POINT('Ctrl Pts',(1.79447240321515,1.,1.18430321697432));
#29102=CARTESIAN_POINT('Ctrl Pts',(1.79151291552689,-1.,1.17866429440809));
#29103=CARTESIAN_POINT('Ctrl Pts',(1.79151291552689,1.,1.17866429440809));
#29104=CARTESIAN_POINT('Ctrl Pts',(1.78852398877616,-1.,1.17305363177328));
#29105=CARTESIAN_POINT('Ctrl Pts',(1.78852398877616,1.,1.17305363177328));
#29106=CARTESIAN_POINT('Ctrl Pts',(1.78550566040443,-1.,1.16747166312303));
#29107=CARTESIAN_POINT('Ctrl Pts',(1.78550566040443,1.,1.16747166312303));
#29108=CARTESIAN_POINT('Ctrl Pts',(1.78245795881009,-1.,1.16191881298499));
#29109=CARTESIAN_POINT('Ctrl Pts',(1.78245795881009,1.,1.16191881298499));
#29110=CARTESIAN_POINT('Ctrl Pts',(1.77938085564275,-1.,1.15639547194698));
#29111=CARTESIAN_POINT('Ctrl Pts',(1.77938085564275,1.,1.15639547194698));
#29112=CARTESIAN_POINT('Ctrl Pts',(1.7762742255701,-1.,1.15090197841515));
#29113=CARTESIAN_POINT('Ctrl Pts',(1.7762742255701,1.,1.15090197841515));
#29114=CARTESIAN_POINT('Ctrl Pts',(1.77313777896194,-1.,1.1454385822692));
#29115=CARTESIAN_POINT('Ctrl Pts',(1.77313777896194,1.,1.1454385822692));
#29116=CARTESIAN_POINT('Ctrl Pts',(1.76997111386769,-1.,1.14000548336975));
#29117=CARTESIAN_POINT('Ctrl Pts',(1.76997111386769,1.,1.14000548336975));
#29118=CARTESIAN_POINT('Ctrl Pts',(1.76677384551862,-1.,1.1346029180462));
#29119=CARTESIAN_POINT('Ctrl Pts',(1.76677384551862,1.,1.1346029180462));
#29120=CARTESIAN_POINT('Ctrl Pts',(1.7635457196617,-1.,1.12923123555075));
#29121=CARTESIAN_POINT('Ctrl Pts',(1.7635457196617,1.,1.12923123555075));
#29122=CARTESIAN_POINT('Ctrl Pts',(1.76028671825096,-1.,1.12389096855086));
#29123=CARTESIAN_POINT('Ctrl Pts',(1.76028671825096,1.,1.12389096855086));
#29124=CARTESIAN_POINT('Ctrl Pts',(1.75699720772105,-1.,1.11858293216763));
#29125=CARTESIAN_POINT('Ctrl Pts',(1.75699720772105,1.,1.11858293216763));
#29126=CARTESIAN_POINT('Ctrl Pts',(1.7536777209463,-1.,1.11330807582551));
#29127=CARTESIAN_POINT('Ctrl Pts',(1.7536777209463,1.,1.11330807582551));
#29128=CARTESIAN_POINT('Ctrl Pts',(1.7503286607592,-1.,1.10806728183007));
#29129=CARTESIAN_POINT('Ctrl Pts',(1.7503286607592,1.,1.10806728183007));
#29130=CARTESIAN_POINT('Ctrl Pts',(1.74695004214923,-1.,1.10286118991143));
#29131=CARTESIAN_POINT('Ctrl Pts',(1.74695004214923,1.,1.10286118991143));
#29132=CARTESIAN_POINT('Ctrl Pts',(1.74354119236208,-1.,1.09768999241226));
#29133=CARTESIAN_POINT('Ctrl Pts',(1.74354119236208,1.,1.09768999241226));
#29134=CARTESIAN_POINT('Ctrl Pts',(1.74010053962247,-1.,1.09255329056493));
#29135=CARTESIAN_POINT('Ctrl Pts',(1.74010053962247,1.,1.09255329056493));
#29136=CARTESIAN_POINT('Ctrl Pts',(1.73662628326091,-1.,1.08745056285427));
#29137=CARTESIAN_POINT('Ctrl Pts',(1.73662628326091,1.,1.08745056285427));
#29138=CARTESIAN_POINT('Ctrl Pts',(1.73311705663407,-1.,1.08238162784749));
#29139=CARTESIAN_POINT('Ctrl Pts',(1.73311705663407,1.,1.08238162784749));
#29140=CARTESIAN_POINT('Ctrl Pts',(1.72957248977424,-1.,1.0773470373727));
#29141=CARTESIAN_POINT('Ctrl Pts',(1.72957248977424,1.,1.0773470373727));
#29142=CARTESIAN_POINT('Ctrl Pts',(1.72599406198488,-1.,1.07234866990252));
#29143=CARTESIAN_POINT('Ctrl Pts',(1.72599406198488,1.,1.07234866990252));
#29144=CARTESIAN_POINT('Ctrl Pts',(1.72238500928453,-1.,1.06738966975462));
#29145=CARTESIAN_POINT('Ctrl Pts',(1.72238500928453,1.,1.06738966975462));
#29146=CARTESIAN_POINT('Ctrl Pts',(1.71874858456904,-1.,1.06247324680647));
#29147=CARTESIAN_POINT('Ctrl Pts',(1.71874858456904,1.,1.06247324680647));
#29148=CARTESIAN_POINT('Ctrl Pts',(1.7150865442702,-1.,1.05760163192479));
#29149=CARTESIAN_POINT('Ctrl Pts',(1.7150865442702,1.,1.05760163192479));
#29150=CARTESIAN_POINT('Ctrl Pts',(1.71139783543989,-1.,1.05277517202855));
#29151=CARTESIAN_POINT('Ctrl Pts',(1.71139783543989,1.,1.05277517202855));
#29152=CARTESIAN_POINT('Ctrl Pts',(1.70767646263649,-1.,1.04799085404995));
#29153=CARTESIAN_POINT('Ctrl Pts',(1.70767646263649,1.,1.04799085404995));
#29154=CARTESIAN_POINT('Ctrl Pts',(1.70391338707982,-1.,1.04324363334554));
#29155=CARTESIAN_POINT('Ctrl Pts',(1.70391338707982,1.,1.04324363334554));
#29156=CARTESIAN_POINT('Ctrl Pts',(1.70010052930962,-1.,1.03852922490789));
#29157=CARTESIAN_POINT('Ctrl Pts',(1.70010052930962,1.,1.03852922490789));
#29158=CARTESIAN_POINT('Ctrl Pts',(1.69623414782771,-1.,1.03384646003588));
#29159=CARTESIAN_POINT('Ctrl Pts',(1.69623414782771,1.,1.03384646003588));
#29160=CARTESIAN_POINT('Ctrl Pts',(1.69231840863458,-1.,1.02919977579147));
#29161=CARTESIAN_POINT('Ctrl Pts',(1.69231840863458,1.,1.02919977579147));
#29162=CARTESIAN_POINT('Ctrl Pts',(1.68836910178447,-1.,1.02460180535255));
#29163=CARTESIAN_POINT('Ctrl Pts',(1.68836910178447,1.,1.02460180535255));
#29164=CARTESIAN_POINT('Ctrl Pts',(1.68440578021706,-1.,1.02006795074201));
#29165=CARTESIAN_POINT('Ctrl Pts',(1.68440578021706,1.,1.02006795074201));
#29166=CARTESIAN_POINT('Ctrl Pts',(1.68044289894798,-1.,1.01561026162773));
#29167=CARTESIAN_POINT('Ctrl Pts',(1.68044289894798,1.,1.01561026162773));
#29168=CARTESIAN_POINT('Ctrl Pts',(1.67648246776464,-1.,1.01123236493511));
#29169=CARTESIAN_POINT('Ctrl Pts',(1.67648246776464,1.,1.01123236493511));
#29170=CARTESIAN_POINT('Ctrl Pts',(1.67250335383293,-1.,1.00692206696414));
#29171=CARTESIAN_POINT('Ctrl Pts',(1.67250335383293,1.,1.00692206696414));
#29172=CARTESIAN_POINT('Ctrl Pts',(1.66846059277303,-1.,1.00265091003727));
#29173=CARTESIAN_POINT('Ctrl Pts',(1.66846059277303,1.,1.00265091003727));
#29174=CARTESIAN_POINT('Ctrl Pts',(1.66430758030376,-1.,0.998389654952758));
#29175=CARTESIAN_POINT('Ctrl Pts',(1.66430758030376,1.,0.998389654952758));
#29176=CARTESIAN_POINT('Ctrl Pts',(1.66001553809947,-1.,0.994121836661306));
#29177=CARTESIAN_POINT('Ctrl Pts',(1.66001553809947,1.,0.994121836661306));
#29178=CARTESIAN_POINT('Ctrl Pts',(1.65559044289699,-1.,0.989855627854165));
#29179=CARTESIAN_POINT('Ctrl Pts',(1.65559044289699,1.,0.989855627854165));
#29180=CARTESIAN_POINT('Ctrl Pts',(1.65110016612638,-1.,0.985642622920821));
#29181=CARTESIAN_POINT('Ctrl Pts',(1.65110016612638,1.,0.985642622920821));
#29182=CARTESIAN_POINT('Ctrl Pts',(1.64665139190656,-1.,0.981562530939489));
#29183=CARTESIAN_POINT('Ctrl Pts',(1.64665139190656,1.,0.981562530939489));
#29184=CARTESIAN_POINT('Ctrl Pts',(1.64233990826687,-1.,0.977689794119417));
#29185=CARTESIAN_POINT('Ctrl Pts',(1.64233990826687,1.,0.977689794119417));
#29186=CARTESIAN_POINT('Ctrl Pts',(1.63820952658144,-1.,0.974066058287419));
#29187=CARTESIAN_POINT('Ctrl Pts',(1.63820952658144,1.,0.974066058287419));
#29188=CARTESIAN_POINT('Ctrl Pts',(1.63420665729798,-1.,0.970669715997509));
#29189=CARTESIAN_POINT('Ctrl Pts',(1.63420665729798,1.,0.970669715997509));
#29190=CARTESIAN_POINT('Ctrl Pts',(1.63013849959461,-1.,0.967387853230345));
#29191=CARTESIAN_POINT('Ctrl Pts',(1.63013849959461,1.,0.967387853230345));
#29192=CARTESIAN_POINT('Ctrl Pts',(1.62571930670187,-1.,0.964046107040536));
#29193=CARTESIAN_POINT('Ctrl Pts',(1.62571930670187,1.,0.964046107040536));
#29194=CARTESIAN_POINT('Ctrl Pts',(1.62061638140221,-1.,0.960438326101729));
#29195=CARTESIAN_POINT('Ctrl Pts',(1.62061638140221,1.,0.960438326101729));
#29196=CARTESIAN_POINT('Ctrl Pts',(1.61449324337085,-1.,0.956354422920671));
#29197=CARTESIAN_POINT('Ctrl Pts',(1.61449324337085,1.,0.956354422920671));
#29198=CARTESIAN_POINT('Ctrl Pts',(1.60706069896936,-1.,0.951613284356035));
#29199=CARTESIAN_POINT('Ctrl Pts',(1.60706069896936,1.,0.951613284356035));
#29200=CARTESIAN_POINT('Ctrl Pts',(1.59810042043673,-1.,0.946078063315257));
#29201=CARTESIAN_POINT('Ctrl Pts',(1.59810042043673,1.,0.946078063315257));
#29202=CARTESIAN_POINT('Ctrl Pts',(1.58744937487176,-1.,0.939646377893399));
#29203=CARTESIAN_POINT('Ctrl Pts',(1.58744937487176,1.,0.939646377893399));
#29204=CARTESIAN_POINT('Ctrl Pts',(1.57499388382243,-1.,0.932246680108685));
#29205=CARTESIAN_POINT('Ctrl Pts',(1.57499388382243,1.,0.932246680108685));
#29206=CARTESIAN_POINT('Ctrl Pts',(1.56065988578893,-1.,0.923832188944341));
#29207=CARTESIAN_POINT('Ctrl Pts',(1.56065988578893,1.,0.923832188944341));
#29208=CARTESIAN_POINT('Ctrl Pts',(1.54440491149498,-1.,0.914375919026456));
#29209=CARTESIAN_POINT('Ctrl Pts',(1.54440491149498,1.,0.914375919026456));
#29210=CARTESIAN_POINT('Ctrl Pts',(1.52984849887993,-1.,0.905967409625651));
#29211=CARTESIAN_POINT('Ctrl Pts',(1.52984849887993,1.,0.905967409625651));
#29212=CARTESIAN_POINT('Ctrl Pts',(1.51805569590094,-1.,0.899185047483511));
#29213=CARTESIAN_POINT('Ctrl Pts',(1.51805569590094,1.,0.899185047483511));
#29214=CARTESIAN_POINT('Ctrl Pts',(1.50980486806688,-1.,0.894452006964544));
#29215=CARTESIAN_POINT('Ctrl Pts',(1.50980486806688,1.,0.894452006964544));
#29216=CARTESIAN_POINT('Ctrl Pts',(1.5055822144029,-1.,0.892032620296856));
#29217=CARTESIAN_POINT('Ctrl Pts',(1.5055822144029,1.,0.892032620296856));
#29218=CARTESIAN_POINT('',(1.81978687191668,1.,1.23627494547115));
#29219=CARTESIAN_POINT('Ctrl Pts',(1.81978687191668,1.,1.23627494547115));
#29220=CARTESIAN_POINT('Ctrl Pts',(1.81925017193666,1.,1.23509651170476));
#29221=CARTESIAN_POINT('Ctrl Pts',(1.81817389921279,1.,1.2327422452705));
#29222=CARTESIAN_POINT('Ctrl Pts',(1.8165508718364,1.,1.2292186489137));
#29223=CARTESIAN_POINT('Ctrl Pts',(1.81436959210434,1.,1.2245361330495));
#29224=CARTESIAN_POINT('Ctrl Pts',(1.81161420806656,1.,1.21870906103557));
#29225=CARTESIAN_POINT('Ctrl Pts',(1.80882996917129,1.,1.21290815708314));
#29226=CARTESIAN_POINT('Ctrl Pts',(1.80601678480707,1.,1.20713356605475));
#29227=CARTESIAN_POINT('Ctrl Pts',(1.80317454838603,1.,1.20138548938974));
#29228=CARTESIAN_POINT('Ctrl Pts',(1.80030314369879,1.,1.19566418930242));
#29229=CARTESIAN_POINT('Ctrl Pts',(1.79740245923478,1.,1.18996997934445));
#29230=CARTESIAN_POINT('Ctrl Pts',(1.79447240321515,1.,1.18430321697432));
#29231=CARTESIAN_POINT('Ctrl Pts',(1.79151291552689,1.,1.17866429440809));
#29232=CARTESIAN_POINT('Ctrl Pts',(1.78852398877616,1.,1.17305363177328));
#29233=CARTESIAN_POINT('Ctrl Pts',(1.78550566040443,1.,1.16747166312303));
#29234=CARTESIAN_POINT('Ctrl Pts',(1.78245795881009,1.,1.16191881298499));
#29235=CARTESIAN_POINT('Ctrl Pts',(1.77938085564275,1.,1.15639547194698));
#29236=CARTESIAN_POINT('Ctrl Pts',(1.7762742255701,1.,1.15090197841515));
#29237=CARTESIAN_POINT('Ctrl Pts',(1.77313777896194,1.,1.1454385822692));
#29238=CARTESIAN_POINT('Ctrl Pts',(1.76997111386769,1.,1.14000548336975));
#29239=CARTESIAN_POINT('Ctrl Pts',(1.76677384551862,1.,1.1346029180462));
#29240=CARTESIAN_POINT('Ctrl Pts',(1.7635457196617,1.,1.12923123555075));
#29241=CARTESIAN_POINT('Ctrl Pts',(1.76028671825096,1.,1.12389096855086));
#29242=CARTESIAN_POINT('Ctrl Pts',(1.75699720772105,1.,1.11858293216763));
#29243=CARTESIAN_POINT('Ctrl Pts',(1.7536777209463,1.,1.11330807582551));
#29244=CARTESIAN_POINT('Ctrl Pts',(1.7503286607592,1.,1.10806728183007));
#29245=CARTESIAN_POINT('Ctrl Pts',(1.74695004214923,1.,1.10286118991143));
#29246=CARTESIAN_POINT('Ctrl Pts',(1.74354119236208,1.,1.09768999241226));
#29247=CARTESIAN_POINT('Ctrl Pts',(1.74010053962247,1.,1.09255329056493));
#29248=CARTESIAN_POINT('Ctrl Pts',(1.73662628326091,1.,1.08745056285427));
#29249=CARTESIAN_POINT('Ctrl Pts',(1.73311705663407,1.,1.08238162784749));
#29250=CARTESIAN_POINT('Ctrl Pts',(1.72957248977424,1.,1.0773470373727));
#29251=CARTESIAN_POINT('Ctrl Pts',(1.72599406198488,1.,1.07234866990252));
#29252=CARTESIAN_POINT('Ctrl Pts',(1.72238500928453,1.,1.06738966975462));
#29253=CARTESIAN_POINT('Ctrl Pts',(1.71874858456904,1.,1.06247324680647));
#29254=CARTESIAN_POINT('Ctrl Pts',(1.7150865442702,1.,1.05760163192479));
#29255=CARTESIAN_POINT('Ctrl Pts',(1.71139783543989,1.,1.05277517202855));
#29256=CARTESIAN_POINT('Ctrl Pts',(1.70767646263649,1.,1.04799085404995));
#29257=CARTESIAN_POINT('Ctrl Pts',(1.70391338707982,1.,1.04324363334554));
#29258=CARTESIAN_POINT('Ctrl Pts',(1.70010052930962,1.,1.03852922490789));
#29259=CARTESIAN_POINT('Ctrl Pts',(1.69623414782771,1.,1.03384646003588));
#29260=CARTESIAN_POINT('Ctrl Pts',(1.69231840863458,1.,1.02919977579147));
#29261=CARTESIAN_POINT('Ctrl Pts',(1.68836910178447,1.,1.02460180535255));
#29262=CARTESIAN_POINT('Ctrl Pts',(1.68440578021706,1.,1.02006795074201));
#29263=CARTESIAN_POINT('Ctrl Pts',(1.68044289894798,1.,1.01561026162773));
#29264=CARTESIAN_POINT('Ctrl Pts',(1.67648246776464,1.,1.01123236493511));
#29265=CARTESIAN_POINT('Ctrl Pts',(1.67250335383293,1.,1.00692206696414));
#29266=CARTESIAN_POINT('Ctrl Pts',(1.66846059277303,1.,1.00265091003727));
#29267=CARTESIAN_POINT('Ctrl Pts',(1.66430758030376,1.,0.998389654952758));
#29268=CARTESIAN_POINT('Ctrl Pts',(1.66001553809947,1.,0.994121836661306));
#29269=CARTESIAN_POINT('Ctrl Pts',(1.65559044289699,1.,0.989855627854165));
#29270=CARTESIAN_POINT('Ctrl Pts',(1.65110016612638,1.,0.985642622920821));
#29271=CARTESIAN_POINT('Ctrl Pts',(1.64665139190656,1.,0.981562530939489));
#29272=CARTESIAN_POINT('Ctrl Pts',(1.64233990826687,1.,0.977689794119417));
#29273=CARTESIAN_POINT('Ctrl Pts',(1.63820952658144,1.,0.974066058287419));
#29274=CARTESIAN_POINT('Ctrl Pts',(1.63420665729798,1.,0.970669715997509));
#29275=CARTESIAN_POINT('Ctrl Pts',(1.63013849959461,1.,0.967387853230345));
#29276=CARTESIAN_POINT('Ctrl Pts',(1.62571930670187,1.,0.964046107040536));
#29277=CARTESIAN_POINT('Ctrl Pts',(1.62061638140221,1.,0.960438326101729));
#29278=CARTESIAN_POINT('Ctrl Pts',(1.61449324337085,1.,0.956354422920671));
#29279=CARTESIAN_POINT('Ctrl Pts',(1.60706069896936,1.,0.951613284356035));
#29280=CARTESIAN_POINT('Ctrl Pts',(1.59810042043673,1.,0.946078063315257));
#29281=CARTESIAN_POINT('Ctrl Pts',(1.58744937487176,1.,0.939646377893399));
#29282=CARTESIAN_POINT('Ctrl Pts',(1.57499388382243,1.,0.932246680108685));
#29283=CARTESIAN_POINT('Ctrl Pts',(1.56065988578893,1.,0.923832188944341));
#29284=CARTESIAN_POINT('Ctrl Pts',(1.54440491149498,1.,0.914375919026456));
#29285=CARTESIAN_POINT('Ctrl Pts',(1.52984849887993,1.,0.905967409625651));
#29286=CARTESIAN_POINT('Ctrl Pts',(1.51805569590094,1.,0.899185047483511));
#29287=CARTESIAN_POINT('Ctrl Pts',(1.50980486806688,1.,0.894452006964544));
#29288=CARTESIAN_POINT('Ctrl Pts',(1.5055822144029,1.,0.892032620296856));
#29289=CARTESIAN_POINT('',(1.81978687191668,0.,1.23627494547115));
#29290=CARTESIAN_POINT('Origin',(1.73811241238545,0.,1.34869019493419));
#29291=CARTESIAN_POINT('',(1.73811241238545,1.,1.34869019493419));
#29292=CARTESIAN_POINT('',(1.81978687191668,1.,1.23627494547115));
#29293=CARTESIAN_POINT('',(1.73811241238545,0.,1.34869019493419));
#29294=CARTESIAN_POINT('Ctrl Pts',(1.31362392696032,-1.,1.15624053661742));
#29295=CARTESIAN_POINT('Ctrl Pts',(1.31362392696032,1.,1.15624053661742));
#29296=CARTESIAN_POINT('Ctrl Pts',(1.31722977216397,-1.,1.15950888730809));
#29297=CARTESIAN_POINT('Ctrl Pts',(1.31722977216397,1.,1.15950888730809));
#29298=CARTESIAN_POINT('Ctrl Pts',(1.32428080721772,-1.,1.16589330093588));
#29299=CARTESIAN_POINT('Ctrl Pts',(1.32428080721772,1.,1.16589330093588));
#29300=CARTESIAN_POINT('Ctrl Pts',(1.33437539347008,-1.,1.17501305789857));
#29301=CARTESIAN_POINT('Ctrl Pts',(1.33437539347008,1.,1.17501305789857));
#29302=CARTESIAN_POINT('Ctrl Pts',(1.34687054001093,-1.,1.18625865667441));
#29303=CARTESIAN_POINT('Ctrl Pts',(1.34687054001093,1.,1.18625865667441));
#29304=CARTESIAN_POINT('Ctrl Pts',(1.36088705043885,-1.,1.1987959077932));
#29305=CARTESIAN_POINT('Ctrl Pts',(1.36088705043885,1.,1.1987959077932));
#29306=CARTESIAN_POINT('Ctrl Pts',(1.37331915607905,-1.,1.20982812925645));
#29307=CARTESIAN_POINT('Ctrl Pts',(1.37331915607905,1.,1.20982812925645));
#29308=CARTESIAN_POINT('Ctrl Pts',(1.38420564527715,-1.,1.21938737280852));
#29309=CARTESIAN_POINT('Ctrl Pts',(1.38420564527715,1.,1.21938737280852));
#29310=CARTESIAN_POINT('Ctrl Pts',(1.39361389568796,-1.,1.22752961899387));
#29311=CARTESIAN_POINT('Ctrl Pts',(1.39361389568796,1.,1.22752961899387));
#29312=CARTESIAN_POINT('Ctrl Pts',(1.40164708206106,-1.,1.23434087290423));
#29313=CARTESIAN_POINT('Ctrl Pts',(1.40164708206106,1.,1.23434087290423));
#29314=CARTESIAN_POINT('Ctrl Pts',(1.40845295531283,-1.,1.23994455029534));
#29315=CARTESIAN_POINT('Ctrl Pts',(1.40845295531283,1.,1.23994455029534));
#29316=CARTESIAN_POINT('Ctrl Pts',(1.41422913175179,-1.,1.24450600513056));
#29317=CARTESIAN_POINT('Ctrl Pts',(1.41422913175179,1.,1.24450600513056));
#29318=CARTESIAN_POINT('Ctrl Pts',(1.41923722596025,-1.,1.24824430986571));
#29319=CARTESIAN_POINT('Ctrl Pts',(1.41923722596025,1.,1.24824430986571));
#29320=CARTESIAN_POINT('Ctrl Pts',(1.42378102115575,-1.,1.2514145557001));
#29321=CARTESIAN_POINT('Ctrl Pts',(1.42378102115575,1.,1.2514145557001));
#29322=CARTESIAN_POINT('Ctrl Pts',(1.42815938799387,-1.,1.25426945222639));
#29323=CARTESIAN_POINT('Ctrl Pts',(1.42815938799387,1.,1.25426945222639));
#29324=CARTESIAN_POINT('Ctrl Pts',(1.43262645609691,-1.,1.25702687965755));
#29325=CARTESIAN_POINT('Ctrl Pts',(1.43262645609691,1.,1.25702687965755));
#29326=CARTESIAN_POINT('Ctrl Pts',(1.43734919180847,-1.,1.25983531012005));
#29327=CARTESIAN_POINT('Ctrl Pts',(1.43734919180847,1.,1.25983531012005));
#29328=CARTESIAN_POINT('Ctrl Pts',(1.44236470511303,-1.,1.26273903323859));
#29329=CARTESIAN_POINT('Ctrl Pts',(1.44236470511303,1.,1.26273903323859));
#29330=CARTESIAN_POINT('Ctrl Pts',(1.44761985001662,-1.,1.26570925118868));
#29331=CARTESIAN_POINT('Ctrl Pts',(1.44761985001662,1.,1.26570925118868));
#29332=CARTESIAN_POINT('Ctrl Pts',(1.45301422764247,-1.,1.2686778680489));
#29333=CARTESIAN_POINT('Ctrl Pts',(1.45301422764247,1.,1.2686778680489));
#29334=CARTESIAN_POINT('Ctrl Pts',(1.45843906294697,-1.,1.27156805265289));
#29335=CARTESIAN_POINT('Ctrl Pts',(1.45843906294697,1.,1.27156805265289));
#29336=CARTESIAN_POINT('Ctrl Pts',(1.46382431332476,-1.,1.27433119897822));
#29337=CARTESIAN_POINT('Ctrl Pts',(1.46382431332476,1.,1.27433119897822));
#29338=CARTESIAN_POINT('Ctrl Pts',(1.46916035917133,-1.,1.2769641483109));
#29339=CARTESIAN_POINT('Ctrl Pts',(1.46916035917133,1.,1.2769641483109));
#29340=CARTESIAN_POINT('Ctrl Pts',(1.4744717526707,-1.,1.2794891824849));
#29341=CARTESIAN_POINT('Ctrl Pts',(1.4744717526707,1.,1.2794891824849));
#29342=CARTESIAN_POINT('Ctrl Pts',(1.47980070347095,-1.,1.28194158939517));
#29343=CARTESIAN_POINT('Ctrl Pts',(1.47980070347095,1.,1.28194158939517));
#29344=CARTESIAN_POINT('Ctrl Pts',(1.4851881711891,-1.,1.28435533880201));
#29345=CARTESIAN_POINT('Ctrl Pts',(1.4851881711891,1.,1.28435533880201));
#29346=CARTESIAN_POINT('Ctrl Pts',(1.4906522831278,-1.,1.2867467611644));
#29347=CARTESIAN_POINT('Ctrl Pts',(1.4906522831278,1.,1.2867467611644));
#29348=CARTESIAN_POINT('Ctrl Pts',(1.49618896881754,-1.,1.28911506584254));
#29349=CARTESIAN_POINT('Ctrl Pts',(1.49618896881754,1.,1.28911506584254));
#29350=CARTESIAN_POINT('Ctrl Pts',(1.50178230149776,-1.,1.29145022885181));
#29351=CARTESIAN_POINT('Ctrl Pts',(1.50178230149776,1.,1.29145022885181));
#29352=CARTESIAN_POINT('Ctrl Pts',(1.50741159078365,-1.,1.29373841372842));
#29353=CARTESIAN_POINT('Ctrl Pts',(1.50741159078365,1.,1.29373841372842));
#29354=CARTESIAN_POINT('Ctrl Pts',(1.51305994241402,-1.,1.29596850710509));
#29355=CARTESIAN_POINT('Ctrl Pts',(1.51305994241402,1.,1.29596850710509));
#29356=CARTESIAN_POINT('Ctrl Pts',(1.51872184912724,-1.,1.29813791800747));
#29357=CARTESIAN_POINT('Ctrl Pts',(1.51872184912724,1.,1.29813791800747));
#29358=CARTESIAN_POINT('Ctrl Pts',(1.52439957861062,-1.,1.30024984366328));
#29359=CARTESIAN_POINT('Ctrl Pts',(1.52439957861062,1.,1.30024984366328));
#29360=CARTESIAN_POINT('Ctrl Pts',(1.53009970283891,-1.,1.30231064395568));
#29361=CARTESIAN_POINT('Ctrl Pts',(1.53009970283891,1.,1.30231064395568));
#29362=CARTESIAN_POINT('Ctrl Pts',(1.53582981268977,-1.,1.30432735639489));
#29363=CARTESIAN_POINT('Ctrl Pts',(1.53582981268977,1.,1.30432735639489));
#29364=CARTESIAN_POINT('Ctrl Pts',(1.54159462645432,-1.,1.30630475189556));
#29365=CARTESIAN_POINT('Ctrl Pts',(1.54159462645432,1.,1.30630475189556));
#29366=CARTESIAN_POINT('Ctrl Pts',(1.54739413957185,-1.,1.30824393907473));
#29367=CARTESIAN_POINT('Ctrl Pts',(1.54739413957185,1.,1.30824393907473));
#29368=CARTESIAN_POINT('Ctrl Pts',(1.55322568759481,-1.,1.31014393684222));
#29369=CARTESIAN_POINT('Ctrl Pts',(1.55322568759481,1.,1.31014393684222));
#29370=CARTESIAN_POINT('Ctrl Pts',(1.55908521254821,-1.,1.31200264341696));
#29371=CARTESIAN_POINT('Ctrl Pts',(1.55908521254821,1.,1.31200264341696));
#29372=CARTESIAN_POINT('Ctrl Pts',(1.56496872402353,-1.,1.31381795281002));
#29373=CARTESIAN_POINT('Ctrl Pts',(1.56496872402353,1.,1.31381795281002));
#29374=CARTESIAN_POINT('Ctrl Pts',(1.57087397835723,-1.,1.31558903860016));
#29375=CARTESIAN_POINT('Ctrl Pts',(1.57087397835723,1.,1.31558903860016));
#29376=CARTESIAN_POINT('Ctrl Pts',(1.5768005650559,-1.,1.31731642317187));
#29377=CARTESIAN_POINT('Ctrl Pts',(1.5768005650559,1.,1.31731642317187));
#29378=CARTESIAN_POINT('Ctrl Pts',(1.58274907898834,-1.,1.31900135021432));
#29379=CARTESIAN_POINT('Ctrl Pts',(1.58274907898834,1.,1.31900135021432));
#29380=CARTESIAN_POINT('Ctrl Pts',(1.58872057258245,-1.,1.32064537110892));
#29381=CARTESIAN_POINT('Ctrl Pts',(1.58872057258245,1.,1.32064537110892));
#29382=CARTESIAN_POINT('Ctrl Pts',(1.59471591079403,-1.,1.32224985747682));
#29383=CARTESIAN_POINT('Ctrl Pts',(1.59471591079403,1.,1.32224985747682));
#29384=CARTESIAN_POINT('Ctrl Pts',(1.60073511858687,-1.,1.32381550858256));
#29385=CARTESIAN_POINT('Ctrl Pts',(1.60073511858687,1.,1.32381550858256));
#29386=CARTESIAN_POINT('Ctrl Pts',(1.60677758290954,-1.,1.32534250785782));
#29387=CARTESIAN_POINT('Ctrl Pts',(1.60677758290954,1.,1.32534250785782));
#29388=CARTESIAN_POINT('Ctrl Pts',(1.6128423401575,-1.,1.32683074483356));
#29389=CARTESIAN_POINT('Ctrl Pts',(1.6128423401575,1.,1.32683074483356));
#29390=CARTESIAN_POINT('Ctrl Pts',(1.61892832270724,-1.,1.32828000610449));
#29391=CARTESIAN_POINT('Ctrl Pts',(1.61892832270724,1.,1.32828000610449));
#29392=CARTESIAN_POINT('Ctrl Pts',(1.62503464209797,-1.,1.3296901950568));
#29393=CARTESIAN_POINT('Ctrl Pts',(1.62503464209797,1.,1.3296901950568));
#29394=CARTESIAN_POINT('Ctrl Pts',(1.63116079730923,-1.,1.33106149345645));
#29395=CARTESIAN_POINT('Ctrl Pts',(1.63116079730923,1.,1.33106149345645));
#29396=CARTESIAN_POINT('Ctrl Pts',(1.63730653475089,-1.,1.33239425103724));
#29397=CARTESIAN_POINT('Ctrl Pts',(1.63730653475089,1.,1.33239425103724));
#29398=CARTESIAN_POINT('Ctrl Pts',(1.6434717485603,-1.,1.33368890676572));
#29399=CARTESIAN_POINT('Ctrl Pts',(1.6434717485603,1.,1.33368890676572));
#29400=CARTESIAN_POINT('Ctrl Pts',(1.6496563728683,-1.,1.33494590467993));
#29401=CARTESIAN_POINT('Ctrl Pts',(1.6496563728683,1.,1.33494590467993));
#29402=CARTESIAN_POINT('Ctrl Pts',(1.65586025952593,-1.,1.33616559745172));
#29403=CARTESIAN_POINT('Ctrl Pts',(1.65586025952593,1.,1.33616559745172));
#29404=CARTESIAN_POINT('Ctrl Pts',(1.66208312541983,-1.,1.33734820885262));
#29405=CARTESIAN_POINT('Ctrl Pts',(1.66208312541983,1.,1.33734820885262));
#29406=CARTESIAN_POINT('Ctrl Pts',(1.66832460783989,-1.,1.33849388654388));
#29407=CARTESIAN_POINT('Ctrl Pts',(1.66832460783989,1.,1.33849388654388));
#29408=CARTESIAN_POINT('Ctrl Pts',(1.67458429426086,-1.,1.3396027347034));
#29409=CARTESIAN_POINT('Ctrl Pts',(1.67458429426086,1.,1.3396027347034));
#29410=CARTESIAN_POINT('Ctrl Pts',(1.68086176030362,-1.,1.34067485185203));
#29411=CARTESIAN_POINT('Ctrl Pts',(1.68086176030362,1.,1.34067485185203));
#29412=CARTESIAN_POINT('Ctrl Pts',(1.68715660868764,-1.,1.341710374848));
#29413=CARTESIAN_POINT('Ctrl Pts',(1.68715660868764,1.,1.341710374848));
#29414=CARTESIAN_POINT('Ctrl Pts',(1.6934684849687,-1.,1.34270948206319));
#29415=CARTESIAN_POINT('Ctrl Pts',(1.6934684849687,1.,1.34270948206319));
#29416=CARTESIAN_POINT('Ctrl Pts',(1.69979707754427,-1.,1.34367237124483));
#29417=CARTESIAN_POINT('Ctrl Pts',(1.69979707754427,1.,1.34367237124483));
#29418=CARTESIAN_POINT('Ctrl Pts',(1.70614212266738,-1.,1.34459924533831));
#29419=CARTESIAN_POINT('Ctrl Pts',(1.70614212266738,1.,1.34459924533831));
#29420=CARTESIAN_POINT('Ctrl Pts',(1.71250340686822,-1.,1.34549029589416));
#29421=CARTESIAN_POINT('Ctrl Pts',(1.71250340686822,1.,1.34549029589416));
#29422=CARTESIAN_POINT('Ctrl Pts',(1.7188807715049,-1.,1.34634568653227));
#29423=CARTESIAN_POINT('Ctrl Pts',(1.7188807715049,1.,1.34634568653227));
#29424=CARTESIAN_POINT('Ctrl Pts',(1.72527410680674,-1.,1.34716554819527));
#29425=CARTESIAN_POINT('Ctrl Pts',(1.72527410680674,1.,1.34716554819527));
#29426=CARTESIAN_POINT('Ctrl Pts',(1.7304014965394,-1.,1.34779309152035));
#29427=CARTESIAN_POINT('Ctrl Pts',(1.7304014965394,1.,1.34779309152035));
#29428=CARTESIAN_POINT('Ctrl Pts',(1.73425417885907,-1.,1.34824783112887));
#29429=CARTESIAN_POINT('Ctrl Pts',(1.73425417885907,1.,1.34824783112887));
#29430=CARTESIAN_POINT('Ctrl Pts',(1.73682580585691,-1.,1.34854391898045));
#29431=CARTESIAN_POINT('Ctrl Pts',(1.73682580585691,1.,1.34854391898045));
#29432=CARTESIAN_POINT('Ctrl Pts',(1.73811241238545,-1.,1.34869019493419));
#29433=CARTESIAN_POINT('Ctrl Pts',(1.73811241238545,1.,1.34869019493419));
#29434=CARTESIAN_POINT('',(1.31362392696032,1.,1.15624053661742));
#29435=CARTESIAN_POINT('Ctrl Pts',(1.31362392696032,1.,1.15624053661742));
#29436=CARTESIAN_POINT('Ctrl Pts',(1.31722977216397,1.,1.15950888730809));
#29437=CARTESIAN_POINT('Ctrl Pts',(1.32428080721772,1.,1.16589330093588));
#29438=CARTESIAN_POINT('Ctrl Pts',(1.33437539347008,1.,1.17501305789857));
#29439=CARTESIAN_POINT('Ctrl Pts',(1.34687054001093,1.,1.18625865667441));
#29440=CARTESIAN_POINT('Ctrl Pts',(1.36088705043885,1.,1.1987959077932));
#29441=CARTESIAN_POINT('Ctrl Pts',(1.37331915607905,1.,1.20982812925645));
#29442=CARTESIAN_POINT('Ctrl Pts',(1.38420564527715,1.,1.21938737280852));
#29443=CARTESIAN_POINT('Ctrl Pts',(1.39361389568796,1.,1.22752961899387));
#29444=CARTESIAN_POINT('Ctrl Pts',(1.40164708206106,1.,1.23434087290423));
#29445=CARTESIAN_POINT('Ctrl Pts',(1.40845295531283,1.,1.23994455029534));
#29446=CARTESIAN_POINT('Ctrl Pts',(1.41422913175179,1.,1.24450600513056));
#29447=CARTESIAN_POINT('Ctrl Pts',(1.41923722596025,1.,1.24824430986571));
#29448=CARTESIAN_POINT('Ctrl Pts',(1.42378102115575,1.,1.2514145557001));
#29449=CARTESIAN_POINT('Ctrl Pts',(1.42815938799387,1.,1.25426945222639));
#29450=CARTESIAN_POINT('Ctrl Pts',(1.43262645609691,1.,1.25702687965755));
#29451=CARTESIAN_POINT('Ctrl Pts',(1.43734919180847,1.,1.25983531012005));
#29452=CARTESIAN_POINT('Ctrl Pts',(1.44236470511303,1.,1.26273903323859));
#29453=CARTESIAN_POINT('Ctrl Pts',(1.44761985001662,1.,1.26570925118868));
#29454=CARTESIAN_POINT('Ctrl Pts',(1.45301422764247,1.,1.2686778680489));
#29455=CARTESIAN_POINT('Ctrl Pts',(1.45843906294697,1.,1.27156805265289));
#29456=CARTESIAN_POINT('Ctrl Pts',(1.46382431332476,1.,1.27433119897822));
#29457=CARTESIAN_POINT('Ctrl Pts',(1.46916035917133,1.,1.2769641483109));
#29458=CARTESIAN_POINT('Ctrl Pts',(1.4744717526707,1.,1.2794891824849));
#29459=CARTESIAN_POINT('Ctrl Pts',(1.47980070347095,1.,1.28194158939517));
#29460=CARTESIAN_POINT('Ctrl Pts',(1.4851881711891,1.,1.28435533880201));
#29461=CARTESIAN_POINT('Ctrl Pts',(1.4906522831278,1.,1.2867467611644));
#29462=CARTESIAN_POINT('Ctrl Pts',(1.49618896881754,1.,1.28911506584254));
#29463=CARTESIAN_POINT('Ctrl Pts',(1.50178230149776,1.,1.29145022885181));
#29464=CARTESIAN_POINT('Ctrl Pts',(1.50741159078365,1.,1.29373841372842));
#29465=CARTESIAN_POINT('Ctrl Pts',(1.51305994241402,1.,1.29596850710509));
#29466=CARTESIAN_POINT('Ctrl Pts',(1.51872184912724,1.,1.29813791800747));
#29467=CARTESIAN_POINT('Ctrl Pts',(1.52439957861062,1.,1.30024984366328));
#29468=CARTESIAN_POINT('Ctrl Pts',(1.53009970283891,1.,1.30231064395568));
#29469=CARTESIAN_POINT('Ctrl Pts',(1.53582981268977,1.,1.30432735639489));
#29470=CARTESIAN_POINT('Ctrl Pts',(1.54159462645432,1.,1.30630475189556));
#29471=CARTESIAN_POINT('Ctrl Pts',(1.54739413957185,1.,1.30824393907473));
#29472=CARTESIAN_POINT('Ctrl Pts',(1.55322568759481,1.,1.31014393684222));
#29473=CARTESIAN_POINT('Ctrl Pts',(1.55908521254821,1.,1.31200264341696));
#29474=CARTESIAN_POINT('Ctrl Pts',(1.56496872402353,1.,1.31381795281002));
#29475=CARTESIAN_POINT('Ctrl Pts',(1.57087397835723,1.,1.31558903860016));
#29476=CARTESIAN_POINT('Ctrl Pts',(1.5768005650559,1.,1.31731642317187));
#29477=CARTESIAN_POINT('Ctrl Pts',(1.58274907898834,1.,1.31900135021432));
#29478=CARTESIAN_POINT('Ctrl Pts',(1.58872057258245,1.,1.32064537110892));
#29479=CARTESIAN_POINT('Ctrl Pts',(1.59471591079403,1.,1.32224985747682));
#29480=CARTESIAN_POINT('Ctrl Pts',(1.60073511858687,1.,1.32381550858256));
#29481=CARTESIAN_POINT('Ctrl Pts',(1.60677758290954,1.,1.32534250785782));
#29482=CARTESIAN_POINT('Ctrl Pts',(1.6128423401575,1.,1.32683074483356));
#29483=CARTESIAN_POINT('Ctrl Pts',(1.61892832270724,1.,1.32828000610449));
#29484=CARTESIAN_POINT('Ctrl Pts',(1.62503464209797,1.,1.3296901950568));
#29485=CARTESIAN_POINT('Ctrl Pts',(1.63116079730923,1.,1.33106149345645));
#29486=CARTESIAN_POINT('Ctrl Pts',(1.63730653475089,1.,1.33239425103724));
#29487=CARTESIAN_POINT('Ctrl Pts',(1.6434717485603,1.,1.33368890676572));
#29488=CARTESIAN_POINT('Ctrl Pts',(1.6496563728683,1.,1.33494590467993));
#29489=CARTESIAN_POINT('Ctrl Pts',(1.65586025952593,1.,1.33616559745172));
#29490=CARTESIAN_POINT('Ctrl Pts',(1.66208312541983,1.,1.33734820885262));
#29491=CARTESIAN_POINT('Ctrl Pts',(1.66832460783989,1.,1.33849388654388));
#29492=CARTESIAN_POINT('Ctrl Pts',(1.67458429426086,1.,1.3396027347034));
#29493=CARTESIAN_POINT('Ctrl Pts',(1.68086176030362,1.,1.34067485185203));
#29494=CARTESIAN_POINT('Ctrl Pts',(1.68715660868764,1.,1.341710374848));
#29495=CARTESIAN_POINT('Ctrl Pts',(1.6934684849687,1.,1.34270948206319));
#29496=CARTESIAN_POINT('Ctrl Pts',(1.69979707754427,1.,1.34367237124483));
#29497=CARTESIAN_POINT('Ctrl Pts',(1.70614212266738,1.,1.34459924533831));
#29498=CARTESIAN_POINT('Ctrl Pts',(1.71250340686822,1.,1.34549029589416));
#29499=CARTESIAN_POINT('Ctrl Pts',(1.7188807715049,1.,1.34634568653227));
#29500=CARTESIAN_POINT('Ctrl Pts',(1.72527410680674,1.,1.34716554819527));
#29501=CARTESIAN_POINT('Ctrl Pts',(1.7304014965394,1.,1.34779309152035));
#29502=CARTESIAN_POINT('Ctrl Pts',(1.73425417885907,1.,1.34824783112887));
#29503=CARTESIAN_POINT('Ctrl Pts',(1.73682580585691,1.,1.34854391898045));
#29504=CARTESIAN_POINT('Ctrl Pts',(1.73811241238545,1.,1.34869019493419));
#29505=CARTESIAN_POINT('',(1.31362392696032,0.,1.15624053661742));
#29506=CARTESIAN_POINT('Origin',(0.,0.,0.));
#29507=CARTESIAN_POINT('',(1.15624053661742,1.,1.31362392696033));
#29508=CARTESIAN_POINT('Origin',(0.,1.,0.));
#29509=CARTESIAN_POINT('',(1.15624053661742,0.,1.31362392696032));
#29510=CARTESIAN_POINT('Ctrl Pts',(1.34869019493419,-1.,1.73811241238545));
#29511=CARTESIAN_POINT('Ctrl Pts',(1.34869019493419,1.,1.73811241238545));
#29512=CARTESIAN_POINT('Ctrl Pts',(1.34854391898145,-1.,1.73682580585819));
#29513=CARTESIAN_POINT('Ctrl Pts',(1.34854391898145,1.,1.73682580585819));
#29514=CARTESIAN_POINT('Ctrl Pts',(1.34824783113158,-1.,1.73425417886255));
#29515=CARTESIAN_POINT('Ctrl Pts',(1.34824783113158,1.,1.73425417886255));
#29516=CARTESIAN_POINT('Ctrl Pts',(1.3477930915247,-1.,1.73040149654497));
#29517=CARTESIAN_POINT('Ctrl Pts',(1.3477930915247,1.,1.73040149654497));
#29518=CARTESIAN_POINT('Ctrl Pts',(1.34716554820013,-1.,1.72527410681298));
#29519=CARTESIAN_POINT('Ctrl Pts',(1.34716554820013,1.,1.72527410681298));
#29520=CARTESIAN_POINT('Ctrl Pts',(1.34634568653586,-1.,1.7188807715095));
#29521=CARTESIAN_POINT('Ctrl Pts',(1.34634568653586,1.,1.7188807715095));
#29522=CARTESIAN_POINT('Ctrl Pts',(1.34549029589563,-1.,1.71250340687011));
#29523=CARTESIAN_POINT('Ctrl Pts',(1.34549029589563,1.,1.71250340687011));
#29524=CARTESIAN_POINT('Ctrl Pts',(1.34459924533783,-1.,1.70614212266676));
#29525=CARTESIAN_POINT('Ctrl Pts',(1.34459924533783,1.,1.70614212266676));
#29526=CARTESIAN_POINT('Ctrl Pts',(1.34367237124322,-1.,1.69979707754221));
#29527=CARTESIAN_POINT('Ctrl Pts',(1.34367237124322,1.,1.69979707754221));
#29528=CARTESIAN_POINT('Ctrl Pts',(1.34270948206139,-1.,1.6934684849664));
#29529=CARTESIAN_POINT('Ctrl Pts',(1.34270948206139,1.,1.6934684849664));
#29530=CARTESIAN_POINT('Ctrl Pts',(1.34171037484673,-1.,1.68715660868602));
#29531=CARTESIAN_POINT('Ctrl Pts',(1.34171037484673,1.,1.68715660868602));
#29532=CARTESIAN_POINT('Ctrl Pts',(1.3406748518516,-1.,1.68086176030308));
#29533=CARTESIAN_POINT('Ctrl Pts',(1.3406748518516,1.,1.68086176030308));
#29534=CARTESIAN_POINT('Ctrl Pts',(1.33960273470372,-1.,1.67458429426126));
#29535=CARTESIAN_POINT('Ctrl Pts',(1.33960273470372,1.,1.67458429426126));
#29536=CARTESIAN_POINT('Ctrl Pts',(1.33849388654458,-1.,1.66832460784078));
#29537=CARTESIAN_POINT('Ctrl Pts',(1.33849388654458,1.,1.66832460784078));
#29538=CARTESIAN_POINT('Ctrl Pts',(1.33734820885331,-1.,1.66208312542073));
#29539=CARTESIAN_POINT('Ctrl Pts',(1.33734820885331,1.,1.66208312542073));
#29540=CARTESIAN_POINT('Ctrl Pts',(1.33616559745217,-1.,1.65586025952651));
#29541=CARTESIAN_POINT('Ctrl Pts',(1.33616559745217,1.,1.65586025952651));
#29542=CARTESIAN_POINT('Ctrl Pts',(1.33494590468003,-1.,1.64965637286843));
#29543=CARTESIAN_POINT('Ctrl Pts',(1.33494590468003,1.,1.64965637286843));
#29544=CARTESIAN_POINT('Ctrl Pts',(1.33368890676554,-1.,1.64347174856007));
#29545=CARTESIAN_POINT('Ctrl Pts',(1.33368890676554,1.,1.64347174856007));
#29546=CARTESIAN_POINT('Ctrl Pts',(1.33239425103694,-1.,1.6373065347505));
#29547=CARTESIAN_POINT('Ctrl Pts',(1.33239425103694,1.,1.6373065347505));
#29548=CARTESIAN_POINT('Ctrl Pts',(1.33106149345618,-1.,1.63116079730887));
#29549=CARTESIAN_POINT('Ctrl Pts',(1.33106149345618,1.,1.63116079730887));
#29550=CARTESIAN_POINT('Ctrl Pts',(1.32969019505665,-1.,1.62503464209777));
#29551=CARTESIAN_POINT('Ctrl Pts',(1.32969019505665,1.,1.62503464209777));
#29552=CARTESIAN_POINT('Ctrl Pts',(1.32828000610448,-1.,1.61892832270723));
#29553=CARTESIAN_POINT('Ctrl Pts',(1.32828000610448,1.,1.61892832270723));
#29554=CARTESIAN_POINT('Ctrl Pts',(1.32683074483365,-1.,1.61284234015762));
#29555=CARTESIAN_POINT('Ctrl Pts',(1.32683074483365,1.,1.61284234015762));
#29556=CARTESIAN_POINT('Ctrl Pts',(1.32534250785794,-1.,1.6067775829097));
#29557=CARTESIAN_POINT('Ctrl Pts',(1.32534250785794,1.,1.6067775829097));
#29558=CARTESIAN_POINT('Ctrl Pts',(1.32381550858266,-1.,1.600735118587));
#29559=CARTESIAN_POINT('Ctrl Pts',(1.32381550858266,1.,1.600735118587));
#29560=CARTESIAN_POINT('Ctrl Pts',(1.32224985747686,-1.,1.59471591079408));
#29561=CARTESIAN_POINT('Ctrl Pts',(1.32224985747686,1.,1.59471591079408));
#29562=CARTESIAN_POINT('Ctrl Pts',(1.32064537110891,-1.,1.58872057258244));
#29563=CARTESIAN_POINT('Ctrl Pts',(1.32064537110891,1.,1.58872057258244));
#29564=CARTESIAN_POINT('Ctrl Pts',(1.31900135021428,-1.,1.58274907898829));
#29565=CARTESIAN_POINT('Ctrl Pts',(1.31900135021428,1.,1.58274907898829));
#29566=CARTESIAN_POINT('Ctrl Pts',(1.31731642317183,-1.,1.57680056505585));
#29567=CARTESIAN_POINT('Ctrl Pts',(1.31731642317183,1.,1.57680056505585));
#29568=CARTESIAN_POINT('Ctrl Pts',(1.31558903860015,-1.,1.57087397835721));
#29569=CARTESIAN_POINT('Ctrl Pts',(1.31558903860015,1.,1.57087397835721));
#29570=CARTESIAN_POINT('Ctrl Pts',(1.31381795281002,-1.,1.56496872402352));
#29571=CARTESIAN_POINT('Ctrl Pts',(1.31381795281002,1.,1.56496872402352));
#29572=CARTESIAN_POINT('Ctrl Pts',(1.31200264341696,-1.,1.55908521254822));
#29573=CARTESIAN_POINT('Ctrl Pts',(1.31200264341696,1.,1.55908521254822));
#29574=CARTESIAN_POINT('Ctrl Pts',(1.31014393684221,-1.,1.55322568759481));
#29575=CARTESIAN_POINT('Ctrl Pts',(1.31014393684221,1.,1.55322568759481));
#29576=CARTESIAN_POINT('Ctrl Pts',(1.30824393907471,-1.,1.54739413957183));
#29577=CARTESIAN_POINT('Ctrl Pts',(1.30824393907471,1.,1.54739413957183));
#29578=CARTESIAN_POINT('Ctrl Pts',(1.30630475189553,-1.,1.54159462645428));
#29579=CARTESIAN_POINT('Ctrl Pts',(1.30630475189553,1.,1.54159462645428));
#29580=CARTESIAN_POINT('Ctrl Pts',(1.30432735639487,-1.,1.53582981268976));
#29581=CARTESIAN_POINT('Ctrl Pts',(1.30432735639487,1.,1.53582981268976));
#29582=CARTESIAN_POINT('Ctrl Pts',(1.3023106439557,-1.,1.53009970283893));
#29583=CARTESIAN_POINT('Ctrl Pts',(1.3023106439557,1.,1.53009970283893));
#29584=CARTESIAN_POINT('Ctrl Pts',(1.30024984366334,-1.,1.5243995786107));
#29585=CARTESIAN_POINT('Ctrl Pts',(1.30024984366334,1.,1.5243995786107));
#29586=CARTESIAN_POINT('Ctrl Pts',(1.29813791800757,-1.,1.51872184912735));
#29587=CARTESIAN_POINT('Ctrl Pts',(1.29813791800757,1.,1.51872184912735));
#29588=CARTESIAN_POINT('Ctrl Pts',(1.29596850710518,-1.,1.51305994241412));
#29589=CARTESIAN_POINT('Ctrl Pts',(1.29596850710518,1.,1.51305994241412));
#29590=CARTESIAN_POINT('Ctrl Pts',(1.29373841372843,-1.,1.50741159078367));
#29591=CARTESIAN_POINT('Ctrl Pts',(1.29373841372843,1.,1.50741159078367));
#29592=CARTESIAN_POINT('Ctrl Pts',(1.29145022885171,-1.,1.50178230149764));
#29593=CARTESIAN_POINT('Ctrl Pts',(1.29145022885171,1.,1.50178230149764));
#29594=CARTESIAN_POINT('Ctrl Pts',(1.28911506584232,-1.,1.49618896881729));
#29595=CARTESIAN_POINT('Ctrl Pts',(1.28911506584232,1.,1.49618896881729));
#29596=CARTESIAN_POINT('Ctrl Pts',(1.28674676116415,-1.,1.4906522831275));
#29597=CARTESIAN_POINT('Ctrl Pts',(1.28674676116415,1.,1.4906522831275));
#29598=CARTESIAN_POINT('Ctrl Pts',(1.28435533880184,-1.,1.48518817118891));
#29599=CARTESIAN_POINT('Ctrl Pts',(1.28435533880184,1.,1.48518817118891));
#29600=CARTESIAN_POINT('Ctrl Pts',(1.28194158939522,-1.,1.47980070347102));
#29601=CARTESIAN_POINT('Ctrl Pts',(1.28194158939522,1.,1.47980070347102));
#29602=CARTESIAN_POINT('Ctrl Pts',(1.27948918248524,-1.,1.4744717526711));
#29603=CARTESIAN_POINT('Ctrl Pts',(1.27948918248524,1.,1.4744717526711));
#29604=CARTESIAN_POINT('Ctrl Pts',(1.27696414831144,-1.,1.46916035917197));
#29605=CARTESIAN_POINT('Ctrl Pts',(1.27696414831144,1.,1.46916035917197));
#29606=CARTESIAN_POINT('Ctrl Pts',(1.27433119897877,-1.,1.4638243133254));
#29607=CARTESIAN_POINT('Ctrl Pts',(1.27433119897877,1.,1.4638243133254));
#29608=CARTESIAN_POINT('Ctrl Pts',(1.27156805265312,-1.,1.45843906294725));
#29609=CARTESIAN_POINT('Ctrl Pts',(1.27156805265312,1.,1.45843906294725));
#29610=CARTESIAN_POINT('Ctrl Pts',(1.26867786804854,-1.,1.45301422764205));
#29611=CARTESIAN_POINT('Ctrl Pts',(1.26867786804854,1.,1.45301422764205));
#29612=CARTESIAN_POINT('Ctrl Pts',(1.26570925118767,-1.,1.44761985001544));
#29613=CARTESIAN_POINT('Ctrl Pts',(1.26570925118767,1.,1.44761985001544));
#29614=CARTESIAN_POINT('Ctrl Pts',(1.26273903323723,-1.,1.44236470511145));
#29615=CARTESIAN_POINT('Ctrl Pts',(1.26273903323723,1.,1.44236470511145));
#29616=CARTESIAN_POINT('Ctrl Pts',(1.25983531011894,-1.,1.43734919180719));
#29617=CARTESIAN_POINT('Ctrl Pts',(1.25983531011894,1.,1.43734919180719));
#29618=CARTESIAN_POINT('Ctrl Pts',(1.25702687965744,-1.,1.43262645609679));
#29619=CARTESIAN_POINT('Ctrl Pts',(1.25702687965744,1.,1.43262645609679));
#29620=CARTESIAN_POINT('Ctrl Pts',(1.25426945222783,-1.,1.42815938799555));
#29621=CARTESIAN_POINT('Ctrl Pts',(1.25426945222783,1.,1.42815938799555));
#29622=CARTESIAN_POINT('Ctrl Pts',(1.25141455570299,-1.,1.42378102115911));
#29623=CARTESIAN_POINT('Ctrl Pts',(1.25141455570299,1.,1.42378102115911));
#29624=CARTESIAN_POINT('Ctrl Pts',(1.24824430986911,-1.,1.41923722596421));
#29625=CARTESIAN_POINT('Ctrl Pts',(1.24824430986911,1.,1.41923722596421));
#29626=CARTESIAN_POINT('Ctrl Pts',(1.24450600513278,-1.,1.41422913175437));
#29627=CARTESIAN_POINT('Ctrl Pts',(1.24450600513278,1.,1.41422913175437));
#29628=CARTESIAN_POINT('Ctrl Pts',(1.23994455029421,-1.,1.40845295531151));
#29629=CARTESIAN_POINT('Ctrl Pts',(1.23994455029421,1.,1.40845295531151));
#29630=CARTESIAN_POINT('Ctrl Pts',(1.23434087289768,-1.,1.40164708205345));
#29631=CARTESIAN_POINT('Ctrl Pts',(1.23434087289768,1.,1.40164708205345));
#29632=CARTESIAN_POINT('Ctrl Pts',(1.22752961898063,-1.,1.39361389567257));
#29633=CARTESIAN_POINT('Ctrl Pts',(1.22752961898063,1.,1.39361389567257));
#29634=CARTESIAN_POINT('Ctrl Pts',(1.21938737278853,-1.,1.38420564525391));
#29635=CARTESIAN_POINT('Ctrl Pts',(1.21938737278853,1.,1.38420564525391));
#29636=CARTESIAN_POINT('Ctrl Pts',(1.20982812923113,-1.,1.37331915604962));
#29637=CARTESIAN_POINT('Ctrl Pts',(1.20982812923113,1.,1.37331915604962));
#29638=CARTESIAN_POINT('Ctrl Pts',(1.1987959077656,-1.,1.36088705040677));
#29639=CARTESIAN_POINT('Ctrl Pts',(1.1987959077656,1.,1.36088705040677));
#29640=CARTESIAN_POINT('Ctrl Pts',(1.18625865664915,-1.,1.34687053998157));
#29641=CARTESIAN_POINT('Ctrl Pts',(1.18625865664915,1.,1.34687053998157));
#29642=CARTESIAN_POINT('Ctrl Pts',(1.17501305787994,-1.,1.33437539344842));
#29643=CARTESIAN_POINT('Ctrl Pts',(1.17501305787994,1.,1.33437539344842));
#29644=CARTESIAN_POINT('Ctrl Pts',(1.16589330092532,-1.,1.32428080720544));
#29645=CARTESIAN_POINT('Ctrl Pts',(1.16589330092532,1.,1.32428080720544));
#29646=CARTESIAN_POINT('Ctrl Pts',(1.15950888730433,-1.,1.3172297721596));
#29647=CARTESIAN_POINT('Ctrl Pts',(1.15950888730433,1.,1.3172297721596));
#29648=CARTESIAN_POINT('Ctrl Pts',(1.15624053661742,-1.,1.31362392696033));
#29649=CARTESIAN_POINT('Ctrl Pts',(1.15624053661742,1.,1.31362392696033));
#29650=CARTESIAN_POINT('',(1.34869019493419,1.,1.73811241238545));
#29651=CARTESIAN_POINT('Ctrl Pts',(1.34869019493419,1.,1.73811241238545));
#29652=CARTESIAN_POINT('Ctrl Pts',(1.34854391898145,1.,1.73682580585819));
#29653=CARTESIAN_POINT('Ctrl Pts',(1.34824783113158,1.,1.73425417886255));
#29654=CARTESIAN_POINT('Ctrl Pts',(1.3477930915247,1.,1.73040149654497));
#29655=CARTESIAN_POINT('Ctrl Pts',(1.34716554820013,1.,1.72527410681298));
#29656=CARTESIAN_POINT('Ctrl Pts',(1.34634568653586,1.,1.7188807715095));
#29657=CARTESIAN_POINT('Ctrl Pts',(1.34549029589563,1.,1.71250340687011));
#29658=CARTESIAN_POINT('Ctrl Pts',(1.34459924533783,1.,1.70614212266676));
#29659=CARTESIAN_POINT('Ctrl Pts',(1.34367237124322,1.,1.69979707754221));
#29660=CARTESIAN_POINT('Ctrl Pts',(1.34270948206139,1.,1.6934684849664));
#29661=CARTESIAN_POINT('Ctrl Pts',(1.34171037484673,1.,1.68715660868602));
#29662=CARTESIAN_POINT('Ctrl Pts',(1.3406748518516,1.,1.68086176030308));
#29663=CARTESIAN_POINT('Ctrl Pts',(1.33960273470372,1.,1.67458429426126));
#29664=CARTESIAN_POINT('Ctrl Pts',(1.33849388654458,1.,1.66832460784078));
#29665=CARTESIAN_POINT('Ctrl Pts',(1.33734820885331,1.,1.66208312542073));
#29666=CARTESIAN_POINT('Ctrl Pts',(1.33616559745217,1.,1.65586025952651));
#29667=CARTESIAN_POINT('Ctrl Pts',(1.33494590468003,1.,1.64965637286843));
#29668=CARTESIAN_POINT('Ctrl Pts',(1.33368890676554,1.,1.64347174856007));
#29669=CARTESIAN_POINT('Ctrl Pts',(1.33239425103694,1.,1.6373065347505));
#29670=CARTESIAN_POINT('Ctrl Pts',(1.33106149345618,1.,1.63116079730887));
#29671=CARTESIAN_POINT('Ctrl Pts',(1.32969019505665,1.,1.62503464209777));
#29672=CARTESIAN_POINT('Ctrl Pts',(1.32828000610448,1.,1.61892832270723));
#29673=CARTESIAN_POINT('Ctrl Pts',(1.32683074483365,1.,1.61284234015762));
#29674=CARTESIAN_POINT('Ctrl Pts',(1.32534250785794,1.,1.6067775829097));
#29675=CARTESIAN_POINT('Ctrl Pts',(1.32381550858266,1.,1.600735118587));
#29676=CARTESIAN_POINT('Ctrl Pts',(1.32224985747686,1.,1.59471591079408));
#29677=CARTESIAN_POINT('Ctrl Pts',(1.32064537110891,1.,1.58872057258244));
#29678=CARTESIAN_POINT('Ctrl Pts',(1.31900135021428,1.,1.58274907898829));
#29679=CARTESIAN_POINT('Ctrl Pts',(1.31731642317183,1.,1.57680056505585));
#29680=CARTESIAN_POINT('Ctrl Pts',(1.31558903860015,1.,1.57087397835721));
#29681=CARTESIAN_POINT('Ctrl Pts',(1.31381795281002,1.,1.56496872402352));
#29682=CARTESIAN_POINT('Ctrl Pts',(1.31200264341696,1.,1.55908521254822));
#29683=CARTESIAN_POINT('Ctrl Pts',(1.31014393684221,1.,1.55322568759481));
#29684=CARTESIAN_POINT('Ctrl Pts',(1.30824393907471,1.,1.54739413957183));
#29685=CARTESIAN_POINT('Ctrl Pts',(1.30630475189553,1.,1.54159462645428));
#29686=CARTESIAN_POINT('Ctrl Pts',(1.30432735639487,1.,1.53582981268976));
#29687=CARTESIAN_POINT('Ctrl Pts',(1.3023106439557,1.,1.53009970283893));
#29688=CARTESIAN_POINT('Ctrl Pts',(1.30024984366334,1.,1.5243995786107));
#29689=CARTESIAN_POINT('Ctrl Pts',(1.29813791800757,1.,1.51872184912735));
#29690=CARTESIAN_POINT('Ctrl Pts',(1.29596850710518,1.,1.51305994241412));
#29691=CARTESIAN_POINT('Ctrl Pts',(1.29373841372843,1.,1.50741159078367));
#29692=CARTESIAN_POINT('Ctrl Pts',(1.29145022885171,1.,1.50178230149764));
#29693=CARTESIAN_POINT('Ctrl Pts',(1.28911506584232,1.,1.49618896881729));
#29694=CARTESIAN_POINT('Ctrl Pts',(1.28674676116415,1.,1.4906522831275));
#29695=CARTESIAN_POINT('Ctrl Pts',(1.28435533880184,1.,1.48518817118891));
#29696=CARTESIAN_POINT('Ctrl Pts',(1.28194158939522,1.,1.47980070347102));
#29697=CARTESIAN_POINT('Ctrl Pts',(1.27948918248524,1.,1.4744717526711));
#29698=CARTESIAN_POINT('Ctrl Pts',(1.27696414831144,1.,1.46916035917197));
#29699=CARTESIAN_POINT('Ctrl Pts',(1.27433119897877,1.,1.4638243133254));
#29700=CARTESIAN_POINT('Ctrl Pts',(1.27156805265312,1.,1.45843906294725));
#29701=CARTESIAN_POINT('Ctrl Pts',(1.26867786804854,1.,1.45301422764205));
#29702=CARTESIAN_POINT('Ctrl Pts',(1.26570925118767,1.,1.44761985001544));
#29703=CARTESIAN_POINT('Ctrl Pts',(1.26273903323723,1.,1.44236470511145));
#29704=CARTESIAN_POINT('Ctrl Pts',(1.25983531011894,1.,1.43734919180719));
#29705=CARTESIAN_POINT('Ctrl Pts',(1.25702687965744,1.,1.43262645609679));
#29706=CARTESIAN_POINT('Ctrl Pts',(1.25426945222783,1.,1.42815938799555));
#29707=CARTESIAN_POINT('Ctrl Pts',(1.25141455570299,1.,1.42378102115911));
#29708=CARTESIAN_POINT('Ctrl Pts',(1.24824430986911,1.,1.41923722596421));
#29709=CARTESIAN_POINT('Ctrl Pts',(1.24450600513278,1.,1.41422913175437));
#29710=CARTESIAN_POINT('Ctrl Pts',(1.23994455029421,1.,1.40845295531151));
#29711=CARTESIAN_POINT('Ctrl Pts',(1.23434087289768,1.,1.40164708205345));
#29712=CARTESIAN_POINT('Ctrl Pts',(1.22752961898063,1.,1.39361389567257));
#29713=CARTESIAN_POINT('Ctrl Pts',(1.21938737278853,1.,1.38420564525391));
#29714=CARTESIAN_POINT('Ctrl Pts',(1.20982812923113,1.,1.37331915604962));
#29715=CARTESIAN_POINT('Ctrl Pts',(1.1987959077656,1.,1.36088705040677));
#29716=CARTESIAN_POINT('Ctrl Pts',(1.18625865664915,1.,1.34687053998157));
#29717=CARTESIAN_POINT('Ctrl Pts',(1.17501305787994,1.,1.33437539344842));
#29718=CARTESIAN_POINT('Ctrl Pts',(1.16589330092532,1.,1.32428080720544));
#29719=CARTESIAN_POINT('Ctrl Pts',(1.15950888730433,1.,1.3172297721596));
#29720=CARTESIAN_POINT('Ctrl Pts',(1.15624053661742,1.,1.31362392696033));
#29721=CARTESIAN_POINT('',(1.34869019493419,0.,1.73811241238545));
#29722=CARTESIAN_POINT('Origin',(1.23627494547115,0.,1.81978687191668));
#29723=CARTESIAN_POINT('',(1.23627494547115,1.,1.81978687191668));
#29724=CARTESIAN_POINT('',(1.34869019493419,1.,1.73811241238545));
#29725=CARTESIAN_POINT('',(1.23627494547115,0.,1.81978687191668));
#29726=CARTESIAN_POINT('Ctrl Pts',(0.892032620296855,-1.,1.5055822144029));
#29727=CARTESIAN_POINT('Ctrl Pts',(0.892032620296855,1.,1.5055822144029));
#29728=CARTESIAN_POINT('Ctrl Pts',(0.894452006967538,-1.,1.50980486807181));
#29729=CARTESIAN_POINT('Ctrl Pts',(0.894452006967538,1.,1.50980486807181));
#29730=CARTESIAN_POINT('Ctrl Pts',(0.89918504749193,-1.,1.51805569591479));
#29731=CARTESIAN_POINT('Ctrl Pts',(0.89918504749193,1.,1.51805569591479));
#29732=CARTESIAN_POINT('Ctrl Pts',(0.905967409640498,-1.,1.52984849890434));
#29733=CARTESIAN_POINT('Ctrl Pts',(0.905967409640498,1.,1.52984849890434));
#29734=CARTESIAN_POINT('Ctrl Pts',(0.914375919046579,-1.,1.54440491152808));
#29735=CARTESIAN_POINT('Ctrl Pts',(0.914375919046579,1.,1.54440491152808));
#29736=CARTESIAN_POINT('Ctrl Pts',(0.923832188966322,-1.,1.56065988582509));
#29737=CARTESIAN_POINT('Ctrl Pts',(0.923832188966322,1.,1.56065988582509));
#29738=CARTESIAN_POINT('Ctrl Pts',(0.932246680128848,-1.,1.57499388385561));
#29739=CARTESIAN_POINT('Ctrl Pts',(0.932246680128848,1.,1.57499388385561));
#29740=CARTESIAN_POINT('Ctrl Pts',(0.939646377909319,-1.,1.58744937489796));
#29741=CARTESIAN_POINT('Ctrl Pts',(0.939646377909319,1.,1.58744937489796));
#29742=CARTESIAN_POINT('Ctrl Pts',(0.946078063325795,-1.,1.59810042045408));
#29743=CARTESIAN_POINT('Ctrl Pts',(0.946078063325795,1.,1.59810042045408));
#29744=CARTESIAN_POINT('Ctrl Pts',(0.951613284361247,-1.,1.60706069897794));
#29745=CARTESIAN_POINT('Ctrl Pts',(0.951613284361247,1.,1.60706069897794));
#29746=CARTESIAN_POINT('Ctrl Pts',(0.956354422921572,-1.,1.61449324337233));
#29747=CARTESIAN_POINT('Ctrl Pts',(0.956354422921572,1.,1.61449324337233));
#29748=CARTESIAN_POINT('Ctrl Pts',(0.960438326099958,-1.,1.62061638139929));
#29749=CARTESIAN_POINT('Ctrl Pts',(0.960438326099958,1.,1.62061638139929));
#29750=CARTESIAN_POINT('Ctrl Pts',(0.964046107037821,-1.,1.6257193066974));
#29751=CARTESIAN_POINT('Ctrl Pts',(0.964046107037821,1.,1.6257193066974));
#29752=CARTESIAN_POINT('Ctrl Pts',(0.967387853228041,-1.,1.63013849959083));
#29753=CARTESIAN_POINT('Ctrl Pts',(0.967387853228041,1.,1.63013849959083));
#29754=CARTESIAN_POINT('Ctrl Pts',(0.970669715996356,-1.,1.63420665729609));
#29755=CARTESIAN_POINT('Ctrl Pts',(0.970669715996356,1.,1.63420665729609));
#29756=CARTESIAN_POINT('Ctrl Pts',(0.974066058287501,-1.,1.63820952658157));
#29757=CARTESIAN_POINT('Ctrl Pts',(0.974066058287501,1.,1.63820952658157));
#29758=CARTESIAN_POINT('Ctrl Pts',(0.977689794120296,-1.,1.64233990826831));
#29759=CARTESIAN_POINT('Ctrl Pts',(0.977689794120296,1.,1.64233990826831));
#29760=CARTESIAN_POINT('Ctrl Pts',(0.981562530940574,-1.,1.64665139190834));
#29761=CARTESIAN_POINT('Ctrl Pts',(0.981562530940574,1.,1.64665139190834));
#29762=CARTESIAN_POINT('Ctrl Pts',(0.985642622921626,-1.,1.6511001661277));
#29763=CARTESIAN_POINT('Ctrl Pts',(0.985642622921626,1.,1.6511001661277));
#29764=CARTESIAN_POINT('Ctrl Pts',(0.98985562785445,-1.,1.65559044289746));
#29765=CARTESIAN_POINT('Ctrl Pts',(0.98985562785445,1.,1.65559044289746));
#29766=CARTESIAN_POINT('Ctrl Pts',(0.994121836661115,-1.,1.66001553809916));
#29767=CARTESIAN_POINT('Ctrl Pts',(0.994121836661115,1.,1.66001553809916));
#29768=CARTESIAN_POINT('Ctrl Pts',(0.998389654952317,-1.,1.66430758030304));
#29769=CARTESIAN_POINT('Ctrl Pts',(0.998389654952317,1.,1.66430758030304));
#29770=CARTESIAN_POINT('Ctrl Pts',(1.00265091003682,-1.,1.66846059277231));
#29771=CARTESIAN_POINT('Ctrl Pts',(1.00265091003682,1.,1.66846059277231));
#29772=CARTESIAN_POINT('Ctrl Pts',(1.00692206696387,-1.,1.67250335383248));
#29773=CARTESIAN_POINT('Ctrl Pts',(1.00692206696387,1.,1.67250335383248));
#29774=CARTESIAN_POINT('Ctrl Pts',(1.01123236493507,-1.,1.67648246776457));
#29775=CARTESIAN_POINT('Ctrl Pts',(1.01123236493507,1.,1.67648246776457));
#29776=CARTESIAN_POINT('Ctrl Pts',(1.01561026162786,-1.,1.6804428989482));
#29777=CARTESIAN_POINT('Ctrl Pts',(1.01561026162786,1.,1.6804428989482));
#29778=CARTESIAN_POINT('Ctrl Pts',(1.02006795074222,-1.,1.68440578021739));
#29779=CARTESIAN_POINT('Ctrl Pts',(1.02006795074222,1.,1.68440578021739));
#29780=CARTESIAN_POINT('Ctrl Pts',(1.02460180535272,-1.,1.68836910178475));
#29781=CARTESIAN_POINT('Ctrl Pts',(1.02460180535272,1.,1.68836910178475));
#29782=CARTESIAN_POINT('Ctrl Pts',(1.02919977579155,-1.,1.69231840863471));
#29783=CARTESIAN_POINT('Ctrl Pts',(1.02919977579155,1.,1.69231840863471));
#29784=CARTESIAN_POINT('Ctrl Pts',(1.03384646003587,-1.,1.69623414782769));
#29785=CARTESIAN_POINT('Ctrl Pts',(1.03384646003587,1.,1.69623414782769));
#29786=CARTESIAN_POINT('Ctrl Pts',(1.03852922490782,-1.,1.70010052930951));
#29787=CARTESIAN_POINT('Ctrl Pts',(1.03852922490782,1.,1.70010052930951));
#29788=CARTESIAN_POINT('Ctrl Pts',(1.04324363334546,-1.,1.70391338707969));
#29789=CARTESIAN_POINT('Ctrl Pts',(1.04324363334546,1.,1.70391338707969));
#29790=CARTESIAN_POINT('Ctrl Pts',(1.0479908540499,-1.,1.70767646263641));
#29791=CARTESIAN_POINT('Ctrl Pts',(1.0479908540499,1.,1.70767646263641));
#29792=CARTESIAN_POINT('Ctrl Pts',(1.05277517202853,-1.,1.71139783543986));
#29793=CARTESIAN_POINT('Ctrl Pts',(1.05277517202853,1.,1.71139783543986));
#29794=CARTESIAN_POINT('Ctrl Pts',(1.05760163192481,-1.,1.71508654427022));
#29795=CARTESIAN_POINT('Ctrl Pts',(1.05760163192481,1.,1.71508654427022));
#29796=CARTESIAN_POINT('Ctrl Pts',(1.06247324680649,-1.,1.71874858456908));
#29797=CARTESIAN_POINT('Ctrl Pts',(1.06247324680649,1.,1.71874858456908));
#29798=CARTESIAN_POINT('Ctrl Pts',(1.06738966975463,-1.,1.72238500928456));
#29799=CARTESIAN_POINT('Ctrl Pts',(1.06738966975463,1.,1.72238500928456));
#29800=CARTESIAN_POINT('Ctrl Pts',(1.07234866990252,-1.,1.72599406198489));
#29801=CARTESIAN_POINT('Ctrl Pts',(1.07234866990252,1.,1.72599406198489));
#29802=CARTESIAN_POINT('Ctrl Pts',(1.0773470373727,-1.,1.72957248977424));
#29803=CARTESIAN_POINT('Ctrl Pts',(1.0773470373727,1.,1.72957248977424));
#29804=CARTESIAN_POINT('Ctrl Pts',(1.08238162784749,-1.,1.73311705663407));
#29805=CARTESIAN_POINT('Ctrl Pts',(1.08238162784749,1.,1.73311705663407));
#29806=CARTESIAN_POINT('Ctrl Pts',(1.08745056285429,-1.,1.73662628326093));
#29807=CARTESIAN_POINT('Ctrl Pts',(1.08745056285429,1.,1.73662628326093));
#29808=CARTESIAN_POINT('Ctrl Pts',(1.09255329056496,-1.,1.74010053962252));
#29809=CARTESIAN_POINT('Ctrl Pts',(1.09255329056496,1.,1.74010053962252));
#29810=CARTESIAN_POINT('Ctrl Pts',(1.09768999241229,-1.,1.74354119236212));
#29811=CARTESIAN_POINT('Ctrl Pts',(1.09768999241229,1.,1.74354119236212));
#29812=CARTESIAN_POINT('Ctrl Pts',(1.10286118991144,-1.,1.74695004214924));
#29813=CARTESIAN_POINT('Ctrl Pts',(1.10286118991144,1.,1.74695004214924));
#29814=CARTESIAN_POINT('Ctrl Pts',(1.10806728183003,-1.,1.75032866075914));
#29815=CARTESIAN_POINT('Ctrl Pts',(1.10806728183003,1.,1.75032866075914));
#29816=CARTESIAN_POINT('Ctrl Pts',(1.11330807582542,-1.,1.75367772094617));
#29817=CARTESIAN_POINT('Ctrl Pts',(1.11330807582542,1.,1.75367772094617));
#29818=CARTESIAN_POINT('Ctrl Pts',(1.11858293216752,-1.,1.75699720772089));
#29819=CARTESIAN_POINT('Ctrl Pts',(1.11858293216752,1.,1.75699720772089));
#29820=CARTESIAN_POINT('Ctrl Pts',(1.12389096855078,-1.,1.76028671825084));
#29821=CARTESIAN_POINT('Ctrl Pts',(1.12389096855078,1.,1.76028671825084));
#29822=CARTESIAN_POINT('Ctrl Pts',(1.12923123555076,-1.,1.76354571966171));
#29823=CARTESIAN_POINT('Ctrl Pts',(1.12923123555076,1.,1.76354571966171));
#29824=CARTESIAN_POINT('Ctrl Pts',(1.13460291804634,-1.,1.76677384551883));
#29825=CARTESIAN_POINT('Ctrl Pts',(1.13460291804634,1.,1.76677384551883));
#29826=CARTESIAN_POINT('Ctrl Pts',(1.14000548337,-1.,1.76997111386806));
#29827=CARTESIAN_POINT('Ctrl Pts',(1.14000548337,1.,1.76997111386806));
#29828=CARTESIAN_POINT('Ctrl Pts',(1.14543858226948,-1.,1.77313777896234));
#29829=CARTESIAN_POINT('Ctrl Pts',(1.14543858226948,1.,1.77313777896234));
#29830=CARTESIAN_POINT('Ctrl Pts',(1.15090197841531,-1.,1.77627422557034));
#29831=CARTESIAN_POINT('Ctrl Pts',(1.15090197841531,1.,1.77627422557034));
#29832=CARTESIAN_POINT('Ctrl Pts',(1.15639547194689,-1.,1.77938085564261));
#29833=CARTESIAN_POINT('Ctrl Pts',(1.15639547194689,1.,1.77938085564261));
#29834=CARTESIAN_POINT('Ctrl Pts',(1.16191881298458,-1.,1.78245795880949));
#29835=CARTESIAN_POINT('Ctrl Pts',(1.16191881298458,1.,1.78245795880949));
#29836=CARTESIAN_POINT('Ctrl Pts',(1.16747166312239,-1.,1.78550566040349));
#29837=CARTESIAN_POINT('Ctrl Pts',(1.16747166312239,1.,1.78550566040349));
#29838=CARTESIAN_POINT('Ctrl Pts',(1.17305363177265,-1.,1.78852398877523));
#29839=CARTESIAN_POINT('Ctrl Pts',(1.17305363177265,1.,1.78852398877523));
#29840=CARTESIAN_POINT('Ctrl Pts',(1.17866429440781,-1.,1.79151291552646));
#29841=CARTESIAN_POINT('Ctrl Pts',(1.17866429440781,1.,1.79151291552646));
#29842=CARTESIAN_POINT('Ctrl Pts',(1.18430321697471,-1.,1.79447240321572));
#29843=CARTESIAN_POINT('Ctrl Pts',(1.18430321697471,1.,1.79447240321572));
#29844=CARTESIAN_POINT('Ctrl Pts',(1.1899699793456,-1.,1.79740245923649));
#29845=CARTESIAN_POINT('Ctrl Pts',(1.1899699793456,1.,1.79740245923649));
#29846=CARTESIAN_POINT('Ctrl Pts',(1.19566418930405,-1.,1.80030314370121));
#29847=CARTESIAN_POINT('Ctrl Pts',(1.19566418930405,1.,1.80030314370121));
#29848=CARTESIAN_POINT('Ctrl Pts',(1.2013854893912,-1.,1.8031745483882));
#29849=CARTESIAN_POINT('Ctrl Pts',(1.2013854893912,1.,1.8031745483882));
#29850=CARTESIAN_POINT('Ctrl Pts',(1.20713356605519,-1.,1.80601678480772));
#29851=CARTESIAN_POINT('Ctrl Pts',(1.20713356605519,1.,1.80601678480772));
#29852=CARTESIAN_POINT('Ctrl Pts',(1.2129081570818,-1.,1.80882996916931));
#29853=CARTESIAN_POINT('Ctrl Pts',(1.2129081570818,1.,1.80882996916931));
#29854=CARTESIAN_POINT('Ctrl Pts',(1.2187090610323,-1.,1.81161420806172));
#29855=CARTESIAN_POINT('Ctrl Pts',(1.2187090610323,1.,1.81161420806172));
#29856=CARTESIAN_POINT('Ctrl Pts',(1.22453613304507,-1.,1.81436959209778));
#29857=CARTESIAN_POINT('Ctrl Pts',(1.22453613304507,1.,1.81436959209778));
#29858=CARTESIAN_POINT('Ctrl Pts',(1.22921864890975,-1.,1.81655087183054));
#29859=CARTESIAN_POINT('Ctrl Pts',(1.22921864890975,1.,1.81655087183054));
#29860=CARTESIAN_POINT('Ctrl Pts',(1.23274224526804,-1.,1.81817389920914));
#29861=CARTESIAN_POINT('Ctrl Pts',(1.23274224526804,1.,1.81817389920914));
#29862=CARTESIAN_POINT('Ctrl Pts',(1.23509651170384,-1.,1.81925017193531));
#29863=CARTESIAN_POINT('Ctrl Pts',(1.23509651170384,1.,1.81925017193531));
#29864=CARTESIAN_POINT('Ctrl Pts',(1.23627494547115,-1.,1.81978687191668));
#29865=CARTESIAN_POINT('Ctrl Pts',(1.23627494547115,1.,1.81978687191668));
#29866=CARTESIAN_POINT('',(0.892032620296855,1.,1.5055822144029));
#29867=CARTESIAN_POINT('Ctrl Pts',(0.892032620296855,1.,1.5055822144029));
#29868=CARTESIAN_POINT('Ctrl Pts',(0.894452006967538,1.,1.50980486807181));
#29869=CARTESIAN_POINT('Ctrl Pts',(0.89918504749193,1.,1.51805569591479));
#29870=CARTESIAN_POINT('Ctrl Pts',(0.905967409640498,1.,1.52984849890434));
#29871=CARTESIAN_POINT('Ctrl Pts',(0.914375919046579,1.,1.54440491152808));
#29872=CARTESIAN_POINT('Ctrl Pts',(0.923832188966322,1.,1.56065988582509));
#29873=CARTESIAN_POINT('Ctrl Pts',(0.932246680128848,1.,1.57499388385561));
#29874=CARTESIAN_POINT('Ctrl Pts',(0.939646377909319,1.,1.58744937489796));
#29875=CARTESIAN_POINT('Ctrl Pts',(0.946078063325795,1.,1.59810042045408));
#29876=CARTESIAN_POINT('Ctrl Pts',(0.951613284361247,1.,1.60706069897794));
#29877=CARTESIAN_POINT('Ctrl Pts',(0.956354422921572,1.,1.61449324337233));
#29878=CARTESIAN_POINT('Ctrl Pts',(0.960438326099958,1.,1.62061638139929));
#29879=CARTESIAN_POINT('Ctrl Pts',(0.964046107037821,1.,1.6257193066974));
#29880=CARTESIAN_POINT('Ctrl Pts',(0.967387853228041,1.,1.63013849959083));
#29881=CARTESIAN_POINT('Ctrl Pts',(0.970669715996356,1.,1.63420665729609));
#29882=CARTESIAN_POINT('Ctrl Pts',(0.974066058287501,1.,1.63820952658157));
#29883=CARTESIAN_POINT('Ctrl Pts',(0.977689794120296,1.,1.64233990826831));
#29884=CARTESIAN_POINT('Ctrl Pts',(0.981562530940574,1.,1.64665139190834));
#29885=CARTESIAN_POINT('Ctrl Pts',(0.985642622921626,1.,1.6511001661277));
#29886=CARTESIAN_POINT('Ctrl Pts',(0.98985562785445,1.,1.65559044289746));
#29887=CARTESIAN_POINT('Ctrl Pts',(0.994121836661115,1.,1.66001553809916));
#29888=CARTESIAN_POINT('Ctrl Pts',(0.998389654952317,1.,1.66430758030304));
#29889=CARTESIAN_POINT('Ctrl Pts',(1.00265091003682,1.,1.66846059277231));
#29890=CARTESIAN_POINT('Ctrl Pts',(1.00692206696387,1.,1.67250335383248));
#29891=CARTESIAN_POINT('Ctrl Pts',(1.01123236493507,1.,1.67648246776457));
#29892=CARTESIAN_POINT('Ctrl Pts',(1.01561026162786,1.,1.6804428989482));
#29893=CARTESIAN_POINT('Ctrl Pts',(1.02006795074222,1.,1.68440578021739));
#29894=CARTESIAN_POINT('Ctrl Pts',(1.02460180535272,1.,1.68836910178475));
#29895=CARTESIAN_POINT('Ctrl Pts',(1.02919977579155,1.,1.69231840863471));
#29896=CARTESIAN_POINT('Ctrl Pts',(1.03384646003587,1.,1.69623414782769));
#29897=CARTESIAN_POINT('Ctrl Pts',(1.03852922490782,1.,1.70010052930951));
#29898=CARTESIAN_POINT('Ctrl Pts',(1.04324363334546,1.,1.70391338707969));
#29899=CARTESIAN_POINT('Ctrl Pts',(1.0479908540499,1.,1.70767646263641));
#29900=CARTESIAN_POINT('Ctrl Pts',(1.05277517202853,1.,1.71139783543986));
#29901=CARTESIAN_POINT('Ctrl Pts',(1.05760163192481,1.,1.71508654427022));
#29902=CARTESIAN_POINT('Ctrl Pts',(1.06247324680649,1.,1.71874858456908));
#29903=CARTESIAN_POINT('Ctrl Pts',(1.06738966975463,1.,1.72238500928456));
#29904=CARTESIAN_POINT('Ctrl Pts',(1.07234866990252,1.,1.72599406198489));
#29905=CARTESIAN_POINT('Ctrl Pts',(1.0773470373727,1.,1.72957248977424));
#29906=CARTESIAN_POINT('Ctrl Pts',(1.08238162784749,1.,1.73311705663407));
#29907=CARTESIAN_POINT('Ctrl Pts',(1.08745056285429,1.,1.73662628326093));
#29908=CARTESIAN_POINT('Ctrl Pts',(1.09255329056496,1.,1.74010053962252));
#29909=CARTESIAN_POINT('Ctrl Pts',(1.09768999241229,1.,1.74354119236212));
#29910=CARTESIAN_POINT('Ctrl Pts',(1.10286118991144,1.,1.74695004214924));
#29911=CARTESIAN_POINT('Ctrl Pts',(1.10806728183003,1.,1.75032866075914));
#29912=CARTESIAN_POINT('Ctrl Pts',(1.11330807582542,1.,1.75367772094617));
#29913=CARTESIAN_POINT('Ctrl Pts',(1.11858293216752,1.,1.75699720772089));
#29914=CARTESIAN_POINT('Ctrl Pts',(1.12389096855078,1.,1.76028671825084));
#29915=CARTESIAN_POINT('Ctrl Pts',(1.12923123555076,1.,1.76354571966171));
#29916=CARTESIAN_POINT('Ctrl Pts',(1.13460291804634,1.,1.76677384551883));
#29917=CARTESIAN_POINT('Ctrl Pts',(1.14000548337,1.,1.76997111386806));
#29918=CARTESIAN_POINT('Ctrl Pts',(1.14543858226948,1.,1.77313777896234));
#29919=CARTESIAN_POINT('Ctrl Pts',(1.15090197841531,1.,1.77627422557034));
#29920=CARTESIAN_POINT('Ctrl Pts',(1.15639547194689,1.,1.77938085564261));
#29921=CARTESIAN_POINT('Ctrl Pts',(1.16191881298458,1.,1.78245795880949));
#29922=CARTESIAN_POINT('Ctrl Pts',(1.16747166312239,1.,1.78550566040349));
#29923=CARTESIAN_POINT('Ctrl Pts',(1.17305363177265,1.,1.78852398877523));
#29924=CARTESIAN_POINT('Ctrl Pts',(1.17866429440781,1.,1.79151291552646));
#29925=CARTESIAN_POINT('Ctrl Pts',(1.18430321697471,1.,1.79447240321572));
#29926=CARTESIAN_POINT('Ctrl Pts',(1.1899699793456,1.,1.79740245923649));
#29927=CARTESIAN_POINT('Ctrl Pts',(1.19566418930405,1.,1.80030314370121));
#29928=CARTESIAN_POINT('Ctrl Pts',(1.2013854893912,1.,1.8031745483882));
#29929=CARTESIAN_POINT('Ctrl Pts',(1.20713356605519,1.,1.80601678480772));
#29930=CARTESIAN_POINT('Ctrl Pts',(1.2129081570818,1.,1.80882996916931));
#29931=CARTESIAN_POINT('Ctrl Pts',(1.2187090610323,1.,1.81161420806172));
#29932=CARTESIAN_POINT('Ctrl Pts',(1.22453613304507,1.,1.81436959209778));
#29933=CARTESIAN_POINT('Ctrl Pts',(1.22921864890975,1.,1.81655087183054));
#29934=CARTESIAN_POINT('Ctrl Pts',(1.23274224526804,1.,1.81817389920914));
#29935=CARTESIAN_POINT('Ctrl Pts',(1.23509651170384,1.,1.81925017193531));
#29936=CARTESIAN_POINT('Ctrl Pts',(1.23627494547115,1.,1.81978687191668));
#29937=CARTESIAN_POINT('',(0.892032620296854,0.,1.5055822144029));
#29938=CARTESIAN_POINT('Origin',(0.,0.,0.));
#29939=CARTESIAN_POINT('',(0.693717979106305,1.,1.60662857109684));
#29940=CARTESIAN_POINT('Origin',(0.,1.,0.));
#29941=CARTESIAN_POINT('',(0.693717979106305,0.,1.60662857109684));
#29942=CARTESIAN_POINT('Ctrl Pts',(0.7455743247944,-1.,2.0698113262342));
#29943=CARTESIAN_POINT('Ctrl Pts',(0.7455743247944,1.,2.0698113262342));
#29944=CARTESIAN_POINT('Ctrl Pts',(0.745832791378367,-1.,2.06854248895728));
#29945=CARTESIAN_POINT('Ctrl Pts',(0.745832791378367,1.,2.06854248895728));
#29946=CARTESIAN_POINT('Ctrl Pts',(0.7463458715442,-1.,2.06600523016815));
#29947=CARTESIAN_POINT('Ctrl Pts',(0.7463458715442,1.,2.06600523016815));
#29948=CARTESIAN_POINT('Ctrl Pts',(0.747103932787919,-1.,2.06220058927826));
#29949=CARTESIAN_POINT('Ctrl Pts',(0.747103932787919,1.,2.06220058927826));
#29950=CARTESIAN_POINT('Ctrl Pts',(0.748091554183802,-1.,2.05713023031007));
#29951=CARTESIAN_POINT('Ctrl Pts',(0.748091554183802,1.,2.05713023031007));
#29952=CARTESIAN_POINT('Ctrl Pts',(0.749287468665046,-1.,2.05079645592154));
#29953=CARTESIAN_POINT('Ctrl Pts',(0.749287468665046,1.,2.05079645592154));
#29954=CARTESIAN_POINT('Ctrl Pts',(0.750444657875575,-1.,2.04446689147979));
#29955=CARTESIAN_POINT('Ctrl Pts',(0.750444657875575,1.,2.04446689147979));
#29956=CARTESIAN_POINT('Ctrl Pts',(0.751562963361115,-1.,2.03814160092099));
#29957=CARTESIAN_POINT('Ctrl Pts',(0.751562963361115,1.,2.03814160092099));
#29958=CARTESIAN_POINT('Ctrl Pts',(0.75264218048721,-1.,2.03182068456221));
#29959=CARTESIAN_POINT('Ctrl Pts',(0.75264218048721,1.,2.03182068456221));
#29960=CARTESIAN_POINT('Ctrl Pts',(0.753682061112768,-1.,2.02550428623313));
#29961=CARTESIAN_POINT('Ctrl Pts',(0.753682061112768,1.,2.02550428623313));
#29962=CARTESIAN_POINT('Ctrl Pts',(0.754682330722816,-1.,2.01919259405809));
#29963=CARTESIAN_POINT('Ctrl Pts',(0.754682330722816,1.,2.01919259405809));
#29964=CARTESIAN_POINT('Ctrl Pts',(0.755642704957865,-1.,2.01288584328084));
#29965=CARTESIAN_POINT('Ctrl Pts',(0.755642704957865,1.,2.01288584328084));
#29966=CARTESIAN_POINT('Ctrl Pts',(0.75656290464667,-1.,2.0065843158773));
#29967=CARTESIAN_POINT('Ctrl Pts',(0.75656290464667,1.,2.0065843158773));
#29968=CARTESIAN_POINT('Ctrl Pts',(0.757442676862724,-1.,2.00028834739178));
#29969=CARTESIAN_POINT('Ctrl Pts',(0.757442676862724,1.,2.00028834739178));
#29970=CARTESIAN_POINT('Ctrl Pts',(0.758281796766761,-1.,1.99399831098817));
#29971=CARTESIAN_POINT('Ctrl Pts',(0.758281796766761,1.,1.99399831098817));
#29972=CARTESIAN_POINT('Ctrl Pts',(0.759080037802488,-1.,1.98771456680874));
#29973=CARTESIAN_POINT('Ctrl Pts',(0.759080037802488,1.,1.98771456680874));
#29974=CARTESIAN_POINT('Ctrl Pts',(0.75983714745219,-1.,1.98143741418172));
#29975=CARTESIAN_POINT('Ctrl Pts',(0.75983714745219,1.,1.98143741418172));
#29976=CARTESIAN_POINT('Ctrl Pts',(0.760552825409757,-1.,1.97516705321494));
#29977=CARTESIAN_POINT('Ctrl Pts',(0.760552825409757,1.,1.97516705321494));
#29978=CARTESIAN_POINT('Ctrl Pts',(0.76122669048382,-1.,1.96890351582499));
#29979=CARTESIAN_POINT('Ctrl Pts',(0.76122669048382,1.,1.96890351582499));
#29980=CARTESIAN_POINT('Ctrl Pts',(0.761858300014423,-1.,1.96264672744186));
#29981=CARTESIAN_POINT('Ctrl Pts',(0.761858300014423,1.,1.96264672744186));
#29982=CARTESIAN_POINT('Ctrl Pts',(0.762447203806178,-1.,1.95639665309869));
#29983=CARTESIAN_POINT('Ctrl Pts',(0.762447203806178,1.,1.95639665309869));
#29984=CARTESIAN_POINT('Ctrl Pts',(0.762992990878769,-1.,1.95015342590024));
#29985=CARTESIAN_POINT('Ctrl Pts',(0.762992990878769,1.,1.95015342590024));
#29986=CARTESIAN_POINT('Ctrl Pts',(0.763495333538629,-1.,1.9439174661764));
#29987=CARTESIAN_POINT('Ctrl Pts',(0.763495333538629,1.,1.9439174661764));
#29988=CARTESIAN_POINT('Ctrl Pts',(0.763954049121458,-1.,1.93768964875886));
#29989=CARTESIAN_POINT('Ctrl Pts',(0.763954049121458,1.,1.93768964875886));
#29990=CARTESIAN_POINT('Ctrl Pts',(0.76436901067394,-1.,1.93147105496382));
#29991=CARTESIAN_POINT('Ctrl Pts',(0.76436901067394,1.,1.93147105496382));
#29992=CARTESIAN_POINT('Ctrl Pts',(0.764740025488211,-1.,1.92526263537048));
#29993=CARTESIAN_POINT('Ctrl Pts',(0.764740025488211,1.,1.92526263537048));
#29994=CARTESIAN_POINT('Ctrl Pts',(0.765066729667088,-1.,1.91906491634196));
#29995=CARTESIAN_POINT('Ctrl Pts',(0.765066729667088,1.,1.91906491634196));
#29996=CARTESIAN_POINT('Ctrl Pts',(0.765348465884722,-1.,1.91287765805169));
#29997=CARTESIAN_POINT('Ctrl Pts',(0.765348465884722,1.,1.91287765805169));
#29998=CARTESIAN_POINT('Ctrl Pts',(0.765584196937919,-1.,1.90669961402356));
#29999=CARTESIAN_POINT('Ctrl Pts',(0.765584196937919,1.,1.90669961402356));
#30000=CARTESIAN_POINT('Ctrl Pts',(0.765772772593386,-1.,1.90052930393596));
#30001=CARTESIAN_POINT('Ctrl Pts',(0.765772772593386,1.,1.90052930393596));
#30002=CARTESIAN_POINT('Ctrl Pts',(0.765913193856978,-1.,1.89436577771388));
#30003=CARTESIAN_POINT('Ctrl Pts',(0.765913193856978,1.,1.89436577771388));
#30004=CARTESIAN_POINT('Ctrl Pts',(0.766004837062091,-1.,1.88820926433409));
#30005=CARTESIAN_POINT('Ctrl Pts',(0.766004837062091,1.,1.88820926433409));
#30006=CARTESIAN_POINT('Ctrl Pts',(0.766047794851864,-1.,1.88206215302561));
#30007=CARTESIAN_POINT('Ctrl Pts',(0.766047794851864,1.,1.88206215302561));
#30008=CARTESIAN_POINT('Ctrl Pts',(0.766042837036744,-1.,1.87592888967883));
#30009=CARTESIAN_POINT('Ctrl Pts',(0.766042837036744,1.,1.87592888967883));
#30010=CARTESIAN_POINT('Ctrl Pts',(0.765990708546091,-1.,1.86981398314341));
#30011=CARTESIAN_POINT('Ctrl Pts',(0.765990708546091,1.,1.86981398314341));
#30012=CARTESIAN_POINT('Ctrl Pts',(0.765891519092547,-1.,1.86372027063312));
#30013=CARTESIAN_POINT('Ctrl Pts',(0.765891519092547,1.,1.86372027063312));
#30014=CARTESIAN_POINT('Ctrl Pts',(0.765744212909318,-1.,1.85764741390394));
#30015=CARTESIAN_POINT('Ctrl Pts',(0.765744212909318,1.,1.85764741390394));
#30016=CARTESIAN_POINT('Ctrl Pts',(0.765545710619062,-1.,1.85158945130063));
#30017=CARTESIAN_POINT('Ctrl Pts',(0.765545710619062,1.,1.85158945130063));
#30018=CARTESIAN_POINT('Ctrl Pts',(0.765291664862029,-1.,1.84553698875924));
#30019=CARTESIAN_POINT('Ctrl Pts',(0.765291664862029,1.,1.84553698875924));
#30020=CARTESIAN_POINT('Ctrl Pts',(0.764978057881737,-1.,1.83948181064835));
#30021=CARTESIAN_POINT('Ctrl Pts',(0.764978057881737,1.,1.83948181064835));
#30022=CARTESIAN_POINT('Ctrl Pts',(0.764602549687853,-1.,1.83342077227142));
#30023=CARTESIAN_POINT('Ctrl Pts',(0.764602549687853,1.,1.83342077227142));
#30024=CARTESIAN_POINT('Ctrl Pts',(0.764165902605995,-1.,1.82735991200065));
#30025=CARTESIAN_POINT('Ctrl Pts',(0.764165902605995,1.,1.82735991200065));
#30026=CARTESIAN_POINT('Ctrl Pts',(0.763673465462726,-1.,1.82131873145266));
#30027=CARTESIAN_POINT('Ctrl Pts',(0.763673465462726,1.,1.82131873145266));
#30028=CARTESIAN_POINT('Ctrl Pts',(0.763132003836634,-1.,1.8153211840553));
#30029=CARTESIAN_POINT('Ctrl Pts',(0.763132003836634,1.,1.8153211840553));
#30030=CARTESIAN_POINT('Ctrl Pts',(0.762546129463938,-1.,1.80938551463965));
#30031=CARTESIAN_POINT('Ctrl Pts',(0.762546129463938,1.,1.80938551463965));
#30032=CARTESIAN_POINT('Ctrl Pts',(0.761915336443547,-1.,1.80351583877342));
#30033=CARTESIAN_POINT('Ctrl Pts',(0.761915336443547,1.,1.80351583877342));
#30034=CARTESIAN_POINT('Ctrl Pts',(0.761229695230558,-1.,1.79768986997783));
#30035=CARTESIAN_POINT('Ctrl Pts',(0.761229695230558,1.,1.79768986997783));
#30036=CARTESIAN_POINT('Ctrl Pts',(0.760469555880749,-1.,1.7918581561088));
#30037=CARTESIAN_POINT('Ctrl Pts',(0.760469555880749,1.,1.7918581561088));
#30038=CARTESIAN_POINT('Ctrl Pts',(0.759614401110189,-1.,1.78596964884604));
#30039=CARTESIAN_POINT('Ctrl Pts',(0.759614401110189,1.,1.78596964884604));
#30040=CARTESIAN_POINT('Ctrl Pts',(0.758650626677518,-1.,1.77999411220945));
#30041=CARTESIAN_POINT('Ctrl Pts',(0.758650626677518,1.,1.77999411220945));
#30042=CARTESIAN_POINT('Ctrl Pts',(0.757578264077028,-1.,1.77394167108292));
#30043=CARTESIAN_POINT('Ctrl Pts',(0.757578264077028,1.,1.77394167108292));
#30044=CARTESIAN_POINT('Ctrl Pts',(0.75642189602781,-1.,1.76789396002998));
#30045=CARTESIAN_POINT('Ctrl Pts',(0.75642189602781,1.,1.76789396002998));
#30046=CARTESIAN_POINT('Ctrl Pts',(0.755220979974461,-1.,1.76197817240128));
#30047=CARTESIAN_POINT('Ctrl Pts',(0.755220979974461,1.,1.76197817240128));
#30048=CARTESIAN_POINT('Ctrl Pts',(0.754009254027828,-1.,1.75631083600019));
#30049=CARTESIAN_POINT('Ctrl Pts',(0.754009254027828,1.,1.75631083600019));
#30050=CARTESIAN_POINT('Ctrl Pts',(0.752797683531314,-1.,1.75095139468794));
#30051=CARTESIAN_POINT('Ctrl Pts',(0.752797683531314,1.,1.75095139468794));
#30052=CARTESIAN_POINT('Ctrl Pts',(0.751555614164482,-1.,1.74585086852502));
#30053=CARTESIAN_POINT('Ctrl Pts',(0.751555614164482,1.,1.74585086852502));
#30054=CARTESIAN_POINT('Ctrl Pts',(0.750193435981249,-1.,1.74080458267114));
#30055=CARTESIAN_POINT('Ctrl Pts',(0.750193435981249,1.,1.74080458267114));
#30056=CARTESIAN_POINT('Ctrl Pts',(0.74858246295687,-1.,1.7355035168033));
#30057=CARTESIAN_POINT('Ctrl Pts',(0.74858246295687,1.,1.7355035168033));
#30058=CARTESIAN_POINT('Ctrl Pts',(0.746574710097752,-1.,1.72958533647714));
#30059=CARTESIAN_POINT('Ctrl Pts',(0.746574710097752,1.,1.72958533647714));
#30060=CARTESIAN_POINT('Ctrl Pts',(0.744021445433093,-1.,1.72268229916769));
#30061=CARTESIAN_POINT('Ctrl Pts',(0.744021445433093,1.,1.72268229916769));
#30062=CARTESIAN_POINT('Ctrl Pts',(0.74079516202821,-1.,1.71447789751001));
#30063=CARTESIAN_POINT('Ctrl Pts',(0.74079516202821,1.,1.71447789751001));
#30064=CARTESIAN_POINT('Ctrl Pts',(0.736799665716932,-1.,1.70473309004249));
#30065=CARTESIAN_POINT('Ctrl Pts',(0.736799665716932,1.,1.70473309004249));
#30066=CARTESIAN_POINT('Ctrl Pts',(0.731963238685357,-1.,1.69326921972915));
#30067=CARTESIAN_POINT('Ctrl Pts',(0.731963238685357,1.,1.69326921972915));
#30068=CARTESIAN_POINT('Ctrl Pts',(0.726235967982445,-1.,1.67996158451922));
#30069=CARTESIAN_POINT('Ctrl Pts',(0.726235967982445,1.,1.67996158451922));
#30070=CARTESIAN_POINT('Ctrl Pts',(0.719585433787949,-1.,1.66472880551777));
#30071=CARTESIAN_POINT('Ctrl Pts',(0.719585433787949,1.,1.66472880551777));
#30072=CARTESIAN_POINT('Ctrl Pts',(0.711993139340447,-1.,1.64752408828442));
#30073=CARTESIAN_POINT('Ctrl Pts',(0.711993139340447,1.,1.64752408828442));
#30074=CARTESIAN_POINT('Ctrl Pts',(0.705159151977294,-1.,1.6321654166204));
#30075=CARTESIAN_POINT('Ctrl Pts',(0.705159151977294,1.,1.6321654166204));
#30076=CARTESIAN_POINT('Ctrl Pts',(0.699605146398836,-1.,1.61974673471117));
#30077=CARTESIAN_POINT('Ctrl Pts',(0.699605146398836,1.,1.61974673471117));
#30078=CARTESIAN_POINT('Ctrl Pts',(0.69571209787897,-1.,1.61106790957619));
#30079=CARTESIAN_POINT('Ctrl Pts',(0.69571209787897,1.,1.61106790957619));
#30080=CARTESIAN_POINT('Ctrl Pts',(0.693717979106305,-1.,1.60662857109684));
#30081=CARTESIAN_POINT('Ctrl Pts',(0.693717979106305,1.,1.60662857109684));
#30082=CARTESIAN_POINT('',(0.7455743247944,1.,2.0698113262342));
#30083=CARTESIAN_POINT('Ctrl Pts',(0.7455743247944,1.,2.0698113262342));
#30084=CARTESIAN_POINT('Ctrl Pts',(0.745832791378367,1.,2.06854248895728));
#30085=CARTESIAN_POINT('Ctrl Pts',(0.7463458715442,1.,2.06600523016815));
#30086=CARTESIAN_POINT('Ctrl Pts',(0.747103932787919,1.,2.06220058927826));
#30087=CARTESIAN_POINT('Ctrl Pts',(0.748091554183802,1.,2.05713023031007));
#30088=CARTESIAN_POINT('Ctrl Pts',(0.749287468665046,1.,2.05079645592154));
#30089=CARTESIAN_POINT('Ctrl Pts',(0.750444657875575,1.,2.04446689147979));
#30090=CARTESIAN_POINT('Ctrl Pts',(0.751562963361115,1.,2.03814160092099));
#30091=CARTESIAN_POINT('Ctrl Pts',(0.75264218048721,1.,2.03182068456221));
#30092=CARTESIAN_POINT('Ctrl Pts',(0.753682061112768,1.,2.02550428623313));
#30093=CARTESIAN_POINT('Ctrl Pts',(0.754682330722816,1.,2.01919259405809));
#30094=CARTESIAN_POINT('Ctrl Pts',(0.755642704957865,1.,2.01288584328084));
#30095=CARTESIAN_POINT('Ctrl Pts',(0.75656290464667,1.,2.0065843158773));
#30096=CARTESIAN_POINT('Ctrl Pts',(0.757442676862724,1.,2.00028834739178));
#30097=CARTESIAN_POINT('Ctrl Pts',(0.758281796766761,1.,1.99399831098817));
#30098=CARTESIAN_POINT('Ctrl Pts',(0.759080037802488,1.,1.98771456680874));
#30099=CARTESIAN_POINT('Ctrl Pts',(0.75983714745219,1.,1.98143741418172));
#30100=CARTESIAN_POINT('Ctrl Pts',(0.760552825409757,1.,1.97516705321494));
#30101=CARTESIAN_POINT('Ctrl Pts',(0.76122669048382,1.,1.96890351582499));
#30102=CARTESIAN_POINT('Ctrl Pts',(0.761858300014423,1.,1.96264672744186));
#30103=CARTESIAN_POINT('Ctrl Pts',(0.762447203806178,1.,1.95639665309869));
#30104=CARTESIAN_POINT('Ctrl Pts',(0.762992990878769,1.,1.95015342590024));
#30105=CARTESIAN_POINT('Ctrl Pts',(0.763495333538629,1.,1.9439174661764));
#30106=CARTESIAN_POINT('Ctrl Pts',(0.763954049121458,1.,1.93768964875886));
#30107=CARTESIAN_POINT('Ctrl Pts',(0.76436901067394,1.,1.93147105496382));
#30108=CARTESIAN_POINT('Ctrl Pts',(0.764740025488211,1.,1.92526263537048));
#30109=CARTESIAN_POINT('Ctrl Pts',(0.765066729667088,1.,1.91906491634196));
#30110=CARTESIAN_POINT('Ctrl Pts',(0.765348465884722,1.,1.91287765805169));
#30111=CARTESIAN_POINT('Ctrl Pts',(0.765584196937919,1.,1.90669961402356));
#30112=CARTESIAN_POINT('Ctrl Pts',(0.765772772593386,1.,1.90052930393596));
#30113=CARTESIAN_POINT('Ctrl Pts',(0.765913193856978,1.,1.89436577771388));
#30114=CARTESIAN_POINT('Ctrl Pts',(0.766004837062091,1.,1.88820926433409));
#30115=CARTESIAN_POINT('Ctrl Pts',(0.766047794851864,1.,1.88206215302561));
#30116=CARTESIAN_POINT('Ctrl Pts',(0.766042837036744,1.,1.87592888967883));
#30117=CARTESIAN_POINT('Ctrl Pts',(0.765990708546091,1.,1.86981398314341));
#30118=CARTESIAN_POINT('Ctrl Pts',(0.765891519092547,1.,1.86372027063312));
#30119=CARTESIAN_POINT('Ctrl Pts',(0.765744212909318,1.,1.85764741390394));
#30120=CARTESIAN_POINT('Ctrl Pts',(0.765545710619062,1.,1.85158945130063));
#30121=CARTESIAN_POINT('Ctrl Pts',(0.765291664862029,1.,1.84553698875924));
#30122=CARTESIAN_POINT('Ctrl Pts',(0.764978057881737,1.,1.83948181064835));
#30123=CARTESIAN_POINT('Ctrl Pts',(0.764602549687853,1.,1.83342077227142));
#30124=CARTESIAN_POINT('Ctrl Pts',(0.764165902605995,1.,1.82735991200065));
#30125=CARTESIAN_POINT('Ctrl Pts',(0.763673465462726,1.,1.82131873145266));
#30126=CARTESIAN_POINT('Ctrl Pts',(0.763132003836634,1.,1.8153211840553));
#30127=CARTESIAN_POINT('Ctrl Pts',(0.762546129463938,1.,1.80938551463965));
#30128=CARTESIAN_POINT('Ctrl Pts',(0.761915336443547,1.,1.80351583877342));
#30129=CARTESIAN_POINT('Ctrl Pts',(0.761229695230558,1.,1.79768986997783));
#30130=CARTESIAN_POINT('Ctrl Pts',(0.760469555880749,1.,1.7918581561088));
#30131=CARTESIAN_POINT('Ctrl Pts',(0.759614401110189,1.,1.78596964884604));
#30132=CARTESIAN_POINT('Ctrl Pts',(0.758650626677518,1.,1.77999411220945));
#30133=CARTESIAN_POINT('Ctrl Pts',(0.757578264077028,1.,1.77394167108292));
#30134=CARTESIAN_POINT('Ctrl Pts',(0.75642189602781,1.,1.76789396002998));
#30135=CARTESIAN_POINT('Ctrl Pts',(0.755220979974461,1.,1.76197817240128));
#30136=CARTESIAN_POINT('Ctrl Pts',(0.754009254027828,1.,1.75631083600019));
#30137=CARTESIAN_POINT('Ctrl Pts',(0.752797683531314,1.,1.75095139468794));
#30138=CARTESIAN_POINT('Ctrl Pts',(0.751555614164482,1.,1.74585086852502));
#30139=CARTESIAN_POINT('Ctrl Pts',(0.750193435981249,1.,1.74080458267114));
#30140=CARTESIAN_POINT('Ctrl Pts',(0.74858246295687,1.,1.7355035168033));
#30141=CARTESIAN_POINT('Ctrl Pts',(0.746574710097752,1.,1.72958533647714));
#30142=CARTESIAN_POINT('Ctrl Pts',(0.744021445433093,1.,1.72268229916769));
#30143=CARTESIAN_POINT('Ctrl Pts',(0.74079516202821,1.,1.71447789751001));
#30144=CARTESIAN_POINT('Ctrl Pts',(0.736799665716932,1.,1.70473309004249));
#30145=CARTESIAN_POINT('Ctrl Pts',(0.731963238685357,1.,1.69326921972915));
#30146=CARTESIAN_POINT('Ctrl Pts',(0.726235967982445,1.,1.67996158451922));
#30147=CARTESIAN_POINT('Ctrl Pts',(0.719585433787949,1.,1.66472880551777));
#30148=CARTESIAN_POINT('Ctrl Pts',(0.711993139340447,1.,1.64752408828442));
#30149=CARTESIAN_POINT('Ctrl Pts',(0.705159151977294,1.,1.6321654166204));
#30150=CARTESIAN_POINT('Ctrl Pts',(0.699605146398836,1.,1.61974673471117));
#30151=CARTESIAN_POINT('Ctrl Pts',(0.69571209787897,1.,1.61106790957619));
#30152=CARTESIAN_POINT('Ctrl Pts',(0.693717979106305,1.,1.60662857109684));
#30153=CARTESIAN_POINT('',(0.7455743247944,0.,2.0698113262342));
#30154=CARTESIAN_POINT('Origin',(0.61342227326009,0.,2.11275013067528));
#30155=CARTESIAN_POINT('',(0.61342227326009,1.,2.11275013067528));
#30156=CARTESIAN_POINT('',(0.7455743247944,1.,2.0698113262342));
#30157=CARTESIAN_POINT('',(0.61342227326009,0.,2.11275013067528));
#30158=CARTESIAN_POINT('Ctrl Pts',(0.383122945602004,-1.,1.7075470150345));
#30159=CARTESIAN_POINT('Ctrl Pts',(0.383122945602004,1.,1.7075470150345));
#30160=CARTESIAN_POINT('Ctrl Pts',(0.384119047315541,-1.,1.71231062891958));
#30161=CARTESIAN_POINT('Ctrl Pts',(0.384119047315541,1.,1.71231062891958));
#30162=CARTESIAN_POINT('Ctrl Pts',(0.38607079032701,-1.,1.72162022246158));
#30163=CARTESIAN_POINT('Ctrl Pts',(0.38607079032701,1.,1.72162022246158));
#30164=CARTESIAN_POINT('Ctrl Pts',(0.388877023509191,-1.,1.7349317097561));
#30165=CARTESIAN_POINT('Ctrl Pts',(0.388877023509191,1.,1.7349317097561));
#30166=CARTESIAN_POINT('Ctrl Pts',(0.392375812294307,-1.,1.75137405313962));
#30167=CARTESIAN_POINT('Ctrl Pts',(0.392375812294307,1.,1.75137405313962));
#30168=CARTESIAN_POINT('Ctrl Pts',(0.39634619612042,-1.,1.7697556004756));
#30169=CARTESIAN_POINT('Ctrl Pts',(0.39634619612042,1.,1.7697556004756));
#30170=CARTESIAN_POINT('Ctrl Pts',(0.39991940378308,-1.,1.78598826347533));
#30171=CARTESIAN_POINT('Ctrl Pts',(0.39991940378308,1.,1.78598826347533));
#30172=CARTESIAN_POINT('Ctrl Pts',(0.403107976170441,-1.,1.80012077176221));
#30173=CARTESIAN_POINT('Ctrl Pts',(0.403107976170441,1.,1.80012077176221));
#30174=CARTESIAN_POINT('Ctrl Pts',(0.405933518411838,-1.,1.81223801813988));
#30175=CARTESIAN_POINT('Ctrl Pts',(0.405933518411838,1.,1.81223801813988));
#30176=CARTESIAN_POINT('Ctrl Pts',(0.408428948108533,-1.,1.8224702267854));
#30177=CARTESIAN_POINT('Ctrl Pts',(0.408428948108533,1.,1.8224702267854));
#30178=CARTESIAN_POINT('Ctrl Pts',(0.410641256301674,-1.,1.83100408895216));
#30179=CARTESIAN_POINT('Ctrl Pts',(0.410641256301674,1.,1.83100408895216));
#30180=CARTESIAN_POINT('Ctrl Pts',(0.412633125322161,-1.,1.83808953475839));
#30181=CARTESIAN_POINT('Ctrl Pts',(0.412633125322161,1.,1.83808953475839));
#30182=CARTESIAN_POINT('Ctrl Pts',(0.41448743825434,-1.,1.8440575707371));
#30183=CARTESIAN_POINT('Ctrl Pts',(0.41448743825434,1.,1.8440575707371));
#30184=CARTESIAN_POINT('Ctrl Pts',(0.416300022038864,-1.,1.84929312929882));
#30185=CARTESIAN_POINT('Ctrl Pts',(0.416300022038864,1.,1.84929312929882));
#30186=CARTESIAN_POINT('Ctrl Pts',(0.418164129143534,-1.,1.85417632856234));
#30187=CARTESIAN_POINT('Ctrl Pts',(0.418164129143534,1.,1.85417632856234));
#30188=CARTESIAN_POINT('Ctrl Pts',(0.420157287975619,-1.,1.85903281096686));
#30189=CARTESIAN_POINT('Ctrl Pts',(0.420157287975619,1.,1.85903281096686));
#30190=CARTESIAN_POINT('Ctrl Pts',(0.422327307418275,-1.,1.86408083334028));
#30191=CARTESIAN_POINT('Ctrl Pts',(0.422327307418275,1.,1.86408083334028));
#30192=CARTESIAN_POINT('Ctrl Pts',(0.424678177291358,-1.,1.86937803944323));
#30193=CARTESIAN_POINT('Ctrl Pts',(0.424678177291358,1.,1.86937803944323));
#30194=CARTESIAN_POINT('Ctrl Pts',(0.427183828519102,-1.,1.87486989291484));
#30195=CARTESIAN_POINT('Ctrl Pts',(0.427183828519102,1.,1.87486989291484));
#30196=CARTESIAN_POINT('Ctrl Pts',(0.429803062482344,-1.,1.88044229001832));
#30197=CARTESIAN_POINT('Ctrl Pts',(0.429803062482344,1.,1.88044229001832));
#30198=CARTESIAN_POINT('Ctrl Pts',(0.432493038548748,-1.,1.88596913666793));
#30199=CARTESIAN_POINT('Ctrl Pts',(0.432493038548748,1.,1.88596913666793));
#30200=CARTESIAN_POINT('Ctrl Pts',(0.435225660963383,-1.,1.89136993975504));
#30201=CARTESIAN_POINT('Ctrl Pts',(0.435225660963383,1.,1.89136993975504));
#30202=CARTESIAN_POINT('Ctrl Pts',(0.437995003948244,-1.,1.89663648956466));
#30203=CARTESIAN_POINT('Ctrl Pts',(0.437995003948244,1.,1.89663648956466));
#30204=CARTESIAN_POINT('Ctrl Pts',(0.440807833704038,-1.,1.90180124389086));
#30205=CARTESIAN_POINT('Ctrl Pts',(0.440807833704038,1.,1.90180124389086));
#30206=CARTESIAN_POINT('Ctrl Pts',(0.44367755684915,-1.,1.90691756144898));
#30207=CARTESIAN_POINT('Ctrl Pts',(0.44367755684915,1.,1.90691756144898));
#30208=CARTESIAN_POINT('Ctrl Pts',(0.446617343485711,-1.,1.9120369998112));
#30209=CARTESIAN_POINT('Ctrl Pts',(0.446617343485711,1.,1.9120369998112));
#30210=CARTESIAN_POINT('Ctrl Pts',(0.449632260106662,-1.,1.91718342555755));
#30211=CARTESIAN_POINT('Ctrl Pts',(0.449632260106662,1.,1.91718342555755));
#30212=CARTESIAN_POINT('Ctrl Pts',(0.452719478359432,-1.,1.92235380648502));
#30213=CARTESIAN_POINT('Ctrl Pts',(0.452719478359432,1.,1.92235380648502));
#30214=CARTESIAN_POINT('Ctrl Pts',(0.45587200517437,-1.,1.92753067150476));
#30215=CARTESIAN_POINT('Ctrl Pts',(0.45587200517437,1.,1.92753067150476));
#30216=CARTESIAN_POINT('Ctrl Pts',(0.459081234547926,-1.,1.93269066517934));
#30217=CARTESIAN_POINT('Ctrl Pts',(0.459081234547926,1.,1.93269066517934));
#30218=CARTESIAN_POINT('Ctrl Pts',(0.462340031009056,-1.,1.93781486640821));
#30219=CARTESIAN_POINT('Ctrl Pts',(0.462340031009056,1.,1.93781486640821));
#30220=CARTESIAN_POINT('Ctrl Pts',(0.46564546202603,-1.,1.9428979419619));
#30221=CARTESIAN_POINT('Ctrl Pts',(0.46564546202603,1.,1.9428979419619));
#30222=CARTESIAN_POINT('Ctrl Pts',(0.468997482913135,-1.,1.94794381136514));
#30223=CARTESIAN_POINT('Ctrl Pts',(0.468997482913135,1.,1.94794381136514));
#30224=CARTESIAN_POINT('Ctrl Pts',(0.472397672264072,-1.,1.95296148278133));
#30225=CARTESIAN_POINT('Ctrl Pts',(0.472397672264072,1.,1.95296148278133));
#30226=CARTESIAN_POINT('Ctrl Pts',(0.475848034683176,-1.,1.95796111148177));
#30227=CARTESIAN_POINT('Ctrl Pts',(0.475848034683176,1.,1.95796111148177));
#30228=CARTESIAN_POINT('Ctrl Pts',(0.479349583074855,-1.,1.96294933055943));
#30229=CARTESIAN_POINT('Ctrl Pts',(0.479349583074855,1.,1.96294933055943));
#30230=CARTESIAN_POINT('Ctrl Pts',(0.48290166212069,-1.,1.96792703422362));
#30231=CARTESIAN_POINT('Ctrl Pts',(0.48290166212069,1.,1.96792703422362));
#30232=CARTESIAN_POINT('Ctrl Pts',(0.486502692907658,-1.,1.97289186263272));
#30233=CARTESIAN_POINT('Ctrl Pts',(0.486502692907658,1.,1.97289186263272));
#30234=CARTESIAN_POINT('Ctrl Pts',(0.490150627860952,-1.,1.97783973019229));
#30235=CARTESIAN_POINT('Ctrl Pts',(0.490150627860952,1.,1.97783973019229));
#30236=CARTESIAN_POINT('Ctrl Pts',(0.493843476541494,-1.,1.98276658761821));
#30237=CARTESIAN_POINT('Ctrl Pts',(0.493843476541494,1.,1.98276658761821));
#30238=CARTESIAN_POINT('Ctrl Pts',(0.497579909545574,-1.,1.98767044752932));
#30239=CARTESIAN_POINT('Ctrl Pts',(0.497579909545574,1.,1.98767044752932));
#30240=CARTESIAN_POINT('Ctrl Pts',(0.501359287727146,-1.,1.99255149126155));
#30241=CARTESIAN_POINT('Ctrl Pts',(0.501359287727146,1.,1.99255149126155));
#30242=CARTESIAN_POINT('Ctrl Pts',(0.505181361323026,-1.,1.99741107463572));
#30243=CARTESIAN_POINT('Ctrl Pts',(0.505181361323026,1.,1.99741107463572));
#30244=CARTESIAN_POINT('Ctrl Pts',(0.509046069886157,-1.,2.00225107134734));
#30245=CARTESIAN_POINT('Ctrl Pts',(0.509046069886157,1.,2.00225107134734));
#30246=CARTESIAN_POINT('Ctrl Pts',(0.512953306961792,-1.,2.00707309946949));
#30247=CARTESIAN_POINT('Ctrl Pts',(0.512953306961792,1.,2.00707309946949));
#30248=CARTESIAN_POINT('Ctrl Pts',(0.516902681728687,-1.,2.01187773939242));
#30249=CARTESIAN_POINT('Ctrl Pts',(0.516902681728687,1.,2.01187773939242));
#30250=CARTESIAN_POINT('Ctrl Pts',(0.52089359039937,-1.,2.01666477917286));
#30251=CARTESIAN_POINT('Ctrl Pts',(0.52089359039937,1.,2.01666477917286));
#30252=CARTESIAN_POINT('Ctrl Pts',(0.524925318333476,-1.,2.02143356304698));
#30253=CARTESIAN_POINT('Ctrl Pts',(0.524925318333476,1.,2.02143356304698));
#30254=CARTESIAN_POINT('Ctrl Pts',(0.528997127241914,-1.,2.0261832908329));
#30255=CARTESIAN_POINT('Ctrl Pts',(0.528997127241914,1.,2.0261832908329));
#30256=CARTESIAN_POINT('Ctrl Pts',(0.533108355132976,-1.,2.03091336214426));
#30257=CARTESIAN_POINT('Ctrl Pts',(0.533108355132976,1.,2.03091336214426));
#30258=CARTESIAN_POINT('Ctrl Pts',(0.537258489833262,-1.,2.03562362954037));
#30259=CARTESIAN_POINT('Ctrl Pts',(0.537258489833262,1.,2.03562362954037));
#30260=CARTESIAN_POINT('Ctrl Pts',(0.541447120615659,-1.,2.04031422690527));
#30261=CARTESIAN_POINT('Ctrl Pts',(0.541447120615659,1.,2.04031422690527));
#30262=CARTESIAN_POINT('Ctrl Pts',(0.54567390381743,-1.,2.04498544714588));
#30263=CARTESIAN_POINT('Ctrl Pts',(0.54567390381743,1.,2.04498544714588));
#30264=CARTESIAN_POINT('Ctrl Pts',(0.549938525150295,-1.,2.04963761077958));
#30265=CARTESIAN_POINT('Ctrl Pts',(0.549938525150295,1.,2.04963761077958));
#30266=CARTESIAN_POINT('Ctrl Pts',(0.554240657463906,-1.,2.05427091604413));
#30267=CARTESIAN_POINT('Ctrl Pts',(0.554240657463906,1.,2.05427091604413));
#30268=CARTESIAN_POINT('Ctrl Pts',(0.558579940185151,-1.,2.05888537756462));
#30269=CARTESIAN_POINT('Ctrl Pts',(0.558579940185151,1.,2.05888537756462));
#30270=CARTESIAN_POINT('Ctrl Pts',(0.562955993082261,-1.,2.06348090160589));
#30271=CARTESIAN_POINT('Ctrl Pts',(0.562955993082261,1.,2.06348090160589));
#30272=CARTESIAN_POINT('Ctrl Pts',(0.567368421181087,-1.,2.06805732997334));
#30273=CARTESIAN_POINT('Ctrl Pts',(0.567368421181087,1.,2.06805732997334));
#30274=CARTESIAN_POINT('Ctrl Pts',(0.571816823242602,-1.,2.07261449292824));
#30275=CARTESIAN_POINT('Ctrl Pts',(0.571816823242602,1.,2.07261449292824));
#30276=CARTESIAN_POINT('Ctrl Pts',(0.576300797416844,-1.,2.07715226767559));
#30277=CARTESIAN_POINT('Ctrl Pts',(0.576300797416844,1.,2.07715226767559));
#30278=CARTESIAN_POINT('Ctrl Pts',(0.580819952108063,-1.,2.08167059018418));
#30279=CARTESIAN_POINT('Ctrl Pts',(0.580819952108063,1.,2.08167059018418));
#30280=CARTESIAN_POINT('Ctrl Pts',(0.585373918991617,-1.,2.08616943727951));
#30281=CARTESIAN_POINT('Ctrl Pts',(0.585373918991617,1.,2.08616943727951));
#30282=CARTESIAN_POINT('Ctrl Pts',(0.589962365403406,-1.,2.09064881812129));
#30283=CARTESIAN_POINT('Ctrl Pts',(0.589962365403406,1.,2.09064881812129));
#30284=CARTESIAN_POINT('Ctrl Pts',(0.594585006052162,-1.,2.0951087622027));
#30285=CARTESIAN_POINT('Ctrl Pts',(0.594585006052162,1.,2.0951087622027));
#30286=CARTESIAN_POINT('Ctrl Pts',(0.599241616420533,-1.,2.0995493086477));
#30287=CARTESIAN_POINT('Ctrl Pts',(0.599241616420533,1.,2.0995493086477));
#30288=CARTESIAN_POINT('Ctrl Pts',(0.60393203073603,-1.,2.10397049886949));
#30289=CARTESIAN_POINT('Ctrl Pts',(0.60393203073603,1.,2.10397049886949));
#30290=CARTESIAN_POINT('Ctrl Pts',(0.607711315454876,-1.,2.1074919961518));
#30291=CARTESIAN_POINT('Ctrl Pts',(0.607711315454876,1.,2.1074919961518));
#30292=CARTESIAN_POINT('Ctrl Pts',(0.610560911689898,-1.,2.11012443807238));
#30293=CARTESIAN_POINT('Ctrl Pts',(0.610560911689898,1.,2.11012443807238));
#30294=CARTESIAN_POINT('Ctrl Pts',(0.6124673655618,-1.,2.11187554259986));
#30295=CARTESIAN_POINT('Ctrl Pts',(0.6124673655618,1.,2.11187554259986));
#30296=CARTESIAN_POINT('Ctrl Pts',(0.61342227326009,-1.,2.11275013067528));
#30297=CARTESIAN_POINT('Ctrl Pts',(0.61342227326009,1.,2.11275013067528));
#30298=CARTESIAN_POINT('',(0.383122945602004,1.,1.7075470150345));
#30299=CARTESIAN_POINT('Ctrl Pts',(0.383122945602004,1.,1.7075470150345));
#30300=CARTESIAN_POINT('Ctrl Pts',(0.384119047315541,1.,1.71231062891958));
#30301=CARTESIAN_POINT('Ctrl Pts',(0.38607079032701,1.,1.72162022246158));
#30302=CARTESIAN_POINT('Ctrl Pts',(0.388877023509191,1.,1.7349317097561));
#30303=CARTESIAN_POINT('Ctrl Pts',(0.392375812294307,1.,1.75137405313962));
#30304=CARTESIAN_POINT('Ctrl Pts',(0.39634619612042,1.,1.7697556004756));
#30305=CARTESIAN_POINT('Ctrl Pts',(0.39991940378308,1.,1.78598826347533));
#30306=CARTESIAN_POINT('Ctrl Pts',(0.403107976170441,1.,1.80012077176221));
#30307=CARTESIAN_POINT('Ctrl Pts',(0.405933518411838,1.,1.81223801813988));
#30308=CARTESIAN_POINT('Ctrl Pts',(0.408428948108533,1.,1.8224702267854));
#30309=CARTESIAN_POINT('Ctrl Pts',(0.410641256301674,1.,1.83100408895216));
#30310=CARTESIAN_POINT('Ctrl Pts',(0.412633125322161,1.,1.83808953475839));
#30311=CARTESIAN_POINT('Ctrl Pts',(0.41448743825434,1.,1.8440575707371));
#30312=CARTESIAN_POINT('Ctrl Pts',(0.416300022038864,1.,1.84929312929882));
#30313=CARTESIAN_POINT('Ctrl Pts',(0.418164129143534,1.,1.85417632856234));
#30314=CARTESIAN_POINT('Ctrl Pts',(0.420157287975619,1.,1.85903281096686));
#30315=CARTESIAN_POINT('Ctrl Pts',(0.422327307418275,1.,1.86408083334028));
#30316=CARTESIAN_POINT('Ctrl Pts',(0.424678177291358,1.,1.86937803944323));
#30317=CARTESIAN_POINT('Ctrl Pts',(0.427183828519102,1.,1.87486989291484));
#30318=CARTESIAN_POINT('Ctrl Pts',(0.429803062482344,1.,1.88044229001832));
#30319=CARTESIAN_POINT('Ctrl Pts',(0.432493038548748,1.,1.88596913666793));
#30320=CARTESIAN_POINT('Ctrl Pts',(0.435225660963383,1.,1.89136993975504));
#30321=CARTESIAN_POINT('Ctrl Pts',(0.437995003948244,1.,1.89663648956466));
#30322=CARTESIAN_POINT('Ctrl Pts',(0.440807833704038,1.,1.90180124389086));
#30323=CARTESIAN_POINT('Ctrl Pts',(0.44367755684915,1.,1.90691756144898));
#30324=CARTESIAN_POINT('Ctrl Pts',(0.446617343485711,1.,1.9120369998112));
#30325=CARTESIAN_POINT('Ctrl Pts',(0.449632260106662,1.,1.91718342555755));
#30326=CARTESIAN_POINT('Ctrl Pts',(0.452719478359432,1.,1.92235380648502));
#30327=CARTESIAN_POINT('Ctrl Pts',(0.45587200517437,1.,1.92753067150476));
#30328=CARTESIAN_POINT('Ctrl Pts',(0.459081234547926,1.,1.93269066517934));
#30329=CARTESIAN_POINT('Ctrl Pts',(0.462340031009056,1.,1.93781486640821));
#30330=CARTESIAN_POINT('Ctrl Pts',(0.46564546202603,1.,1.9428979419619));
#30331=CARTESIAN_POINT('Ctrl Pts',(0.468997482913135,1.,1.94794381136514));
#30332=CARTESIAN_POINT('Ctrl Pts',(0.472397672264072,1.,1.95296148278133));
#30333=CARTESIAN_POINT('Ctrl Pts',(0.475848034683176,1.,1.95796111148177));
#30334=CARTESIAN_POINT('Ctrl Pts',(0.479349583074855,1.,1.96294933055943));
#30335=CARTESIAN_POINT('Ctrl Pts',(0.48290166212069,1.,1.96792703422362));
#30336=CARTESIAN_POINT('Ctrl Pts',(0.486502692907658,1.,1.97289186263272));
#30337=CARTESIAN_POINT('Ctrl Pts',(0.490150627860952,1.,1.97783973019229));
#30338=CARTESIAN_POINT('Ctrl Pts',(0.493843476541494,1.,1.98276658761821));
#30339=CARTESIAN_POINT('Ctrl Pts',(0.497579909545574,1.,1.98767044752932));
#30340=CARTESIAN_POINT('Ctrl Pts',(0.501359287727146,1.,1.99255149126155));
#30341=CARTESIAN_POINT('Ctrl Pts',(0.505181361323026,1.,1.99741107463572));
#30342=CARTESIAN_POINT('Ctrl Pts',(0.509046069886157,1.,2.00225107134734));
#30343=CARTESIAN_POINT('Ctrl Pts',(0.512953306961792,1.,2.00707309946949));
#30344=CARTESIAN_POINT('Ctrl Pts',(0.516902681728687,1.,2.01187773939242));
#30345=CARTESIAN_POINT('Ctrl Pts',(0.52089359039937,1.,2.01666477917286));
#30346=CARTESIAN_POINT('Ctrl Pts',(0.524925318333476,1.,2.02143356304698));
#30347=CARTESIAN_POINT('Ctrl Pts',(0.528997127241914,1.,2.0261832908329));
#30348=CARTESIAN_POINT('Ctrl Pts',(0.533108355132976,1.,2.03091336214426));
#30349=CARTESIAN_POINT('Ctrl Pts',(0.537258489833262,1.,2.03562362954037));
#30350=CARTESIAN_POINT('Ctrl Pts',(0.541447120615659,1.,2.04031422690527));
#30351=CARTESIAN_POINT('Ctrl Pts',(0.54567390381743,1.,2.04498544714588));
#30352=CARTESIAN_POINT('Ctrl Pts',(0.549938525150295,1.,2.04963761077958));
#30353=CARTESIAN_POINT('Ctrl Pts',(0.554240657463906,1.,2.05427091604413));
#30354=CARTESIAN_POINT('Ctrl Pts',(0.558579940185151,1.,2.05888537756462));
#30355=CARTESIAN_POINT('Ctrl Pts',(0.562955993082261,1.,2.06348090160589));
#30356=CARTESIAN_POINT('Ctrl Pts',(0.567368421181087,1.,2.06805732997334));
#30357=CARTESIAN_POINT('Ctrl Pts',(0.571816823242602,1.,2.07261449292824));
#30358=CARTESIAN_POINT('Ctrl Pts',(0.576300797416844,1.,2.07715226767559));
#30359=CARTESIAN_POINT('Ctrl Pts',(0.580819952108063,1.,2.08167059018418));
#30360=CARTESIAN_POINT('Ctrl Pts',(0.585373918991617,1.,2.08616943727951));
#30361=CARTESIAN_POINT('Ctrl Pts',(0.589962365403406,1.,2.09064881812129));
#30362=CARTESIAN_POINT('Ctrl Pts',(0.594585006052162,1.,2.0951087622027));
#30363=CARTESIAN_POINT('Ctrl Pts',(0.599241616420533,1.,2.0995493086477));
#30364=CARTESIAN_POINT('Ctrl Pts',(0.60393203073603,1.,2.10397049886949));
#30365=CARTESIAN_POINT('Ctrl Pts',(0.607711315454876,1.,2.1074919961518));
#30366=CARTESIAN_POINT('Ctrl Pts',(0.610560911689898,1.,2.11012443807238));
#30367=CARTESIAN_POINT('Ctrl Pts',(0.6124673655618,1.,2.11187554259986));
#30368=CARTESIAN_POINT('Ctrl Pts',(0.61342227326009,1.,2.11275013067528));
#30369=CARTESIAN_POINT('',(0.383122945602003,0.,1.7075470150345));
#30370=CARTESIAN_POINT('Origin',(0.,0.,0.));
#30371=CARTESIAN_POINT('',(0.163289472382896,1.,1.74236521665491));
#30372=CARTESIAN_POINT('Origin',(0.,1.,0.));
#30373=CARTESIAN_POINT('',(0.163289472382896,0.,1.74236521665491));
#30374=CARTESIAN_POINT('Ctrl Pts',(0.0694764450219578,-1.,2.19890268624765));
#30375=CARTESIAN_POINT('Ctrl Pts',(0.0694764450219578,1.,2.19890268624765));
#30376=CARTESIAN_POINT('Ctrl Pts',(0.0701143536325487,-1.,2.19777582085423));
#30377=CARTESIAN_POINT('Ctrl Pts',(0.0701143536325487,1.,2.19777582085423));
#30378=CARTESIAN_POINT('Ctrl Pts',(0.0713863779526151,-1.,2.19552129484002));
#30379=CARTESIAN_POINT('Ctrl Pts',(0.0713863779526151,1.,2.19552129484002));
#30380=CARTESIAN_POINT('Ctrl Pts',(0.0732830357306722,-1.,2.19213712013662));
#30381=CARTESIAN_POINT('Ctrl Pts',(0.0732830357306722,1.,2.19213712013662));
#30382=CARTESIAN_POINT('Ctrl Pts',(0.0757891465836145,-1.,2.1876201139953));
#30383=CARTESIAN_POINT('Ctrl Pts',(0.0757891465836145,1.,2.1876201139953));
#30384=CARTESIAN_POINT('Ctrl Pts',(0.078883772768524,-1.,2.18196589448887));
#30385=CARTESIAN_POINT('Ctrl Pts',(0.078883772768524,1.,2.18196589448887));
#30386=CARTESIAN_POINT('Ctrl Pts',(0.0819402680872763,-1.,2.176303712113));
#30387=CARTESIAN_POINT('Ctrl Pts',(0.0819402680872763,1.,2.176303712113));
#30388=CARTESIAN_POINT('Ctrl Pts',(0.084958462083537,-1.,2.17063357870952));
#30389=CARTESIAN_POINT('Ctrl Pts',(0.084958462083537,1.,2.17063357870952));
#30390=CARTESIAN_POINT('Ctrl Pts',(0.087938129138692,-1.,2.16495552645014));
#30391=CARTESIAN_POINT('Ctrl Pts',(0.087938129138692,1.,2.16495552645014));
#30392=CARTESIAN_POINT('Ctrl Pts',(0.0908789888107263,-1.,2.15926961544516));
#30393=CARTESIAN_POINT('Ctrl Pts',(0.0908789888107263,1.,2.15926961544516));
#30394=CARTESIAN_POINT('Ctrl Pts',(0.0937807218867641,-1.,2.1535759397817));
#30395=CARTESIAN_POINT('Ctrl Pts',(0.0937807218867641,1.,2.1535759397817));
#30396=CARTESIAN_POINT('Ctrl Pts',(0.0966429852305456,-1.,2.14787463531795));
#30397=CARTESIAN_POINT('Ctrl Pts',(0.0966429852305456,1.,2.14787463531795));
#30398=CARTESIAN_POINT('Ctrl Pts',(0.0994654261990913,-1.,2.14216588396025));
#30399=CARTESIAN_POINT('Ctrl Pts',(0.0994654261990913,1.,2.14216588396025));
#30400=CARTESIAN_POINT('Ctrl Pts',(0.1022477005561,-1.,2.13644992667165));
#30401=CARTESIAN_POINT('Ctrl Pts',(0.1022477005561,1.,2.13644992667165));
#30402=CARTESIAN_POINT('Ctrl Pts',(0.104989479152739,-1.,2.13072704887293));
#30403=CARTESIAN_POINT('Ctrl Pts',(0.104989479152739,1.,2.13072704887293));
#30404=CARTESIAN_POINT('Ctrl Pts',(0.10769043523109,-1.,2.12499752307));
#30405=CARTESIAN_POINT('Ctrl Pts',(0.10769043523109,1.,2.12499752307));
#30406=CARTESIAN_POINT('Ctrl Pts',(0.110350236135025,-1.,2.11926155590865));
#30407=CARTESIAN_POINT('Ctrl Pts',(0.110350236135025,1.,2.11926155590865));
#30408=CARTESIAN_POINT('Ctrl Pts',(0.112968534419737,-1.,2.11351924490306));
#30409=CARTESIAN_POINT('Ctrl Pts',(0.112968534419737,1.,2.11351924490306));
#30410=CARTESIAN_POINT('Ctrl Pts',(0.115544957687926,-1.,2.10777050261309));
#30411=CARTESIAN_POINT('Ctrl Pts',(0.115544957687926,1.,2.10777050261309));
#30412=CARTESIAN_POINT('Ctrl Pts',(0.118079107988355,-1.,2.102015121329));
#30413=CARTESIAN_POINT('Ctrl Pts',(0.118079107988355,1.,2.102015121329));
#30414=CARTESIAN_POINT('Ctrl Pts',(0.120570567965122,-1.,2.0962529286773));
#30415=CARTESIAN_POINT('Ctrl Pts',(0.120570567965122,1.,2.0962529286773));
#30416=CARTESIAN_POINT('Ctrl Pts',(0.123018905621083,-1.,2.09048392424825));
#30417=CARTESIAN_POINT('Ctrl Pts',(0.123018905621083,1.,2.09048392424825));
#30418=CARTESIAN_POINT('Ctrl Pts',(0.125423679412061,-1.,2.08470840653643));
#30419=CARTESIAN_POINT('Ctrl Pts',(0.125423679412061,1.,2.08470840653643));
#30420=CARTESIAN_POINT('Ctrl Pts',(0.12778444527612,-1.,2.07892715110987));
#30421=CARTESIAN_POINT('Ctrl Pts',(0.12778444527612,1.,2.07892715110987));
#30422=CARTESIAN_POINT('Ctrl Pts',(0.130100748328403,-1.,2.07314114713063));
#30423=CARTESIAN_POINT('Ctrl Pts',(0.130100748328403,1.,2.07314114713063));
#30424=CARTESIAN_POINT('Ctrl Pts',(0.13237211154771,-1.,2.06735123910326));
#30425=CARTESIAN_POINT('Ctrl Pts',(0.13237211154771,1.,2.06735123910326));
#30426=CARTESIAN_POINT('Ctrl Pts',(0.134598026192106,-1.,2.06155781517842));
#30427=CARTESIAN_POINT('Ctrl Pts',(0.134598026192106,1.,2.06155781517842));
#30428=CARTESIAN_POINT('Ctrl Pts',(0.136777941218043,-1.,2.05576044414264));
#30429=CARTESIAN_POINT('Ctrl Pts',(0.136777941218043,1.,2.05576044414264));
#30430=CARTESIAN_POINT('Ctrl Pts',(0.138911255368966,-1.,2.04995762001328));
#30431=CARTESIAN_POINT('Ctrl Pts',(0.138911255368966,1.,2.04995762001328));
#30432=CARTESIAN_POINT('Ctrl Pts',(0.140997332152546,-1.,2.04414757947916));
#30433=CARTESIAN_POINT('Ctrl Pts',(0.140997332152546,1.,2.04414757947916));
#30434=CARTESIAN_POINT('Ctrl Pts',(0.143035515058208,-1.,2.03832911025912));
#30435=CARTESIAN_POINT('Ctrl Pts',(0.143035515058208,1.,2.03832911025912));
#30436=CARTESIAN_POINT('Ctrl Pts',(0.145025140186057,-1.,2.03250223739942));
#30437=CARTESIAN_POINT('Ctrl Pts',(0.145025140186057,1.,2.03250223739942));
#30438=CARTESIAN_POINT('Ctrl Pts',(0.146965557332583,-1.,2.02666926182017));
#30439=CARTESIAN_POINT('Ctrl Pts',(0.146965557332583,1.,2.02666926182017));
#30440=CARTESIAN_POINT('Ctrl Pts',(0.148856124775337,-1.,2.02083464969894));
#30441=CARTESIAN_POINT('Ctrl Pts',(0.148856124775337,1.,2.02083464969894));
#30442=CARTESIAN_POINT('Ctrl Pts',(0.150696157673078,-1.,2.01500291940238));
#30443=CARTESIAN_POINT('Ctrl Pts',(0.150696157673078,1.,2.01500291940238));
#30444=CARTESIAN_POINT('Ctrl Pts',(0.152484883621449,-1.,2.00917680318424));
#30445=CARTESIAN_POINT('Ctrl Pts',(0.152484883621449,1.,2.00917680318424));
#30446=CARTESIAN_POINT('Ctrl Pts',(0.154221403049722,-1.,2.00335565310543));
#30447=CARTESIAN_POINT('Ctrl Pts',(0.154221403049722,1.,2.00335565310543));
#30448=CARTESIAN_POINT('Ctrl Pts',(0.155904629548783,-1.,1.99753284771497));
#30449=CARTESIAN_POINT('Ctrl Pts',(0.155904629548783,1.,1.99753284771497));
#30450=CARTESIAN_POINT('Ctrl Pts',(0.157533331459227,-1.,1.99169810931908));
#30451=CARTESIAN_POINT('Ctrl Pts',(0.157533331459227,1.,1.99169810931908));
#30452=CARTESIAN_POINT('Ctrl Pts',(0.159106226437299,-1.,1.98584238283292));
#30453=CARTESIAN_POINT('Ctrl Pts',(0.159106226437299,1.,1.98584238283292));
#30454=CARTESIAN_POINT('Ctrl Pts',(0.160622060784611,-1.,1.97996195437559));
#30455=CARTESIAN_POINT('Ctrl Pts',(0.160622060784611,1.,1.97996195437559));
#30456=CARTESIAN_POINT('Ctrl Pts',(0.162079693556288,-1.,1.97406280235188));
#30457=CARTESIAN_POINT('Ctrl Pts',(0.162079693556288,1.,1.97406280235188));
#30458=CARTESIAN_POINT('Ctrl Pts',(0.163478185457734,-1.,1.96816512677967));
#30459=CARTESIAN_POINT('Ctrl Pts',(0.163478185457734,1.,1.96816512677967));
#30460=CARTESIAN_POINT('Ctrl Pts',(0.164816568920269,-1.,1.96229379940136));
#30461=CARTESIAN_POINT('Ctrl Pts',(0.164816568920269,1.,1.96229379940136));
#30462=CARTESIAN_POINT('Ctrl Pts',(0.166093592002812,-1.,1.9564675971873));
#30463=CARTESIAN_POINT('Ctrl Pts',(0.166093592002812,1.,1.9564675971873));
#30464=CARTESIAN_POINT('Ctrl Pts',(0.167307501784475,-1.,1.95069027794294));
#30465=CARTESIAN_POINT('Ctrl Pts',(0.167307501784475,1.,1.95069027794294));
#30466=CARTESIAN_POINT('Ctrl Pts',(0.168455741607556,-1.,1.94493757756931));
#30467=CARTESIAN_POINT('Ctrl Pts',(0.168455741607556,1.,1.94493757756931));
#30468=CARTESIAN_POINT('Ctrl Pts',(0.16953490481749,-1.,1.93915639211581));
#30469=CARTESIAN_POINT('Ctrl Pts',(0.16953490481749,1.,1.93915639211581));
#30470=CARTESIAN_POINT('Ctrl Pts',(0.170541253116201,-1.,1.93329183155539));
#30471=CARTESIAN_POINT('Ctrl Pts',(0.170541253116201,1.,1.93329183155539));
#30472=CARTESIAN_POINT('Ctrl Pts',(0.171471191532988,-1.,1.92731093582036));
#30473=CARTESIAN_POINT('Ctrl Pts',(0.171471191532988,1.,1.92731093582036));
#30474=CARTESIAN_POINT('Ctrl Pts',(0.172321621259513,-1.,1.9212233439798));
#30475=CARTESIAN_POINT('Ctrl Pts',(0.172321621259513,1.,1.9212233439798));
#30476=CARTESIAN_POINT('Ctrl Pts',(0.173090695383496,-1.,1.91511429159527));
#30477=CARTESIAN_POINT('Ctrl Pts',(0.173090695383496,1.,1.91511429159527));
#30478=CARTESIAN_POINT('Ctrl Pts',(0.173776635257816,-1.,1.90911693975267));
#30479=CARTESIAN_POINT('Ctrl Pts',(0.173776635257816,1.,1.90911693975267));
#30480=CARTESIAN_POINT('Ctrl Pts',(0.174375518661085,-1.,1.90335253862834));
#30481=CARTESIAN_POINT('Ctrl Pts',(0.174375518661085,1.,1.90335253862834));
#30482=CARTESIAN_POINT('Ctrl Pts',(0.174879405091263,-1.,1.89788101117132));
#30483=CARTESIAN_POINT('Ctrl Pts',(0.174879405091263,1.,1.89788101117132));
#30484=CARTESIAN_POINT('Ctrl Pts',(0.175274276190844,-1.,1.892646301985));
#30485=CARTESIAN_POINT('Ctrl Pts',(0.175274276190844,1.,1.892646301985));
#30486=CARTESIAN_POINT('Ctrl Pts',(0.175538155840648,-1.,1.88742606273259));
#30487=CARTESIAN_POINT('Ctrl Pts',(0.175538155840648,1.,1.88742606273259));
#30488=CARTESIAN_POINT('Ctrl Pts',(0.175644148889698,-1.,1.88188663145367));
#30489=CARTESIAN_POINT('Ctrl Pts',(0.175644148889698,1.,1.88188663145367));
#30490=CARTESIAN_POINT('Ctrl Pts',(0.175563480746485,-1.,1.87563767773588));
#30491=CARTESIAN_POINT('Ctrl Pts',(0.175563480746485,1.,1.87563767773588));
#30492=CARTESIAN_POINT('Ctrl Pts',(0.175268337590757,-1.,1.86828349694799));
#30493=CARTESIAN_POINT('Ctrl Pts',(0.175268337590757,1.,1.86828349694799));
#30494=CARTESIAN_POINT('Ctrl Pts',(0.17473525927603,-1.,1.85948367088837));
#30495=CARTESIAN_POINT('Ctrl Pts',(0.17473525927603,1.,1.85948367088837));
#30496=CARTESIAN_POINT('Ctrl Pts',(0.173946627587731,-1.,1.8489811319852));
#30497=CARTESIAN_POINT('Ctrl Pts',(0.173946627587731,1.,1.8489811319852));
#30498=CARTESIAN_POINT('Ctrl Pts',(0.1728894428919,-1.,1.83658380527692));
#30499=CARTESIAN_POINT('Ctrl Pts',(0.1728894428919,1.,1.83658380527692));
#30500=CARTESIAN_POINT('Ctrl Pts',(0.171554770204119,-1.,1.82215766811545));
#30501=CARTESIAN_POINT('Ctrl Pts',(0.171554770204119,1.,1.82215766811545));
#30502=CARTESIAN_POINT('Ctrl Pts',(0.169936923904608,-1.,1.80561530629706));
#30503=CARTESIAN_POINT('Ctrl Pts',(0.169936923904608,1.,1.80561530629706));
#30504=CARTESIAN_POINT('Ctrl Pts',(0.168032772805197,-1.,1.7869064998507));
#30505=CARTESIAN_POINT('Ctrl Pts',(0.168032772805197,1.,1.7869064998507));
#30506=CARTESIAN_POINT('Ctrl Pts',(0.1662793551464,-1.,1.77018771684844));
#30507=CARTESIAN_POINT('Ctrl Pts',(0.1662793551464,1.,1.77018771684844));
#30508=CARTESIAN_POINT('Ctrl Pts',(0.164834765707158,-1.,1.75666056638427));
#30509=CARTESIAN_POINT('Ctrl Pts',(0.164834765707158,1.,1.75666056638427));
#30510=CARTESIAN_POINT('Ctrl Pts',(0.163814161002002,-1.,1.7472034950333));
#30511=CARTESIAN_POINT('Ctrl Pts',(0.163814161002002,1.,1.7472034950333));
#30512=CARTESIAN_POINT('Ctrl Pts',(0.163289472382896,-1.,1.74236521665491));
#30513=CARTESIAN_POINT('Ctrl Pts',(0.163289472382896,1.,1.74236521665491));
#30514=CARTESIAN_POINT('',(0.0694764450219578,1.,2.19890268624765));
#30515=CARTESIAN_POINT('Ctrl Pts',(0.0694764450219578,1.,2.19890268624765));
#30516=CARTESIAN_POINT('Ctrl Pts',(0.0701143536325487,1.,2.19777582085423));
#30517=CARTESIAN_POINT('Ctrl Pts',(0.0713863779526151,1.,2.19552129484002));
#30518=CARTESIAN_POINT('Ctrl Pts',(0.0732830357306722,1.,2.19213712013662));
#30519=CARTESIAN_POINT('Ctrl Pts',(0.0757891465836145,1.,2.1876201139953));
#30520=CARTESIAN_POINT('Ctrl Pts',(0.078883772768524,1.,2.18196589448887));
#30521=CARTESIAN_POINT('Ctrl Pts',(0.0819402680872763,1.,2.176303712113));
#30522=CARTESIAN_POINT('Ctrl Pts',(0.084958462083537,1.,2.17063357870952));
#30523=CARTESIAN_POINT('Ctrl Pts',(0.087938129138692,1.,2.16495552645014));
#30524=CARTESIAN_POINT('Ctrl Pts',(0.0908789888107263,1.,2.15926961544516));
#30525=CARTESIAN_POINT('Ctrl Pts',(0.0937807218867641,1.,2.1535759397817));
#30526=CARTESIAN_POINT('Ctrl Pts',(0.0966429852305456,1.,2.14787463531795));
#30527=CARTESIAN_POINT('Ctrl Pts',(0.0994654261990913,1.,2.14216588396025));
#30528=CARTESIAN_POINT('Ctrl Pts',(0.1022477005561,1.,2.13644992667165));
#30529=CARTESIAN_POINT('Ctrl Pts',(0.104989479152739,1.,2.13072704887293));
#30530=CARTESIAN_POINT('Ctrl Pts',(0.10769043523109,1.,2.12499752307));
#30531=CARTESIAN_POINT('Ctrl Pts',(0.110350236135025,1.,2.11926155590865));
#30532=CARTESIAN_POINT('Ctrl Pts',(0.112968534419737,1.,2.11351924490306));
#30533=CARTESIAN_POINT('Ctrl Pts',(0.115544957687926,1.,2.10777050261309));
#30534=CARTESIAN_POINT('Ctrl Pts',(0.118079107988355,1.,2.102015121329));
#30535=CARTESIAN_POINT('Ctrl Pts',(0.120570567965122,1.,2.0962529286773));
#30536=CARTESIAN_POINT('Ctrl Pts',(0.123018905621083,1.,2.09048392424825));
#30537=CARTESIAN_POINT('Ctrl Pts',(0.125423679412061,1.,2.08470840653643));
#30538=CARTESIAN_POINT('Ctrl Pts',(0.12778444527612,1.,2.07892715110987));
#30539=CARTESIAN_POINT('Ctrl Pts',(0.130100748328403,1.,2.07314114713063));
#30540=CARTESIAN_POINT('Ctrl Pts',(0.13237211154771,1.,2.06735123910326));
#30541=CARTESIAN_POINT('Ctrl Pts',(0.134598026192106,1.,2.06155781517842));
#30542=CARTESIAN_POINT('Ctrl Pts',(0.136777941218043,1.,2.05576044414264));
#30543=CARTESIAN_POINT('Ctrl Pts',(0.138911255368966,1.,2.04995762001328));
#30544=CARTESIAN_POINT('Ctrl Pts',(0.140997332152546,1.,2.04414757947916));
#30545=CARTESIAN_POINT('Ctrl Pts',(0.143035515058208,1.,2.03832911025912));
#30546=CARTESIAN_POINT('Ctrl Pts',(0.145025140186057,1.,2.03250223739942));
#30547=CARTESIAN_POINT('Ctrl Pts',(0.146965557332583,1.,2.02666926182017));
#30548=CARTESIAN_POINT('Ctrl Pts',(0.148856124775337,1.,2.02083464969894));
#30549=CARTESIAN_POINT('Ctrl Pts',(0.150696157673078,1.,2.01500291940238));
#30550=CARTESIAN_POINT('Ctrl Pts',(0.152484883621449,1.,2.00917680318424));
#30551=CARTESIAN_POINT('Ctrl Pts',(0.154221403049722,1.,2.00335565310543));
#30552=CARTESIAN_POINT('Ctrl Pts',(0.155904629548783,1.,1.99753284771497));
#30553=CARTESIAN_POINT('Ctrl Pts',(0.157533331459227,1.,1.99169810931908));
#30554=CARTESIAN_POINT('Ctrl Pts',(0.159106226437299,1.,1.98584238283292));
#30555=CARTESIAN_POINT('Ctrl Pts',(0.160622060784611,1.,1.97996195437559));
#30556=CARTESIAN_POINT('Ctrl Pts',(0.162079693556288,1.,1.97406280235188));
#30557=CARTESIAN_POINT('Ctrl Pts',(0.163478185457734,1.,1.96816512677967));
#30558=CARTESIAN_POINT('Ctrl Pts',(0.164816568920269,1.,1.96229379940136));
#30559=CARTESIAN_POINT('Ctrl Pts',(0.166093592002812,1.,1.9564675971873));
#30560=CARTESIAN_POINT('Ctrl Pts',(0.167307501784475,1.,1.95069027794294));
#30561=CARTESIAN_POINT('Ctrl Pts',(0.168455741607556,1.,1.94493757756931));
#30562=CARTESIAN_POINT('Ctrl Pts',(0.16953490481749,1.,1.93915639211581));
#30563=CARTESIAN_POINT('Ctrl Pts',(0.170541253116201,1.,1.93329183155539));
#30564=CARTESIAN_POINT('Ctrl Pts',(0.171471191532988,1.,1.92731093582036));
#30565=CARTESIAN_POINT('Ctrl Pts',(0.172321621259513,1.,1.9212233439798));
#30566=CARTESIAN_POINT('Ctrl Pts',(0.173090695383496,1.,1.91511429159527));
#30567=CARTESIAN_POINT('Ctrl Pts',(0.173776635257816,1.,1.90911693975267));
#30568=CARTESIAN_POINT('Ctrl Pts',(0.174375518661085,1.,1.90335253862834));
#30569=CARTESIAN_POINT('Ctrl Pts',(0.174879405091263,1.,1.89788101117132));
#30570=CARTESIAN_POINT('Ctrl Pts',(0.175274276190844,1.,1.892646301985));
#30571=CARTESIAN_POINT('Ctrl Pts',(0.175538155840648,1.,1.88742606273259));
#30572=CARTESIAN_POINT('Ctrl Pts',(0.175644148889698,1.,1.88188663145367));
#30573=CARTESIAN_POINT('Ctrl Pts',(0.175563480746485,1.,1.87563767773588));
#30574=CARTESIAN_POINT('Ctrl Pts',(0.175268337590757,1.,1.86828349694799));
#30575=CARTESIAN_POINT('Ctrl Pts',(0.17473525927603,1.,1.85948367088837));
#30576=CARTESIAN_POINT('Ctrl Pts',(0.173946627587731,1.,1.8489811319852));
#30577=CARTESIAN_POINT('Ctrl Pts',(0.1728894428919,1.,1.83658380527692));
#30578=CARTESIAN_POINT('Ctrl Pts',(0.171554770204119,1.,1.82215766811545));
#30579=CARTESIAN_POINT('Ctrl Pts',(0.169936923904608,1.,1.80561530629706));
#30580=CARTESIAN_POINT('Ctrl Pts',(0.168032772805197,1.,1.7869064998507));
#30581=CARTESIAN_POINT('Ctrl Pts',(0.1662793551464,1.,1.77018771684844));
#30582=CARTESIAN_POINT('Ctrl Pts',(0.164834765707158,1.,1.75666056638427));
#30583=CARTESIAN_POINT('Ctrl Pts',(0.163814161002002,1.,1.7472034950333));
#30584=CARTESIAN_POINT('Ctrl Pts',(0.163289472382896,1.,1.74236521665491));
#30585=CARTESIAN_POINT('',(0.0694764450219578,0.,2.19890268624765));
#30586=CARTESIAN_POINT('Origin',(-0.0694764450219586,0.,2.19890268624765));
#30587=CARTESIAN_POINT('',(-0.0694764450219586,1.,2.19890268624765));
#30588=CARTESIAN_POINT('',(0.0694764450219578,1.,2.19890268624765));
#30589=CARTESIAN_POINT('',(-0.0694764450219586,0.,2.19890268624765));
#30590=CARTESIAN_POINT('Ctrl Pts',(-0.163289472382896,-1.,1.74236521665491));
#30591=CARTESIAN_POINT('Ctrl Pts',(-0.163289472382896,1.,1.74236521665491));
#30592=CARTESIAN_POINT('Ctrl Pts',(-0.163814161002474,-1.,1.74720349503904));
#30593=CARTESIAN_POINT('Ctrl Pts',(-0.163814161002474,1.,1.74720349503904));
#30594=CARTESIAN_POINT('Ctrl Pts',(-0.164834765708484,-1.,1.75666056640041));
#30595=CARTESIAN_POINT('Ctrl Pts',(-0.164834765708484,1.,1.75666056640041));
#30596=CARTESIAN_POINT('Ctrl Pts',(-0.166279355148738,-1.,1.77018771687692));
#30597=CARTESIAN_POINT('Ctrl Pts',(-0.166279355148738,1.,1.77018771687692));
#30598=CARTESIAN_POINT('Ctrl Pts',(-0.16803277280837,-1.,1.78690649988931));
#30599=CARTESIAN_POINT('Ctrl Pts',(-0.16803277280837,1.,1.78690649988931));
#30600=CARTESIAN_POINT('Ctrl Pts',(-0.169936923908078,-1.,1.80561530633924));
#30601=CARTESIAN_POINT('Ctrl Pts',(-0.169936923908078,1.,1.80561530633924));
#30602=CARTESIAN_POINT('Ctrl Pts',(-0.171554770207306,-1.,1.82215766815414));
#30603=CARTESIAN_POINT('Ctrl Pts',(-0.171554770207306,1.,1.82215766815414));
#30604=CARTESIAN_POINT('Ctrl Pts',(-0.17288944289442,-1.,1.83658380530747));
#30605=CARTESIAN_POINT('Ctrl Pts',(-0.17288944289442,1.,1.83658380530747));
#30606=CARTESIAN_POINT('Ctrl Pts',(-0.173946627589401,-1.,1.84898113200543));
#30607=CARTESIAN_POINT('Ctrl Pts',(-0.173946627589401,1.,1.84898113200543));
#30608=CARTESIAN_POINT('Ctrl Pts',(-0.174735259276856,-1.,1.85948367089838));
#30609=CARTESIAN_POINT('Ctrl Pts',(-0.174735259276856,1.,1.85948367089838));
#30610=CARTESIAN_POINT('Ctrl Pts',(-0.175268337590901,-1.,1.86828349694972));
#30611=CARTESIAN_POINT('Ctrl Pts',(-0.175268337590901,1.,1.86828349694972));
#30612=CARTESIAN_POINT('Ctrl Pts',(-0.175563480746206,-1.,1.87563767773249));
#30613=CARTESIAN_POINT('Ctrl Pts',(-0.175563480746206,1.,1.87563767773249));
#30614=CARTESIAN_POINT('Ctrl Pts',(-0.175644148889271,-1.,1.88188663144846));
#30615=CARTESIAN_POINT('Ctrl Pts',(-0.175644148889271,1.,1.88188663144846));
#30616=CARTESIAN_POINT('Ctrl Pts',(-0.175538155840286,-1.,1.88742606272818));
#30617=CARTESIAN_POINT('Ctrl Pts',(-0.175538155840286,1.,1.88742606272818));
#30618=CARTESIAN_POINT('Ctrl Pts',(-0.175274276190664,-1.,1.89264630198279));
#30619=CARTESIAN_POINT('Ctrl Pts',(-0.175274276190664,1.,1.89264630198279));
#30620=CARTESIAN_POINT('Ctrl Pts',(-0.174879405091277,-1.,1.89788101117148));
#30621=CARTESIAN_POINT('Ctrl Pts',(-0.174879405091277,1.,1.89788101117148));
#30622=CARTESIAN_POINT('Ctrl Pts',(-0.174375518661222,-1.,1.90335253863003));
#30623=CARTESIAN_POINT('Ctrl Pts',(-0.174375518661222,1.,1.90335253863003));
#30624=CARTESIAN_POINT('Ctrl Pts',(-0.173776635257984,-1.,1.90911693975475));
#30625=CARTESIAN_POINT('Ctrl Pts',(-0.173776635257984,1.,1.90911693975475));
#30626=CARTESIAN_POINT('Ctrl Pts',(-0.173090695383619,-1.,1.91511429159681));
#30627=CARTESIAN_POINT('Ctrl Pts',(-0.173090695383619,1.,1.91511429159681));
#30628=CARTESIAN_POINT('Ctrl Pts',(-0.172321621259557,-1.,1.92122334398034));
#30629=CARTESIAN_POINT('Ctrl Pts',(-0.172321621259557,1.,1.92122334398034));
#30630=CARTESIAN_POINT('Ctrl Pts',(-0.17147119153296,-1.,1.92731093582));
#30631=CARTESIAN_POINT('Ctrl Pts',(-0.17147119153296,1.,1.92731093582));
#30632=CARTESIAN_POINT('Ctrl Pts',(-0.170541253116136,-1.,1.93329183155455));
#30633=CARTESIAN_POINT('Ctrl Pts',(-0.170541253116136,1.,1.93329183155455));
#30634=CARTESIAN_POINT('Ctrl Pts',(-0.169534904817425,-1.,1.93915639211497));
#30635=CARTESIAN_POINT('Ctrl Pts',(-0.169534904817425,1.,1.93915639211497));
#30636=CARTESIAN_POINT('Ctrl Pts',(-0.168455741607516,-1.,1.94493757756879));
#30637=CARTESIAN_POINT('Ctrl Pts',(-0.168455741607516,1.,1.94493757756879));
#30638=CARTESIAN_POINT('Ctrl Pts',(-0.167307501784469,-1.,1.95069027794286));
#30639=CARTESIAN_POINT('Ctrl Pts',(-0.167307501784469,1.,1.95069027794286));
#30640=CARTESIAN_POINT('Ctrl Pts',(-0.166093592002833,-1.,1.95646759718755));
#30641=CARTESIAN_POINT('Ctrl Pts',(-0.166093592002833,1.,1.95646759718755));
#30642=CARTESIAN_POINT('Ctrl Pts',(-0.1648165689203,-1.,1.96229379940174));
#30643=CARTESIAN_POINT('Ctrl Pts',(-0.1648165689203,1.,1.96229379940174));
#30644=CARTESIAN_POINT('Ctrl Pts',(-0.16347818545776,-1.,1.96816512678));
#30645=CARTESIAN_POINT('Ctrl Pts',(-0.16347818545776,1.,1.96816512678));
#30646=CARTESIAN_POINT('Ctrl Pts',(-0.162079693556302,-1.,1.97406280235204));
#30647=CARTESIAN_POINT('Ctrl Pts',(-0.162079693556302,1.,1.97406280235204));
#30648=CARTESIAN_POINT('Ctrl Pts',(-0.16062206078461,-1.,1.97996195437557));
#30649=CARTESIAN_POINT('Ctrl Pts',(-0.16062206078461,1.,1.97996195437557));
#30650=CARTESIAN_POINT('Ctrl Pts',(-0.159106226437289,-1.,1.98584238283279));
#30651=CARTESIAN_POINT('Ctrl Pts',(-0.159106226437289,1.,1.98584238283279));
#30652=CARTESIAN_POINT('Ctrl Pts',(-0.157533331459215,-1.,1.99169810931893));
#30653=CARTESIAN_POINT('Ctrl Pts',(-0.157533331459215,1.,1.99169810931893));
#30654=CARTESIAN_POINT('Ctrl Pts',(-0.155904629548775,-1.,1.99753284771487));
#30655=CARTESIAN_POINT('Ctrl Pts',(-0.155904629548775,1.,1.99753284771487));
#30656=CARTESIAN_POINT('Ctrl Pts',(-0.154221403049719,-1.,2.00335565310539));
#30657=CARTESIAN_POINT('Ctrl Pts',(-0.154221403049719,1.,2.00335565310539));
#30658=CARTESIAN_POINT('Ctrl Pts',(-0.152484883621452,-1.,2.00917680318426));
#30659=CARTESIAN_POINT('Ctrl Pts',(-0.152484883621452,1.,2.00917680318426));
#30660=CARTESIAN_POINT('Ctrl Pts',(-0.150696157673084,-1.,2.01500291940243));
#30661=CARTESIAN_POINT('Ctrl Pts',(-0.150696157673084,1.,2.01500291940243));
#30662=CARTESIAN_POINT('Ctrl Pts',(-0.148856124775343,-1.,2.02083464969897));
#30663=CARTESIAN_POINT('Ctrl Pts',(-0.148856124775343,1.,2.02083464969897));
#30664=CARTESIAN_POINT('Ctrl Pts',(-0.146965557332586,-1.,2.02666926182017));
#30665=CARTESIAN_POINT('Ctrl Pts',(-0.146965557332586,1.,2.02666926182017));
#30666=CARTESIAN_POINT('Ctrl Pts',(-0.145025140186058,-1.,2.03250223739941));
#30667=CARTESIAN_POINT('Ctrl Pts',(-0.145025140186058,1.,2.03250223739941));
#30668=CARTESIAN_POINT('Ctrl Pts',(-0.143035515058208,-1.,2.03832911025913));
#30669=CARTESIAN_POINT('Ctrl Pts',(-0.143035515058208,1.,2.03832911025913));
#30670=CARTESIAN_POINT('Ctrl Pts',(-0.140997332152546,-1.,2.04414757947919));
#30671=CARTESIAN_POINT('Ctrl Pts',(-0.140997332152546,1.,2.04414757947919));
#30672=CARTESIAN_POINT('Ctrl Pts',(-0.138911255368966,-1.,2.04995762001333));
#30673=CARTESIAN_POINT('Ctrl Pts',(-0.138911255368966,1.,2.04995762001333));
#30674=CARTESIAN_POINT('Ctrl Pts',(-0.136777941218044,-1.,2.0557604441427));
#30675=CARTESIAN_POINT('Ctrl Pts',(-0.136777941218044,1.,2.0557604441427));
#30676=CARTESIAN_POINT('Ctrl Pts',(-0.134598026192107,-1.,2.06155781517844));
#30677=CARTESIAN_POINT('Ctrl Pts',(-0.134598026192107,1.,2.06155781517844));
#30678=CARTESIAN_POINT('Ctrl Pts',(-0.13237211154771,-1.,2.06735123910319));
#30679=CARTESIAN_POINT('Ctrl Pts',(-0.13237211154771,1.,2.06735123910319));
#30680=CARTESIAN_POINT('Ctrl Pts',(-0.130100748328401,-1.,2.07314114713047));
#30681=CARTESIAN_POINT('Ctrl Pts',(-0.130100748328401,1.,2.07314114713047));
#30682=CARTESIAN_POINT('Ctrl Pts',(-0.127784445276116,-1.,2.07892715110967));
#30683=CARTESIAN_POINT('Ctrl Pts',(-0.127784445276116,1.,2.07892715110967));
#30684=CARTESIAN_POINT('Ctrl Pts',(-0.125423679412058,-1.,2.08470840653628));
#30685=CARTESIAN_POINT('Ctrl Pts',(-0.125423679412058,1.,2.08470840653628));
#30686=CARTESIAN_POINT('Ctrl Pts',(-0.123018905621083,-1.,2.09048392424826));
#30687=CARTESIAN_POINT('Ctrl Pts',(-0.123018905621083,1.,2.09048392424826));
#30688=CARTESIAN_POINT('Ctrl Pts',(-0.120570567965129,-1.,2.09625292867756));
#30689=CARTESIAN_POINT('Ctrl Pts',(-0.120570567965129,1.,2.09625292867756));
#30690=CARTESIAN_POINT('Ctrl Pts',(-0.118079107988368,-1.,2.10201512132945));
#30691=CARTESIAN_POINT('Ctrl Pts',(-0.118079107988368,1.,2.10201512132945));
#30692=CARTESIAN_POINT('Ctrl Pts',(-0.115544957687941,-1.,2.10777050261359));
#30693=CARTESIAN_POINT('Ctrl Pts',(-0.115544957687941,1.,2.10777050261359));
#30694=CARTESIAN_POINT('Ctrl Pts',(-0.112968534419746,-1.,2.11351924490335));
#30695=CARTESIAN_POINT('Ctrl Pts',(-0.112968534419746,1.,2.11351924490335));
#30696=CARTESIAN_POINT('Ctrl Pts',(-0.11035023613502,-1.,2.11926155590849));
#30697=CARTESIAN_POINT('Ctrl Pts',(-0.11035023613502,1.,2.11926155590849));
#30698=CARTESIAN_POINT('Ctrl Pts',(-0.107690435231068,-1.,2.12499752306927));
#30699=CARTESIAN_POINT('Ctrl Pts',(-0.107690435231068,1.,2.12499752306927));
#30700=CARTESIAN_POINT('Ctrl Pts',(-0.104989479152703,-1.,2.1307270488718));
#30701=CARTESIAN_POINT('Ctrl Pts',(-0.104989479152703,1.,2.1307270488718));
#30702=CARTESIAN_POINT('Ctrl Pts',(-0.102247700556064,-1.,2.13644992667052));
#30703=CARTESIAN_POINT('Ctrl Pts',(-0.102247700556064,1.,2.13644992667052));
#30704=CARTESIAN_POINT('Ctrl Pts',(-0.0994654261990745,-1.,2.14216588395974));
#30705=CARTESIAN_POINT('Ctrl Pts',(-0.0994654261990745,1.,2.14216588395974));
#30706=CARTESIAN_POINT('Ctrl Pts',(-0.0966429852305691,-1.,2.14787463531864));
#30707=CARTESIAN_POINT('Ctrl Pts',(-0.0966429852305691,1.,2.14787463531864));
#30708=CARTESIAN_POINT('Ctrl Pts',(-0.0937807218868348,-1.,2.15357593978377));
#30709=CARTESIAN_POINT('Ctrl Pts',(-0.0937807218868348,1.,2.15357593978377));
#30710=CARTESIAN_POINT('Ctrl Pts',(-0.0908789888108269,-1.,2.15926961544808));
#30711=CARTESIAN_POINT('Ctrl Pts',(-0.0908789888108269,1.,2.15926961544808));
#30712=CARTESIAN_POINT('Ctrl Pts',(-0.0879381291387825,-1.,2.16495552645275));
#30713=CARTESIAN_POINT('Ctrl Pts',(-0.0879381291387825,1.,2.16495552645275));
#30714=CARTESIAN_POINT('Ctrl Pts',(-0.0849584620835646,-1.,2.17063357871031));
#30715=CARTESIAN_POINT('Ctrl Pts',(-0.0849584620835646,1.,2.17063357871031));
#30716=CARTESIAN_POINT('Ctrl Pts',(-0.0819402680871942,-1.,2.1763037121106));
#30717=CARTESIAN_POINT('Ctrl Pts',(-0.0819402680871942,1.,2.1763037121106));
#30718=CARTESIAN_POINT('Ctrl Pts',(-0.078883772768323,-1.,2.18196589448304));
#30719=CARTESIAN_POINT('Ctrl Pts',(-0.078883772768323,1.,2.18196589448304));
#30720=CARTESIAN_POINT('Ctrl Pts',(-0.0757891465833414,-1.,2.1876201139874));
#30721=CARTESIAN_POINT('Ctrl Pts',(-0.0757891465833414,1.,2.1876201139874));
#30722=CARTESIAN_POINT('Ctrl Pts',(-0.0732830357304279,-1.,2.19213712012956));
#30723=CARTESIAN_POINT('Ctrl Pts',(-0.0732830357304279,1.,2.19213712012956));
#30724=CARTESIAN_POINT('Ctrl Pts',(-0.071386377952463,-1.,2.19552129483562));
#30725=CARTESIAN_POINT('Ctrl Pts',(-0.071386377952463,1.,2.19552129483562));
#30726=CARTESIAN_POINT('Ctrl Pts',(-0.0701143536324929,-1.,2.19777582085261));
#30727=CARTESIAN_POINT('Ctrl Pts',(-0.0701143536324929,1.,2.19777582085261));
#30728=CARTESIAN_POINT('Ctrl Pts',(-0.0694764450219586,-1.,2.19890268624765));
#30729=CARTESIAN_POINT('Ctrl Pts',(-0.0694764450219586,1.,2.19890268624765));
#30730=CARTESIAN_POINT('',(-0.163289472382896,1.,1.74236521665491));
#30731=CARTESIAN_POINT('Ctrl Pts',(-0.163289472382896,1.,1.74236521665491));
#30732=CARTESIAN_POINT('Ctrl Pts',(-0.163814161002474,1.,1.74720349503904));
#30733=CARTESIAN_POINT('Ctrl Pts',(-0.164834765708484,1.,1.75666056640041));
#30734=CARTESIAN_POINT('Ctrl Pts',(-0.166279355148738,1.,1.77018771687692));
#30735=CARTESIAN_POINT('Ctrl Pts',(-0.16803277280837,1.,1.78690649988931));
#30736=CARTESIAN_POINT('Ctrl Pts',(-0.169936923908078,1.,1.80561530633924));
#30737=CARTESIAN_POINT('Ctrl Pts',(-0.171554770207306,1.,1.82215766815414));
#30738=CARTESIAN_POINT('Ctrl Pts',(-0.17288944289442,1.,1.83658380530747));
#30739=CARTESIAN_POINT('Ctrl Pts',(-0.173946627589401,1.,1.84898113200543));
#30740=CARTESIAN_POINT('Ctrl Pts',(-0.174735259276856,1.,1.85948367089838));
#30741=CARTESIAN_POINT('Ctrl Pts',(-0.175268337590901,1.,1.86828349694972));
#30742=CARTESIAN_POINT('Ctrl Pts',(-0.175563480746206,1.,1.87563767773249));
#30743=CARTESIAN_POINT('Ctrl Pts',(-0.175644148889271,1.,1.88188663144846));
#30744=CARTESIAN_POINT('Ctrl Pts',(-0.175538155840286,1.,1.88742606272818));
#30745=CARTESIAN_POINT('Ctrl Pts',(-0.175274276190664,1.,1.89264630198279));
#30746=CARTESIAN_POINT('Ctrl Pts',(-0.174879405091277,1.,1.89788101117148));
#30747=CARTESIAN_POINT('Ctrl Pts',(-0.174375518661222,1.,1.90335253863003));
#30748=CARTESIAN_POINT('Ctrl Pts',(-0.173776635257984,1.,1.90911693975475));
#30749=CARTESIAN_POINT('Ctrl Pts',(-0.173090695383619,1.,1.91511429159681));
#30750=CARTESIAN_POINT('Ctrl Pts',(-0.172321621259557,1.,1.92122334398034));
#30751=CARTESIAN_POINT('Ctrl Pts',(-0.17147119153296,1.,1.92731093582));
#30752=CARTESIAN_POINT('Ctrl Pts',(-0.170541253116136,1.,1.93329183155455));
#30753=CARTESIAN_POINT('Ctrl Pts',(-0.169534904817425,1.,1.93915639211497));
#30754=CARTESIAN_POINT('Ctrl Pts',(-0.168455741607516,1.,1.94493757756879));
#30755=CARTESIAN_POINT('Ctrl Pts',(-0.167307501784469,1.,1.95069027794286));
#30756=CARTESIAN_POINT('Ctrl Pts',(-0.166093592002833,1.,1.95646759718755));
#30757=CARTESIAN_POINT('Ctrl Pts',(-0.1648165689203,1.,1.96229379940174));
#30758=CARTESIAN_POINT('Ctrl Pts',(-0.16347818545776,1.,1.96816512678));
#30759=CARTESIAN_POINT('Ctrl Pts',(-0.162079693556302,1.,1.97406280235204));
#30760=CARTESIAN_POINT('Ctrl Pts',(-0.16062206078461,1.,1.97996195437557));
#30761=CARTESIAN_POINT('Ctrl Pts',(-0.159106226437289,1.,1.98584238283279));
#30762=CARTESIAN_POINT('Ctrl Pts',(-0.157533331459215,1.,1.99169810931893));
#30763=CARTESIAN_POINT('Ctrl Pts',(-0.155904629548775,1.,1.99753284771487));
#30764=CARTESIAN_POINT('Ctrl Pts',(-0.154221403049719,1.,2.00335565310539));
#30765=CARTESIAN_POINT('Ctrl Pts',(-0.152484883621452,1.,2.00917680318426));
#30766=CARTESIAN_POINT('Ctrl Pts',(-0.150696157673084,1.,2.01500291940243));
#30767=CARTESIAN_POINT('Ctrl Pts',(-0.148856124775343,1.,2.02083464969897));
#30768=CARTESIAN_POINT('Ctrl Pts',(-0.146965557332586,1.,2.02666926182017));
#30769=CARTESIAN_POINT('Ctrl Pts',(-0.145025140186058,1.,2.03250223739941));
#30770=CARTESIAN_POINT('Ctrl Pts',(-0.143035515058208,1.,2.03832911025913));
#30771=CARTESIAN_POINT('Ctrl Pts',(-0.140997332152546,1.,2.04414757947919));
#30772=CARTESIAN_POINT('Ctrl Pts',(-0.138911255368966,1.,2.04995762001333));
#30773=CARTESIAN_POINT('Ctrl Pts',(-0.136777941218044,1.,2.0557604441427));
#30774=CARTESIAN_POINT('Ctrl Pts',(-0.134598026192107,1.,2.06155781517844));
#30775=CARTESIAN_POINT('Ctrl Pts',(-0.13237211154771,1.,2.06735123910319));
#30776=CARTESIAN_POINT('Ctrl Pts',(-0.130100748328401,1.,2.07314114713047));
#30777=CARTESIAN_POINT('Ctrl Pts',(-0.127784445276116,1.,2.07892715110967));
#30778=CARTESIAN_POINT('Ctrl Pts',(-0.125423679412058,1.,2.08470840653628));
#30779=CARTESIAN_POINT('Ctrl Pts',(-0.123018905621083,1.,2.09048392424826));
#30780=CARTESIAN_POINT('Ctrl Pts',(-0.120570567965129,1.,2.09625292867756));
#30781=CARTESIAN_POINT('Ctrl Pts',(-0.118079107988368,1.,2.10201512132945));
#30782=CARTESIAN_POINT('Ctrl Pts',(-0.115544957687941,1.,2.10777050261359));
#30783=CARTESIAN_POINT('Ctrl Pts',(-0.112968534419746,1.,2.11351924490335));
#30784=CARTESIAN_POINT('Ctrl Pts',(-0.11035023613502,1.,2.11926155590849));
#30785=CARTESIAN_POINT('Ctrl Pts',(-0.107690435231068,1.,2.12499752306927));
#30786=CARTESIAN_POINT('Ctrl Pts',(-0.104989479152703,1.,2.1307270488718));
#30787=CARTESIAN_POINT('Ctrl Pts',(-0.102247700556064,1.,2.13644992667052));
#30788=CARTESIAN_POINT('Ctrl Pts',(-0.0994654261990745,1.,2.14216588395974));
#30789=CARTESIAN_POINT('Ctrl Pts',(-0.0966429852305691,1.,2.14787463531864));
#30790=CARTESIAN_POINT('Ctrl Pts',(-0.0937807218868348,1.,2.15357593978377));
#30791=CARTESIAN_POINT('Ctrl Pts',(-0.0908789888108269,1.,2.15926961544808));
#30792=CARTESIAN_POINT('Ctrl Pts',(-0.0879381291387825,1.,2.16495552645275));
#30793=CARTESIAN_POINT('Ctrl Pts',(-0.0849584620835646,1.,2.17063357871031));
#30794=CARTESIAN_POINT('Ctrl Pts',(-0.0819402680871942,1.,2.1763037121106));
#30795=CARTESIAN_POINT('Ctrl Pts',(-0.078883772768323,1.,2.18196589448304));
#30796=CARTESIAN_POINT('Ctrl Pts',(-0.0757891465833414,1.,2.1876201139874));
#30797=CARTESIAN_POINT('Ctrl Pts',(-0.0732830357304279,1.,2.19213712012956));
#30798=CARTESIAN_POINT('Ctrl Pts',(-0.071386377952463,1.,2.19552129483562));
#30799=CARTESIAN_POINT('Ctrl Pts',(-0.0701143536324929,1.,2.19777582085261));
#30800=CARTESIAN_POINT('Ctrl Pts',(-0.0694764450219586,1.,2.19890268624765));
#30801=CARTESIAN_POINT('',(-0.163289472382897,0.,1.74236521665491));
#30802=CARTESIAN_POINT('Origin',(0.,0.,0.));
#30803=CARTESIAN_POINT('',(-0.383122945602004,1.,1.7075470150345));
#30804=CARTESIAN_POINT('Origin',(0.,1.,0.));
#30805=CARTESIAN_POINT('',(-0.383122945602004,0.,1.7075470150345));
#30806=CARTESIAN_POINT('Ctrl Pts',(-0.61342227326009,-1.,2.11275013067528));
#30807=CARTESIAN_POINT('Ctrl Pts',(-0.61342227326009,1.,2.11275013067528));
#30808=CARTESIAN_POINT('Ctrl Pts',(-0.61246736556225,-1.,2.11187554260142));
#30809=CARTESIAN_POINT('Ctrl Pts',(-0.61246736556225,1.,2.11187554260142));
#30810=CARTESIAN_POINT('Ctrl Pts',(-0.610560911691113,-1.,2.11012443807661));
#30811=CARTESIAN_POINT('Ctrl Pts',(-0.610560911691113,1.,2.11012443807661));
#30812=CARTESIAN_POINT('Ctrl Pts',(-0.607711315456826,-1.,2.10749199615859));
#30813=CARTESIAN_POINT('Ctrl Pts',(-0.607711315456826,1.,2.10749199615859));
#30814=CARTESIAN_POINT('Ctrl Pts',(-0.603932030738212,-1.,2.10397049887709));
#30815=CARTESIAN_POINT('Ctrl Pts',(-0.603932030738212,1.,2.10397049887709));
#30816=CARTESIAN_POINT('Ctrl Pts',(-0.599241616422144,-1.,2.09954930865331));
#30817=CARTESIAN_POINT('Ctrl Pts',(-0.599241616422144,1.,2.09954930865331));
#30818=CARTESIAN_POINT('Ctrl Pts',(-0.594585006052824,-1.,2.09510876220501));
#30819=CARTESIAN_POINT('Ctrl Pts',(-0.594585006052824,1.,2.09510876220501));
#30820=CARTESIAN_POINT('Ctrl Pts',(-0.589962365403189,-1.,2.09064881812053));
#30821=CARTESIAN_POINT('Ctrl Pts',(-0.589962365403189,1.,2.09064881812053));
#30822=CARTESIAN_POINT('Ctrl Pts',(-0.585373918990895,-1.,2.086169437277));
#30823=CARTESIAN_POINT('Ctrl Pts',(-0.585373918990895,1.,2.086169437277));
#30824=CARTESIAN_POINT('Ctrl Pts',(-0.580819952107257,-1.,2.08167059018138));
#30825=CARTESIAN_POINT('Ctrl Pts',(-0.580819952107257,1.,2.08167059018138));
#30826=CARTESIAN_POINT('Ctrl Pts',(-0.576300797416275,-1.,2.07715226767361));
#30827=CARTESIAN_POINT('Ctrl Pts',(-0.576300797416275,1.,2.07715226767361));
#30828=CARTESIAN_POINT('Ctrl Pts',(-0.571816823242411,-1.,2.07261449292757));
#30829=CARTESIAN_POINT('Ctrl Pts',(-0.571816823242411,1.,2.07261449292757));
#30830=CARTESIAN_POINT('Ctrl Pts',(-0.567368421181229,-1.,2.06805732997383));
#30831=CARTESIAN_POINT('Ctrl Pts',(-0.567368421181229,1.,2.06805732997383));
#30832=CARTESIAN_POINT('Ctrl Pts',(-0.562955993082574,-1.,2.06348090160697));
#30833=CARTESIAN_POINT('Ctrl Pts',(-0.562955993082574,1.,2.06348090160697));
#30834=CARTESIAN_POINT('Ctrl Pts',(-0.558579940185467,-1.,2.05888537756571));
#30835=CARTESIAN_POINT('Ctrl Pts',(-0.558579940185467,1.,2.05888537756571));
#30836=CARTESIAN_POINT('Ctrl Pts',(-0.55424065746411,-1.,2.05427091604482));
#30837=CARTESIAN_POINT('Ctrl Pts',(-0.55424065746411,1.,2.05427091604482));
#30838=CARTESIAN_POINT('Ctrl Pts',(-0.549938525150342,-1.,2.04963761077974));
#30839=CARTESIAN_POINT('Ctrl Pts',(-0.549938525150342,1.,2.04963761077974));
#30840=CARTESIAN_POINT('Ctrl Pts',(-0.545673903817348,-1.,2.0449854471456));
#30841=CARTESIAN_POINT('Ctrl Pts',(-0.545673903817348,1.,2.0449854471456));
#30842=CARTESIAN_POINT('Ctrl Pts',(-0.54144712061552,-1.,2.0403142269048));
#30843=CARTESIAN_POINT('Ctrl Pts',(-0.54144712061552,1.,2.0403142269048));
#30844=CARTESIAN_POINT('Ctrl Pts',(-0.537258489833134,-1.,2.03562362953993));
#30845=CARTESIAN_POINT('Ctrl Pts',(-0.537258489833134,1.,2.03562362953993));
#30846=CARTESIAN_POINT('Ctrl Pts',(-0.533108355132905,-1.,2.03091336214401));
#30847=CARTESIAN_POINT('Ctrl Pts',(-0.533108355132905,1.,2.03091336214401));
#30848=CARTESIAN_POINT('Ctrl Pts',(-0.528997127241911,-1.,2.02618329083289));
#30849=CARTESIAN_POINT('Ctrl Pts',(-0.528997127241911,1.,2.02618329083289));
#30850=CARTESIAN_POINT('Ctrl Pts',(-0.524925318333518,-1.,2.02143356304712));
#30851=CARTESIAN_POINT('Ctrl Pts',(-0.524925318333518,1.,2.02143356304712));
#30852=CARTESIAN_POINT('Ctrl Pts',(-0.520893590399428,-1.,2.01666477917305));
#30853=CARTESIAN_POINT('Ctrl Pts',(-0.520893590399428,1.,2.01666477917305));
#30854=CARTESIAN_POINT('Ctrl Pts',(-0.516902681728733,-1.,2.01187773939257));
#30855=CARTESIAN_POINT('Ctrl Pts',(-0.516902681728733,1.,2.01187773939257));
#30856=CARTESIAN_POINT('Ctrl Pts',(-0.512953306961814,-1.,2.00707309946955));
#30857=CARTESIAN_POINT('Ctrl Pts',(-0.512953306961814,1.,2.00707309946955));
#30858=CARTESIAN_POINT('Ctrl Pts',(-0.509046069886152,-1.,2.00225107134733));
#30859=CARTESIAN_POINT('Ctrl Pts',(-0.509046069886152,1.,2.00225107134733));
#30860=CARTESIAN_POINT('Ctrl Pts',(-0.505181361323011,-1.,1.99741107463567));
#30861=CARTESIAN_POINT('Ctrl Pts',(-0.505181361323011,1.,1.99741107463567));
#30862=CARTESIAN_POINT('Ctrl Pts',(-0.501359287727129,-1.,1.9925514912615));
#30863=CARTESIAN_POINT('Ctrl Pts',(-0.501359287727129,1.,1.9925514912615));
#30864=CARTESIAN_POINT('Ctrl Pts',(-0.497579909545564,-1.,1.98767044752929));
#30865=CARTESIAN_POINT('Ctrl Pts',(-0.497579909545564,1.,1.98767044752929));
#30866=CARTESIAN_POINT('Ctrl Pts',(-0.493843476541492,-1.,1.9827665876182));
#30867=CARTESIAN_POINT('Ctrl Pts',(-0.493843476541492,1.,1.9827665876182));
#30868=CARTESIAN_POINT('Ctrl Pts',(-0.490150627860955,-1.,1.97783973019229));
#30869=CARTESIAN_POINT('Ctrl Pts',(-0.490150627860955,1.,1.97783973019229));
#30870=CARTESIAN_POINT('Ctrl Pts',(-0.486502692907661,-1.,1.97289186263272));
#30871=CARTESIAN_POINT('Ctrl Pts',(-0.486502692907661,1.,1.97289186263272));
#30872=CARTESIAN_POINT('Ctrl Pts',(-0.482901662120687,-1.,1.96792703422358));
#30873=CARTESIAN_POINT('Ctrl Pts',(-0.482901662120687,1.,1.96792703422358));
#30874=CARTESIAN_POINT('Ctrl Pts',(-0.479349583074846,-1.,1.96294933055938));
#30875=CARTESIAN_POINT('Ctrl Pts',(-0.479349583074846,1.,1.96294933055938));
#30876=CARTESIAN_POINT('Ctrl Pts',(-0.475848034683172,-1.,1.95796111148175));
#30877=CARTESIAN_POINT('Ctrl Pts',(-0.475848034683172,1.,1.95796111148175));
#30878=CARTESIAN_POINT('Ctrl Pts',(-0.47239767226408,-1.,1.95296148278136));
#30879=CARTESIAN_POINT('Ctrl Pts',(-0.47239767226408,1.,1.95296148278136));
#30880=CARTESIAN_POINT('Ctrl Pts',(-0.468997482913158,-1.,1.94794381136524));
#30881=CARTESIAN_POINT('Ctrl Pts',(-0.468997482913158,1.,1.94794381136524));
#30882=CARTESIAN_POINT('Ctrl Pts',(-0.465645462026065,-1.,1.94289794196205));
#30883=CARTESIAN_POINT('Ctrl Pts',(-0.465645462026065,1.,1.94289794196205));
#30884=CARTESIAN_POINT('Ctrl Pts',(-0.462340031009087,-1.,1.93781486640834));
#30885=CARTESIAN_POINT('Ctrl Pts',(-0.462340031009087,1.,1.93781486640834));
#30886=CARTESIAN_POINT('Ctrl Pts',(-0.459081234547931,-1.,1.93269066517936));
#30887=CARTESIAN_POINT('Ctrl Pts',(-0.459081234547931,1.,1.93269066517936));
#30888=CARTESIAN_POINT('Ctrl Pts',(-0.455872005174335,-1.,1.92753067150461));
#30889=CARTESIAN_POINT('Ctrl Pts',(-0.455872005174335,1.,1.92753067150461));
#30890=CARTESIAN_POINT('Ctrl Pts',(-0.452719478359356,-1.,1.9223538064847));
#30891=CARTESIAN_POINT('Ctrl Pts',(-0.452719478359356,1.,1.9223538064847));
#30892=CARTESIAN_POINT('Ctrl Pts',(-0.449632260106572,-1.,1.91718342555717));
#30893=CARTESIAN_POINT('Ctrl Pts',(-0.449632260106572,1.,1.91718342555717));
#30894=CARTESIAN_POINT('Ctrl Pts',(-0.446617343485651,-1.,1.91203699981095));
#30895=CARTESIAN_POINT('Ctrl Pts',(-0.446617343485651,1.,1.91203699981095));
#30896=CARTESIAN_POINT('Ctrl Pts',(-0.44367755684917,-1.,1.90691756144906));
#30897=CARTESIAN_POINT('Ctrl Pts',(-0.44367755684917,1.,1.90691756144906));
#30898=CARTESIAN_POINT('Ctrl Pts',(-0.440807833704161,-1.,1.90180124389137));
#30899=CARTESIAN_POINT('Ctrl Pts',(-0.440807833704161,1.,1.90180124389137));
#30900=CARTESIAN_POINT('Ctrl Pts',(-0.437995003948443,-1.,1.89663648956549));
#30901=CARTESIAN_POINT('Ctrl Pts',(-0.437995003948443,1.,1.89663648956549));
#30902=CARTESIAN_POINT('Ctrl Pts',(-0.43522566096358,-1.,1.89136993975585));
#30903=CARTESIAN_POINT('Ctrl Pts',(-0.43522566096358,1.,1.89136993975585));
#30904=CARTESIAN_POINT('Ctrl Pts',(-0.432493038548833,-1.,1.88596913666828));
#30905=CARTESIAN_POINT('Ctrl Pts',(-0.432493038548833,1.,1.88596913666828));
#30906=CARTESIAN_POINT('Ctrl Pts',(-0.429803062482217,-1.,1.88044229001778));
#30907=CARTESIAN_POINT('Ctrl Pts',(-0.429803062482217,1.,1.88044229001778));
#30908=CARTESIAN_POINT('Ctrl Pts',(-0.427183828518743,-1.,1.87486989291333));
#30909=CARTESIAN_POINT('Ctrl Pts',(-0.427183828518743,1.,1.87486989291333));
#30910=CARTESIAN_POINT('Ctrl Pts',(-0.424678177290876,-1.,1.8693780394412));
#30911=CARTESIAN_POINT('Ctrl Pts',(-0.424678177290876,1.,1.8693780394412));
#30912=CARTESIAN_POINT('Ctrl Pts',(-0.422327307417885,-1.,1.86408083333863));
#30913=CARTESIAN_POINT('Ctrl Pts',(-0.422327307417885,1.,1.86408083333863));
#30914=CARTESIAN_POINT('Ctrl Pts',(-0.420157287975583,-1.,1.8590328109667));
#30915=CARTESIAN_POINT('Ctrl Pts',(-0.420157287975583,1.,1.8590328109667));
#30916=CARTESIAN_POINT('Ctrl Pts',(-0.418164129144045,-1.,1.8541763285645));
#30917=CARTESIAN_POINT('Ctrl Pts',(-0.418164129144045,1.,1.8541763285645));
#30918=CARTESIAN_POINT('Ctrl Pts',(-0.416300022039885,-1.,1.84929312930314));
#30919=CARTESIAN_POINT('Ctrl Pts',(-0.416300022039885,1.,1.84929312930314));
#30920=CARTESIAN_POINT('Ctrl Pts',(-0.414487438255542,-1.,1.84405757074218));
#30921=CARTESIAN_POINT('Ctrl Pts',(-0.414487438255542,1.,1.84405757074218));
#30922=CARTESIAN_POINT('Ctrl Pts',(-0.412633125322945,-1.,1.8380895347617));
#30923=CARTESIAN_POINT('Ctrl Pts',(-0.412633125322945,1.,1.8380895347617));
#30924=CARTESIAN_POINT('Ctrl Pts',(-0.410641256301276,-1.,1.83100408895047));
#30925=CARTESIAN_POINT('Ctrl Pts',(-0.410641256301276,1.,1.83100408895047));
#30926=CARTESIAN_POINT('Ctrl Pts',(-0.408428948106227,-1.,1.82247022677562));
#30927=CARTESIAN_POINT('Ctrl Pts',(-0.408428948106227,1.,1.82247022677562));
#30928=CARTESIAN_POINT('Ctrl Pts',(-0.405933518407175,-1.,1.81223801812013));
#30929=CARTESIAN_POINT('Ctrl Pts',(-0.405933518407175,1.,1.81223801812013));
#30930=CARTESIAN_POINT('Ctrl Pts',(-0.403107976163396,-1.,1.80012077173238));
#30931=CARTESIAN_POINT('Ctrl Pts',(-0.403107976163396,1.,1.80012077173238));
#30932=CARTESIAN_POINT('Ctrl Pts',(-0.399919403774155,-1.,1.78598826343754));
#30933=CARTESIAN_POINT('Ctrl Pts',(-0.399919403774155,1.,1.78598826343754));
#30934=CARTESIAN_POINT('Ctrl Pts',(-0.396346196110688,-1.,1.76975560043442));
#30935=CARTESIAN_POINT('Ctrl Pts',(-0.396346196110688,1.,1.76975560043442));
#30936=CARTESIAN_POINT('Ctrl Pts',(-0.392375812285395,-1.,1.75137405310193));
#30937=CARTESIAN_POINT('Ctrl Pts',(-0.392375812285395,1.,1.75137405310193));
#30938=CARTESIAN_POINT('Ctrl Pts',(-0.388877023502615,-1.,1.73493170972829));
#30939=CARTESIAN_POINT('Ctrl Pts',(-0.388877023502615,1.,1.73493170972829));
#30940=CARTESIAN_POINT('Ctrl Pts',(-0.386070790323281,-1.,1.72162022244582));
#30941=CARTESIAN_POINT('Ctrl Pts',(-0.386070790323281,1.,1.72162022244582));
#30942=CARTESIAN_POINT('Ctrl Pts',(-0.384119047314215,-1.,1.71231062891398));
#30943=CARTESIAN_POINT('Ctrl Pts',(-0.384119047314215,1.,1.71231062891398));
#30944=CARTESIAN_POINT('Ctrl Pts',(-0.383122945602004,-1.,1.7075470150345));
#30945=CARTESIAN_POINT('Ctrl Pts',(-0.383122945602004,1.,1.7075470150345));
#30946=CARTESIAN_POINT('',(-0.61342227326009,1.,2.11275013067528));
#30947=CARTESIAN_POINT('Ctrl Pts',(-0.61342227326009,1.,2.11275013067528));
#30948=CARTESIAN_POINT('Ctrl Pts',(-0.61246736556225,1.,2.11187554260142));
#30949=CARTESIAN_POINT('Ctrl Pts',(-0.610560911691113,1.,2.11012443807661));
#30950=CARTESIAN_POINT('Ctrl Pts',(-0.607711315456826,1.,2.10749199615859));
#30951=CARTESIAN_POINT('Ctrl Pts',(-0.603932030738212,1.,2.10397049887709));
#30952=CARTESIAN_POINT('Ctrl Pts',(-0.599241616422144,1.,2.09954930865331));
#30953=CARTESIAN_POINT('Ctrl Pts',(-0.594585006052824,1.,2.09510876220501));
#30954=CARTESIAN_POINT('Ctrl Pts',(-0.589962365403189,1.,2.09064881812053));
#30955=CARTESIAN_POINT('Ctrl Pts',(-0.585373918990895,1.,2.086169437277));
#30956=CARTESIAN_POINT('Ctrl Pts',(-0.580819952107257,1.,2.08167059018138));
#30957=CARTESIAN_POINT('Ctrl Pts',(-0.576300797416275,1.,2.07715226767361));
#30958=CARTESIAN_POINT('Ctrl Pts',(-0.571816823242411,1.,2.07261449292757));
#30959=CARTESIAN_POINT('Ctrl Pts',(-0.567368421181229,1.,2.06805732997383));
#30960=CARTESIAN_POINT('Ctrl Pts',(-0.562955993082574,1.,2.06348090160697));
#30961=CARTESIAN_POINT('Ctrl Pts',(-0.558579940185467,1.,2.05888537756571));
#30962=CARTESIAN_POINT('Ctrl Pts',(-0.55424065746411,1.,2.05427091604482));
#30963=CARTESIAN_POINT('Ctrl Pts',(-0.549938525150342,1.,2.04963761077974));
#30964=CARTESIAN_POINT('Ctrl Pts',(-0.545673903817348,1.,2.0449854471456));
#30965=CARTESIAN_POINT('Ctrl Pts',(-0.54144712061552,1.,2.0403142269048));
#30966=CARTESIAN_POINT('Ctrl Pts',(-0.537258489833134,1.,2.03562362953993));
#30967=CARTESIAN_POINT('Ctrl Pts',(-0.533108355132905,1.,2.03091336214401));
#30968=CARTESIAN_POINT('Ctrl Pts',(-0.528997127241911,1.,2.02618329083289));
#30969=CARTESIAN_POINT('Ctrl Pts',(-0.524925318333518,1.,2.02143356304712));
#30970=CARTESIAN_POINT('Ctrl Pts',(-0.520893590399428,1.,2.01666477917305));
#30971=CARTESIAN_POINT('Ctrl Pts',(-0.516902681728733,1.,2.01187773939257));
#30972=CARTESIAN_POINT('Ctrl Pts',(-0.512953306961814,1.,2.00707309946955));
#30973=CARTESIAN_POINT('Ctrl Pts',(-0.509046069886152,1.,2.00225107134733));
#30974=CARTESIAN_POINT('Ctrl Pts',(-0.505181361323011,1.,1.99741107463567));
#30975=CARTESIAN_POINT('Ctrl Pts',(-0.501359287727129,1.,1.9925514912615));
#30976=CARTESIAN_POINT('Ctrl Pts',(-0.497579909545564,1.,1.98767044752929));
#30977=CARTESIAN_POINT('Ctrl Pts',(-0.493843476541492,1.,1.9827665876182));
#30978=CARTESIAN_POINT('Ctrl Pts',(-0.490150627860955,1.,1.97783973019229));
#30979=CARTESIAN_POINT('Ctrl Pts',(-0.486502692907661,1.,1.97289186263272));
#30980=CARTESIAN_POINT('Ctrl Pts',(-0.482901662120687,1.,1.96792703422358));
#30981=CARTESIAN_POINT('Ctrl Pts',(-0.479349583074846,1.,1.96294933055938));
#30982=CARTESIAN_POINT('Ctrl Pts',(-0.475848034683172,1.,1.95796111148175));
#30983=CARTESIAN_POINT('Ctrl Pts',(-0.47239767226408,1.,1.95296148278136));
#30984=CARTESIAN_POINT('Ctrl Pts',(-0.468997482913158,1.,1.94794381136524));
#30985=CARTESIAN_POINT('Ctrl Pts',(-0.465645462026065,1.,1.94289794196205));
#30986=CARTESIAN_POINT('Ctrl Pts',(-0.462340031009087,1.,1.93781486640834));
#30987=CARTESIAN_POINT('Ctrl Pts',(-0.459081234547931,1.,1.93269066517936));
#30988=CARTESIAN_POINT('Ctrl Pts',(-0.455872005174335,1.,1.92753067150461));
#30989=CARTESIAN_POINT('Ctrl Pts',(-0.452719478359356,1.,1.9223538064847));
#30990=CARTESIAN_POINT('Ctrl Pts',(-0.449632260106572,1.,1.91718342555717));
#30991=CARTESIAN_POINT('Ctrl Pts',(-0.446617343485651,1.,1.91203699981095));
#30992=CARTESIAN_POINT('Ctrl Pts',(-0.44367755684917,1.,1.90691756144906));
#30993=CARTESIAN_POINT('Ctrl Pts',(-0.440807833704161,1.,1.90180124389137));
#30994=CARTESIAN_POINT('Ctrl Pts',(-0.437995003948443,1.,1.89663648956549));
#30995=CARTESIAN_POINT('Ctrl Pts',(-0.43522566096358,1.,1.89136993975585));
#30996=CARTESIAN_POINT('Ctrl Pts',(-0.432493038548833,1.,1.88596913666828));
#30997=CARTESIAN_POINT('Ctrl Pts',(-0.429803062482217,1.,1.88044229001778));
#30998=CARTESIAN_POINT('Ctrl Pts',(-0.427183828518743,1.,1.87486989291333));
#30999=CARTESIAN_POINT('Ctrl Pts',(-0.424678177290876,1.,1.8693780394412));
#31000=CARTESIAN_POINT('Ctrl Pts',(-0.422327307417885,1.,1.86408083333863));
#31001=CARTESIAN_POINT('Ctrl Pts',(-0.420157287975583,1.,1.8590328109667));
#31002=CARTESIAN_POINT('Ctrl Pts',(-0.418164129144045,1.,1.8541763285645));
#31003=CARTESIAN_POINT('Ctrl Pts',(-0.416300022039885,1.,1.84929312930314));
#31004=CARTESIAN_POINT('Ctrl Pts',(-0.414487438255542,1.,1.84405757074218));
#31005=CARTESIAN_POINT('Ctrl Pts',(-0.412633125322945,1.,1.8380895347617));
#31006=CARTESIAN_POINT('Ctrl Pts',(-0.410641256301276,1.,1.83100408895047));
#31007=CARTESIAN_POINT('Ctrl Pts',(-0.408428948106227,1.,1.82247022677562));
#31008=CARTESIAN_POINT('Ctrl Pts',(-0.405933518407175,1.,1.81223801812013));
#31009=CARTESIAN_POINT('Ctrl Pts',(-0.403107976163396,1.,1.80012077173238));
#31010=CARTESIAN_POINT('Ctrl Pts',(-0.399919403774155,1.,1.78598826343754));
#31011=CARTESIAN_POINT('Ctrl Pts',(-0.396346196110688,1.,1.76975560043442));
#31012=CARTESIAN_POINT('Ctrl Pts',(-0.392375812285395,1.,1.75137405310193));
#31013=CARTESIAN_POINT('Ctrl Pts',(-0.388877023502615,1.,1.73493170972829));
#31014=CARTESIAN_POINT('Ctrl Pts',(-0.386070790323281,1.,1.72162022244582));
#31015=CARTESIAN_POINT('Ctrl Pts',(-0.384119047314215,1.,1.71231062891398));
#31016=CARTESIAN_POINT('Ctrl Pts',(-0.383122945602004,1.,1.7075470150345));
#31017=CARTESIAN_POINT('',(-0.61342227326009,0.,2.11275013067528));
#31018=CARTESIAN_POINT('Origin',(-0.745574324794401,0.,2.0698113262342));
#31019=CARTESIAN_POINT('',(-0.745574324794401,1.,2.0698113262342));
#31020=CARTESIAN_POINT('',(-0.61342227326009,1.,2.11275013067528));
#31021=CARTESIAN_POINT('',(-0.745574324794401,0.,2.0698113262342));
#31022=CARTESIAN_POINT('Ctrl Pts',(-0.693717979106306,-1.,1.60662857109684));
#31023=CARTESIAN_POINT('Ctrl Pts',(-0.693717979106306,1.,1.60662857109684));
#31024=CARTESIAN_POINT('Ctrl Pts',(-0.695712097881194,-1.,1.61106790958151));
#31025=CARTESIAN_POINT('Ctrl Pts',(-0.695712097881194,1.,1.61106790958151));
#31026=CARTESIAN_POINT('Ctrl Pts',(-0.699605146405088,-1.,1.61974673472612));
#31027=CARTESIAN_POINT('Ctrl Pts',(-0.699605146405088,1.,1.61974673472612));
#31028=CARTESIAN_POINT('Ctrl Pts',(-0.705159151988319,-1.,1.63216541664676));
#31029=CARTESIAN_POINT('Ctrl Pts',(-0.705159151988319,1.,1.63216541664676));
#31030=CARTESIAN_POINT('Ctrl Pts',(-0.711993139355394,-1.,1.64752408832016));
#31031=CARTESIAN_POINT('Ctrl Pts',(-0.711993139355394,1.,1.64752408832016));
#31032=CARTESIAN_POINT('Ctrl Pts',(-0.719585433804282,-1.,1.6647288055568));
#31033=CARTESIAN_POINT('Ctrl Pts',(-0.719585433804282,1.,1.6647288055568));
#31034=CARTESIAN_POINT('Ctrl Pts',(-0.726235967997433,-1.,1.67996158455503));
#31035=CARTESIAN_POINT('Ctrl Pts',(-0.726235967997433,1.,1.67996158455503));
#31036=CARTESIAN_POINT('Ctrl Pts',(-0.731963238697195,-1.,1.69326921975743));
#31037=CARTESIAN_POINT('Ctrl Pts',(-0.731963238697195,1.,1.69326921975743));
#31038=CARTESIAN_POINT('Ctrl Pts',(-0.736799665724771,-1.,1.70473309006121));
#31039=CARTESIAN_POINT('Ctrl Pts',(-0.736799665724771,1.,1.70473309006121));
#31040=CARTESIAN_POINT('Ctrl Pts',(-0.740795162032088,-1.,1.71447789751927));
#31041=CARTESIAN_POINT('Ctrl Pts',(-0.740795162032088,1.,1.71447789751927));
#31042=CARTESIAN_POINT('Ctrl Pts',(-0.744021445433764,-1.,1.7226822991693));
#31043=CARTESIAN_POINT('Ctrl Pts',(-0.744021445433764,1.,1.7226822991693));
#31044=CARTESIAN_POINT('Ctrl Pts',(-0.746574710096436,-1.,1.72958533647399));
#31045=CARTESIAN_POINT('Ctrl Pts',(-0.746574710096436,1.,1.72958533647399));
#31046=CARTESIAN_POINT('Ctrl Pts',(-0.748582462954855,-1.,1.73550351679848));
#31047=CARTESIAN_POINT('Ctrl Pts',(-0.748582462954855,1.,1.73550351679848));
#31048=CARTESIAN_POINT('Ctrl Pts',(-0.75019343597954,-1.,1.74080458266705));
#31049=CARTESIAN_POINT('Ctrl Pts',(-0.75019343597954,1.,1.74080458266705));
#31050=CARTESIAN_POINT('Ctrl Pts',(-0.751555614163629,-1.,1.74585086852298));
#31051=CARTESIAN_POINT('Ctrl Pts',(-0.751555614163629,1.,1.74585086852298));
#31052=CARTESIAN_POINT('Ctrl Pts',(-0.752797683531377,-1.,1.75095139468809));
#31053=CARTESIAN_POINT('Ctrl Pts',(-0.752797683531377,1.,1.75095139468809));
#31054=CARTESIAN_POINT('Ctrl Pts',(-0.75400925402848,-1.,1.75631083600175));
#31055=CARTESIAN_POINT('Ctrl Pts',(-0.75400925402848,1.,1.75631083600175));
#31056=CARTESIAN_POINT('Ctrl Pts',(-0.755220979975262,-1.,1.7619781724032));
#31057=CARTESIAN_POINT('Ctrl Pts',(-0.755220979975262,1.,1.7619781724032));
#31058=CARTESIAN_POINT('Ctrl Pts',(-0.756421896028403,-1.,1.76789396003141));
#31059=CARTESIAN_POINT('Ctrl Pts',(-0.756421896028403,1.,1.76789396003141));
#31060=CARTESIAN_POINT('Ctrl Pts',(-0.757578264077238,-1.,1.77394167108342));
#31061=CARTESIAN_POINT('Ctrl Pts',(-0.757578264077238,1.,1.77394167108342));
#31062=CARTESIAN_POINT('Ctrl Pts',(-0.75865062667738,-1.,1.77999411220912));
#31063=CARTESIAN_POINT('Ctrl Pts',(-0.75865062667738,1.,1.77999411220912));
#31064=CARTESIAN_POINT('Ctrl Pts',(-0.759614401109868,-1.,1.78596964884526));
#31065=CARTESIAN_POINT('Ctrl Pts',(-0.759614401109868,1.,1.78596964884526));
#31066=CARTESIAN_POINT('Ctrl Pts',(-0.760469555880425,-1.,1.79185815610802));
#31067=CARTESIAN_POINT('Ctrl Pts',(-0.760469555880425,1.,1.79185815610802));
#31068=CARTESIAN_POINT('Ctrl Pts',(-0.761229695230359,-1.,1.79768986997735));
#31069=CARTESIAN_POINT('Ctrl Pts',(-0.761229695230359,1.,1.79768986997735));
#31070=CARTESIAN_POINT('Ctrl Pts',(-0.761915336443516,-1.,1.80351583877334));
#31071=CARTESIAN_POINT('Ctrl Pts',(-0.761915336443516,1.,1.80351583877334));
#31072=CARTESIAN_POINT('Ctrl Pts',(-0.762546129464036,-1.,1.80938551463989));
#31073=CARTESIAN_POINT('Ctrl Pts',(-0.762546129464036,1.,1.80938551463989));
#31074=CARTESIAN_POINT('Ctrl Pts',(-0.763132003836783,-1.,1.81532118405566));
#31075=CARTESIAN_POINT('Ctrl Pts',(-0.763132003836783,1.,1.81532118405566));
#31076=CARTESIAN_POINT('Ctrl Pts',(-0.763673465462854,-1.,1.82131873145297));
#31077=CARTESIAN_POINT('Ctrl Pts',(-0.763673465462854,1.,1.82131873145297));
#31078=CARTESIAN_POINT('Ctrl Pts',(-0.764165902606055,-1.,1.8273599120008));
#31079=CARTESIAN_POINT('Ctrl Pts',(-0.764165902606055,1.,1.8273599120008));
#31080=CARTESIAN_POINT('Ctrl Pts',(-0.764602549687845,-1.,1.8334207722714));
#31081=CARTESIAN_POINT('Ctrl Pts',(-0.764602549687845,1.,1.8334207722714));
#31082=CARTESIAN_POINT('Ctrl Pts',(-0.764978057881687,-1.,1.83948181064823));
#31083=CARTESIAN_POINT('Ctrl Pts',(-0.764978057881687,1.,1.83948181064823));
#31084=CARTESIAN_POINT('Ctrl Pts',(-0.765291664861971,-1.,1.8455369887591));
#31085=CARTESIAN_POINT('Ctrl Pts',(-0.765291664861971,1.,1.8455369887591));
#31086=CARTESIAN_POINT('Ctrl Pts',(-0.765545710619023,-1.,1.85158945130054));
#31087=CARTESIAN_POINT('Ctrl Pts',(-0.765545710619023,1.,1.85158945130054));
#31088=CARTESIAN_POINT('Ctrl Pts',(-0.765744212909305,-1.,1.85764741390391));
#31089=CARTESIAN_POINT('Ctrl Pts',(-0.765744212909305,1.,1.85764741390391));
#31090=CARTESIAN_POINT('Ctrl Pts',(-0.765891519092557,-1.,1.86372027063314));
#31091=CARTESIAN_POINT('Ctrl Pts',(-0.765891519092557,1.,1.86372027063314));
#31092=CARTESIAN_POINT('Ctrl Pts',(-0.765990708546111,-1.,1.86981398314345));
#31093=CARTESIAN_POINT('Ctrl Pts',(-0.765990708546111,1.,1.86981398314345));
#31094=CARTESIAN_POINT('Ctrl Pts',(-0.766042837036759,-1.,1.87592888967886));
#31095=CARTESIAN_POINT('Ctrl Pts',(-0.766042837036759,1.,1.87592888967886));
#31096=CARTESIAN_POINT('Ctrl Pts',(-0.766047794851869,-1.,1.88206215302561));
#31097=CARTESIAN_POINT('Ctrl Pts',(-0.766047794851869,1.,1.88206215302561));
#31098=CARTESIAN_POINT('Ctrl Pts',(-0.76600483706209,-1.,1.88820926433409));
#31099=CARTESIAN_POINT('Ctrl Pts',(-0.76600483706209,1.,1.88820926433409));
#31100=CARTESIAN_POINT('Ctrl Pts',(-0.765913193856979,-1.,1.89436577771389));
#31101=CARTESIAN_POINT('Ctrl Pts',(-0.765913193856979,1.,1.89436577771389));
#31102=CARTESIAN_POINT('Ctrl Pts',(-0.765772772593395,-1.,1.90052930393599));
#31103=CARTESIAN_POINT('Ctrl Pts',(-0.765772772593395,1.,1.90052930393599));
#31104=CARTESIAN_POINT('Ctrl Pts',(-0.765584196937936,-1.,1.90669961402362));
#31105=CARTESIAN_POINT('Ctrl Pts',(-0.765584196937936,1.,1.90669961402362));
#31106=CARTESIAN_POINT('Ctrl Pts',(-0.765348465884739,-1.,1.91287765805174));
#31107=CARTESIAN_POINT('Ctrl Pts',(-0.765348465884739,1.,1.91287765805174));
#31108=CARTESIAN_POINT('Ctrl Pts',(-0.765066729667095,-1.,1.91906491634197));
#31109=CARTESIAN_POINT('Ctrl Pts',(-0.765066729667095,1.,1.91906491634197));
#31110=CARTESIAN_POINT('Ctrl Pts',(-0.764740025488189,-1.,1.92526263537041));
#31111=CARTESIAN_POINT('Ctrl Pts',(-0.764740025488189,1.,1.92526263537041));
#31112=CARTESIAN_POINT('Ctrl Pts',(-0.764369010673889,-1.,1.93147105496367));
#31113=CARTESIAN_POINT('Ctrl Pts',(-0.764369010673889,1.,1.93147105496367));
#31114=CARTESIAN_POINT('Ctrl Pts',(-0.763954049121393,-1.,1.93768964875867));
#31115=CARTESIAN_POINT('Ctrl Pts',(-0.763954049121393,1.,1.93768964875867));
#31116=CARTESIAN_POINT('Ctrl Pts',(-0.76349533353858,-1.,1.94391746617626));
#31117=CARTESIAN_POINT('Ctrl Pts',(-0.76349533353858,1.,1.94391746617626));
#31118=CARTESIAN_POINT('Ctrl Pts',(-0.762992990878774,-1.,1.95015342590025));
#31119=CARTESIAN_POINT('Ctrl Pts',(-0.762992990878774,1.,1.95015342590025));
#31120=CARTESIAN_POINT('Ctrl Pts',(-0.762447203806263,-1.,1.95639665309893));
#31121=CARTESIAN_POINT('Ctrl Pts',(-0.762447203806263,1.,1.95639665309893));
#31122=CARTESIAN_POINT('Ctrl Pts',(-0.761858300014575,-1.,1.96264672744229));
#31123=CARTESIAN_POINT('Ctrl Pts',(-0.761858300014575,1.,1.96264672744229));
#31124=CARTESIAN_POINT('Ctrl Pts',(-0.761226690483986,-1.,1.96890351582545));
#31125=CARTESIAN_POINT('Ctrl Pts',(-0.761226690483986,1.,1.96890351582545));
#31126=CARTESIAN_POINT('Ctrl Pts',(-0.760552825409855,-1.,1.97516705321521));
#31127=CARTESIAN_POINT('Ctrl Pts',(-0.760552825409855,1.,1.97516705321521));
#31128=CARTESIAN_POINT('Ctrl Pts',(-0.759837147452135,-1.,1.98143741418156));
#31129=CARTESIAN_POINT('Ctrl Pts',(-0.759837147452135,1.,1.98143741418156));
#31130=CARTESIAN_POINT('Ctrl Pts',(-0.759080037802243,-1.,1.98771456680806));
#31131=CARTESIAN_POINT('Ctrl Pts',(-0.759080037802243,1.,1.98771456680806));
#31132=CARTESIAN_POINT('Ctrl Pts',(-0.758281796766377,-1.,1.9939983109871));
#31133=CARTESIAN_POINT('Ctrl Pts',(-0.758281796766377,1.,1.9939983109871));
#31134=CARTESIAN_POINT('Ctrl Pts',(-0.757442676862341,-1.,2.00028834739072));
#31135=CARTESIAN_POINT('Ctrl Pts',(-0.757442676862341,1.,2.00028834739072));
#31136=CARTESIAN_POINT('Ctrl Pts',(-0.756562904646496,-1.,2.00658431587682));
#31137=CARTESIAN_POINT('Ctrl Pts',(-0.756562904646496,1.,2.00658431587682));
#31138=CARTESIAN_POINT('Ctrl Pts',(-0.7556427049581,-1.,2.01288584328149));
#31139=CARTESIAN_POINT('Ctrl Pts',(-0.7556427049581,1.,2.01288584328149));
#31140=CARTESIAN_POINT('Ctrl Pts',(-0.75468233072352,-1.,2.01919259406003));
#31141=CARTESIAN_POINT('Ctrl Pts',(-0.75468233072352,1.,2.01919259406003));
#31142=CARTESIAN_POINT('Ctrl Pts',(-0.753682061113766,-1.,2.02550428623587));
#31143=CARTESIAN_POINT('Ctrl Pts',(-0.753682061113766,1.,2.02550428623587));
#31144=CARTESIAN_POINT('Ctrl Pts',(-0.752642180488104,-1.,2.03182068456467));
#31145=CARTESIAN_POINT('Ctrl Pts',(-0.752642180488104,1.,2.03182068456467));
#31146=CARTESIAN_POINT('Ctrl Pts',(-0.751562963361384,-1.,2.03814160092173));
#31147=CARTESIAN_POINT('Ctrl Pts',(-0.751562963361384,1.,2.03814160092173));
#31148=CARTESIAN_POINT('Ctrl Pts',(-0.750444657874758,-1.,2.04446689147754));
#31149=CARTESIAN_POINT('Ctrl Pts',(-0.750444657874758,1.,2.04446689147754));
#31150=CARTESIAN_POINT('Ctrl Pts',(-0.749287468663053,-1.,2.05079645591606));
#31151=CARTESIAN_POINT('Ctrl Pts',(-0.749287468663053,1.,2.05079645591606));
#31152=CARTESIAN_POINT('Ctrl Pts',(-0.748091554181101,-1.,2.05713023030263));
#31153=CARTESIAN_POINT('Ctrl Pts',(-0.748091554181101,1.,2.05713023030263));
#31154=CARTESIAN_POINT('Ctrl Pts',(-0.747103932785504,-1.,2.06220058927162));
#31155=CARTESIAN_POINT('Ctrl Pts',(-0.747103932785504,1.,2.06220058927162));
#31156=CARTESIAN_POINT('Ctrl Pts',(-0.746345871542696,-1.,2.06600523016401));
#31157=CARTESIAN_POINT('Ctrl Pts',(-0.746345871542696,1.,2.06600523016401));
#31158=CARTESIAN_POINT('Ctrl Pts',(-0.74583279137781,-1.,2.06854248895575));
#31159=CARTESIAN_POINT('Ctrl Pts',(-0.74583279137781,1.,2.06854248895575));
#31160=CARTESIAN_POINT('Ctrl Pts',(-0.745574324794401,-1.,2.0698113262342));
#31161=CARTESIAN_POINT('Ctrl Pts',(-0.745574324794401,1.,2.0698113262342));
#31162=CARTESIAN_POINT('',(-0.693717979106306,1.,1.60662857109684));
#31163=CARTESIAN_POINT('Ctrl Pts',(-0.693717979106306,1.,1.60662857109684));
#31164=CARTESIAN_POINT('Ctrl Pts',(-0.695712097881194,1.,1.61106790958151));
#31165=CARTESIAN_POINT('Ctrl Pts',(-0.699605146405088,1.,1.61974673472612));
#31166=CARTESIAN_POINT('Ctrl Pts',(-0.705159151988319,1.,1.63216541664676));
#31167=CARTESIAN_POINT('Ctrl Pts',(-0.711993139355394,1.,1.64752408832016));
#31168=CARTESIAN_POINT('Ctrl Pts',(-0.719585433804282,1.,1.6647288055568));
#31169=CARTESIAN_POINT('Ctrl Pts',(-0.726235967997433,1.,1.67996158455503));
#31170=CARTESIAN_POINT('Ctrl Pts',(-0.731963238697195,1.,1.69326921975743));
#31171=CARTESIAN_POINT('Ctrl Pts',(-0.736799665724771,1.,1.70473309006121));
#31172=CARTESIAN_POINT('Ctrl Pts',(-0.740795162032088,1.,1.71447789751927));
#31173=CARTESIAN_POINT('Ctrl Pts',(-0.744021445433764,1.,1.7226822991693));
#31174=CARTESIAN_POINT('Ctrl Pts',(-0.746574710096436,1.,1.72958533647399));
#31175=CARTESIAN_POINT('Ctrl Pts',(-0.748582462954855,1.,1.73550351679848));
#31176=CARTESIAN_POINT('Ctrl Pts',(-0.75019343597954,1.,1.74080458266705));
#31177=CARTESIAN_POINT('Ctrl Pts',(-0.751555614163629,1.,1.74585086852298));
#31178=CARTESIAN_POINT('Ctrl Pts',(-0.752797683531377,1.,1.75095139468809));
#31179=CARTESIAN_POINT('Ctrl Pts',(-0.75400925402848,1.,1.75631083600175));
#31180=CARTESIAN_POINT('Ctrl Pts',(-0.755220979975262,1.,1.7619781724032));
#31181=CARTESIAN_POINT('Ctrl Pts',(-0.756421896028403,1.,1.76789396003141));
#31182=CARTESIAN_POINT('Ctrl Pts',(-0.757578264077238,1.,1.77394167108342));
#31183=CARTESIAN_POINT('Ctrl Pts',(-0.75865062667738,1.,1.77999411220912));
#31184=CARTESIAN_POINT('Ctrl Pts',(-0.759614401109868,1.,1.78596964884526));
#31185=CARTESIAN_POINT('Ctrl Pts',(-0.760469555880425,1.,1.79185815610802));
#31186=CARTESIAN_POINT('Ctrl Pts',(-0.761229695230359,1.,1.79768986997735));
#31187=CARTESIAN_POINT('Ctrl Pts',(-0.761915336443516,1.,1.80351583877334));
#31188=CARTESIAN_POINT('Ctrl Pts',(-0.762546129464036,1.,1.80938551463989));
#31189=CARTESIAN_POINT('Ctrl Pts',(-0.763132003836783,1.,1.81532118405566));
#31190=CARTESIAN_POINT('Ctrl Pts',(-0.763673465462854,1.,1.82131873145297));
#31191=CARTESIAN_POINT('Ctrl Pts',(-0.764165902606055,1.,1.8273599120008));
#31192=CARTESIAN_POINT('Ctrl Pts',(-0.764602549687845,1.,1.8334207722714));
#31193=CARTESIAN_POINT('Ctrl Pts',(-0.764978057881687,1.,1.83948181064823));
#31194=CARTESIAN_POINT('Ctrl Pts',(-0.765291664861971,1.,1.8455369887591));
#31195=CARTESIAN_POINT('Ctrl Pts',(-0.765545710619023,1.,1.85158945130054));
#31196=CARTESIAN_POINT('Ctrl Pts',(-0.765744212909305,1.,1.85764741390391));
#31197=CARTESIAN_POINT('Ctrl Pts',(-0.765891519092557,1.,1.86372027063314));
#31198=CARTESIAN_POINT('Ctrl Pts',(-0.765990708546111,1.,1.86981398314345));
#31199=CARTESIAN_POINT('Ctrl Pts',(-0.766042837036759,1.,1.87592888967886));
#31200=CARTESIAN_POINT('Ctrl Pts',(-0.766047794851869,1.,1.88206215302561));
#31201=CARTESIAN_POINT('Ctrl Pts',(-0.76600483706209,1.,1.88820926433409));
#31202=CARTESIAN_POINT('Ctrl Pts',(-0.765913193856979,1.,1.89436577771389));
#31203=CARTESIAN_POINT('Ctrl Pts',(-0.765772772593395,1.,1.90052930393599));
#31204=CARTESIAN_POINT('Ctrl Pts',(-0.765584196937936,1.,1.90669961402362));
#31205=CARTESIAN_POINT('Ctrl Pts',(-0.765348465884739,1.,1.91287765805174));
#31206=CARTESIAN_POINT('Ctrl Pts',(-0.765066729667095,1.,1.91906491634197));
#31207=CARTESIAN_POINT('Ctrl Pts',(-0.764740025488189,1.,1.92526263537041));
#31208=CARTESIAN_POINT('Ctrl Pts',(-0.764369010673889,1.,1.93147105496367));
#31209=CARTESIAN_POINT('Ctrl Pts',(-0.763954049121393,1.,1.93768964875867));
#31210=CARTESIAN_POINT('Ctrl Pts',(-0.76349533353858,1.,1.94391746617626));
#31211=CARTESIAN_POINT('Ctrl Pts',(-0.762992990878774,1.,1.95015342590025));
#31212=CARTESIAN_POINT('Ctrl Pts',(-0.762447203806263,1.,1.95639665309893));
#31213=CARTESIAN_POINT('Ctrl Pts',(-0.761858300014575,1.,1.96264672744229));
#31214=CARTESIAN_POINT('Ctrl Pts',(-0.761226690483986,1.,1.96890351582545));
#31215=CARTESIAN_POINT('Ctrl Pts',(-0.760552825409855,1.,1.97516705321521));
#31216=CARTESIAN_POINT('Ctrl Pts',(-0.759837147452135,1.,1.98143741418156));
#31217=CARTESIAN_POINT('Ctrl Pts',(-0.759080037802243,1.,1.98771456680806));
#31218=CARTESIAN_POINT('Ctrl Pts',(-0.758281796766377,1.,1.9939983109871));
#31219=CARTESIAN_POINT('Ctrl Pts',(-0.757442676862341,1.,2.00028834739072));
#31220=CARTESIAN_POINT('Ctrl Pts',(-0.756562904646496,1.,2.00658431587682));
#31221=CARTESIAN_POINT('Ctrl Pts',(-0.7556427049581,1.,2.01288584328149));
#31222=CARTESIAN_POINT('Ctrl Pts',(-0.75468233072352,1.,2.01919259406003));
#31223=CARTESIAN_POINT('Ctrl Pts',(-0.753682061113766,1.,2.02550428623587));
#31224=CARTESIAN_POINT('Ctrl Pts',(-0.752642180488104,1.,2.03182068456467));
#31225=CARTESIAN_POINT('Ctrl Pts',(-0.751562963361384,1.,2.03814160092173));
#31226=CARTESIAN_POINT('Ctrl Pts',(-0.750444657874758,1.,2.04446689147754));
#31227=CARTESIAN_POINT('Ctrl Pts',(-0.749287468663053,1.,2.05079645591606));
#31228=CARTESIAN_POINT('Ctrl Pts',(-0.748091554181101,1.,2.05713023030263));
#31229=CARTESIAN_POINT('Ctrl Pts',(-0.747103932785504,1.,2.06220058927162));
#31230=CARTESIAN_POINT('Ctrl Pts',(-0.746345871542696,1.,2.06600523016401));
#31231=CARTESIAN_POINT('Ctrl Pts',(-0.74583279137781,1.,2.06854248895575));
#31232=CARTESIAN_POINT('Ctrl Pts',(-0.745574324794401,1.,2.0698113262342));
#31233=CARTESIAN_POINT('',(-0.693717979106306,0.,1.60662857109684));
#31234=CARTESIAN_POINT('Origin',(0.,0.,0.));
#31235=CARTESIAN_POINT('',(-0.892032620296855,1.,1.5055822144029));
#31236=CARTESIAN_POINT('Origin',(0.,1.,0.));
#31237=CARTESIAN_POINT('',(-0.892032620296855,0.,1.5055822144029));
#31238=CARTESIAN_POINT('Ctrl Pts',(-1.23627494547115,-1.,1.81978687191668));
#31239=CARTESIAN_POINT('Ctrl Pts',(-1.23627494547115,1.,1.81978687191668));
#31240=CARTESIAN_POINT('Ctrl Pts',(-1.23509651170476,-1.,1.81925017193666));
#31241=CARTESIAN_POINT('Ctrl Pts',(-1.23509651170476,1.,1.81925017193666));
#31242=CARTESIAN_POINT('Ctrl Pts',(-1.2327422452705,-1.,1.81817389921279));
#31243=CARTESIAN_POINT('Ctrl Pts',(-1.2327422452705,1.,1.81817389921279));
#31244=CARTESIAN_POINT('Ctrl Pts',(-1.2292186489137,-1.,1.8165508718364));
#31245=CARTESIAN_POINT('Ctrl Pts',(-1.2292186489137,1.,1.8165508718364));
#31246=CARTESIAN_POINT('Ctrl Pts',(-1.2245361330495,-1.,1.81436959210434));
#31247=CARTESIAN_POINT('Ctrl Pts',(-1.2245361330495,1.,1.81436959210434));
#31248=CARTESIAN_POINT('Ctrl Pts',(-1.21870906103557,-1.,1.81161420806656));
#31249=CARTESIAN_POINT('Ctrl Pts',(-1.21870906103557,1.,1.81161420806656));
#31250=CARTESIAN_POINT('Ctrl Pts',(-1.21290815708314,-1.,1.80882996917129));
#31251=CARTESIAN_POINT('Ctrl Pts',(-1.21290815708314,1.,1.80882996917129));
#31252=CARTESIAN_POINT('Ctrl Pts',(-1.20713356605475,-1.,1.80601678480707));
#31253=CARTESIAN_POINT('Ctrl Pts',(-1.20713356605475,1.,1.80601678480707));
#31254=CARTESIAN_POINT('Ctrl Pts',(-1.20138548938974,-1.,1.80317454838603));
#31255=CARTESIAN_POINT('Ctrl Pts',(-1.20138548938974,1.,1.80317454838603));
#31256=CARTESIAN_POINT('Ctrl Pts',(-1.19566418930242,-1.,1.80030314369879));
#31257=CARTESIAN_POINT('Ctrl Pts',(-1.19566418930242,1.,1.80030314369879));
#31258=CARTESIAN_POINT('Ctrl Pts',(-1.18996997934445,-1.,1.79740245923478));
#31259=CARTESIAN_POINT('Ctrl Pts',(-1.18996997934445,1.,1.79740245923478));
#31260=CARTESIAN_POINT('Ctrl Pts',(-1.18430321697432,-1.,1.79447240321515));
#31261=CARTESIAN_POINT('Ctrl Pts',(-1.18430321697432,1.,1.79447240321515));
#31262=CARTESIAN_POINT('Ctrl Pts',(-1.17866429440809,-1.,1.79151291552689));
#31263=CARTESIAN_POINT('Ctrl Pts',(-1.17866429440809,1.,1.79151291552689));
#31264=CARTESIAN_POINT('Ctrl Pts',(-1.17305363177328,-1.,1.78852398877616));
#31265=CARTESIAN_POINT('Ctrl Pts',(-1.17305363177328,1.,1.78852398877616));
#31266=CARTESIAN_POINT('Ctrl Pts',(-1.16747166312303,-1.,1.78550566040443));
#31267=CARTESIAN_POINT('Ctrl Pts',(-1.16747166312303,1.,1.78550566040443));
#31268=CARTESIAN_POINT('Ctrl Pts',(-1.16191881298499,-1.,1.78245795881009));
#31269=CARTESIAN_POINT('Ctrl Pts',(-1.16191881298499,1.,1.78245795881009));
#31270=CARTESIAN_POINT('Ctrl Pts',(-1.15639547194698,-1.,1.77938085564275));
#31271=CARTESIAN_POINT('Ctrl Pts',(-1.15639547194698,1.,1.77938085564275));
#31272=CARTESIAN_POINT('Ctrl Pts',(-1.15090197841515,-1.,1.7762742255701));
#31273=CARTESIAN_POINT('Ctrl Pts',(-1.15090197841515,1.,1.7762742255701));
#31274=CARTESIAN_POINT('Ctrl Pts',(-1.1454385822692,-1.,1.77313777896194));
#31275=CARTESIAN_POINT('Ctrl Pts',(-1.1454385822692,1.,1.77313777896194));
#31276=CARTESIAN_POINT('Ctrl Pts',(-1.14000548336975,-1.,1.76997111386769));
#31277=CARTESIAN_POINT('Ctrl Pts',(-1.14000548336975,1.,1.76997111386769));
#31278=CARTESIAN_POINT('Ctrl Pts',(-1.1346029180462,-1.,1.76677384551862));
#31279=CARTESIAN_POINT('Ctrl Pts',(-1.1346029180462,1.,1.76677384551862));
#31280=CARTESIAN_POINT('Ctrl Pts',(-1.12923123555075,-1.,1.7635457196617));
#31281=CARTESIAN_POINT('Ctrl Pts',(-1.12923123555075,1.,1.7635457196617));
#31282=CARTESIAN_POINT('Ctrl Pts',(-1.12389096855086,-1.,1.76028671825096));
#31283=CARTESIAN_POINT('Ctrl Pts',(-1.12389096855086,1.,1.76028671825096));
#31284=CARTESIAN_POINT('Ctrl Pts',(-1.11858293216763,-1.,1.75699720772105));
#31285=CARTESIAN_POINT('Ctrl Pts',(-1.11858293216763,1.,1.75699720772105));
#31286=CARTESIAN_POINT('Ctrl Pts',(-1.11330807582551,-1.,1.7536777209463));
#31287=CARTESIAN_POINT('Ctrl Pts',(-1.11330807582551,1.,1.7536777209463));
#31288=CARTESIAN_POINT('Ctrl Pts',(-1.10806728183007,-1.,1.7503286607592));
#31289=CARTESIAN_POINT('Ctrl Pts',(-1.10806728183007,1.,1.7503286607592));
#31290=CARTESIAN_POINT('Ctrl Pts',(-1.10286118991143,-1.,1.74695004214923));
#31291=CARTESIAN_POINT('Ctrl Pts',(-1.10286118991143,1.,1.74695004214923));
#31292=CARTESIAN_POINT('Ctrl Pts',(-1.09768999241225,-1.,1.74354119236208));
#31293=CARTESIAN_POINT('Ctrl Pts',(-1.09768999241225,1.,1.74354119236208));
#31294=CARTESIAN_POINT('Ctrl Pts',(-1.09255329056493,-1.,1.74010053962247));
#31295=CARTESIAN_POINT('Ctrl Pts',(-1.09255329056493,1.,1.74010053962247));
#31296=CARTESIAN_POINT('Ctrl Pts',(-1.08745056285427,-1.,1.73662628326091));
#31297=CARTESIAN_POINT('Ctrl Pts',(-1.08745056285427,1.,1.73662628326091));
#31298=CARTESIAN_POINT('Ctrl Pts',(-1.08238162784749,-1.,1.73311705663407));
#31299=CARTESIAN_POINT('Ctrl Pts',(-1.08238162784749,1.,1.73311705663407));
#31300=CARTESIAN_POINT('Ctrl Pts',(-1.0773470373727,-1.,1.72957248977424));
#31301=CARTESIAN_POINT('Ctrl Pts',(-1.0773470373727,1.,1.72957248977424));
#31302=CARTESIAN_POINT('Ctrl Pts',(-1.07234866990252,-1.,1.72599406198488));
#31303=CARTESIAN_POINT('Ctrl Pts',(-1.07234866990252,1.,1.72599406198488));
#31304=CARTESIAN_POINT('Ctrl Pts',(-1.06738966975462,-1.,1.72238500928453));
#31305=CARTESIAN_POINT('Ctrl Pts',(-1.06738966975462,1.,1.72238500928453));
#31306=CARTESIAN_POINT('Ctrl Pts',(-1.06247324680647,-1.,1.71874858456904));
#31307=CARTESIAN_POINT('Ctrl Pts',(-1.06247324680647,1.,1.71874858456904));
#31308=CARTESIAN_POINT('Ctrl Pts',(-1.05760163192479,-1.,1.7150865442702));
#31309=CARTESIAN_POINT('Ctrl Pts',(-1.05760163192479,1.,1.7150865442702));
#31310=CARTESIAN_POINT('Ctrl Pts',(-1.05277517202855,-1.,1.71139783543989));
#31311=CARTESIAN_POINT('Ctrl Pts',(-1.05277517202855,1.,1.71139783543989));
#31312=CARTESIAN_POINT('Ctrl Pts',(-1.04799085404995,-1.,1.70767646263649));
#31313=CARTESIAN_POINT('Ctrl Pts',(-1.04799085404995,1.,1.70767646263649));
#31314=CARTESIAN_POINT('Ctrl Pts',(-1.04324363334554,-1.,1.70391338707982));
#31315=CARTESIAN_POINT('Ctrl Pts',(-1.04324363334554,1.,1.70391338707982));
#31316=CARTESIAN_POINT('Ctrl Pts',(-1.03852922490789,-1.,1.70010052930962));
#31317=CARTESIAN_POINT('Ctrl Pts',(-1.03852922490789,1.,1.70010052930962));
#31318=CARTESIAN_POINT('Ctrl Pts',(-1.03384646003588,-1.,1.69623414782771));
#31319=CARTESIAN_POINT('Ctrl Pts',(-1.03384646003588,1.,1.69623414782771));
#31320=CARTESIAN_POINT('Ctrl Pts',(-1.02919977579147,-1.,1.69231840863458));
#31321=CARTESIAN_POINT('Ctrl Pts',(-1.02919977579147,1.,1.69231840863458));
#31322=CARTESIAN_POINT('Ctrl Pts',(-1.02460180535255,-1.,1.68836910178447));
#31323=CARTESIAN_POINT('Ctrl Pts',(-1.02460180535255,1.,1.68836910178447));
#31324=CARTESIAN_POINT('Ctrl Pts',(-1.02006795074201,-1.,1.68440578021706));
#31325=CARTESIAN_POINT('Ctrl Pts',(-1.02006795074201,1.,1.68440578021706));
#31326=CARTESIAN_POINT('Ctrl Pts',(-1.01561026162773,-1.,1.68044289894798));
#31327=CARTESIAN_POINT('Ctrl Pts',(-1.01561026162773,1.,1.68044289894798));
#31328=CARTESIAN_POINT('Ctrl Pts',(-1.01123236493511,-1.,1.67648246776464));
#31329=CARTESIAN_POINT('Ctrl Pts',(-1.01123236493511,1.,1.67648246776464));
#31330=CARTESIAN_POINT('Ctrl Pts',(-1.00692206696414,-1.,1.67250335383293));
#31331=CARTESIAN_POINT('Ctrl Pts',(-1.00692206696414,1.,1.67250335383293));
#31332=CARTESIAN_POINT('Ctrl Pts',(-1.00265091003727,-1.,1.66846059277303));
#31333=CARTESIAN_POINT('Ctrl Pts',(-1.00265091003727,1.,1.66846059277303));
#31334=CARTESIAN_POINT('Ctrl Pts',(-0.998389654952758,-1.,1.66430758030376));
#31335=CARTESIAN_POINT('Ctrl Pts',(-0.998389654952758,1.,1.66430758030376));
#31336=CARTESIAN_POINT('Ctrl Pts',(-0.994121836661306,-1.,1.66001553809947));
#31337=CARTESIAN_POINT('Ctrl Pts',(-0.994121836661306,1.,1.66001553809947));
#31338=CARTESIAN_POINT('Ctrl Pts',(-0.989855627854165,-1.,1.65559044289699));
#31339=CARTESIAN_POINT('Ctrl Pts',(-0.989855627854165,1.,1.65559044289699));
#31340=CARTESIAN_POINT('Ctrl Pts',(-0.985642622920821,-1.,1.65110016612638));
#31341=CARTESIAN_POINT('Ctrl Pts',(-0.985642622920821,1.,1.65110016612638));
#31342=CARTESIAN_POINT('Ctrl Pts',(-0.981562530939489,-1.,1.64665139190656));
#31343=CARTESIAN_POINT('Ctrl Pts',(-0.981562530939489,1.,1.64665139190656));
#31344=CARTESIAN_POINT('Ctrl Pts',(-0.977689794119416,-1.,1.64233990826687));
#31345=CARTESIAN_POINT('Ctrl Pts',(-0.977689794119416,1.,1.64233990826687));
#31346=CARTESIAN_POINT('Ctrl Pts',(-0.974066058287418,-1.,1.63820952658144));
#31347=CARTESIAN_POINT('Ctrl Pts',(-0.974066058287418,1.,1.63820952658144));
#31348=CARTESIAN_POINT('Ctrl Pts',(-0.970669715997509,-1.,1.63420665729798));
#31349=CARTESIAN_POINT('Ctrl Pts',(-0.970669715997509,1.,1.63420665729798));
#31350=CARTESIAN_POINT('Ctrl Pts',(-0.967387853230345,-1.,1.63013849959461));
#31351=CARTESIAN_POINT('Ctrl Pts',(-0.967387853230345,1.,1.63013849959461));
#31352=CARTESIAN_POINT('Ctrl Pts',(-0.964046107040536,-1.,1.62571930670187));
#31353=CARTESIAN_POINT('Ctrl Pts',(-0.964046107040536,1.,1.62571930670187));
#31354=CARTESIAN_POINT('Ctrl Pts',(-0.960438326101729,-1.,1.62061638140221));
#31355=CARTESIAN_POINT('Ctrl Pts',(-0.960438326101729,1.,1.62061638140221));
#31356=CARTESIAN_POINT('Ctrl Pts',(-0.956354422920671,-1.,1.61449324337085));
#31357=CARTESIAN_POINT('Ctrl Pts',(-0.956354422920671,1.,1.61449324337085));
#31358=CARTESIAN_POINT('Ctrl Pts',(-0.951613284356035,-1.,1.60706069896936));
#31359=CARTESIAN_POINT('Ctrl Pts',(-0.951613284356035,1.,1.60706069896936));
#31360=CARTESIAN_POINT('Ctrl Pts',(-0.946078063315257,-1.,1.59810042043673));
#31361=CARTESIAN_POINT('Ctrl Pts',(-0.946078063315257,1.,1.59810042043673));
#31362=CARTESIAN_POINT('Ctrl Pts',(-0.939646377893399,-1.,1.58744937487176));
#31363=CARTESIAN_POINT('Ctrl Pts',(-0.939646377893399,1.,1.58744937487176));
#31364=CARTESIAN_POINT('Ctrl Pts',(-0.932246680108685,-1.,1.57499388382243));
#31365=CARTESIAN_POINT('Ctrl Pts',(-0.932246680108685,1.,1.57499388382243));
#31366=CARTESIAN_POINT('Ctrl Pts',(-0.923832188944341,-1.,1.56065988578893));
#31367=CARTESIAN_POINT('Ctrl Pts',(-0.923832188944341,1.,1.56065988578893));
#31368=CARTESIAN_POINT('Ctrl Pts',(-0.914375919026456,-1.,1.54440491149498));
#31369=CARTESIAN_POINT('Ctrl Pts',(-0.914375919026456,1.,1.54440491149498));
#31370=CARTESIAN_POINT('Ctrl Pts',(-0.905967409625651,-1.,1.52984849887993));
#31371=CARTESIAN_POINT('Ctrl Pts',(-0.905967409625651,1.,1.52984849887993));
#31372=CARTESIAN_POINT('Ctrl Pts',(-0.899185047483511,-1.,1.51805569590094));
#31373=CARTESIAN_POINT('Ctrl Pts',(-0.899185047483511,1.,1.51805569590094));
#31374=CARTESIAN_POINT('Ctrl Pts',(-0.894452006964543,-1.,1.50980486806688));
#31375=CARTESIAN_POINT('Ctrl Pts',(-0.894452006964543,1.,1.50980486806688));
#31376=CARTESIAN_POINT('Ctrl Pts',(-0.892032620296855,-1.,1.5055822144029));
#31377=CARTESIAN_POINT('Ctrl Pts',(-0.892032620296855,1.,1.5055822144029));
#31378=CARTESIAN_POINT('',(-1.23627494547115,1.,1.81978687191668));
#31379=CARTESIAN_POINT('Ctrl Pts',(-1.23627494547115,1.,1.81978687191668));
#31380=CARTESIAN_POINT('Ctrl Pts',(-1.23509651170476,1.,1.81925017193666));
#31381=CARTESIAN_POINT('Ctrl Pts',(-1.2327422452705,1.,1.81817389921279));
#31382=CARTESIAN_POINT('Ctrl Pts',(-1.2292186489137,1.,1.8165508718364));
#31383=CARTESIAN_POINT('Ctrl Pts',(-1.2245361330495,1.,1.81436959210434));
#31384=CARTESIAN_POINT('Ctrl Pts',(-1.21870906103557,1.,1.81161420806656));
#31385=CARTESIAN_POINT('Ctrl Pts',(-1.21290815708314,1.,1.80882996917129));
#31386=CARTESIAN_POINT('Ctrl Pts',(-1.20713356605475,1.,1.80601678480707));
#31387=CARTESIAN_POINT('Ctrl Pts',(-1.20138548938974,1.,1.80317454838603));
#31388=CARTESIAN_POINT('Ctrl Pts',(-1.19566418930242,1.,1.80030314369879));
#31389=CARTESIAN_POINT('Ctrl Pts',(-1.18996997934445,1.,1.79740245923478));
#31390=CARTESIAN_POINT('Ctrl Pts',(-1.18430321697432,1.,1.79447240321515));
#31391=CARTESIAN_POINT('Ctrl Pts',(-1.17866429440809,1.,1.79151291552689));
#31392=CARTESIAN_POINT('Ctrl Pts',(-1.17305363177328,1.,1.78852398877616));
#31393=CARTESIAN_POINT('Ctrl Pts',(-1.16747166312303,1.,1.78550566040443));
#31394=CARTESIAN_POINT('Ctrl Pts',(-1.16191881298499,1.,1.78245795881009));
#31395=CARTESIAN_POINT('Ctrl Pts',(-1.15639547194698,1.,1.77938085564275));
#31396=CARTESIAN_POINT('Ctrl Pts',(-1.15090197841515,1.,1.7762742255701));
#31397=CARTESIAN_POINT('Ctrl Pts',(-1.1454385822692,1.,1.77313777896194));
#31398=CARTESIAN_POINT('Ctrl Pts',(-1.14000548336975,1.,1.76997111386769));
#31399=CARTESIAN_POINT('Ctrl Pts',(-1.1346029180462,1.,1.76677384551862));
#31400=CARTESIAN_POINT('Ctrl Pts',(-1.12923123555075,1.,1.7635457196617));
#31401=CARTESIAN_POINT('Ctrl Pts',(-1.12389096855086,1.,1.76028671825096));
#31402=CARTESIAN_POINT('Ctrl Pts',(-1.11858293216763,1.,1.75699720772105));
#31403=CARTESIAN_POINT('Ctrl Pts',(-1.11330807582551,1.,1.7536777209463));
#31404=CARTESIAN_POINT('Ctrl Pts',(-1.10806728183007,1.,1.7503286607592));
#31405=CARTESIAN_POINT('Ctrl Pts',(-1.10286118991143,1.,1.74695004214923));
#31406=CARTESIAN_POINT('Ctrl Pts',(-1.09768999241225,1.,1.74354119236208));
#31407=CARTESIAN_POINT('Ctrl Pts',(-1.09255329056493,1.,1.74010053962247));
#31408=CARTESIAN_POINT('Ctrl Pts',(-1.08745056285427,1.,1.73662628326091));
#31409=CARTESIAN_POINT('Ctrl Pts',(-1.08238162784749,1.,1.73311705663407));
#31410=CARTESIAN_POINT('Ctrl Pts',(-1.0773470373727,1.,1.72957248977424));
#31411=CARTESIAN_POINT('Ctrl Pts',(-1.07234866990252,1.,1.72599406198488));
#31412=CARTESIAN_POINT('Ctrl Pts',(-1.06738966975462,1.,1.72238500928453));
#31413=CARTESIAN_POINT('Ctrl Pts',(-1.06247324680647,1.,1.71874858456904));
#31414=CARTESIAN_POINT('Ctrl Pts',(-1.05760163192479,1.,1.7150865442702));
#31415=CARTESIAN_POINT('Ctrl Pts',(-1.05277517202855,1.,1.71139783543989));
#31416=CARTESIAN_POINT('Ctrl Pts',(-1.04799085404995,1.,1.70767646263649));
#31417=CARTESIAN_POINT('Ctrl Pts',(-1.04324363334554,1.,1.70391338707982));
#31418=CARTESIAN_POINT('Ctrl Pts',(-1.03852922490789,1.,1.70010052930962));
#31419=CARTESIAN_POINT('Ctrl Pts',(-1.03384646003588,1.,1.69623414782771));
#31420=CARTESIAN_POINT('Ctrl Pts',(-1.02919977579147,1.,1.69231840863458));
#31421=CARTESIAN_POINT('Ctrl Pts',(-1.02460180535255,1.,1.68836910178447));
#31422=CARTESIAN_POINT('Ctrl Pts',(-1.02006795074201,1.,1.68440578021706));
#31423=CARTESIAN_POINT('Ctrl Pts',(-1.01561026162773,1.,1.68044289894798));
#31424=CARTESIAN_POINT('Ctrl Pts',(-1.01123236493511,1.,1.67648246776464));
#31425=CARTESIAN_POINT('Ctrl Pts',(-1.00692206696414,1.,1.67250335383293));
#31426=CARTESIAN_POINT('Ctrl Pts',(-1.00265091003727,1.,1.66846059277303));
#31427=CARTESIAN_POINT('Ctrl Pts',(-0.998389654952758,1.,1.66430758030376));
#31428=CARTESIAN_POINT('Ctrl Pts',(-0.994121836661306,1.,1.66001553809947));
#31429=CARTESIAN_POINT('Ctrl Pts',(-0.989855627854165,1.,1.65559044289699));
#31430=CARTESIAN_POINT('Ctrl Pts',(-0.985642622920821,1.,1.65110016612638));
#31431=CARTESIAN_POINT('Ctrl Pts',(-0.981562530939489,1.,1.64665139190656));
#31432=CARTESIAN_POINT('Ctrl Pts',(-0.977689794119416,1.,1.64233990826687));
#31433=CARTESIAN_POINT('Ctrl Pts',(-0.974066058287418,1.,1.63820952658144));
#31434=CARTESIAN_POINT('Ctrl Pts',(-0.970669715997509,1.,1.63420665729798));
#31435=CARTESIAN_POINT('Ctrl Pts',(-0.967387853230345,1.,1.63013849959461));
#31436=CARTESIAN_POINT('Ctrl Pts',(-0.964046107040536,1.,1.62571930670187));
#31437=CARTESIAN_POINT('Ctrl Pts',(-0.960438326101729,1.,1.62061638140221));
#31438=CARTESIAN_POINT('Ctrl Pts',(-0.956354422920671,1.,1.61449324337085));
#31439=CARTESIAN_POINT('Ctrl Pts',(-0.951613284356035,1.,1.60706069896936));
#31440=CARTESIAN_POINT('Ctrl Pts',(-0.946078063315257,1.,1.59810042043673));
#31441=CARTESIAN_POINT('Ctrl Pts',(-0.939646377893399,1.,1.58744937487176));
#31442=CARTESIAN_POINT('Ctrl Pts',(-0.932246680108685,1.,1.57499388382243));
#31443=CARTESIAN_POINT('Ctrl Pts',(-0.923832188944341,1.,1.56065988578893));
#31444=CARTESIAN_POINT('Ctrl Pts',(-0.914375919026456,1.,1.54440491149498));
#31445=CARTESIAN_POINT('Ctrl Pts',(-0.905967409625651,1.,1.52984849887993));
#31446=CARTESIAN_POINT('Ctrl Pts',(-0.899185047483511,1.,1.51805569590094));
#31447=CARTESIAN_POINT('Ctrl Pts',(-0.894452006964543,1.,1.50980486806688));
#31448=CARTESIAN_POINT('Ctrl Pts',(-0.892032620296855,1.,1.5055822144029));
#31449=CARTESIAN_POINT('',(-1.23627494547115,0.,1.81978687191668));
#31450=CARTESIAN_POINT('Origin',(-1.34869019493419,0.,1.73811241238545));
#31451=CARTESIAN_POINT('',(-1.34869019493419,1.,1.73811241238545));
#31452=CARTESIAN_POINT('',(-1.23627494547115,1.,1.81978687191668));
#31453=CARTESIAN_POINT('',(-1.34869019493419,0.,1.73811241238545));
#31454=CARTESIAN_POINT('Ctrl Pts',(-1.15624053661742,-1.,1.31362392696032));
#31455=CARTESIAN_POINT('Ctrl Pts',(-1.15624053661742,1.,1.31362392696032));
#31456=CARTESIAN_POINT('Ctrl Pts',(-1.15950888730809,-1.,1.31722977216397));
#31457=CARTESIAN_POINT('Ctrl Pts',(-1.15950888730809,1.,1.31722977216397));
#31458=CARTESIAN_POINT('Ctrl Pts',(-1.16589330093588,-1.,1.32428080721772));
#31459=CARTESIAN_POINT('Ctrl Pts',(-1.16589330093588,1.,1.32428080721772));
#31460=CARTESIAN_POINT('Ctrl Pts',(-1.17501305789857,-1.,1.33437539347008));
#31461=CARTESIAN_POINT('Ctrl Pts',(-1.17501305789857,1.,1.33437539347008));
#31462=CARTESIAN_POINT('Ctrl Pts',(-1.18625865667441,-1.,1.34687054001093));
#31463=CARTESIAN_POINT('Ctrl Pts',(-1.18625865667441,1.,1.34687054001093));
#31464=CARTESIAN_POINT('Ctrl Pts',(-1.1987959077932,-1.,1.36088705043885));
#31465=CARTESIAN_POINT('Ctrl Pts',(-1.1987959077932,1.,1.36088705043885));
#31466=CARTESIAN_POINT('Ctrl Pts',(-1.20982812925645,-1.,1.37331915607905));
#31467=CARTESIAN_POINT('Ctrl Pts',(-1.20982812925645,1.,1.37331915607905));
#31468=CARTESIAN_POINT('Ctrl Pts',(-1.21938737280852,-1.,1.38420564527715));
#31469=CARTESIAN_POINT('Ctrl Pts',(-1.21938737280852,1.,1.38420564527715));
#31470=CARTESIAN_POINT('Ctrl Pts',(-1.22752961899387,-1.,1.39361389568796));
#31471=CARTESIAN_POINT('Ctrl Pts',(-1.22752961899387,1.,1.39361389568796));
#31472=CARTESIAN_POINT('Ctrl Pts',(-1.23434087290423,-1.,1.40164708206106));
#31473=CARTESIAN_POINT('Ctrl Pts',(-1.23434087290423,1.,1.40164708206106));
#31474=CARTESIAN_POINT('Ctrl Pts',(-1.23994455029534,-1.,1.40845295531283));
#31475=CARTESIAN_POINT('Ctrl Pts',(-1.23994455029534,1.,1.40845295531283));
#31476=CARTESIAN_POINT('Ctrl Pts',(-1.24450600513056,-1.,1.41422913175179));
#31477=CARTESIAN_POINT('Ctrl Pts',(-1.24450600513056,1.,1.41422913175179));
#31478=CARTESIAN_POINT('Ctrl Pts',(-1.24824430986571,-1.,1.41923722596025));
#31479=CARTESIAN_POINT('Ctrl Pts',(-1.24824430986571,1.,1.41923722596025));
#31480=CARTESIAN_POINT('Ctrl Pts',(-1.2514145557001,-1.,1.42378102115575));
#31481=CARTESIAN_POINT('Ctrl Pts',(-1.2514145557001,1.,1.42378102115575));
#31482=CARTESIAN_POINT('Ctrl Pts',(-1.25426945222639,-1.,1.42815938799387));
#31483=CARTESIAN_POINT('Ctrl Pts',(-1.25426945222639,1.,1.42815938799387));
#31484=CARTESIAN_POINT('Ctrl Pts',(-1.25702687965755,-1.,1.43262645609691));
#31485=CARTESIAN_POINT('Ctrl Pts',(-1.25702687965755,1.,1.43262645609691));
#31486=CARTESIAN_POINT('Ctrl Pts',(-1.25983531012005,-1.,1.43734919180848));
#31487=CARTESIAN_POINT('Ctrl Pts',(-1.25983531012005,1.,1.43734919180848));
#31488=CARTESIAN_POINT('Ctrl Pts',(-1.26273903323859,-1.,1.44236470511303));
#31489=CARTESIAN_POINT('Ctrl Pts',(-1.26273903323859,1.,1.44236470511303));
#31490=CARTESIAN_POINT('Ctrl Pts',(-1.26570925118868,-1.,1.44761985001662));
#31491=CARTESIAN_POINT('Ctrl Pts',(-1.26570925118868,1.,1.44761985001662));
#31492=CARTESIAN_POINT('Ctrl Pts',(-1.2686778680489,-1.,1.45301422764247));
#31493=CARTESIAN_POINT('Ctrl Pts',(-1.2686778680489,1.,1.45301422764247));
#31494=CARTESIAN_POINT('Ctrl Pts',(-1.27156805265289,-1.,1.45843906294697));
#31495=CARTESIAN_POINT('Ctrl Pts',(-1.27156805265289,1.,1.45843906294697));
#31496=CARTESIAN_POINT('Ctrl Pts',(-1.27433119897822,-1.,1.46382431332476));
#31497=CARTESIAN_POINT('Ctrl Pts',(-1.27433119897822,1.,1.46382431332476));
#31498=CARTESIAN_POINT('Ctrl Pts',(-1.27696414831089,-1.,1.46916035917133));
#31499=CARTESIAN_POINT('Ctrl Pts',(-1.27696414831089,1.,1.46916035917133));
#31500=CARTESIAN_POINT('Ctrl Pts',(-1.2794891824849,-1.,1.4744717526707));
#31501=CARTESIAN_POINT('Ctrl Pts',(-1.2794891824849,1.,1.4744717526707));
#31502=CARTESIAN_POINT('Ctrl Pts',(-1.28194158939517,-1.,1.47980070347095));
#31503=CARTESIAN_POINT('Ctrl Pts',(-1.28194158939517,1.,1.47980070347095));
#31504=CARTESIAN_POINT('Ctrl Pts',(-1.28435533880201,-1.,1.4851881711891));
#31505=CARTESIAN_POINT('Ctrl Pts',(-1.28435533880201,1.,1.4851881711891));
#31506=CARTESIAN_POINT('Ctrl Pts',(-1.2867467611644,-1.,1.4906522831278));
#31507=CARTESIAN_POINT('Ctrl Pts',(-1.2867467611644,1.,1.4906522831278));
#31508=CARTESIAN_POINT('Ctrl Pts',(-1.28911506584254,-1.,1.49618896881754));
#31509=CARTESIAN_POINT('Ctrl Pts',(-1.28911506584254,1.,1.49618896881754));
#31510=CARTESIAN_POINT('Ctrl Pts',(-1.29145022885181,-1.,1.50178230149776));
#31511=CARTESIAN_POINT('Ctrl Pts',(-1.29145022885181,1.,1.50178230149776));
#31512=CARTESIAN_POINT('Ctrl Pts',(-1.29373841372842,-1.,1.50741159078365));
#31513=CARTESIAN_POINT('Ctrl Pts',(-1.29373841372842,1.,1.50741159078365));
#31514=CARTESIAN_POINT('Ctrl Pts',(-1.29596850710509,-1.,1.51305994241402));
#31515=CARTESIAN_POINT('Ctrl Pts',(-1.29596850710509,1.,1.51305994241402));
#31516=CARTESIAN_POINT('Ctrl Pts',(-1.29813791800747,-1.,1.51872184912724));
#31517=CARTESIAN_POINT('Ctrl Pts',(-1.29813791800747,1.,1.51872184912724));
#31518=CARTESIAN_POINT('Ctrl Pts',(-1.30024984366328,-1.,1.52439957861062));
#31519=CARTESIAN_POINT('Ctrl Pts',(-1.30024984366328,1.,1.52439957861062));
#31520=CARTESIAN_POINT('Ctrl Pts',(-1.30231064395568,-1.,1.53009970283891));
#31521=CARTESIAN_POINT('Ctrl Pts',(-1.30231064395568,1.,1.53009970283891));
#31522=CARTESIAN_POINT('Ctrl Pts',(-1.30432735639489,-1.,1.53582981268977));
#31523=CARTESIAN_POINT('Ctrl Pts',(-1.30432735639489,1.,1.53582981268977));
#31524=CARTESIAN_POINT('Ctrl Pts',(-1.30630475189556,-1.,1.54159462645432));
#31525=CARTESIAN_POINT('Ctrl Pts',(-1.30630475189556,1.,1.54159462645432));
#31526=CARTESIAN_POINT('Ctrl Pts',(-1.30824393907473,-1.,1.54739413957185));
#31527=CARTESIAN_POINT('Ctrl Pts',(-1.30824393907473,1.,1.54739413957185));
#31528=CARTESIAN_POINT('Ctrl Pts',(-1.31014393684222,-1.,1.55322568759481));
#31529=CARTESIAN_POINT('Ctrl Pts',(-1.31014393684222,1.,1.55322568759481));
#31530=CARTESIAN_POINT('Ctrl Pts',(-1.31200264341696,-1.,1.55908521254821));
#31531=CARTESIAN_POINT('Ctrl Pts',(-1.31200264341696,1.,1.55908521254821));
#31532=CARTESIAN_POINT('Ctrl Pts',(-1.31381795281002,-1.,1.56496872402353));
#31533=CARTESIAN_POINT('Ctrl Pts',(-1.31381795281002,1.,1.56496872402353));
#31534=CARTESIAN_POINT('Ctrl Pts',(-1.31558903860016,-1.,1.57087397835723));
#31535=CARTESIAN_POINT('Ctrl Pts',(-1.31558903860016,1.,1.57087397835723));
#31536=CARTESIAN_POINT('Ctrl Pts',(-1.31731642317187,-1.,1.5768005650559));
#31537=CARTESIAN_POINT('Ctrl Pts',(-1.31731642317187,1.,1.5768005650559));
#31538=CARTESIAN_POINT('Ctrl Pts',(-1.31900135021432,-1.,1.58274907898834));
#31539=CARTESIAN_POINT('Ctrl Pts',(-1.31900135021432,1.,1.58274907898834));
#31540=CARTESIAN_POINT('Ctrl Pts',(-1.32064537110892,-1.,1.58872057258245));
#31541=CARTESIAN_POINT('Ctrl Pts',(-1.32064537110892,1.,1.58872057258245));
#31542=CARTESIAN_POINT('Ctrl Pts',(-1.32224985747682,-1.,1.59471591079403));
#31543=CARTESIAN_POINT('Ctrl Pts',(-1.32224985747682,1.,1.59471591079403));
#31544=CARTESIAN_POINT('Ctrl Pts',(-1.32381550858256,-1.,1.60073511858687));
#31545=CARTESIAN_POINT('Ctrl Pts',(-1.32381550858256,1.,1.60073511858687));
#31546=CARTESIAN_POINT('Ctrl Pts',(-1.32534250785782,-1.,1.60677758290954));
#31547=CARTESIAN_POINT('Ctrl Pts',(-1.32534250785782,1.,1.60677758290954));
#31548=CARTESIAN_POINT('Ctrl Pts',(-1.32683074483356,-1.,1.6128423401575));
#31549=CARTESIAN_POINT('Ctrl Pts',(-1.32683074483356,1.,1.6128423401575));
#31550=CARTESIAN_POINT('Ctrl Pts',(-1.32828000610449,-1.,1.61892832270724));
#31551=CARTESIAN_POINT('Ctrl Pts',(-1.32828000610449,1.,1.61892832270724));
#31552=CARTESIAN_POINT('Ctrl Pts',(-1.3296901950568,-1.,1.62503464209797));
#31553=CARTESIAN_POINT('Ctrl Pts',(-1.3296901950568,1.,1.62503464209797));
#31554=CARTESIAN_POINT('Ctrl Pts',(-1.33106149345645,-1.,1.63116079730923));
#31555=CARTESIAN_POINT('Ctrl Pts',(-1.33106149345645,1.,1.63116079730923));
#31556=CARTESIAN_POINT('Ctrl Pts',(-1.33239425103724,-1.,1.63730653475089));
#31557=CARTESIAN_POINT('Ctrl Pts',(-1.33239425103724,1.,1.63730653475089));
#31558=CARTESIAN_POINT('Ctrl Pts',(-1.33368890676572,-1.,1.6434717485603));
#31559=CARTESIAN_POINT('Ctrl Pts',(-1.33368890676572,1.,1.6434717485603));
#31560=CARTESIAN_POINT('Ctrl Pts',(-1.33494590467993,-1.,1.6496563728683));
#31561=CARTESIAN_POINT('Ctrl Pts',(-1.33494590467993,1.,1.6496563728683));
#31562=CARTESIAN_POINT('Ctrl Pts',(-1.33616559745172,-1.,1.65586025952593));
#31563=CARTESIAN_POINT('Ctrl Pts',(-1.33616559745172,1.,1.65586025952593));
#31564=CARTESIAN_POINT('Ctrl Pts',(-1.33734820885262,-1.,1.66208312541983));
#31565=CARTESIAN_POINT('Ctrl Pts',(-1.33734820885262,1.,1.66208312541983));
#31566=CARTESIAN_POINT('Ctrl Pts',(-1.33849388654388,-1.,1.66832460783989));
#31567=CARTESIAN_POINT('Ctrl Pts',(-1.33849388654388,1.,1.66832460783989));
#31568=CARTESIAN_POINT('Ctrl Pts',(-1.3396027347034,-1.,1.67458429426086));
#31569=CARTESIAN_POINT('Ctrl Pts',(-1.3396027347034,1.,1.67458429426086));
#31570=CARTESIAN_POINT('Ctrl Pts',(-1.34067485185203,-1.,1.68086176030362));
#31571=CARTESIAN_POINT('Ctrl Pts',(-1.34067485185203,1.,1.68086176030362));
#31572=CARTESIAN_POINT('Ctrl Pts',(-1.341710374848,-1.,1.68715660868764));
#31573=CARTESIAN_POINT('Ctrl Pts',(-1.341710374848,1.,1.68715660868764));
#31574=CARTESIAN_POINT('Ctrl Pts',(-1.34270948206319,-1.,1.6934684849687));
#31575=CARTESIAN_POINT('Ctrl Pts',(-1.34270948206319,1.,1.6934684849687));
#31576=CARTESIAN_POINT('Ctrl Pts',(-1.34367237124483,-1.,1.69979707754427));
#31577=CARTESIAN_POINT('Ctrl Pts',(-1.34367237124483,1.,1.69979707754427));
#31578=CARTESIAN_POINT('Ctrl Pts',(-1.34459924533831,-1.,1.70614212266738));
#31579=CARTESIAN_POINT('Ctrl Pts',(-1.34459924533831,1.,1.70614212266738));
#31580=CARTESIAN_POINT('Ctrl Pts',(-1.34549029589416,-1.,1.71250340686822));
#31581=CARTESIAN_POINT('Ctrl Pts',(-1.34549029589416,1.,1.71250340686822));
#31582=CARTESIAN_POINT('Ctrl Pts',(-1.34634568653227,-1.,1.7188807715049));
#31583=CARTESIAN_POINT('Ctrl Pts',(-1.34634568653227,1.,1.7188807715049));
#31584=CARTESIAN_POINT('Ctrl Pts',(-1.34716554819527,-1.,1.72527410680674));
#31585=CARTESIAN_POINT('Ctrl Pts',(-1.34716554819527,1.,1.72527410680674));
#31586=CARTESIAN_POINT('Ctrl Pts',(-1.34779309152035,-1.,1.7304014965394));
#31587=CARTESIAN_POINT('Ctrl Pts',(-1.34779309152035,1.,1.7304014965394));
#31588=CARTESIAN_POINT('Ctrl Pts',(-1.34824783112887,-1.,1.73425417885907));
#31589=CARTESIAN_POINT('Ctrl Pts',(-1.34824783112887,1.,1.73425417885907));
#31590=CARTESIAN_POINT('Ctrl Pts',(-1.34854391898045,-1.,1.73682580585691));
#31591=CARTESIAN_POINT('Ctrl Pts',(-1.34854391898045,1.,1.73682580585691));
#31592=CARTESIAN_POINT('Ctrl Pts',(-1.34869019493419,-1.,1.73811241238545));
#31593=CARTESIAN_POINT('Ctrl Pts',(-1.34869019493419,1.,1.73811241238545));
#31594=CARTESIAN_POINT('',(-1.15624053661742,1.,1.31362392696032));
#31595=CARTESIAN_POINT('Ctrl Pts',(-1.15624053661742,1.,1.31362392696032));
#31596=CARTESIAN_POINT('Ctrl Pts',(-1.15950888730809,1.,1.31722977216397));
#31597=CARTESIAN_POINT('Ctrl Pts',(-1.16589330093588,1.,1.32428080721772));
#31598=CARTESIAN_POINT('Ctrl Pts',(-1.17501305789857,1.,1.33437539347008));
#31599=CARTESIAN_POINT('Ctrl Pts',(-1.18625865667441,1.,1.34687054001093));
#31600=CARTESIAN_POINT('Ctrl Pts',(-1.1987959077932,1.,1.36088705043885));
#31601=CARTESIAN_POINT('Ctrl Pts',(-1.20982812925645,1.,1.37331915607905));
#31602=CARTESIAN_POINT('Ctrl Pts',(-1.21938737280852,1.,1.38420564527715));
#31603=CARTESIAN_POINT('Ctrl Pts',(-1.22752961899387,1.,1.39361389568796));
#31604=CARTESIAN_POINT('Ctrl Pts',(-1.23434087290423,1.,1.40164708206106));
#31605=CARTESIAN_POINT('Ctrl Pts',(-1.23994455029534,1.,1.40845295531283));
#31606=CARTESIAN_POINT('Ctrl Pts',(-1.24450600513056,1.,1.41422913175179));
#31607=CARTESIAN_POINT('Ctrl Pts',(-1.24824430986571,1.,1.41923722596025));
#31608=CARTESIAN_POINT('Ctrl Pts',(-1.2514145557001,1.,1.42378102115575));
#31609=CARTESIAN_POINT('Ctrl Pts',(-1.25426945222639,1.,1.42815938799387));
#31610=CARTESIAN_POINT('Ctrl Pts',(-1.25702687965755,1.,1.43262645609691));
#31611=CARTESIAN_POINT('Ctrl Pts',(-1.25983531012005,1.,1.43734919180848));
#31612=CARTESIAN_POINT('Ctrl Pts',(-1.26273903323859,1.,1.44236470511303));
#31613=CARTESIAN_POINT('Ctrl Pts',(-1.26570925118868,1.,1.44761985001662));
#31614=CARTESIAN_POINT('Ctrl Pts',(-1.2686778680489,1.,1.45301422764247));
#31615=CARTESIAN_POINT('Ctrl Pts',(-1.27156805265289,1.,1.45843906294697));
#31616=CARTESIAN_POINT('Ctrl Pts',(-1.27433119897822,1.,1.46382431332476));
#31617=CARTESIAN_POINT('Ctrl Pts',(-1.27696414831089,1.,1.46916035917133));
#31618=CARTESIAN_POINT('Ctrl Pts',(-1.2794891824849,1.,1.4744717526707));
#31619=CARTESIAN_POINT('Ctrl Pts',(-1.28194158939517,1.,1.47980070347095));
#31620=CARTESIAN_POINT('Ctrl Pts',(-1.28435533880201,1.,1.4851881711891));
#31621=CARTESIAN_POINT('Ctrl Pts',(-1.2867467611644,1.,1.4906522831278));
#31622=CARTESIAN_POINT('Ctrl Pts',(-1.28911506584254,1.,1.49618896881754));
#31623=CARTESIAN_POINT('Ctrl Pts',(-1.29145022885181,1.,1.50178230149776));
#31624=CARTESIAN_POINT('Ctrl Pts',(-1.29373841372842,1.,1.50741159078365));
#31625=CARTESIAN_POINT('Ctrl Pts',(-1.29596850710509,1.,1.51305994241402));
#31626=CARTESIAN_POINT('Ctrl Pts',(-1.29813791800747,1.,1.51872184912724));
#31627=CARTESIAN_POINT('Ctrl Pts',(-1.30024984366328,1.,1.52439957861062));
#31628=CARTESIAN_POINT('Ctrl Pts',(-1.30231064395568,1.,1.53009970283891));
#31629=CARTESIAN_POINT('Ctrl Pts',(-1.30432735639489,1.,1.53582981268977));
#31630=CARTESIAN_POINT('Ctrl Pts',(-1.30630475189556,1.,1.54159462645432));
#31631=CARTESIAN_POINT('Ctrl Pts',(-1.30824393907473,1.,1.54739413957185));
#31632=CARTESIAN_POINT('Ctrl Pts',(-1.31014393684222,1.,1.55322568759481));
#31633=CARTESIAN_POINT('Ctrl Pts',(-1.31200264341696,1.,1.55908521254821));
#31634=CARTESIAN_POINT('Ctrl Pts',(-1.31381795281002,1.,1.56496872402353));
#31635=CARTESIAN_POINT('Ctrl Pts',(-1.31558903860016,1.,1.57087397835723));
#31636=CARTESIAN_POINT('Ctrl Pts',(-1.31731642317187,1.,1.5768005650559));
#31637=CARTESIAN_POINT('Ctrl Pts',(-1.31900135021432,1.,1.58274907898834));
#31638=CARTESIAN_POINT('Ctrl Pts',(-1.32064537110892,1.,1.58872057258245));
#31639=CARTESIAN_POINT('Ctrl Pts',(-1.32224985747682,1.,1.59471591079403));
#31640=CARTESIAN_POINT('Ctrl Pts',(-1.32381550858256,1.,1.60073511858687));
#31641=CARTESIAN_POINT('Ctrl Pts',(-1.32534250785782,1.,1.60677758290954));
#31642=CARTESIAN_POINT('Ctrl Pts',(-1.32683074483356,1.,1.6128423401575));
#31643=CARTESIAN_POINT('Ctrl Pts',(-1.32828000610449,1.,1.61892832270724));
#31644=CARTESIAN_POINT('Ctrl Pts',(-1.3296901950568,1.,1.62503464209797));
#31645=CARTESIAN_POINT('Ctrl Pts',(-1.33106149345645,1.,1.63116079730923));
#31646=CARTESIAN_POINT('Ctrl Pts',(-1.33239425103724,1.,1.63730653475089));
#31647=CARTESIAN_POINT('Ctrl Pts',(-1.33368890676572,1.,1.6434717485603));
#31648=CARTESIAN_POINT('Ctrl Pts',(-1.33494590467993,1.,1.6496563728683));
#31649=CARTESIAN_POINT('Ctrl Pts',(-1.33616559745172,1.,1.65586025952593));
#31650=CARTESIAN_POINT('Ctrl Pts',(-1.33734820885262,1.,1.66208312541983));
#31651=CARTESIAN_POINT('Ctrl Pts',(-1.33849388654388,1.,1.66832460783989));
#31652=CARTESIAN_POINT('Ctrl Pts',(-1.3396027347034,1.,1.67458429426086));
#31653=CARTESIAN_POINT('Ctrl Pts',(-1.34067485185203,1.,1.68086176030362));
#31654=CARTESIAN_POINT('Ctrl Pts',(-1.341710374848,1.,1.68715660868764));
#31655=CARTESIAN_POINT('Ctrl Pts',(-1.34270948206319,1.,1.6934684849687));
#31656=CARTESIAN_POINT('Ctrl Pts',(-1.34367237124483,1.,1.69979707754427));
#31657=CARTESIAN_POINT('Ctrl Pts',(-1.34459924533831,1.,1.70614212266738));
#31658=CARTESIAN_POINT('Ctrl Pts',(-1.34549029589416,1.,1.71250340686822));
#31659=CARTESIAN_POINT('Ctrl Pts',(-1.34634568653227,1.,1.7188807715049));
#31660=CARTESIAN_POINT('Ctrl Pts',(-1.34716554819527,1.,1.72527410680674));
#31661=CARTESIAN_POINT('Ctrl Pts',(-1.34779309152035,1.,1.7304014965394));
#31662=CARTESIAN_POINT('Ctrl Pts',(-1.34824783112887,1.,1.73425417885907));
#31663=CARTESIAN_POINT('Ctrl Pts',(-1.34854391898045,1.,1.73682580585691));
#31664=CARTESIAN_POINT('Ctrl Pts',(-1.34869019493419,1.,1.73811241238545));
#31665=CARTESIAN_POINT('',(-1.15624053661742,0.,1.31362392696032));
#31666=CARTESIAN_POINT('Origin',(0.,0.,0.));
#31667=CARTESIAN_POINT('',(-1.31362392696033,1.,1.15624053661742));
#31668=CARTESIAN_POINT('Origin',(0.,1.,0.));
#31669=CARTESIAN_POINT('',(-1.31362392696033,0.,1.15624053661742));
#31670=CARTESIAN_POINT('Ctrl Pts',(-1.73811241238545,-1.,1.34869019493419));
#31671=CARTESIAN_POINT('Ctrl Pts',(-1.73811241238545,1.,1.34869019493419));
#31672=CARTESIAN_POINT('Ctrl Pts',(-1.73682580585819,-1.,1.34854391898145));
#31673=CARTESIAN_POINT('Ctrl Pts',(-1.73682580585819,1.,1.34854391898145));
#31674=CARTESIAN_POINT('Ctrl Pts',(-1.73425417886255,-1.,1.34824783113158));
#31675=CARTESIAN_POINT('Ctrl Pts',(-1.73425417886255,1.,1.34824783113158));
#31676=CARTESIAN_POINT('Ctrl Pts',(-1.73040149654497,-1.,1.3477930915247));
#31677=CARTESIAN_POINT('Ctrl Pts',(-1.73040149654497,1.,1.3477930915247));
#31678=CARTESIAN_POINT('Ctrl Pts',(-1.72527410681298,-1.,1.34716554820013));
#31679=CARTESIAN_POINT('Ctrl Pts',(-1.72527410681298,1.,1.34716554820013));
#31680=CARTESIAN_POINT('Ctrl Pts',(-1.7188807715095,-1.,1.34634568653586));
#31681=CARTESIAN_POINT('Ctrl Pts',(-1.7188807715095,1.,1.34634568653586));
#31682=CARTESIAN_POINT('Ctrl Pts',(-1.71250340687011,-1.,1.34549029589563));
#31683=CARTESIAN_POINT('Ctrl Pts',(-1.71250340687011,1.,1.34549029589563));
#31684=CARTESIAN_POINT('Ctrl Pts',(-1.70614212266676,-1.,1.34459924533783));
#31685=CARTESIAN_POINT('Ctrl Pts',(-1.70614212266676,1.,1.34459924533783));
#31686=CARTESIAN_POINT('Ctrl Pts',(-1.69979707754221,-1.,1.34367237124322));
#31687=CARTESIAN_POINT('Ctrl Pts',(-1.69979707754221,1.,1.34367237124322));
#31688=CARTESIAN_POINT('Ctrl Pts',(-1.6934684849664,-1.,1.34270948206139));
#31689=CARTESIAN_POINT('Ctrl Pts',(-1.6934684849664,1.,1.34270948206139));
#31690=CARTESIAN_POINT('Ctrl Pts',(-1.68715660868602,-1.,1.34171037484673));
#31691=CARTESIAN_POINT('Ctrl Pts',(-1.68715660868602,1.,1.34171037484673));
#31692=CARTESIAN_POINT('Ctrl Pts',(-1.68086176030308,-1.,1.3406748518516));
#31693=CARTESIAN_POINT('Ctrl Pts',(-1.68086176030308,1.,1.3406748518516));
#31694=CARTESIAN_POINT('Ctrl Pts',(-1.67458429426126,-1.,1.33960273470372));
#31695=CARTESIAN_POINT('Ctrl Pts',(-1.67458429426126,1.,1.33960273470372));
#31696=CARTESIAN_POINT('Ctrl Pts',(-1.66832460784078,-1.,1.33849388654458));
#31697=CARTESIAN_POINT('Ctrl Pts',(-1.66832460784078,1.,1.33849388654458));
#31698=CARTESIAN_POINT('Ctrl Pts',(-1.66208312542073,-1.,1.33734820885331));
#31699=CARTESIAN_POINT('Ctrl Pts',(-1.66208312542073,1.,1.33734820885331));
#31700=CARTESIAN_POINT('Ctrl Pts',(-1.65586025952651,-1.,1.33616559745217));
#31701=CARTESIAN_POINT('Ctrl Pts',(-1.65586025952651,1.,1.33616559745217));
#31702=CARTESIAN_POINT('Ctrl Pts',(-1.64965637286843,-1.,1.33494590468003));
#31703=CARTESIAN_POINT('Ctrl Pts',(-1.64965637286843,1.,1.33494590468003));
#31704=CARTESIAN_POINT('Ctrl Pts',(-1.64347174856007,-1.,1.33368890676554));
#31705=CARTESIAN_POINT('Ctrl Pts',(-1.64347174856007,1.,1.33368890676554));
#31706=CARTESIAN_POINT('Ctrl Pts',(-1.6373065347505,-1.,1.33239425103694));
#31707=CARTESIAN_POINT('Ctrl Pts',(-1.6373065347505,1.,1.33239425103694));
#31708=CARTESIAN_POINT('Ctrl Pts',(-1.63116079730887,-1.,1.33106149345618));
#31709=CARTESIAN_POINT('Ctrl Pts',(-1.63116079730887,1.,1.33106149345618));
#31710=CARTESIAN_POINT('Ctrl Pts',(-1.62503464209777,-1.,1.32969019505665));
#31711=CARTESIAN_POINT('Ctrl Pts',(-1.62503464209777,1.,1.32969019505665));
#31712=CARTESIAN_POINT('Ctrl Pts',(-1.61892832270723,-1.,1.32828000610448));
#31713=CARTESIAN_POINT('Ctrl Pts',(-1.61892832270723,1.,1.32828000610448));
#31714=CARTESIAN_POINT('Ctrl Pts',(-1.61284234015762,-1.,1.32683074483365));
#31715=CARTESIAN_POINT('Ctrl Pts',(-1.61284234015762,1.,1.32683074483365));
#31716=CARTESIAN_POINT('Ctrl Pts',(-1.6067775829097,-1.,1.32534250785794));
#31717=CARTESIAN_POINT('Ctrl Pts',(-1.6067775829097,1.,1.32534250785794));
#31718=CARTESIAN_POINT('Ctrl Pts',(-1.600735118587,-1.,1.32381550858266));
#31719=CARTESIAN_POINT('Ctrl Pts',(-1.600735118587,1.,1.32381550858266));
#31720=CARTESIAN_POINT('Ctrl Pts',(-1.59471591079408,-1.,1.32224985747686));
#31721=CARTESIAN_POINT('Ctrl Pts',(-1.59471591079408,1.,1.32224985747686));
#31722=CARTESIAN_POINT('Ctrl Pts',(-1.58872057258244,-1.,1.32064537110891));
#31723=CARTESIAN_POINT('Ctrl Pts',(-1.58872057258244,1.,1.32064537110891));
#31724=CARTESIAN_POINT('Ctrl Pts',(-1.58274907898829,-1.,1.31900135021428));
#31725=CARTESIAN_POINT('Ctrl Pts',(-1.58274907898829,1.,1.31900135021428));
#31726=CARTESIAN_POINT('Ctrl Pts',(-1.57680056505585,-1.,1.31731642317183));
#31727=CARTESIAN_POINT('Ctrl Pts',(-1.57680056505585,1.,1.31731642317183));
#31728=CARTESIAN_POINT('Ctrl Pts',(-1.57087397835721,-1.,1.31558903860015));
#31729=CARTESIAN_POINT('Ctrl Pts',(-1.57087397835721,1.,1.31558903860015));
#31730=CARTESIAN_POINT('Ctrl Pts',(-1.56496872402352,-1.,1.31381795281002));
#31731=CARTESIAN_POINT('Ctrl Pts',(-1.56496872402352,1.,1.31381795281002));
#31732=CARTESIAN_POINT('Ctrl Pts',(-1.55908521254822,-1.,1.31200264341696));
#31733=CARTESIAN_POINT('Ctrl Pts',(-1.55908521254822,1.,1.31200264341696));
#31734=CARTESIAN_POINT('Ctrl Pts',(-1.55322568759481,-1.,1.31014393684221));
#31735=CARTESIAN_POINT('Ctrl Pts',(-1.55322568759481,1.,1.31014393684221));
#31736=CARTESIAN_POINT('Ctrl Pts',(-1.54739413957183,-1.,1.30824393907471));
#31737=CARTESIAN_POINT('Ctrl Pts',(-1.54739413957183,1.,1.30824393907471));
#31738=CARTESIAN_POINT('Ctrl Pts',(-1.54159462645428,-1.,1.30630475189553));
#31739=CARTESIAN_POINT('Ctrl Pts',(-1.54159462645428,1.,1.30630475189553));
#31740=CARTESIAN_POINT('Ctrl Pts',(-1.53582981268976,-1.,1.30432735639487));
#31741=CARTESIAN_POINT('Ctrl Pts',(-1.53582981268976,1.,1.30432735639487));
#31742=CARTESIAN_POINT('Ctrl Pts',(-1.53009970283893,-1.,1.3023106439557));
#31743=CARTESIAN_POINT('Ctrl Pts',(-1.53009970283893,1.,1.3023106439557));
#31744=CARTESIAN_POINT('Ctrl Pts',(-1.5243995786107,-1.,1.30024984366334));
#31745=CARTESIAN_POINT('Ctrl Pts',(-1.5243995786107,1.,1.30024984366334));
#31746=CARTESIAN_POINT('Ctrl Pts',(-1.51872184912735,-1.,1.29813791800757));
#31747=CARTESIAN_POINT('Ctrl Pts',(-1.51872184912735,1.,1.29813791800757));
#31748=CARTESIAN_POINT('Ctrl Pts',(-1.51305994241412,-1.,1.29596850710518));
#31749=CARTESIAN_POINT('Ctrl Pts',(-1.51305994241412,1.,1.29596850710518));
#31750=CARTESIAN_POINT('Ctrl Pts',(-1.50741159078367,-1.,1.29373841372843));
#31751=CARTESIAN_POINT('Ctrl Pts',(-1.50741159078367,1.,1.29373841372843));
#31752=CARTESIAN_POINT('Ctrl Pts',(-1.50178230149764,-1.,1.29145022885171));
#31753=CARTESIAN_POINT('Ctrl Pts',(-1.50178230149764,1.,1.29145022885171));
#31754=CARTESIAN_POINT('Ctrl Pts',(-1.49618896881729,-1.,1.28911506584232));
#31755=CARTESIAN_POINT('Ctrl Pts',(-1.49618896881729,1.,1.28911506584232));
#31756=CARTESIAN_POINT('Ctrl Pts',(-1.4906522831275,-1.,1.28674676116415));
#31757=CARTESIAN_POINT('Ctrl Pts',(-1.4906522831275,1.,1.28674676116415));
#31758=CARTESIAN_POINT('Ctrl Pts',(-1.48518817118891,-1.,1.28435533880184));
#31759=CARTESIAN_POINT('Ctrl Pts',(-1.48518817118891,1.,1.28435533880184));
#31760=CARTESIAN_POINT('Ctrl Pts',(-1.47980070347102,-1.,1.28194158939522));
#31761=CARTESIAN_POINT('Ctrl Pts',(-1.47980070347102,1.,1.28194158939522));
#31762=CARTESIAN_POINT('Ctrl Pts',(-1.4744717526711,-1.,1.27948918248524));
#31763=CARTESIAN_POINT('Ctrl Pts',(-1.4744717526711,1.,1.27948918248524));
#31764=CARTESIAN_POINT('Ctrl Pts',(-1.46916035917197,-1.,1.27696414831144));
#31765=CARTESIAN_POINT('Ctrl Pts',(-1.46916035917197,1.,1.27696414831144));
#31766=CARTESIAN_POINT('Ctrl Pts',(-1.4638243133254,-1.,1.27433119897877));
#31767=CARTESIAN_POINT('Ctrl Pts',(-1.4638243133254,1.,1.27433119897877));
#31768=CARTESIAN_POINT('Ctrl Pts',(-1.45843906294725,-1.,1.27156805265312));
#31769=CARTESIAN_POINT('Ctrl Pts',(-1.45843906294725,1.,1.27156805265312));
#31770=CARTESIAN_POINT('Ctrl Pts',(-1.45301422764205,-1.,1.26867786804854));
#31771=CARTESIAN_POINT('Ctrl Pts',(-1.45301422764205,1.,1.26867786804854));
#31772=CARTESIAN_POINT('Ctrl Pts',(-1.44761985001544,-1.,1.26570925118767));
#31773=CARTESIAN_POINT('Ctrl Pts',(-1.44761985001544,1.,1.26570925118767));
#31774=CARTESIAN_POINT('Ctrl Pts',(-1.44236470511145,-1.,1.26273903323723));
#31775=CARTESIAN_POINT('Ctrl Pts',(-1.44236470511145,1.,1.26273903323723));
#31776=CARTESIAN_POINT('Ctrl Pts',(-1.43734919180719,-1.,1.25983531011894));
#31777=CARTESIAN_POINT('Ctrl Pts',(-1.43734919180719,1.,1.25983531011894));
#31778=CARTESIAN_POINT('Ctrl Pts',(-1.43262645609679,-1.,1.25702687965744));
#31779=CARTESIAN_POINT('Ctrl Pts',(-1.43262645609679,1.,1.25702687965744));
#31780=CARTESIAN_POINT('Ctrl Pts',(-1.42815938799555,-1.,1.25426945222783));
#31781=CARTESIAN_POINT('Ctrl Pts',(-1.42815938799555,1.,1.25426945222783));
#31782=CARTESIAN_POINT('Ctrl Pts',(-1.42378102115911,-1.,1.25141455570299));
#31783=CARTESIAN_POINT('Ctrl Pts',(-1.42378102115911,1.,1.25141455570299));
#31784=CARTESIAN_POINT('Ctrl Pts',(-1.41923722596421,-1.,1.24824430986911));
#31785=CARTESIAN_POINT('Ctrl Pts',(-1.41923722596421,1.,1.24824430986911));
#31786=CARTESIAN_POINT('Ctrl Pts',(-1.41422913175437,-1.,1.24450600513278));
#31787=CARTESIAN_POINT('Ctrl Pts',(-1.41422913175437,1.,1.24450600513278));
#31788=CARTESIAN_POINT('Ctrl Pts',(-1.40845295531151,-1.,1.23994455029421));
#31789=CARTESIAN_POINT('Ctrl Pts',(-1.40845295531151,1.,1.23994455029421));
#31790=CARTESIAN_POINT('Ctrl Pts',(-1.40164708205345,-1.,1.23434087289768));
#31791=CARTESIAN_POINT('Ctrl Pts',(-1.40164708205345,1.,1.23434087289768));
#31792=CARTESIAN_POINT('Ctrl Pts',(-1.39361389567257,-1.,1.22752961898063));
#31793=CARTESIAN_POINT('Ctrl Pts',(-1.39361389567257,1.,1.22752961898063));
#31794=CARTESIAN_POINT('Ctrl Pts',(-1.38420564525391,-1.,1.21938737278853));
#31795=CARTESIAN_POINT('Ctrl Pts',(-1.38420564525391,1.,1.21938737278853));
#31796=CARTESIAN_POINT('Ctrl Pts',(-1.37331915604962,-1.,1.20982812923113));
#31797=CARTESIAN_POINT('Ctrl Pts',(-1.37331915604962,1.,1.20982812923113));
#31798=CARTESIAN_POINT('Ctrl Pts',(-1.36088705040677,-1.,1.1987959077656));
#31799=CARTESIAN_POINT('Ctrl Pts',(-1.36088705040677,1.,1.1987959077656));
#31800=CARTESIAN_POINT('Ctrl Pts',(-1.34687053998157,-1.,1.18625865664915));
#31801=CARTESIAN_POINT('Ctrl Pts',(-1.34687053998157,1.,1.18625865664915));
#31802=CARTESIAN_POINT('Ctrl Pts',(-1.33437539344842,-1.,1.17501305787994));
#31803=CARTESIAN_POINT('Ctrl Pts',(-1.33437539344842,1.,1.17501305787994));
#31804=CARTESIAN_POINT('Ctrl Pts',(-1.32428080720544,-1.,1.16589330092532));
#31805=CARTESIAN_POINT('Ctrl Pts',(-1.32428080720544,1.,1.16589330092532));
#31806=CARTESIAN_POINT('Ctrl Pts',(-1.3172297721596,-1.,1.15950888730433));
#31807=CARTESIAN_POINT('Ctrl Pts',(-1.3172297721596,1.,1.15950888730433));
#31808=CARTESIAN_POINT('Ctrl Pts',(-1.31362392696033,-1.,1.15624053661742));
#31809=CARTESIAN_POINT('Ctrl Pts',(-1.31362392696033,1.,1.15624053661742));
#31810=CARTESIAN_POINT('',(-1.73811241238545,1.,1.34869019493419));
#31811=CARTESIAN_POINT('Ctrl Pts',(-1.73811241238545,1.,1.34869019493419));
#31812=CARTESIAN_POINT('Ctrl Pts',(-1.73682580585819,1.,1.34854391898145));
#31813=CARTESIAN_POINT('Ctrl Pts',(-1.73425417886255,1.,1.34824783113158));
#31814=CARTESIAN_POINT('Ctrl Pts',(-1.73040149654497,1.,1.3477930915247));
#31815=CARTESIAN_POINT('Ctrl Pts',(-1.72527410681298,1.,1.34716554820013));
#31816=CARTESIAN_POINT('Ctrl Pts',(-1.7188807715095,1.,1.34634568653586));
#31817=CARTESIAN_POINT('Ctrl Pts',(-1.71250340687011,1.,1.34549029589563));
#31818=CARTESIAN_POINT('Ctrl Pts',(-1.70614212266676,1.,1.34459924533783));
#31819=CARTESIAN_POINT('Ctrl Pts',(-1.69979707754221,1.,1.34367237124322));
#31820=CARTESIAN_POINT('Ctrl Pts',(-1.6934684849664,1.,1.34270948206139));
#31821=CARTESIAN_POINT('Ctrl Pts',(-1.68715660868602,1.,1.34171037484673));
#31822=CARTESIAN_POINT('Ctrl Pts',(-1.68086176030308,1.,1.3406748518516));
#31823=CARTESIAN_POINT('Ctrl Pts',(-1.67458429426126,1.,1.33960273470372));
#31824=CARTESIAN_POINT('Ctrl Pts',(-1.66832460784078,1.,1.33849388654458));
#31825=CARTESIAN_POINT('Ctrl Pts',(-1.66208312542073,1.,1.33734820885331));
#31826=CARTESIAN_POINT('Ctrl Pts',(-1.65586025952651,1.,1.33616559745217));
#31827=CARTESIAN_POINT('Ctrl Pts',(-1.64965637286843,1.,1.33494590468003));
#31828=CARTESIAN_POINT('Ctrl Pts',(-1.64347174856007,1.,1.33368890676554));
#31829=CARTESIAN_POINT('Ctrl Pts',(-1.6373065347505,1.,1.33239425103694));
#31830=CARTESIAN_POINT('Ctrl Pts',(-1.63116079730887,1.,1.33106149345618));
#31831=CARTESIAN_POINT('Ctrl Pts',(-1.62503464209777,1.,1.32969019505665));
#31832=CARTESIAN_POINT('Ctrl Pts',(-1.61892832270723,1.,1.32828000610448));
#31833=CARTESIAN_POINT('Ctrl Pts',(-1.61284234015762,1.,1.32683074483365));
#31834=CARTESIAN_POINT('Ctrl Pts',(-1.6067775829097,1.,1.32534250785794));
#31835=CARTESIAN_POINT('Ctrl Pts',(-1.600735118587,1.,1.32381550858266));
#31836=CARTESIAN_POINT('Ctrl Pts',(-1.59471591079408,1.,1.32224985747686));
#31837=CARTESIAN_POINT('Ctrl Pts',(-1.58872057258244,1.,1.32064537110891));
#31838=CARTESIAN_POINT('Ctrl Pts',(-1.58274907898829,1.,1.31900135021428));
#31839=CARTESIAN_POINT('Ctrl Pts',(-1.57680056505585,1.,1.31731642317183));
#31840=CARTESIAN_POINT('Ctrl Pts',(-1.57087397835721,1.,1.31558903860015));
#31841=CARTESIAN_POINT('Ctrl Pts',(-1.56496872402352,1.,1.31381795281002));
#31842=CARTESIAN_POINT('Ctrl Pts',(-1.55908521254822,1.,1.31200264341696));
#31843=CARTESIAN_POINT('Ctrl Pts',(-1.55322568759481,1.,1.31014393684221));
#31844=CARTESIAN_POINT('Ctrl Pts',(-1.54739413957183,1.,1.30824393907471));
#31845=CARTESIAN_POINT('Ctrl Pts',(-1.54159462645428,1.,1.30630475189553));
#31846=CARTESIAN_POINT('Ctrl Pts',(-1.53582981268976,1.,1.30432735639487));
#31847=CARTESIAN_POINT('Ctrl Pts',(-1.53009970283893,1.,1.3023106439557));
#31848=CARTESIAN_POINT('Ctrl Pts',(-1.5243995786107,1.,1.30024984366334));
#31849=CARTESIAN_POINT('Ctrl Pts',(-1.51872184912735,1.,1.29813791800757));
#31850=CARTESIAN_POINT('Ctrl Pts',(-1.51305994241412,1.,1.29596850710518));
#31851=CARTESIAN_POINT('Ctrl Pts',(-1.50741159078367,1.,1.29373841372843));
#31852=CARTESIAN_POINT('Ctrl Pts',(-1.50178230149764,1.,1.29145022885171));
#31853=CARTESIAN_POINT('Ctrl Pts',(-1.49618896881729,1.,1.28911506584232));
#31854=CARTESIAN_POINT('Ctrl Pts',(-1.4906522831275,1.,1.28674676116415));
#31855=CARTESIAN_POINT('Ctrl Pts',(-1.48518817118891,1.,1.28435533880184));
#31856=CARTESIAN_POINT('Ctrl Pts',(-1.47980070347102,1.,1.28194158939522));
#31857=CARTESIAN_POINT('Ctrl Pts',(-1.4744717526711,1.,1.27948918248524));
#31858=CARTESIAN_POINT('Ctrl Pts',(-1.46916035917197,1.,1.27696414831144));
#31859=CARTESIAN_POINT('Ctrl Pts',(-1.4638243133254,1.,1.27433119897877));
#31860=CARTESIAN_POINT('Ctrl Pts',(-1.45843906294725,1.,1.27156805265312));
#31861=CARTESIAN_POINT('Ctrl Pts',(-1.45301422764205,1.,1.26867786804854));
#31862=CARTESIAN_POINT('Ctrl Pts',(-1.44761985001544,1.,1.26570925118767));
#31863=CARTESIAN_POINT('Ctrl Pts',(-1.44236470511145,1.,1.26273903323723));
#31864=CARTESIAN_POINT('Ctrl Pts',(-1.43734919180719,1.,1.25983531011894));
#31865=CARTESIAN_POINT('Ctrl Pts',(-1.43262645609679,1.,1.25702687965744));
#31866=CARTESIAN_POINT('Ctrl Pts',(-1.42815938799555,1.,1.25426945222783));
#31867=CARTESIAN_POINT('Ctrl Pts',(-1.42378102115911,1.,1.25141455570299));
#31868=CARTESIAN_POINT('Ctrl Pts',(-1.41923722596421,1.,1.24824430986911));
#31869=CARTESIAN_POINT('Ctrl Pts',(-1.41422913175437,1.,1.24450600513278));
#31870=CARTESIAN_POINT('Ctrl Pts',(-1.40845295531151,1.,1.23994455029421));
#31871=CARTESIAN_POINT('Ctrl Pts',(-1.40164708205345,1.,1.23434087289768));
#31872=CARTESIAN_POINT('Ctrl Pts',(-1.39361389567257,1.,1.22752961898063));
#31873=CARTESIAN_POINT('Ctrl Pts',(-1.38420564525391,1.,1.21938737278853));
#31874=CARTESIAN_POINT('Ctrl Pts',(-1.37331915604962,1.,1.20982812923113));
#31875=CARTESIAN_POINT('Ctrl Pts',(-1.36088705040677,1.,1.1987959077656));
#31876=CARTESIAN_POINT('Ctrl Pts',(-1.34687053998157,1.,1.18625865664915));
#31877=CARTESIAN_POINT('Ctrl Pts',(-1.33437539344842,1.,1.17501305787994));
#31878=CARTESIAN_POINT('Ctrl Pts',(-1.32428080720544,1.,1.16589330092532));
#31879=CARTESIAN_POINT('Ctrl Pts',(-1.3172297721596,1.,1.15950888730433));
#31880=CARTESIAN_POINT('Ctrl Pts',(-1.31362392696033,1.,1.15624053661742));
#31881=CARTESIAN_POINT('',(-1.73811241238545,0.,1.34869019493419));
#31882=CARTESIAN_POINT('Origin',(-1.81978687191668,0.,1.23627494547115));
#31883=CARTESIAN_POINT('',(-1.81978687191668,1.,1.23627494547115));
#31884=CARTESIAN_POINT('',(-1.73811241238545,1.,1.34869019493419));
#31885=CARTESIAN_POINT('',(-1.81978687191668,0.,1.23627494547115));
#31886=CARTESIAN_POINT('Ctrl Pts',(-1.5055822144029,-1.,0.892032620296855));
#31887=CARTESIAN_POINT('Ctrl Pts',(-1.5055822144029,1.,0.892032620296855));
#31888=CARTESIAN_POINT('Ctrl Pts',(-1.50980486807181,-1.,0.894452006967538));
#31889=CARTESIAN_POINT('Ctrl Pts',(-1.50980486807181,1.,0.894452006967538));
#31890=CARTESIAN_POINT('Ctrl Pts',(-1.51805569591479,-1.,0.89918504749193));
#31891=CARTESIAN_POINT('Ctrl Pts',(-1.51805569591479,1.,0.89918504749193));
#31892=CARTESIAN_POINT('Ctrl Pts',(-1.52984849890434,-1.,0.905967409640499));
#31893=CARTESIAN_POINT('Ctrl Pts',(-1.52984849890434,1.,0.905967409640499));
#31894=CARTESIAN_POINT('Ctrl Pts',(-1.54440491152808,-1.,0.91437591904658));
#31895=CARTESIAN_POINT('Ctrl Pts',(-1.54440491152808,1.,0.91437591904658));
#31896=CARTESIAN_POINT('Ctrl Pts',(-1.56065988582509,-1.,0.923832188966322));
#31897=CARTESIAN_POINT('Ctrl Pts',(-1.56065988582509,1.,0.923832188966322));
#31898=CARTESIAN_POINT('Ctrl Pts',(-1.57499388385561,-1.,0.932246680128849));
#31899=CARTESIAN_POINT('Ctrl Pts',(-1.57499388385561,1.,0.932246680128849));
#31900=CARTESIAN_POINT('Ctrl Pts',(-1.58744937489796,-1.,0.939646377909319));
#31901=CARTESIAN_POINT('Ctrl Pts',(-1.58744937489796,1.,0.939646377909319));
#31902=CARTESIAN_POINT('Ctrl Pts',(-1.59810042045408,-1.,0.946078063325796));
#31903=CARTESIAN_POINT('Ctrl Pts',(-1.59810042045408,1.,0.946078063325796));
#31904=CARTESIAN_POINT('Ctrl Pts',(-1.60706069897794,-1.,0.951613284361248));
#31905=CARTESIAN_POINT('Ctrl Pts',(-1.60706069897794,1.,0.951613284361248));
#31906=CARTESIAN_POINT('Ctrl Pts',(-1.61449324337233,-1.,0.956354422921573));
#31907=CARTESIAN_POINT('Ctrl Pts',(-1.61449324337233,1.,0.956354422921573));
#31908=CARTESIAN_POINT('Ctrl Pts',(-1.62061638139929,-1.,0.960438326099958));
#31909=CARTESIAN_POINT('Ctrl Pts',(-1.62061638139929,1.,0.960438326099958));
#31910=CARTESIAN_POINT('Ctrl Pts',(-1.6257193066974,-1.,0.964046107037821));
#31911=CARTESIAN_POINT('Ctrl Pts',(-1.6257193066974,1.,0.964046107037821));
#31912=CARTESIAN_POINT('Ctrl Pts',(-1.63013849959083,-1.,0.967387853228041));
#31913=CARTESIAN_POINT('Ctrl Pts',(-1.63013849959083,1.,0.967387853228041));
#31914=CARTESIAN_POINT('Ctrl Pts',(-1.63420665729609,-1.,0.970669715996356));
#31915=CARTESIAN_POINT('Ctrl Pts',(-1.63420665729609,1.,0.970669715996356));
#31916=CARTESIAN_POINT('Ctrl Pts',(-1.63820952658157,-1.,0.974066058287501));
#31917=CARTESIAN_POINT('Ctrl Pts',(-1.63820952658157,1.,0.974066058287501));
#31918=CARTESIAN_POINT('Ctrl Pts',(-1.64233990826831,-1.,0.977689794120297));
#31919=CARTESIAN_POINT('Ctrl Pts',(-1.64233990826831,1.,0.977689794120297));
#31920=CARTESIAN_POINT('Ctrl Pts',(-1.64665139190834,-1.,0.981562530940574));
#31921=CARTESIAN_POINT('Ctrl Pts',(-1.64665139190834,1.,0.981562530940574));
#31922=CARTESIAN_POINT('Ctrl Pts',(-1.6511001661277,-1.,0.985642622921626));
#31923=CARTESIAN_POINT('Ctrl Pts',(-1.6511001661277,1.,0.985642622921626));
#31924=CARTESIAN_POINT('Ctrl Pts',(-1.65559044289746,-1.,0.98985562785445));
#31925=CARTESIAN_POINT('Ctrl Pts',(-1.65559044289746,1.,0.98985562785445));
#31926=CARTESIAN_POINT('Ctrl Pts',(-1.66001553809916,-1.,0.994121836661116));
#31927=CARTESIAN_POINT('Ctrl Pts',(-1.66001553809916,1.,0.994121836661116));
#31928=CARTESIAN_POINT('Ctrl Pts',(-1.66430758030304,-1.,0.998389654952317));
#31929=CARTESIAN_POINT('Ctrl Pts',(-1.66430758030304,1.,0.998389654952317));
#31930=CARTESIAN_POINT('Ctrl Pts',(-1.66846059277231,-1.,1.00265091003682));
#31931=CARTESIAN_POINT('Ctrl Pts',(-1.66846059277231,1.,1.00265091003682));
#31932=CARTESIAN_POINT('Ctrl Pts',(-1.67250335383248,-1.,1.00692206696387));
#31933=CARTESIAN_POINT('Ctrl Pts',(-1.67250335383248,1.,1.00692206696387));
#31934=CARTESIAN_POINT('Ctrl Pts',(-1.67648246776457,-1.,1.01123236493507));
#31935=CARTESIAN_POINT('Ctrl Pts',(-1.67648246776457,1.,1.01123236493507));
#31936=CARTESIAN_POINT('Ctrl Pts',(-1.6804428989482,-1.,1.01561026162787));
#31937=CARTESIAN_POINT('Ctrl Pts',(-1.6804428989482,1.,1.01561026162787));
#31938=CARTESIAN_POINT('Ctrl Pts',(-1.68440578021739,-1.,1.02006795074222));
#31939=CARTESIAN_POINT('Ctrl Pts',(-1.68440578021739,1.,1.02006795074222));
#31940=CARTESIAN_POINT('Ctrl Pts',(-1.68836910178475,-1.,1.02460180535272));
#31941=CARTESIAN_POINT('Ctrl Pts',(-1.68836910178475,1.,1.02460180535272));
#31942=CARTESIAN_POINT('Ctrl Pts',(-1.69231840863471,-1.,1.02919977579155));
#31943=CARTESIAN_POINT('Ctrl Pts',(-1.69231840863471,1.,1.02919977579155));
#31944=CARTESIAN_POINT('Ctrl Pts',(-1.69623414782769,-1.,1.03384646003587));
#31945=CARTESIAN_POINT('Ctrl Pts',(-1.69623414782769,1.,1.03384646003587));
#31946=CARTESIAN_POINT('Ctrl Pts',(-1.70010052930951,-1.,1.03852922490782));
#31947=CARTESIAN_POINT('Ctrl Pts',(-1.70010052930951,1.,1.03852922490782));
#31948=CARTESIAN_POINT('Ctrl Pts',(-1.70391338707969,-1.,1.04324363334546));
#31949=CARTESIAN_POINT('Ctrl Pts',(-1.70391338707969,1.,1.04324363334546));
#31950=CARTESIAN_POINT('Ctrl Pts',(-1.70767646263641,-1.,1.0479908540499));
#31951=CARTESIAN_POINT('Ctrl Pts',(-1.70767646263641,1.,1.0479908540499));
#31952=CARTESIAN_POINT('Ctrl Pts',(-1.71139783543986,-1.,1.05277517202854));
#31953=CARTESIAN_POINT('Ctrl Pts',(-1.71139783543986,1.,1.05277517202854));
#31954=CARTESIAN_POINT('Ctrl Pts',(-1.71508654427022,-1.,1.05760163192481));
#31955=CARTESIAN_POINT('Ctrl Pts',(-1.71508654427022,1.,1.05760163192481));
#31956=CARTESIAN_POINT('Ctrl Pts',(-1.71874858456908,-1.,1.0624732468065));
#31957=CARTESIAN_POINT('Ctrl Pts',(-1.71874858456908,1.,1.0624732468065));
#31958=CARTESIAN_POINT('Ctrl Pts',(-1.72238500928456,-1.,1.06738966975463));
#31959=CARTESIAN_POINT('Ctrl Pts',(-1.72238500928456,1.,1.06738966975463));
#31960=CARTESIAN_POINT('Ctrl Pts',(-1.72599406198489,-1.,1.07234866990252));
#31961=CARTESIAN_POINT('Ctrl Pts',(-1.72599406198489,1.,1.07234866990252));
#31962=CARTESIAN_POINT('Ctrl Pts',(-1.72957248977424,-1.,1.0773470373727));
#31963=CARTESIAN_POINT('Ctrl Pts',(-1.72957248977424,1.,1.0773470373727));
#31964=CARTESIAN_POINT('Ctrl Pts',(-1.73311705663407,-1.,1.08238162784749));
#31965=CARTESIAN_POINT('Ctrl Pts',(-1.73311705663407,1.,1.08238162784749));
#31966=CARTESIAN_POINT('Ctrl Pts',(-1.73662628326093,-1.,1.08745056285429));
#31967=CARTESIAN_POINT('Ctrl Pts',(-1.73662628326093,1.,1.08745056285429));
#31968=CARTESIAN_POINT('Ctrl Pts',(-1.74010053962252,-1.,1.09255329056496));
#31969=CARTESIAN_POINT('Ctrl Pts',(-1.74010053962252,1.,1.09255329056496));
#31970=CARTESIAN_POINT('Ctrl Pts',(-1.74354119236212,-1.,1.09768999241229));
#31971=CARTESIAN_POINT('Ctrl Pts',(-1.74354119236212,1.,1.09768999241229));
#31972=CARTESIAN_POINT('Ctrl Pts',(-1.74695004214924,-1.,1.10286118991144));
#31973=CARTESIAN_POINT('Ctrl Pts',(-1.74695004214924,1.,1.10286118991144));
#31974=CARTESIAN_POINT('Ctrl Pts',(-1.75032866075914,-1.,1.10806728183003));
#31975=CARTESIAN_POINT('Ctrl Pts',(-1.75032866075914,1.,1.10806728183003));
#31976=CARTESIAN_POINT('Ctrl Pts',(-1.75367772094617,-1.,1.11330807582542));
#31977=CARTESIAN_POINT('Ctrl Pts',(-1.75367772094617,1.,1.11330807582542));
#31978=CARTESIAN_POINT('Ctrl Pts',(-1.75699720772089,-1.,1.11858293216752));
#31979=CARTESIAN_POINT('Ctrl Pts',(-1.75699720772089,1.,1.11858293216752));
#31980=CARTESIAN_POINT('Ctrl Pts',(-1.76028671825084,-1.,1.12389096855078));
#31981=CARTESIAN_POINT('Ctrl Pts',(-1.76028671825084,1.,1.12389096855078));
#31982=CARTESIAN_POINT('Ctrl Pts',(-1.76354571966171,-1.,1.12923123555076));
#31983=CARTESIAN_POINT('Ctrl Pts',(-1.76354571966171,1.,1.12923123555076));
#31984=CARTESIAN_POINT('Ctrl Pts',(-1.76677384551883,-1.,1.13460291804635));
#31985=CARTESIAN_POINT('Ctrl Pts',(-1.76677384551883,1.,1.13460291804635));
#31986=CARTESIAN_POINT('Ctrl Pts',(-1.76997111386806,-1.,1.14000548337));
#31987=CARTESIAN_POINT('Ctrl Pts',(-1.76997111386806,1.,1.14000548337));
#31988=CARTESIAN_POINT('Ctrl Pts',(-1.77313777896234,-1.,1.14543858226948));
#31989=CARTESIAN_POINT('Ctrl Pts',(-1.77313777896234,1.,1.14543858226948));
#31990=CARTESIAN_POINT('Ctrl Pts',(-1.77627422557034,-1.,1.15090197841531));
#31991=CARTESIAN_POINT('Ctrl Pts',(-1.77627422557034,1.,1.15090197841531));
#31992=CARTESIAN_POINT('Ctrl Pts',(-1.77938085564261,-1.,1.15639547194689));
#31993=CARTESIAN_POINT('Ctrl Pts',(-1.77938085564261,1.,1.15639547194689));
#31994=CARTESIAN_POINT('Ctrl Pts',(-1.78245795880949,-1.,1.16191881298458));
#31995=CARTESIAN_POINT('Ctrl Pts',(-1.78245795880949,1.,1.16191881298458));
#31996=CARTESIAN_POINT('Ctrl Pts',(-1.78550566040349,-1.,1.16747166312239));
#31997=CARTESIAN_POINT('Ctrl Pts',(-1.78550566040349,1.,1.16747166312239));
#31998=CARTESIAN_POINT('Ctrl Pts',(-1.78852398877523,-1.,1.17305363177265));
#31999=CARTESIAN_POINT('Ctrl Pts',(-1.78852398877523,1.,1.17305363177265));
#32000=CARTESIAN_POINT('Ctrl Pts',(-1.79151291552646,-1.,1.17866429440781));
#32001=CARTESIAN_POINT('Ctrl Pts',(-1.79151291552646,1.,1.17866429440781));
#32002=CARTESIAN_POINT('Ctrl Pts',(-1.79447240321572,-1.,1.18430321697471));
#32003=CARTESIAN_POINT('Ctrl Pts',(-1.79447240321572,1.,1.18430321697471));
#32004=CARTESIAN_POINT('Ctrl Pts',(-1.79740245923649,-1.,1.1899699793456));
#32005=CARTESIAN_POINT('Ctrl Pts',(-1.79740245923649,1.,1.1899699793456));
#32006=CARTESIAN_POINT('Ctrl Pts',(-1.80030314370121,-1.,1.19566418930405));
#32007=CARTESIAN_POINT('Ctrl Pts',(-1.80030314370121,1.,1.19566418930405));
#32008=CARTESIAN_POINT('Ctrl Pts',(-1.8031745483882,-1.,1.2013854893912));
#32009=CARTESIAN_POINT('Ctrl Pts',(-1.8031745483882,1.,1.2013854893912));
#32010=CARTESIAN_POINT('Ctrl Pts',(-1.80601678480772,-1.,1.20713356605519));
#32011=CARTESIAN_POINT('Ctrl Pts',(-1.80601678480772,1.,1.20713356605519));
#32012=CARTESIAN_POINT('Ctrl Pts',(-1.80882996916931,-1.,1.2129081570818));
#32013=CARTESIAN_POINT('Ctrl Pts',(-1.80882996916931,1.,1.2129081570818));
#32014=CARTESIAN_POINT('Ctrl Pts',(-1.81161420806172,-1.,1.2187090610323));
#32015=CARTESIAN_POINT('Ctrl Pts',(-1.81161420806172,1.,1.2187090610323));
#32016=CARTESIAN_POINT('Ctrl Pts',(-1.81436959209778,-1.,1.22453613304507));
#32017=CARTESIAN_POINT('Ctrl Pts',(-1.81436959209778,1.,1.22453613304507));
#32018=CARTESIAN_POINT('Ctrl Pts',(-1.81655087183054,-1.,1.22921864890975));
#32019=CARTESIAN_POINT('Ctrl Pts',(-1.81655087183054,1.,1.22921864890975));
#32020=CARTESIAN_POINT('Ctrl Pts',(-1.81817389920914,-1.,1.23274224526804));
#32021=CARTESIAN_POINT('Ctrl Pts',(-1.81817389920914,1.,1.23274224526804));
#32022=CARTESIAN_POINT('Ctrl Pts',(-1.81925017193531,-1.,1.23509651170384));
#32023=CARTESIAN_POINT('Ctrl Pts',(-1.81925017193531,1.,1.23509651170384));
#32024=CARTESIAN_POINT('Ctrl Pts',(-1.81978687191668,-1.,1.23627494547115));
#32025=CARTESIAN_POINT('Ctrl Pts',(-1.81978687191668,1.,1.23627494547115));
#32026=CARTESIAN_POINT('',(-1.5055822144029,1.,0.892032620296855));
#32027=CARTESIAN_POINT('Ctrl Pts',(-1.5055822144029,1.,0.892032620296855));
#32028=CARTESIAN_POINT('Ctrl Pts',(-1.50980486807181,1.,0.894452006967538));
#32029=CARTESIAN_POINT('Ctrl Pts',(-1.51805569591479,1.,0.89918504749193));
#32030=CARTESIAN_POINT('Ctrl Pts',(-1.52984849890434,1.,0.905967409640499));
#32031=CARTESIAN_POINT('Ctrl Pts',(-1.54440491152808,1.,0.91437591904658));
#32032=CARTESIAN_POINT('Ctrl Pts',(-1.56065988582509,1.,0.923832188966322));
#32033=CARTESIAN_POINT('Ctrl Pts',(-1.57499388385561,1.,0.932246680128849));
#32034=CARTESIAN_POINT('Ctrl Pts',(-1.58744937489796,1.,0.939646377909319));
#32035=CARTESIAN_POINT('Ctrl Pts',(-1.59810042045408,1.,0.946078063325796));
#32036=CARTESIAN_POINT('Ctrl Pts',(-1.60706069897794,1.,0.951613284361248));
#32037=CARTESIAN_POINT('Ctrl Pts',(-1.61449324337233,1.,0.956354422921573));
#32038=CARTESIAN_POINT('Ctrl Pts',(-1.62061638139929,1.,0.960438326099958));
#32039=CARTESIAN_POINT('Ctrl Pts',(-1.6257193066974,1.,0.964046107037821));
#32040=CARTESIAN_POINT('Ctrl Pts',(-1.63013849959083,1.,0.967387853228041));
#32041=CARTESIAN_POINT('Ctrl Pts',(-1.63420665729609,1.,0.970669715996356));
#32042=CARTESIAN_POINT('Ctrl Pts',(-1.63820952658157,1.,0.974066058287501));
#32043=CARTESIAN_POINT('Ctrl Pts',(-1.64233990826831,1.,0.977689794120297));
#32044=CARTESIAN_POINT('Ctrl Pts',(-1.64665139190834,1.,0.981562530940574));
#32045=CARTESIAN_POINT('Ctrl Pts',(-1.6511001661277,1.,0.985642622921626));
#32046=CARTESIAN_POINT('Ctrl Pts',(-1.65559044289746,1.,0.98985562785445));
#32047=CARTESIAN_POINT('Ctrl Pts',(-1.66001553809916,1.,0.994121836661116));
#32048=CARTESIAN_POINT('Ctrl Pts',(-1.66430758030304,1.,0.998389654952317));
#32049=CARTESIAN_POINT('Ctrl Pts',(-1.66846059277231,1.,1.00265091003682));
#32050=CARTESIAN_POINT('Ctrl Pts',(-1.67250335383248,1.,1.00692206696387));
#32051=CARTESIAN_POINT('Ctrl Pts',(-1.67648246776457,1.,1.01123236493507));
#32052=CARTESIAN_POINT('Ctrl Pts',(-1.6804428989482,1.,1.01561026162787));
#32053=CARTESIAN_POINT('Ctrl Pts',(-1.68440578021739,1.,1.02006795074222));
#32054=CARTESIAN_POINT('Ctrl Pts',(-1.68836910178475,1.,1.02460180535272));
#32055=CARTESIAN_POINT('Ctrl Pts',(-1.69231840863471,1.,1.02919977579155));
#32056=CARTESIAN_POINT('Ctrl Pts',(-1.69623414782769,1.,1.03384646003587));
#32057=CARTESIAN_POINT('Ctrl Pts',(-1.70010052930951,1.,1.03852922490782));
#32058=CARTESIAN_POINT('Ctrl Pts',(-1.70391338707969,1.,1.04324363334546));
#32059=CARTESIAN_POINT('Ctrl Pts',(-1.70767646263641,1.,1.0479908540499));
#32060=CARTESIAN_POINT('Ctrl Pts',(-1.71139783543986,1.,1.05277517202854));
#32061=CARTESIAN_POINT('Ctrl Pts',(-1.71508654427022,1.,1.05760163192481));
#32062=CARTESIAN_POINT('Ctrl Pts',(-1.71874858456908,1.,1.0624732468065));
#32063=CARTESIAN_POINT('Ctrl Pts',(-1.72238500928456,1.,1.06738966975463));
#32064=CARTESIAN_POINT('Ctrl Pts',(-1.72599406198489,1.,1.07234866990252));
#32065=CARTESIAN_POINT('Ctrl Pts',(-1.72957248977424,1.,1.0773470373727));
#32066=CARTESIAN_POINT('Ctrl Pts',(-1.73311705663407,1.,1.08238162784749));
#32067=CARTESIAN_POINT('Ctrl Pts',(-1.73662628326093,1.,1.08745056285429));
#32068=CARTESIAN_POINT('Ctrl Pts',(-1.74010053962252,1.,1.09255329056496));
#32069=CARTESIAN_POINT('Ctrl Pts',(-1.74354119236212,1.,1.09768999241229));
#32070=CARTESIAN_POINT('Ctrl Pts',(-1.74695004214924,1.,1.10286118991144));
#32071=CARTESIAN_POINT('Ctrl Pts',(-1.75032866075914,1.,1.10806728183003));
#32072=CARTESIAN_POINT('Ctrl Pts',(-1.75367772094617,1.,1.11330807582542));
#32073=CARTESIAN_POINT('Ctrl Pts',(-1.75699720772089,1.,1.11858293216752));
#32074=CARTESIAN_POINT('Ctrl Pts',(-1.76028671825084,1.,1.12389096855078));
#32075=CARTESIAN_POINT('Ctrl Pts',(-1.76354571966171,1.,1.12923123555076));
#32076=CARTESIAN_POINT('Ctrl Pts',(-1.76677384551883,1.,1.13460291804635));
#32077=CARTESIAN_POINT('Ctrl Pts',(-1.76997111386806,1.,1.14000548337));
#32078=CARTESIAN_POINT('Ctrl Pts',(-1.77313777896234,1.,1.14543858226948));
#32079=CARTESIAN_POINT('Ctrl Pts',(-1.77627422557034,1.,1.15090197841531));
#32080=CARTESIAN_POINT('Ctrl Pts',(-1.77938085564261,1.,1.15639547194689));
#32081=CARTESIAN_POINT('Ctrl Pts',(-1.78245795880949,1.,1.16191881298458));
#32082=CARTESIAN_POINT('Ctrl Pts',(-1.78550566040349,1.,1.16747166312239));
#32083=CARTESIAN_POINT('Ctrl Pts',(-1.78852398877523,1.,1.17305363177265));
#32084=CARTESIAN_POINT('Ctrl Pts',(-1.79151291552646,1.,1.17866429440781));
#32085=CARTESIAN_POINT('Ctrl Pts',(-1.79447240321572,1.,1.18430321697471));
#32086=CARTESIAN_POINT('Ctrl Pts',(-1.79740245923649,1.,1.1899699793456));
#32087=CARTESIAN_POINT('Ctrl Pts',(-1.80030314370121,1.,1.19566418930405));
#32088=CARTESIAN_POINT('Ctrl Pts',(-1.8031745483882,1.,1.2013854893912));
#32089=CARTESIAN_POINT('Ctrl Pts',(-1.80601678480772,1.,1.20713356605519));
#32090=CARTESIAN_POINT('Ctrl Pts',(-1.80882996916931,1.,1.2129081570818));
#32091=CARTESIAN_POINT('Ctrl Pts',(-1.81161420806172,1.,1.2187090610323));
#32092=CARTESIAN_POINT('Ctrl Pts',(-1.81436959209778,1.,1.22453613304507));
#32093=CARTESIAN_POINT('Ctrl Pts',(-1.81655087183054,1.,1.22921864890975));
#32094=CARTESIAN_POINT('Ctrl Pts',(-1.81817389920914,1.,1.23274224526804));
#32095=CARTESIAN_POINT('Ctrl Pts',(-1.81925017193531,1.,1.23509651170384));
#32096=CARTESIAN_POINT('Ctrl Pts',(-1.81978687191668,1.,1.23627494547115));
#32097=CARTESIAN_POINT('',(-1.5055822144029,0.,0.892032620296856));
#32098=CARTESIAN_POINT('Origin',(0.,0.,0.));
#32099=CARTESIAN_POINT('',(-1.60662857109684,1.,0.693717979106305));
#32100=CARTESIAN_POINT('Origin',(0.,1.,0.));
#32101=CARTESIAN_POINT('',(-1.60662857109684,0.,0.693717979106306));
#32102=CARTESIAN_POINT('Ctrl Pts',(-2.0698113262342,-1.,0.7455743247944));
#32103=CARTESIAN_POINT('Ctrl Pts',(-2.0698113262342,1.,0.7455743247944));
#32104=CARTESIAN_POINT('Ctrl Pts',(-2.06854248895728,-1.,0.745832791378367));
#32105=CARTESIAN_POINT('Ctrl Pts',(-2.06854248895728,1.,0.745832791378367));
#32106=CARTESIAN_POINT('Ctrl Pts',(-2.06600523016815,-1.,0.7463458715442));
#32107=CARTESIAN_POINT('Ctrl Pts',(-2.06600523016815,1.,0.7463458715442));
#32108=CARTESIAN_POINT('Ctrl Pts',(-2.06220058927826,-1.,0.747103932787919));
#32109=CARTESIAN_POINT('Ctrl Pts',(-2.06220058927826,1.,0.747103932787919));
#32110=CARTESIAN_POINT('Ctrl Pts',(-2.05713023031006,-1.,0.748091554183802));
#32111=CARTESIAN_POINT('Ctrl Pts',(-2.05713023031006,1.,0.748091554183802));
#32112=CARTESIAN_POINT('Ctrl Pts',(-2.05079645592154,-1.,0.749287468665046));
#32113=CARTESIAN_POINT('Ctrl Pts',(-2.05079645592154,1.,0.749287468665046));
#32114=CARTESIAN_POINT('Ctrl Pts',(-2.04446689147979,-1.,0.750444657875576));
#32115=CARTESIAN_POINT('Ctrl Pts',(-2.04446689147979,1.,0.750444657875576));
#32116=CARTESIAN_POINT('Ctrl Pts',(-2.03814160092099,-1.,0.751562963361115));
#32117=CARTESIAN_POINT('Ctrl Pts',(-2.03814160092099,1.,0.751562963361115));
#32118=CARTESIAN_POINT('Ctrl Pts',(-2.03182068456221,-1.,0.752642180487211));
#32119=CARTESIAN_POINT('Ctrl Pts',(-2.03182068456221,1.,0.752642180487211));
#32120=CARTESIAN_POINT('Ctrl Pts',(-2.02550428623313,-1.,0.753682061112768));
#32121=CARTESIAN_POINT('Ctrl Pts',(-2.02550428623313,1.,0.753682061112768));
#32122=CARTESIAN_POINT('Ctrl Pts',(-2.01919259405809,-1.,0.754682330722816));
#32123=CARTESIAN_POINT('Ctrl Pts',(-2.01919259405809,1.,0.754682330722816));
#32124=CARTESIAN_POINT('Ctrl Pts',(-2.01288584328084,-1.,0.755642704957865));
#32125=CARTESIAN_POINT('Ctrl Pts',(-2.01288584328084,1.,0.755642704957865));
#32126=CARTESIAN_POINT('Ctrl Pts',(-2.0065843158773,-1.,0.75656290464667));
#32127=CARTESIAN_POINT('Ctrl Pts',(-2.0065843158773,1.,0.75656290464667));
#32128=CARTESIAN_POINT('Ctrl Pts',(-2.00028834739178,-1.,0.757442676862724));
#32129=CARTESIAN_POINT('Ctrl Pts',(-2.00028834739178,1.,0.757442676862724));
#32130=CARTESIAN_POINT('Ctrl Pts',(-1.99399831098817,-1.,0.758281796766761));
#32131=CARTESIAN_POINT('Ctrl Pts',(-1.99399831098817,1.,0.758281796766761));
#32132=CARTESIAN_POINT('Ctrl Pts',(-1.98771456680874,-1.,0.759080037802488));
#32133=CARTESIAN_POINT('Ctrl Pts',(-1.98771456680874,1.,0.759080037802488));
#32134=CARTESIAN_POINT('Ctrl Pts',(-1.98143741418172,-1.,0.75983714745219));
#32135=CARTESIAN_POINT('Ctrl Pts',(-1.98143741418172,1.,0.75983714745219));
#32136=CARTESIAN_POINT('Ctrl Pts',(-1.97516705321494,-1.,0.760552825409757));
#32137=CARTESIAN_POINT('Ctrl Pts',(-1.97516705321494,1.,0.760552825409757));
#32138=CARTESIAN_POINT('Ctrl Pts',(-1.96890351582499,-1.,0.76122669048382));
#32139=CARTESIAN_POINT('Ctrl Pts',(-1.96890351582499,1.,0.76122669048382));
#32140=CARTESIAN_POINT('Ctrl Pts',(-1.96264672744186,-1.,0.761858300014423));
#32141=CARTESIAN_POINT('Ctrl Pts',(-1.96264672744186,1.,0.761858300014423));
#32142=CARTESIAN_POINT('Ctrl Pts',(-1.95639665309869,-1.,0.762447203806179));
#32143=CARTESIAN_POINT('Ctrl Pts',(-1.95639665309869,1.,0.762447203806179));
#32144=CARTESIAN_POINT('Ctrl Pts',(-1.95015342590024,-1.,0.762992990878769));
#32145=CARTESIAN_POINT('Ctrl Pts',(-1.95015342590024,1.,0.762992990878769));
#32146=CARTESIAN_POINT('Ctrl Pts',(-1.9439174661764,-1.,0.763495333538629));
#32147=CARTESIAN_POINT('Ctrl Pts',(-1.9439174661764,1.,0.763495333538629));
#32148=CARTESIAN_POINT('Ctrl Pts',(-1.93768964875886,-1.,0.763954049121458));
#32149=CARTESIAN_POINT('Ctrl Pts',(-1.93768964875886,1.,0.763954049121458));
#32150=CARTESIAN_POINT('Ctrl Pts',(-1.93147105496382,-1.,0.76436901067394));
#32151=CARTESIAN_POINT('Ctrl Pts',(-1.93147105496382,1.,0.76436901067394));
#32152=CARTESIAN_POINT('Ctrl Pts',(-1.92526263537048,-1.,0.764740025488211));
#32153=CARTESIAN_POINT('Ctrl Pts',(-1.92526263537048,1.,0.764740025488211));
#32154=CARTESIAN_POINT('Ctrl Pts',(-1.91906491634196,-1.,0.765066729667088));
#32155=CARTESIAN_POINT('Ctrl Pts',(-1.91906491634196,1.,0.765066729667088));
#32156=CARTESIAN_POINT('Ctrl Pts',(-1.91287765805169,-1.,0.765348465884722));
#32157=CARTESIAN_POINT('Ctrl Pts',(-1.91287765805169,1.,0.765348465884722));
#32158=CARTESIAN_POINT('Ctrl Pts',(-1.90669961402356,-1.,0.765584196937919));
#32159=CARTESIAN_POINT('Ctrl Pts',(-1.90669961402356,1.,0.765584196937919));
#32160=CARTESIAN_POINT('Ctrl Pts',(-1.90052930393596,-1.,0.765772772593386));
#32161=CARTESIAN_POINT('Ctrl Pts',(-1.90052930393596,1.,0.765772772593386));
#32162=CARTESIAN_POINT('Ctrl Pts',(-1.89436577771388,-1.,0.765913193856978));
#32163=CARTESIAN_POINT('Ctrl Pts',(-1.89436577771388,1.,0.765913193856978));
#32164=CARTESIAN_POINT('Ctrl Pts',(-1.88820926433409,-1.,0.766004837062091));
#32165=CARTESIAN_POINT('Ctrl Pts',(-1.88820926433409,1.,0.766004837062091));
#32166=CARTESIAN_POINT('Ctrl Pts',(-1.88206215302561,-1.,0.766047794851864));
#32167=CARTESIAN_POINT('Ctrl Pts',(-1.88206215302561,1.,0.766047794851864));
#32168=CARTESIAN_POINT('Ctrl Pts',(-1.87592888967883,-1.,0.766042837036744));
#32169=CARTESIAN_POINT('Ctrl Pts',(-1.87592888967883,1.,0.766042837036744));
#32170=CARTESIAN_POINT('Ctrl Pts',(-1.86981398314341,-1.,0.765990708546091));
#32171=CARTESIAN_POINT('Ctrl Pts',(-1.86981398314341,1.,0.765990708546091));
#32172=CARTESIAN_POINT('Ctrl Pts',(-1.86372027063312,-1.,0.765891519092547));
#32173=CARTESIAN_POINT('Ctrl Pts',(-1.86372027063312,1.,0.765891519092547));
#32174=CARTESIAN_POINT('Ctrl Pts',(-1.85764741390394,-1.,0.765744212909318));
#32175=CARTESIAN_POINT('Ctrl Pts',(-1.85764741390394,1.,0.765744212909318));
#32176=CARTESIAN_POINT('Ctrl Pts',(-1.85158945130063,-1.,0.765545710619062));
#32177=CARTESIAN_POINT('Ctrl Pts',(-1.85158945130063,1.,0.765545710619062));
#32178=CARTESIAN_POINT('Ctrl Pts',(-1.84553698875924,-1.,0.765291664862029));
#32179=CARTESIAN_POINT('Ctrl Pts',(-1.84553698875924,1.,0.765291664862029));
#32180=CARTESIAN_POINT('Ctrl Pts',(-1.83948181064835,-1.,0.764978057881737));
#32181=CARTESIAN_POINT('Ctrl Pts',(-1.83948181064835,1.,0.764978057881737));
#32182=CARTESIAN_POINT('Ctrl Pts',(-1.83342077227142,-1.,0.764602549687853));
#32183=CARTESIAN_POINT('Ctrl Pts',(-1.83342077227142,1.,0.764602549687853));
#32184=CARTESIAN_POINT('Ctrl Pts',(-1.82735991200065,-1.,0.764165902605995));
#32185=CARTESIAN_POINT('Ctrl Pts',(-1.82735991200065,1.,0.764165902605995));
#32186=CARTESIAN_POINT('Ctrl Pts',(-1.82131873145266,-1.,0.763673465462726));
#32187=CARTESIAN_POINT('Ctrl Pts',(-1.82131873145266,1.,0.763673465462726));
#32188=CARTESIAN_POINT('Ctrl Pts',(-1.8153211840553,-1.,0.763132003836634));
#32189=CARTESIAN_POINT('Ctrl Pts',(-1.8153211840553,1.,0.763132003836634));
#32190=CARTESIAN_POINT('Ctrl Pts',(-1.80938551463965,-1.,0.762546129463938));
#32191=CARTESIAN_POINT('Ctrl Pts',(-1.80938551463965,1.,0.762546129463938));
#32192=CARTESIAN_POINT('Ctrl Pts',(-1.80351583877342,-1.,0.761915336443547));
#32193=CARTESIAN_POINT('Ctrl Pts',(-1.80351583877342,1.,0.761915336443547));
#32194=CARTESIAN_POINT('Ctrl Pts',(-1.79768986997783,-1.,0.761229695230558));
#32195=CARTESIAN_POINT('Ctrl Pts',(-1.79768986997783,1.,0.761229695230558));
#32196=CARTESIAN_POINT('Ctrl Pts',(-1.7918581561088,-1.,0.760469555880749));
#32197=CARTESIAN_POINT('Ctrl Pts',(-1.7918581561088,1.,0.760469555880749));
#32198=CARTESIAN_POINT('Ctrl Pts',(-1.78596964884604,-1.,0.759614401110189));
#32199=CARTESIAN_POINT('Ctrl Pts',(-1.78596964884604,1.,0.759614401110189));
#32200=CARTESIAN_POINT('Ctrl Pts',(-1.77999411220945,-1.,0.758650626677518));
#32201=CARTESIAN_POINT('Ctrl Pts',(-1.77999411220945,1.,0.758650626677518));
#32202=CARTESIAN_POINT('Ctrl Pts',(-1.77394167108292,-1.,0.757578264077029));
#32203=CARTESIAN_POINT('Ctrl Pts',(-1.77394167108292,1.,0.757578264077029));
#32204=CARTESIAN_POINT('Ctrl Pts',(-1.76789396002998,-1.,0.75642189602781));
#32205=CARTESIAN_POINT('Ctrl Pts',(-1.76789396002998,1.,0.75642189602781));
#32206=CARTESIAN_POINT('Ctrl Pts',(-1.76197817240128,-1.,0.755220979974461));
#32207=CARTESIAN_POINT('Ctrl Pts',(-1.76197817240128,1.,0.755220979974461));
#32208=CARTESIAN_POINT('Ctrl Pts',(-1.75631083600019,-1.,0.754009254027829));
#32209=CARTESIAN_POINT('Ctrl Pts',(-1.75631083600019,1.,0.754009254027829));
#32210=CARTESIAN_POINT('Ctrl Pts',(-1.75095139468794,-1.,0.752797683531314));
#32211=CARTESIAN_POINT('Ctrl Pts',(-1.75095139468794,1.,0.752797683531314));
#32212=CARTESIAN_POINT('Ctrl Pts',(-1.74585086852502,-1.,0.751555614164482));
#32213=CARTESIAN_POINT('Ctrl Pts',(-1.74585086852502,1.,0.751555614164482));
#32214=CARTESIAN_POINT('Ctrl Pts',(-1.74080458267114,-1.,0.750193435981249));
#32215=CARTESIAN_POINT('Ctrl Pts',(-1.74080458267114,1.,0.750193435981249));
#32216=CARTESIAN_POINT('Ctrl Pts',(-1.7355035168033,-1.,0.74858246295687));
#32217=CARTESIAN_POINT('Ctrl Pts',(-1.7355035168033,1.,0.74858246295687));
#32218=CARTESIAN_POINT('Ctrl Pts',(-1.72958533647714,-1.,0.746574710097752));
#32219=CARTESIAN_POINT('Ctrl Pts',(-1.72958533647714,1.,0.746574710097752));
#32220=CARTESIAN_POINT('Ctrl Pts',(-1.72268229916769,-1.,0.744021445433093));
#32221=CARTESIAN_POINT('Ctrl Pts',(-1.72268229916769,1.,0.744021445433093));
#32222=CARTESIAN_POINT('Ctrl Pts',(-1.71447789751001,-1.,0.74079516202821));
#32223=CARTESIAN_POINT('Ctrl Pts',(-1.71447789751001,1.,0.74079516202821));
#32224=CARTESIAN_POINT('Ctrl Pts',(-1.70473309004249,-1.,0.736799665716932));
#32225=CARTESIAN_POINT('Ctrl Pts',(-1.70473309004249,1.,0.736799665716932));
#32226=CARTESIAN_POINT('Ctrl Pts',(-1.69326921972915,-1.,0.731963238685357));
#32227=CARTESIAN_POINT('Ctrl Pts',(-1.69326921972915,1.,0.731963238685357));
#32228=CARTESIAN_POINT('Ctrl Pts',(-1.67996158451922,-1.,0.726235967982445));
#32229=CARTESIAN_POINT('Ctrl Pts',(-1.67996158451922,1.,0.726235967982445));
#32230=CARTESIAN_POINT('Ctrl Pts',(-1.66472880551777,-1.,0.71958543378795));
#32231=CARTESIAN_POINT('Ctrl Pts',(-1.66472880551777,1.,0.71958543378795));
#32232=CARTESIAN_POINT('Ctrl Pts',(-1.64752408828442,-1.,0.711993139340447));
#32233=CARTESIAN_POINT('Ctrl Pts',(-1.64752408828442,1.,0.711993139340447));
#32234=CARTESIAN_POINT('Ctrl Pts',(-1.6321654166204,-1.,0.705159151977294));
#32235=CARTESIAN_POINT('Ctrl Pts',(-1.6321654166204,1.,0.705159151977294));
#32236=CARTESIAN_POINT('Ctrl Pts',(-1.61974673471117,-1.,0.699605146398837));
#32237=CARTESIAN_POINT('Ctrl Pts',(-1.61974673471117,1.,0.699605146398837));
#32238=CARTESIAN_POINT('Ctrl Pts',(-1.61106790957619,-1.,0.69571209787897));
#32239=CARTESIAN_POINT('Ctrl Pts',(-1.61106790957619,1.,0.69571209787897));
#32240=CARTESIAN_POINT('Ctrl Pts',(-1.60662857109684,-1.,0.693717979106305));
#32241=CARTESIAN_POINT('Ctrl Pts',(-1.60662857109684,1.,0.693717979106305));
#32242=CARTESIAN_POINT('',(-2.0698113262342,1.,0.7455743247944));
#32243=CARTESIAN_POINT('Ctrl Pts',(-2.0698113262342,1.,0.7455743247944));
#32244=CARTESIAN_POINT('Ctrl Pts',(-2.06854248895728,1.,0.745832791378367));
#32245=CARTESIAN_POINT('Ctrl Pts',(-2.06600523016815,1.,0.7463458715442));
#32246=CARTESIAN_POINT('Ctrl Pts',(-2.06220058927826,1.,0.747103932787919));
#32247=CARTESIAN_POINT('Ctrl Pts',(-2.05713023031006,1.,0.748091554183802));
#32248=CARTESIAN_POINT('Ctrl Pts',(-2.05079645592154,1.,0.749287468665046));
#32249=CARTESIAN_POINT('Ctrl Pts',(-2.04446689147979,1.,0.750444657875576));
#32250=CARTESIAN_POINT('Ctrl Pts',(-2.03814160092099,1.,0.751562963361115));
#32251=CARTESIAN_POINT('Ctrl Pts',(-2.03182068456221,1.,0.752642180487211));
#32252=CARTESIAN_POINT('Ctrl Pts',(-2.02550428623313,1.,0.753682061112768));
#32253=CARTESIAN_POINT('Ctrl Pts',(-2.01919259405809,1.,0.754682330722816));
#32254=CARTESIAN_POINT('Ctrl Pts',(-2.01288584328084,1.,0.755642704957865));
#32255=CARTESIAN_POINT('Ctrl Pts',(-2.0065843158773,1.,0.75656290464667));
#32256=CARTESIAN_POINT('Ctrl Pts',(-2.00028834739178,1.,0.757442676862724));
#32257=CARTESIAN_POINT('Ctrl Pts',(-1.99399831098817,1.,0.758281796766761));
#32258=CARTESIAN_POINT('Ctrl Pts',(-1.98771456680874,1.,0.759080037802488));
#32259=CARTESIAN_POINT('Ctrl Pts',(-1.98143741418172,1.,0.75983714745219));
#32260=CARTESIAN_POINT('Ctrl Pts',(-1.97516705321494,1.,0.760552825409757));
#32261=CARTESIAN_POINT('Ctrl Pts',(-1.96890351582499,1.,0.76122669048382));
#32262=CARTESIAN_POINT('Ctrl Pts',(-1.96264672744186,1.,0.761858300014423));
#32263=CARTESIAN_POINT('Ctrl Pts',(-1.95639665309869,1.,0.762447203806179));
#32264=CARTESIAN_POINT('Ctrl Pts',(-1.95015342590024,1.,0.762992990878769));
#32265=CARTESIAN_POINT('Ctrl Pts',(-1.9439174661764,1.,0.763495333538629));
#32266=CARTESIAN_POINT('Ctrl Pts',(-1.93768964875886,1.,0.763954049121458));
#32267=CARTESIAN_POINT('Ctrl Pts',(-1.93147105496382,1.,0.76436901067394));
#32268=CARTESIAN_POINT('Ctrl Pts',(-1.92526263537048,1.,0.764740025488211));
#32269=CARTESIAN_POINT('Ctrl Pts',(-1.91906491634196,1.,0.765066729667088));
#32270=CARTESIAN_POINT('Ctrl Pts',(-1.91287765805169,1.,0.765348465884722));
#32271=CARTESIAN_POINT('Ctrl Pts',(-1.90669961402356,1.,0.765584196937919));
#32272=CARTESIAN_POINT('Ctrl Pts',(-1.90052930393596,1.,0.765772772593386));
#32273=CARTESIAN_POINT('Ctrl Pts',(-1.89436577771388,1.,0.765913193856978));
#32274=CARTESIAN_POINT('Ctrl Pts',(-1.88820926433409,1.,0.766004837062091));
#32275=CARTESIAN_POINT('Ctrl Pts',(-1.88206215302561,1.,0.766047794851864));
#32276=CARTESIAN_POINT('Ctrl Pts',(-1.87592888967883,1.,0.766042837036744));
#32277=CARTESIAN_POINT('Ctrl Pts',(-1.86981398314341,1.,0.765990708546091));
#32278=CARTESIAN_POINT('Ctrl Pts',(-1.86372027063312,1.,0.765891519092547));
#32279=CARTESIAN_POINT('Ctrl Pts',(-1.85764741390394,1.,0.765744212909318));
#32280=CARTESIAN_POINT('Ctrl Pts',(-1.85158945130063,1.,0.765545710619062));
#32281=CARTESIAN_POINT('Ctrl Pts',(-1.84553698875924,1.,0.765291664862029));
#32282=CARTESIAN_POINT('Ctrl Pts',(-1.83948181064835,1.,0.764978057881737));
#32283=CARTESIAN_POINT('Ctrl Pts',(-1.83342077227142,1.,0.764602549687853));
#32284=CARTESIAN_POINT('Ctrl Pts',(-1.82735991200065,1.,0.764165902605995));
#32285=CARTESIAN_POINT('Ctrl Pts',(-1.82131873145266,1.,0.763673465462726));
#32286=CARTESIAN_POINT('Ctrl Pts',(-1.8153211840553,1.,0.763132003836634));
#32287=CARTESIAN_POINT('Ctrl Pts',(-1.80938551463965,1.,0.762546129463938));
#32288=CARTESIAN_POINT('Ctrl Pts',(-1.80351583877342,1.,0.761915336443547));
#32289=CARTESIAN_POINT('Ctrl Pts',(-1.79768986997783,1.,0.761229695230558));
#32290=CARTESIAN_POINT('Ctrl Pts',(-1.7918581561088,1.,0.760469555880749));
#32291=CARTESIAN_POINT('Ctrl Pts',(-1.78596964884604,1.,0.759614401110189));
#32292=CARTESIAN_POINT('Ctrl Pts',(-1.77999411220945,1.,0.758650626677518));
#32293=CARTESIAN_POINT('Ctrl Pts',(-1.77394167108292,1.,0.757578264077029));
#32294=CARTESIAN_POINT('Ctrl Pts',(-1.76789396002998,1.,0.75642189602781));
#32295=CARTESIAN_POINT('Ctrl Pts',(-1.76197817240128,1.,0.755220979974461));
#32296=CARTESIAN_POINT('Ctrl Pts',(-1.75631083600019,1.,0.754009254027829));
#32297=CARTESIAN_POINT('Ctrl Pts',(-1.75095139468794,1.,0.752797683531314));
#32298=CARTESIAN_POINT('Ctrl Pts',(-1.74585086852502,1.,0.751555614164482));
#32299=CARTESIAN_POINT('Ctrl Pts',(-1.74080458267114,1.,0.750193435981249));
#32300=CARTESIAN_POINT('Ctrl Pts',(-1.7355035168033,1.,0.74858246295687));
#32301=CARTESIAN_POINT('Ctrl Pts',(-1.72958533647714,1.,0.746574710097752));
#32302=CARTESIAN_POINT('Ctrl Pts',(-1.72268229916769,1.,0.744021445433093));
#32303=CARTESIAN_POINT('Ctrl Pts',(-1.71447789751001,1.,0.74079516202821));
#32304=CARTESIAN_POINT('Ctrl Pts',(-1.70473309004249,1.,0.736799665716932));
#32305=CARTESIAN_POINT('Ctrl Pts',(-1.69326921972915,1.,0.731963238685357));
#32306=CARTESIAN_POINT('Ctrl Pts',(-1.67996158451922,1.,0.726235967982445));
#32307=CARTESIAN_POINT('Ctrl Pts',(-1.66472880551777,1.,0.71958543378795));
#32308=CARTESIAN_POINT('Ctrl Pts',(-1.64752408828442,1.,0.711993139340447));
#32309=CARTESIAN_POINT('Ctrl Pts',(-1.6321654166204,1.,0.705159151977294));
#32310=CARTESIAN_POINT('Ctrl Pts',(-1.61974673471117,1.,0.699605146398837));
#32311=CARTESIAN_POINT('Ctrl Pts',(-1.61106790957619,1.,0.69571209787897));
#32312=CARTESIAN_POINT('Ctrl Pts',(-1.60662857109684,1.,0.693717979106305));
#32313=CARTESIAN_POINT('',(-2.0698113262342,0.,0.7455743247944));
#32314=CARTESIAN_POINT('Origin',(-2.11275013067528,0.,0.61342227326009));
#32315=CARTESIAN_POINT('',(-2.11275013067528,1.,0.61342227326009));
#32316=CARTESIAN_POINT('',(-2.0698113262342,1.,0.7455743247944));
#32317=CARTESIAN_POINT('',(-2.11275013067528,0.,0.61342227326009));
#32318=CARTESIAN_POINT('Ctrl Pts',(-1.7075470150345,-1.,0.383122945602004));
#32319=CARTESIAN_POINT('Ctrl Pts',(-1.7075470150345,1.,0.383122945602004));
#32320=CARTESIAN_POINT('Ctrl Pts',(-1.71231062891958,-1.,0.384119047315542));
#32321=CARTESIAN_POINT('Ctrl Pts',(-1.71231062891958,1.,0.384119047315542));
#32322=CARTESIAN_POINT('Ctrl Pts',(-1.72162022246158,-1.,0.38607079032701));
#32323=CARTESIAN_POINT('Ctrl Pts',(-1.72162022246158,1.,0.38607079032701));
#32324=CARTESIAN_POINT('Ctrl Pts',(-1.7349317097561,-1.,0.388877023509191));
#32325=CARTESIAN_POINT('Ctrl Pts',(-1.7349317097561,1.,0.388877023509191));
#32326=CARTESIAN_POINT('Ctrl Pts',(-1.75137405313962,-1.,0.392375812294307));
#32327=CARTESIAN_POINT('Ctrl Pts',(-1.75137405313962,1.,0.392375812294307));
#32328=CARTESIAN_POINT('Ctrl Pts',(-1.7697556004756,-1.,0.39634619612042));
#32329=CARTESIAN_POINT('Ctrl Pts',(-1.7697556004756,1.,0.39634619612042));
#32330=CARTESIAN_POINT('Ctrl Pts',(-1.78598826347533,-1.,0.39991940378308));
#32331=CARTESIAN_POINT('Ctrl Pts',(-1.78598826347533,1.,0.39991940378308));
#32332=CARTESIAN_POINT('Ctrl Pts',(-1.80012077176221,-1.,0.403107976170441));
#32333=CARTESIAN_POINT('Ctrl Pts',(-1.80012077176221,1.,0.403107976170441));
#32334=CARTESIAN_POINT('Ctrl Pts',(-1.81223801813988,-1.,0.405933518411838));
#32335=CARTESIAN_POINT('Ctrl Pts',(-1.81223801813988,1.,0.405933518411838));
#32336=CARTESIAN_POINT('Ctrl Pts',(-1.8224702267854,-1.,0.408428948108533));
#32337=CARTESIAN_POINT('Ctrl Pts',(-1.8224702267854,1.,0.408428948108533));
#32338=CARTESIAN_POINT('Ctrl Pts',(-1.83100408895216,-1.,0.410641256301675));
#32339=CARTESIAN_POINT('Ctrl Pts',(-1.83100408895216,1.,0.410641256301675));
#32340=CARTESIAN_POINT('Ctrl Pts',(-1.83808953475839,-1.,0.412633125322161));
#32341=CARTESIAN_POINT('Ctrl Pts',(-1.83808953475839,1.,0.412633125322161));
#32342=CARTESIAN_POINT('Ctrl Pts',(-1.8440575707371,-1.,0.41448743825434));
#32343=CARTESIAN_POINT('Ctrl Pts',(-1.8440575707371,1.,0.41448743825434));
#32344=CARTESIAN_POINT('Ctrl Pts',(-1.84929312929882,-1.,0.416300022038864));
#32345=CARTESIAN_POINT('Ctrl Pts',(-1.84929312929882,1.,0.416300022038864));
#32346=CARTESIAN_POINT('Ctrl Pts',(-1.85417632856234,-1.,0.418164129143534));
#32347=CARTESIAN_POINT('Ctrl Pts',(-1.85417632856234,1.,0.418164129143534));
#32348=CARTESIAN_POINT('Ctrl Pts',(-1.85903281096686,-1.,0.420157287975619));
#32349=CARTESIAN_POINT('Ctrl Pts',(-1.85903281096686,1.,0.420157287975619));
#32350=CARTESIAN_POINT('Ctrl Pts',(-1.86408083334028,-1.,0.422327307418275));
#32351=CARTESIAN_POINT('Ctrl Pts',(-1.86408083334028,1.,0.422327307418275));
#32352=CARTESIAN_POINT('Ctrl Pts',(-1.86937803944323,-1.,0.424678177291359));
#32353=CARTESIAN_POINT('Ctrl Pts',(-1.86937803944323,1.,0.424678177291359));
#32354=CARTESIAN_POINT('Ctrl Pts',(-1.87486989291484,-1.,0.427183828519102));
#32355=CARTESIAN_POINT('Ctrl Pts',(-1.87486989291484,1.,0.427183828519102));
#32356=CARTESIAN_POINT('Ctrl Pts',(-1.88044229001832,-1.,0.429803062482344));
#32357=CARTESIAN_POINT('Ctrl Pts',(-1.88044229001832,1.,0.429803062482344));
#32358=CARTESIAN_POINT('Ctrl Pts',(-1.88596913666793,-1.,0.432493038548748));
#32359=CARTESIAN_POINT('Ctrl Pts',(-1.88596913666793,1.,0.432493038548748));
#32360=CARTESIAN_POINT('Ctrl Pts',(-1.89136993975504,-1.,0.435225660963383));
#32361=CARTESIAN_POINT('Ctrl Pts',(-1.89136993975504,1.,0.435225660963383));
#32362=CARTESIAN_POINT('Ctrl Pts',(-1.89663648956466,-1.,0.437995003948244));
#32363=CARTESIAN_POINT('Ctrl Pts',(-1.89663648956466,1.,0.437995003948244));
#32364=CARTESIAN_POINT('Ctrl Pts',(-1.90180124389086,-1.,0.440807833704038));
#32365=CARTESIAN_POINT('Ctrl Pts',(-1.90180124389086,1.,0.440807833704038));
#32366=CARTESIAN_POINT('Ctrl Pts',(-1.90691756144898,-1.,0.44367755684915));
#32367=CARTESIAN_POINT('Ctrl Pts',(-1.90691756144898,1.,0.44367755684915));
#32368=CARTESIAN_POINT('Ctrl Pts',(-1.9120369998112,-1.,0.446617343485711));
#32369=CARTESIAN_POINT('Ctrl Pts',(-1.9120369998112,1.,0.446617343485711));
#32370=CARTESIAN_POINT('Ctrl Pts',(-1.91718342555755,-1.,0.449632260106662));
#32371=CARTESIAN_POINT('Ctrl Pts',(-1.91718342555755,1.,0.449632260106662));
#32372=CARTESIAN_POINT('Ctrl Pts',(-1.92235380648502,-1.,0.452719478359432));
#32373=CARTESIAN_POINT('Ctrl Pts',(-1.92235380648502,1.,0.452719478359432));
#32374=CARTESIAN_POINT('Ctrl Pts',(-1.92753067150476,-1.,0.455872005174371));
#32375=CARTESIAN_POINT('Ctrl Pts',(-1.92753067150476,1.,0.455872005174371));
#32376=CARTESIAN_POINT('Ctrl Pts',(-1.93269066517934,-1.,0.459081234547926));
#32377=CARTESIAN_POINT('Ctrl Pts',(-1.93269066517934,1.,0.459081234547926));
#32378=CARTESIAN_POINT('Ctrl Pts',(-1.93781486640821,-1.,0.462340031009056));
#32379=CARTESIAN_POINT('Ctrl Pts',(-1.93781486640821,1.,0.462340031009056));
#32380=CARTESIAN_POINT('Ctrl Pts',(-1.9428979419619,-1.,0.46564546202603));
#32381=CARTESIAN_POINT('Ctrl Pts',(-1.9428979419619,1.,0.46564546202603));
#32382=CARTESIAN_POINT('Ctrl Pts',(-1.94794381136514,-1.,0.468997482913135));
#32383=CARTESIAN_POINT('Ctrl Pts',(-1.94794381136514,1.,0.468997482913135));
#32384=CARTESIAN_POINT('Ctrl Pts',(-1.95296148278133,-1.,0.472397672264072));
#32385=CARTESIAN_POINT('Ctrl Pts',(-1.95296148278133,1.,0.472397672264072));
#32386=CARTESIAN_POINT('Ctrl Pts',(-1.95796111148177,-1.,0.475848034683176));
#32387=CARTESIAN_POINT('Ctrl Pts',(-1.95796111148177,1.,0.475848034683176));
#32388=CARTESIAN_POINT('Ctrl Pts',(-1.96294933055943,-1.,0.479349583074855));
#32389=CARTESIAN_POINT('Ctrl Pts',(-1.96294933055943,1.,0.479349583074855));
#32390=CARTESIAN_POINT('Ctrl Pts',(-1.96792703422362,-1.,0.48290166212069));
#32391=CARTESIAN_POINT('Ctrl Pts',(-1.96792703422362,1.,0.48290166212069));
#32392=CARTESIAN_POINT('Ctrl Pts',(-1.97289186263272,-1.,0.486502692907659));
#32393=CARTESIAN_POINT('Ctrl Pts',(-1.97289186263272,1.,0.486502692907659));
#32394=CARTESIAN_POINT('Ctrl Pts',(-1.97783973019229,-1.,0.490150627860952));
#32395=CARTESIAN_POINT('Ctrl Pts',(-1.97783973019229,1.,0.490150627860952));
#32396=CARTESIAN_POINT('Ctrl Pts',(-1.98276658761821,-1.,0.493843476541494));
#32397=CARTESIAN_POINT('Ctrl Pts',(-1.98276658761821,1.,0.493843476541494));
#32398=CARTESIAN_POINT('Ctrl Pts',(-1.98767044752932,-1.,0.497579909545574));
#32399=CARTESIAN_POINT('Ctrl Pts',(-1.98767044752932,1.,0.497579909545574));
#32400=CARTESIAN_POINT('Ctrl Pts',(-1.99255149126155,-1.,0.501359287727146));
#32401=CARTESIAN_POINT('Ctrl Pts',(-1.99255149126155,1.,0.501359287727146));
#32402=CARTESIAN_POINT('Ctrl Pts',(-1.99741107463572,-1.,0.505181361323026));
#32403=CARTESIAN_POINT('Ctrl Pts',(-1.99741107463572,1.,0.505181361323026));
#32404=CARTESIAN_POINT('Ctrl Pts',(-2.00225107134734,-1.,0.509046069886157));
#32405=CARTESIAN_POINT('Ctrl Pts',(-2.00225107134734,1.,0.509046069886157));
#32406=CARTESIAN_POINT('Ctrl Pts',(-2.00707309946949,-1.,0.512953306961792));
#32407=CARTESIAN_POINT('Ctrl Pts',(-2.00707309946949,1.,0.512953306961792));
#32408=CARTESIAN_POINT('Ctrl Pts',(-2.01187773939242,-1.,0.516902681728687));
#32409=CARTESIAN_POINT('Ctrl Pts',(-2.01187773939242,1.,0.516902681728687));
#32410=CARTESIAN_POINT('Ctrl Pts',(-2.01666477917286,-1.,0.52089359039937));
#32411=CARTESIAN_POINT('Ctrl Pts',(-2.01666477917286,1.,0.52089359039937));
#32412=CARTESIAN_POINT('Ctrl Pts',(-2.02143356304698,-1.,0.524925318333476));
#32413=CARTESIAN_POINT('Ctrl Pts',(-2.02143356304698,1.,0.524925318333476));
#32414=CARTESIAN_POINT('Ctrl Pts',(-2.0261832908329,-1.,0.528997127241914));
#32415=CARTESIAN_POINT('Ctrl Pts',(-2.0261832908329,1.,0.528997127241914));
#32416=CARTESIAN_POINT('Ctrl Pts',(-2.03091336214426,-1.,0.533108355132976));
#32417=CARTESIAN_POINT('Ctrl Pts',(-2.03091336214426,1.,0.533108355132976));
#32418=CARTESIAN_POINT('Ctrl Pts',(-2.03562362954037,-1.,0.537258489833262));
#32419=CARTESIAN_POINT('Ctrl Pts',(-2.03562362954037,1.,0.537258489833262));
#32420=CARTESIAN_POINT('Ctrl Pts',(-2.04031422690527,-1.,0.541447120615659));
#32421=CARTESIAN_POINT('Ctrl Pts',(-2.04031422690527,1.,0.541447120615659));
#32422=CARTESIAN_POINT('Ctrl Pts',(-2.04498544714588,-1.,0.54567390381743));
#32423=CARTESIAN_POINT('Ctrl Pts',(-2.04498544714588,1.,0.54567390381743));
#32424=CARTESIAN_POINT('Ctrl Pts',(-2.04963761077958,-1.,0.549938525150295));
#32425=CARTESIAN_POINT('Ctrl Pts',(-2.04963761077958,1.,0.549938525150295));
#32426=CARTESIAN_POINT('Ctrl Pts',(-2.05427091604413,-1.,0.554240657463906));
#32427=CARTESIAN_POINT('Ctrl Pts',(-2.05427091604413,1.,0.554240657463906));
#32428=CARTESIAN_POINT('Ctrl Pts',(-2.05888537756462,-1.,0.558579940185151));
#32429=CARTESIAN_POINT('Ctrl Pts',(-2.05888537756462,1.,0.558579940185151));
#32430=CARTESIAN_POINT('Ctrl Pts',(-2.06348090160589,-1.,0.562955993082261));
#32431=CARTESIAN_POINT('Ctrl Pts',(-2.06348090160589,1.,0.562955993082261));
#32432=CARTESIAN_POINT('Ctrl Pts',(-2.06805732997334,-1.,0.567368421181087));
#32433=CARTESIAN_POINT('Ctrl Pts',(-2.06805732997334,1.,0.567368421181087));
#32434=CARTESIAN_POINT('Ctrl Pts',(-2.07261449292824,-1.,0.571816823242603));
#32435=CARTESIAN_POINT('Ctrl Pts',(-2.07261449292824,1.,0.571816823242603));
#32436=CARTESIAN_POINT('Ctrl Pts',(-2.07715226767559,-1.,0.576300797416844));
#32437=CARTESIAN_POINT('Ctrl Pts',(-2.07715226767559,1.,0.576300797416844));
#32438=CARTESIAN_POINT('Ctrl Pts',(-2.08167059018418,-1.,0.580819952108063));
#32439=CARTESIAN_POINT('Ctrl Pts',(-2.08167059018418,1.,0.580819952108063));
#32440=CARTESIAN_POINT('Ctrl Pts',(-2.08616943727951,-1.,0.585373918991617));
#32441=CARTESIAN_POINT('Ctrl Pts',(-2.08616943727951,1.,0.585373918991617));
#32442=CARTESIAN_POINT('Ctrl Pts',(-2.09064881812129,-1.,0.589962365403406));
#32443=CARTESIAN_POINT('Ctrl Pts',(-2.09064881812129,1.,0.589962365403406));
#32444=CARTESIAN_POINT('Ctrl Pts',(-2.0951087622027,-1.,0.594585006052162));
#32445=CARTESIAN_POINT('Ctrl Pts',(-2.0951087622027,1.,0.594585006052162));
#32446=CARTESIAN_POINT('Ctrl Pts',(-2.0995493086477,-1.,0.599241616420533));
#32447=CARTESIAN_POINT('Ctrl Pts',(-2.0995493086477,1.,0.599241616420533));
#32448=CARTESIAN_POINT('Ctrl Pts',(-2.10397049886949,-1.,0.60393203073603));
#32449=CARTESIAN_POINT('Ctrl Pts',(-2.10397049886949,1.,0.60393203073603));
#32450=CARTESIAN_POINT('Ctrl Pts',(-2.1074919961518,-1.,0.607711315454876));
#32451=CARTESIAN_POINT('Ctrl Pts',(-2.1074919961518,1.,0.607711315454876));
#32452=CARTESIAN_POINT('Ctrl Pts',(-2.11012443807238,-1.,0.610560911689899));
#32453=CARTESIAN_POINT('Ctrl Pts',(-2.11012443807238,1.,0.610560911689899));
#32454=CARTESIAN_POINT('Ctrl Pts',(-2.11187554259986,-1.,0.6124673655618));
#32455=CARTESIAN_POINT('Ctrl Pts',(-2.11187554259986,1.,0.6124673655618));
#32456=CARTESIAN_POINT('Ctrl Pts',(-2.11275013067528,-1.,0.61342227326009));
#32457=CARTESIAN_POINT('Ctrl Pts',(-2.11275013067528,1.,0.61342227326009));
#32458=CARTESIAN_POINT('',(-1.7075470150345,1.,0.383122945602004));
#32459=CARTESIAN_POINT('Ctrl Pts',(-1.7075470150345,1.,0.383122945602004));
#32460=CARTESIAN_POINT('Ctrl Pts',(-1.71231062891958,1.,0.384119047315542));
#32461=CARTESIAN_POINT('Ctrl Pts',(-1.72162022246158,1.,0.38607079032701));
#32462=CARTESIAN_POINT('Ctrl Pts',(-1.7349317097561,1.,0.388877023509191));
#32463=CARTESIAN_POINT('Ctrl Pts',(-1.75137405313962,1.,0.392375812294307));
#32464=CARTESIAN_POINT('Ctrl Pts',(-1.7697556004756,1.,0.39634619612042));
#32465=CARTESIAN_POINT('Ctrl Pts',(-1.78598826347533,1.,0.39991940378308));
#32466=CARTESIAN_POINT('Ctrl Pts',(-1.80012077176221,1.,0.403107976170441));
#32467=CARTESIAN_POINT('Ctrl Pts',(-1.81223801813988,1.,0.405933518411838));
#32468=CARTESIAN_POINT('Ctrl Pts',(-1.8224702267854,1.,0.408428948108533));
#32469=CARTESIAN_POINT('Ctrl Pts',(-1.83100408895216,1.,0.410641256301675));
#32470=CARTESIAN_POINT('Ctrl Pts',(-1.83808953475839,1.,0.412633125322161));
#32471=CARTESIAN_POINT('Ctrl Pts',(-1.8440575707371,1.,0.41448743825434));
#32472=CARTESIAN_POINT('Ctrl Pts',(-1.84929312929882,1.,0.416300022038864));
#32473=CARTESIAN_POINT('Ctrl Pts',(-1.85417632856234,1.,0.418164129143534));
#32474=CARTESIAN_POINT('Ctrl Pts',(-1.85903281096686,1.,0.420157287975619));
#32475=CARTESIAN_POINT('Ctrl Pts',(-1.86408083334028,1.,0.422327307418275));
#32476=CARTESIAN_POINT('Ctrl Pts',(-1.86937803944323,1.,0.424678177291359));
#32477=CARTESIAN_POINT('Ctrl Pts',(-1.87486989291484,1.,0.427183828519102));
#32478=CARTESIAN_POINT('Ctrl Pts',(-1.88044229001832,1.,0.429803062482344));
#32479=CARTESIAN_POINT('Ctrl Pts',(-1.88596913666793,1.,0.432493038548748));
#32480=CARTESIAN_POINT('Ctrl Pts',(-1.89136993975504,1.,0.435225660963383));
#32481=CARTESIAN_POINT('Ctrl Pts',(-1.89663648956466,1.,0.437995003948244));
#32482=CARTESIAN_POINT('Ctrl Pts',(-1.90180124389086,1.,0.440807833704038));
#32483=CARTESIAN_POINT('Ctrl Pts',(-1.90691756144898,1.,0.44367755684915));
#32484=CARTESIAN_POINT('Ctrl Pts',(-1.9120369998112,1.,0.446617343485711));
#32485=CARTESIAN_POINT('Ctrl Pts',(-1.91718342555755,1.,0.449632260106662));
#32486=CARTESIAN_POINT('Ctrl Pts',(-1.92235380648502,1.,0.452719478359432));
#32487=CARTESIAN_POINT('Ctrl Pts',(-1.92753067150476,1.,0.455872005174371));
#32488=CARTESIAN_POINT('Ctrl Pts',(-1.93269066517934,1.,0.459081234547926));
#32489=CARTESIAN_POINT('Ctrl Pts',(-1.93781486640821,1.,0.462340031009056));
#32490=CARTESIAN_POINT('Ctrl Pts',(-1.9428979419619,1.,0.46564546202603));
#32491=CARTESIAN_POINT('Ctrl Pts',(-1.94794381136514,1.,0.468997482913135));
#32492=CARTESIAN_POINT('Ctrl Pts',(-1.95296148278133,1.,0.472397672264072));
#32493=CARTESIAN_POINT('Ctrl Pts',(-1.95796111148177,1.,0.475848034683176));
#32494=CARTESIAN_POINT('Ctrl Pts',(-1.96294933055943,1.,0.479349583074855));
#32495=CARTESIAN_POINT('Ctrl Pts',(-1.96792703422362,1.,0.48290166212069));
#32496=CARTESIAN_POINT('Ctrl Pts',(-1.97289186263272,1.,0.486502692907659));
#32497=CARTESIAN_POINT('Ctrl Pts',(-1.97783973019229,1.,0.490150627860952));
#32498=CARTESIAN_POINT('Ctrl Pts',(-1.98276658761821,1.,0.493843476541494));
#32499=CARTESIAN_POINT('Ctrl Pts',(-1.98767044752932,1.,0.497579909545574));
#32500=CARTESIAN_POINT('Ctrl Pts',(-1.99255149126155,1.,0.501359287727146));
#32501=CARTESIAN_POINT('Ctrl Pts',(-1.99741107463572,1.,0.505181361323026));
#32502=CARTESIAN_POINT('Ctrl Pts',(-2.00225107134734,1.,0.509046069886157));
#32503=CARTESIAN_POINT('Ctrl Pts',(-2.00707309946949,1.,0.512953306961792));
#32504=CARTESIAN_POINT('Ctrl Pts',(-2.01187773939242,1.,0.516902681728687));
#32505=CARTESIAN_POINT('Ctrl Pts',(-2.01666477917286,1.,0.52089359039937));
#32506=CARTESIAN_POINT('Ctrl Pts',(-2.02143356304698,1.,0.524925318333476));
#32507=CARTESIAN_POINT('Ctrl Pts',(-2.0261832908329,1.,0.528997127241914));
#32508=CARTESIAN_POINT('Ctrl Pts',(-2.03091336214426,1.,0.533108355132976));
#32509=CARTESIAN_POINT('Ctrl Pts',(-2.03562362954037,1.,0.537258489833262));
#32510=CARTESIAN_POINT('Ctrl Pts',(-2.04031422690527,1.,0.541447120615659));
#32511=CARTESIAN_POINT('Ctrl Pts',(-2.04498544714588,1.,0.54567390381743));
#32512=CARTESIAN_POINT('Ctrl Pts',(-2.04963761077958,1.,0.549938525150295));
#32513=CARTESIAN_POINT('Ctrl Pts',(-2.05427091604413,1.,0.554240657463906));
#32514=CARTESIAN_POINT('Ctrl Pts',(-2.05888537756462,1.,0.558579940185151));
#32515=CARTESIAN_POINT('Ctrl Pts',(-2.06348090160589,1.,0.562955993082261));
#32516=CARTESIAN_POINT('Ctrl Pts',(-2.06805732997334,1.,0.567368421181087));
#32517=CARTESIAN_POINT('Ctrl Pts',(-2.07261449292824,1.,0.571816823242603));
#32518=CARTESIAN_POINT('Ctrl Pts',(-2.07715226767559,1.,0.576300797416844));
#32519=CARTESIAN_POINT('Ctrl Pts',(-2.08167059018418,1.,0.580819952108063));
#32520=CARTESIAN_POINT('Ctrl Pts',(-2.08616943727951,1.,0.585373918991617));
#32521=CARTESIAN_POINT('Ctrl Pts',(-2.09064881812129,1.,0.589962365403406));
#32522=CARTESIAN_POINT('Ctrl Pts',(-2.0951087622027,1.,0.594585006052162));
#32523=CARTESIAN_POINT('Ctrl Pts',(-2.0995493086477,1.,0.599241616420533));
#32524=CARTESIAN_POINT('Ctrl Pts',(-2.10397049886949,1.,0.60393203073603));
#32525=CARTESIAN_POINT('Ctrl Pts',(-2.1074919961518,1.,0.607711315454876));
#32526=CARTESIAN_POINT('Ctrl Pts',(-2.11012443807238,1.,0.610560911689899));
#32527=CARTESIAN_POINT('Ctrl Pts',(-2.11187554259986,1.,0.6124673655618));
#32528=CARTESIAN_POINT('Ctrl Pts',(-2.11275013067528,1.,0.61342227326009));
#32529=CARTESIAN_POINT('',(-1.7075470150345,0.,0.383122945602003));
#32530=CARTESIAN_POINT('Origin',(0.,0.,0.));
#32531=CARTESIAN_POINT('',(-1.74236521665491,1.,0.163289472382896));
#32532=CARTESIAN_POINT('Origin',(0.,1.,0.));
#32533=CARTESIAN_POINT('',(-1.74236521665491,0.,0.163289472382896));
#32534=CARTESIAN_POINT('Ctrl Pts',(-2.19890268624765,-1.,0.069476445021958));
#32535=CARTESIAN_POINT('Ctrl Pts',(-2.19890268624765,1.,0.069476445021958));
#32536=CARTESIAN_POINT('Ctrl Pts',(-2.19777582085423,-1.,0.0701143536325489));
#32537=CARTESIAN_POINT('Ctrl Pts',(-2.19777582085423,1.,0.0701143536325489));
#32538=CARTESIAN_POINT('Ctrl Pts',(-2.19552129484002,-1.,0.0713863779526153));
#32539=CARTESIAN_POINT('Ctrl Pts',(-2.19552129484002,1.,0.0713863779526153));
#32540=CARTESIAN_POINT('Ctrl Pts',(-2.19213712013662,-1.,0.0732830357306724));
#32541=CARTESIAN_POINT('Ctrl Pts',(-2.19213712013662,1.,0.0732830357306724));
#32542=CARTESIAN_POINT('Ctrl Pts',(-2.1876201139953,-1.,0.0757891465836146));
#32543=CARTESIAN_POINT('Ctrl Pts',(-2.1876201139953,1.,0.0757891465836146));
#32544=CARTESIAN_POINT('Ctrl Pts',(-2.18196589448887,-1.,0.0788837727685241));
#32545=CARTESIAN_POINT('Ctrl Pts',(-2.18196589448887,1.,0.0788837727685241));
#32546=CARTESIAN_POINT('Ctrl Pts',(-2.176303712113,-1.,0.0819402680872764));
#32547=CARTESIAN_POINT('Ctrl Pts',(-2.176303712113,1.,0.0819402680872764));
#32548=CARTESIAN_POINT('Ctrl Pts',(-2.17063357870952,-1.,0.0849584620835371));
#32549=CARTESIAN_POINT('Ctrl Pts',(-2.17063357870952,1.,0.0849584620835371));
#32550=CARTESIAN_POINT('Ctrl Pts',(-2.16495552645014,-1.,0.0879381291386921));
#32551=CARTESIAN_POINT('Ctrl Pts',(-2.16495552645014,1.,0.0879381291386921));
#32552=CARTESIAN_POINT('Ctrl Pts',(-2.15926961544516,-1.,0.0908789888107264));
#32553=CARTESIAN_POINT('Ctrl Pts',(-2.15926961544516,1.,0.0908789888107264));
#32554=CARTESIAN_POINT('Ctrl Pts',(-2.1535759397817,-1.,0.0937807218867642));
#32555=CARTESIAN_POINT('Ctrl Pts',(-2.1535759397817,1.,0.0937807218867642));
#32556=CARTESIAN_POINT('Ctrl Pts',(-2.14787463531795,-1.,0.0966429852305457));
#32557=CARTESIAN_POINT('Ctrl Pts',(-2.14787463531795,1.,0.0966429852305457));
#32558=CARTESIAN_POINT('Ctrl Pts',(-2.14216588396025,-1.,0.0994654261990914));
#32559=CARTESIAN_POINT('Ctrl Pts',(-2.14216588396025,1.,0.0994654261990914));
#32560=CARTESIAN_POINT('Ctrl Pts',(-2.13644992667165,-1.,0.1022477005561));
#32561=CARTESIAN_POINT('Ctrl Pts',(-2.13644992667165,1.,0.1022477005561));
#32562=CARTESIAN_POINT('Ctrl Pts',(-2.13072704887293,-1.,0.104989479152739));
#32563=CARTESIAN_POINT('Ctrl Pts',(-2.13072704887293,1.,0.104989479152739));
#32564=CARTESIAN_POINT('Ctrl Pts',(-2.12499752307,-1.,0.10769043523109));
#32565=CARTESIAN_POINT('Ctrl Pts',(-2.12499752307,1.,0.10769043523109));
#32566=CARTESIAN_POINT('Ctrl Pts',(-2.11926155590865,-1.,0.110350236135025));
#32567=CARTESIAN_POINT('Ctrl Pts',(-2.11926155590865,1.,0.110350236135025));
#32568=CARTESIAN_POINT('Ctrl Pts',(-2.11351924490306,-1.,0.112968534419737));
#32569=CARTESIAN_POINT('Ctrl Pts',(-2.11351924490306,1.,0.112968534419737));
#32570=CARTESIAN_POINT('Ctrl Pts',(-2.10777050261309,-1.,0.115544957687926));
#32571=CARTESIAN_POINT('Ctrl Pts',(-2.10777050261309,1.,0.115544957687926));
#32572=CARTESIAN_POINT('Ctrl Pts',(-2.102015121329,-1.,0.118079107988355));
#32573=CARTESIAN_POINT('Ctrl Pts',(-2.102015121329,1.,0.118079107988355));
#32574=CARTESIAN_POINT('Ctrl Pts',(-2.0962529286773,-1.,0.120570567965122));
#32575=CARTESIAN_POINT('Ctrl Pts',(-2.0962529286773,1.,0.120570567965122));
#32576=CARTESIAN_POINT('Ctrl Pts',(-2.09048392424825,-1.,0.123018905621083));
#32577=CARTESIAN_POINT('Ctrl Pts',(-2.09048392424825,1.,0.123018905621083));
#32578=CARTESIAN_POINT('Ctrl Pts',(-2.08470840653643,-1.,0.125423679412061));
#32579=CARTESIAN_POINT('Ctrl Pts',(-2.08470840653643,1.,0.125423679412061));
#32580=CARTESIAN_POINT('Ctrl Pts',(-2.07892715110987,-1.,0.12778444527612));
#32581=CARTESIAN_POINT('Ctrl Pts',(-2.07892715110987,1.,0.12778444527612));
#32582=CARTESIAN_POINT('Ctrl Pts',(-2.07314114713063,-1.,0.130100748328403));
#32583=CARTESIAN_POINT('Ctrl Pts',(-2.07314114713063,1.,0.130100748328403));
#32584=CARTESIAN_POINT('Ctrl Pts',(-2.06735123910326,-1.,0.13237211154771));
#32585=CARTESIAN_POINT('Ctrl Pts',(-2.06735123910326,1.,0.13237211154771));
#32586=CARTESIAN_POINT('Ctrl Pts',(-2.06155781517842,-1.,0.134598026192106));
#32587=CARTESIAN_POINT('Ctrl Pts',(-2.06155781517842,1.,0.134598026192106));
#32588=CARTESIAN_POINT('Ctrl Pts',(-2.05576044414264,-1.,0.136777941218043));
#32589=CARTESIAN_POINT('Ctrl Pts',(-2.05576044414264,1.,0.136777941218043));
#32590=CARTESIAN_POINT('Ctrl Pts',(-2.04995762001328,-1.,0.138911255368966));
#32591=CARTESIAN_POINT('Ctrl Pts',(-2.04995762001328,1.,0.138911255368966));
#32592=CARTESIAN_POINT('Ctrl Pts',(-2.04414757947916,-1.,0.140997332152546));
#32593=CARTESIAN_POINT('Ctrl Pts',(-2.04414757947916,1.,0.140997332152546));
#32594=CARTESIAN_POINT('Ctrl Pts',(-2.03832911025912,-1.,0.143035515058209));
#32595=CARTESIAN_POINT('Ctrl Pts',(-2.03832911025912,1.,0.143035515058209));
#32596=CARTESIAN_POINT('Ctrl Pts',(-2.03250223739942,-1.,0.145025140186057));
#32597=CARTESIAN_POINT('Ctrl Pts',(-2.03250223739942,1.,0.145025140186057));
#32598=CARTESIAN_POINT('Ctrl Pts',(-2.02666926182017,-1.,0.146965557332583));
#32599=CARTESIAN_POINT('Ctrl Pts',(-2.02666926182017,1.,0.146965557332583));
#32600=CARTESIAN_POINT('Ctrl Pts',(-2.02083464969894,-1.,0.148856124775337));
#32601=CARTESIAN_POINT('Ctrl Pts',(-2.02083464969894,1.,0.148856124775337));
#32602=CARTESIAN_POINT('Ctrl Pts',(-2.01500291940238,-1.,0.150696157673078));
#32603=CARTESIAN_POINT('Ctrl Pts',(-2.01500291940238,1.,0.150696157673078));
#32604=CARTESIAN_POINT('Ctrl Pts',(-2.00917680318424,-1.,0.15248488362145));
#32605=CARTESIAN_POINT('Ctrl Pts',(-2.00917680318424,1.,0.15248488362145));
#32606=CARTESIAN_POINT('Ctrl Pts',(-2.00335565310543,-1.,0.154221403049722));
#32607=CARTESIAN_POINT('Ctrl Pts',(-2.00335565310543,1.,0.154221403049722));
#32608=CARTESIAN_POINT('Ctrl Pts',(-1.99753284771497,-1.,0.155904629548783));
#32609=CARTESIAN_POINT('Ctrl Pts',(-1.99753284771497,1.,0.155904629548783));
#32610=CARTESIAN_POINT('Ctrl Pts',(-1.99169810931908,-1.,0.157533331459227));
#32611=CARTESIAN_POINT('Ctrl Pts',(-1.99169810931908,1.,0.157533331459227));
#32612=CARTESIAN_POINT('Ctrl Pts',(-1.98584238283292,-1.,0.159106226437299));
#32613=CARTESIAN_POINT('Ctrl Pts',(-1.98584238283292,1.,0.159106226437299));
#32614=CARTESIAN_POINT('Ctrl Pts',(-1.97996195437559,-1.,0.160622060784611));
#32615=CARTESIAN_POINT('Ctrl Pts',(-1.97996195437559,1.,0.160622060784611));
#32616=CARTESIAN_POINT('Ctrl Pts',(-1.97406280235188,-1.,0.162079693556288));
#32617=CARTESIAN_POINT('Ctrl Pts',(-1.97406280235188,1.,0.162079693556288));
#32618=CARTESIAN_POINT('Ctrl Pts',(-1.96816512677967,-1.,0.163478185457734));
#32619=CARTESIAN_POINT('Ctrl Pts',(-1.96816512677967,1.,0.163478185457734));
#32620=CARTESIAN_POINT('Ctrl Pts',(-1.96229379940136,-1.,0.164816568920269));
#32621=CARTESIAN_POINT('Ctrl Pts',(-1.96229379940136,1.,0.164816568920269));
#32622=CARTESIAN_POINT('Ctrl Pts',(-1.9564675971873,-1.,0.166093592002812));
#32623=CARTESIAN_POINT('Ctrl Pts',(-1.9564675971873,1.,0.166093592002812));
#32624=CARTESIAN_POINT('Ctrl Pts',(-1.95069027794294,-1.,0.167307501784475));
#32625=CARTESIAN_POINT('Ctrl Pts',(-1.95069027794294,1.,0.167307501784475));
#32626=CARTESIAN_POINT('Ctrl Pts',(-1.94493757756931,-1.,0.168455741607556));
#32627=CARTESIAN_POINT('Ctrl Pts',(-1.94493757756931,1.,0.168455741607556));
#32628=CARTESIAN_POINT('Ctrl Pts',(-1.93915639211581,-1.,0.169534904817491));
#32629=CARTESIAN_POINT('Ctrl Pts',(-1.93915639211581,1.,0.169534904817491));
#32630=CARTESIAN_POINT('Ctrl Pts',(-1.93329183155539,-1.,0.170541253116201));
#32631=CARTESIAN_POINT('Ctrl Pts',(-1.93329183155539,1.,0.170541253116201));
#32632=CARTESIAN_POINT('Ctrl Pts',(-1.92731093582036,-1.,0.171471191532988));
#32633=CARTESIAN_POINT('Ctrl Pts',(-1.92731093582036,1.,0.171471191532988));
#32634=CARTESIAN_POINT('Ctrl Pts',(-1.9212233439798,-1.,0.172321621259514));
#32635=CARTESIAN_POINT('Ctrl Pts',(-1.9212233439798,1.,0.172321621259514));
#32636=CARTESIAN_POINT('Ctrl Pts',(-1.91511429159527,-1.,0.173090695383496));
#32637=CARTESIAN_POINT('Ctrl Pts',(-1.91511429159527,1.,0.173090695383496));
#32638=CARTESIAN_POINT('Ctrl Pts',(-1.90911693975267,-1.,0.173776635257817));
#32639=CARTESIAN_POINT('Ctrl Pts',(-1.90911693975267,1.,0.173776635257817));
#32640=CARTESIAN_POINT('Ctrl Pts',(-1.90335253862834,-1.,0.174375518661085));
#32641=CARTESIAN_POINT('Ctrl Pts',(-1.90335253862834,1.,0.174375518661085));
#32642=CARTESIAN_POINT('Ctrl Pts',(-1.89788101117132,-1.,0.174879405091263));
#32643=CARTESIAN_POINT('Ctrl Pts',(-1.89788101117132,1.,0.174879405091263));
#32644=CARTESIAN_POINT('Ctrl Pts',(-1.892646301985,-1.,0.175274276190844));
#32645=CARTESIAN_POINT('Ctrl Pts',(-1.892646301985,1.,0.175274276190844));
#32646=CARTESIAN_POINT('Ctrl Pts',(-1.88742606273259,-1.,0.175538155840648));
#32647=CARTESIAN_POINT('Ctrl Pts',(-1.88742606273259,1.,0.175538155840648));
#32648=CARTESIAN_POINT('Ctrl Pts',(-1.88188663145367,-1.,0.175644148889698));
#32649=CARTESIAN_POINT('Ctrl Pts',(-1.88188663145367,1.,0.175644148889698));
#32650=CARTESIAN_POINT('Ctrl Pts',(-1.87563767773588,-1.,0.175563480746485));
#32651=CARTESIAN_POINT('Ctrl Pts',(-1.87563767773588,1.,0.175563480746485));
#32652=CARTESIAN_POINT('Ctrl Pts',(-1.86828349694799,-1.,0.175268337590758));
#32653=CARTESIAN_POINT('Ctrl Pts',(-1.86828349694799,1.,0.175268337590758));
#32654=CARTESIAN_POINT('Ctrl Pts',(-1.85948367088837,-1.,0.17473525927603));
#32655=CARTESIAN_POINT('Ctrl Pts',(-1.85948367088837,1.,0.17473525927603));
#32656=CARTESIAN_POINT('Ctrl Pts',(-1.8489811319852,-1.,0.173946627587731));
#32657=CARTESIAN_POINT('Ctrl Pts',(-1.8489811319852,1.,0.173946627587731));
#32658=CARTESIAN_POINT('Ctrl Pts',(-1.83658380527692,-1.,0.1728894428919));
#32659=CARTESIAN_POINT('Ctrl Pts',(-1.83658380527692,1.,0.1728894428919));
#32660=CARTESIAN_POINT('Ctrl Pts',(-1.82215766811545,-1.,0.171554770204119));
#32661=CARTESIAN_POINT('Ctrl Pts',(-1.82215766811545,1.,0.171554770204119));
#32662=CARTESIAN_POINT('Ctrl Pts',(-1.80561530629706,-1.,0.169936923904608));
#32663=CARTESIAN_POINT('Ctrl Pts',(-1.80561530629706,1.,0.169936923904608));
#32664=CARTESIAN_POINT('Ctrl Pts',(-1.7869064998507,-1.,0.168032772805197));
#32665=CARTESIAN_POINT('Ctrl Pts',(-1.7869064998507,1.,0.168032772805197));
#32666=CARTESIAN_POINT('Ctrl Pts',(-1.77018771684844,-1.,0.1662793551464));
#32667=CARTESIAN_POINT('Ctrl Pts',(-1.77018771684844,1.,0.1662793551464));
#32668=CARTESIAN_POINT('Ctrl Pts',(-1.75666056638427,-1.,0.164834765707158));
#32669=CARTESIAN_POINT('Ctrl Pts',(-1.75666056638427,1.,0.164834765707158));
#32670=CARTESIAN_POINT('Ctrl Pts',(-1.7472034950333,-1.,0.163814161002002));
#32671=CARTESIAN_POINT('Ctrl Pts',(-1.7472034950333,1.,0.163814161002002));
#32672=CARTESIAN_POINT('Ctrl Pts',(-1.74236521665491,-1.,0.163289472382896));
#32673=CARTESIAN_POINT('Ctrl Pts',(-1.74236521665491,1.,0.163289472382896));
#32674=CARTESIAN_POINT('',(-2.19890268624765,1.,0.069476445021958));
#32675=CARTESIAN_POINT('Ctrl Pts',(-2.19890268624765,1.,0.069476445021958));
#32676=CARTESIAN_POINT('Ctrl Pts',(-2.19777582085423,1.,0.0701143536325489));
#32677=CARTESIAN_POINT('Ctrl Pts',(-2.19552129484002,1.,0.0713863779526153));
#32678=CARTESIAN_POINT('Ctrl Pts',(-2.19213712013662,1.,0.0732830357306724));
#32679=CARTESIAN_POINT('Ctrl Pts',(-2.1876201139953,1.,0.0757891465836146));
#32680=CARTESIAN_POINT('Ctrl Pts',(-2.18196589448887,1.,0.0788837727685241));
#32681=CARTESIAN_POINT('Ctrl Pts',(-2.176303712113,1.,0.0819402680872764));
#32682=CARTESIAN_POINT('Ctrl Pts',(-2.17063357870952,1.,0.0849584620835371));
#32683=CARTESIAN_POINT('Ctrl Pts',(-2.16495552645014,1.,0.0879381291386921));
#32684=CARTESIAN_POINT('Ctrl Pts',(-2.15926961544516,1.,0.0908789888107264));
#32685=CARTESIAN_POINT('Ctrl Pts',(-2.1535759397817,1.,0.0937807218867642));
#32686=CARTESIAN_POINT('Ctrl Pts',(-2.14787463531795,1.,0.0966429852305457));
#32687=CARTESIAN_POINT('Ctrl Pts',(-2.14216588396025,1.,0.0994654261990914));
#32688=CARTESIAN_POINT('Ctrl Pts',(-2.13644992667165,1.,0.1022477005561));
#32689=CARTESIAN_POINT('Ctrl Pts',(-2.13072704887293,1.,0.104989479152739));
#32690=CARTESIAN_POINT('Ctrl Pts',(-2.12499752307,1.,0.10769043523109));
#32691=CARTESIAN_POINT('Ctrl Pts',(-2.11926155590865,1.,0.110350236135025));
#32692=CARTESIAN_POINT('Ctrl Pts',(-2.11351924490306,1.,0.112968534419737));
#32693=CARTESIAN_POINT('Ctrl Pts',(-2.10777050261309,1.,0.115544957687926));
#32694=CARTESIAN_POINT('Ctrl Pts',(-2.102015121329,1.,0.118079107988355));
#32695=CARTESIAN_POINT('Ctrl Pts',(-2.0962529286773,1.,0.120570567965122));
#32696=CARTESIAN_POINT('Ctrl Pts',(-2.09048392424825,1.,0.123018905621083));
#32697=CARTESIAN_POINT('Ctrl Pts',(-2.08470840653643,1.,0.125423679412061));
#32698=CARTESIAN_POINT('Ctrl Pts',(-2.07892715110987,1.,0.12778444527612));
#32699=CARTESIAN_POINT('Ctrl Pts',(-2.07314114713063,1.,0.130100748328403));
#32700=CARTESIAN_POINT('Ctrl Pts',(-2.06735123910326,1.,0.13237211154771));
#32701=CARTESIAN_POINT('Ctrl Pts',(-2.06155781517842,1.,0.134598026192106));
#32702=CARTESIAN_POINT('Ctrl Pts',(-2.05576044414264,1.,0.136777941218043));
#32703=CARTESIAN_POINT('Ctrl Pts',(-2.04995762001328,1.,0.138911255368966));
#32704=CARTESIAN_POINT('Ctrl Pts',(-2.04414757947916,1.,0.140997332152546));
#32705=CARTESIAN_POINT('Ctrl Pts',(-2.03832911025912,1.,0.143035515058209));
#32706=CARTESIAN_POINT('Ctrl Pts',(-2.03250223739942,1.,0.145025140186057));
#32707=CARTESIAN_POINT('Ctrl Pts',(-2.02666926182017,1.,0.146965557332583));
#32708=CARTESIAN_POINT('Ctrl Pts',(-2.02083464969894,1.,0.148856124775337));
#32709=CARTESIAN_POINT('Ctrl Pts',(-2.01500291940238,1.,0.150696157673078));
#32710=CARTESIAN_POINT('Ctrl Pts',(-2.00917680318424,1.,0.15248488362145));
#32711=CARTESIAN_POINT('Ctrl Pts',(-2.00335565310543,1.,0.154221403049722));
#32712=CARTESIAN_POINT('Ctrl Pts',(-1.99753284771497,1.,0.155904629548783));
#32713=CARTESIAN_POINT('Ctrl Pts',(-1.99169810931908,1.,0.157533331459227));
#32714=CARTESIAN_POINT('Ctrl Pts',(-1.98584238283292,1.,0.159106226437299));
#32715=CARTESIAN_POINT('Ctrl Pts',(-1.97996195437559,1.,0.160622060784611));
#32716=CARTESIAN_POINT('Ctrl Pts',(-1.97406280235188,1.,0.162079693556288));
#32717=CARTESIAN_POINT('Ctrl Pts',(-1.96816512677967,1.,0.163478185457734));
#32718=CARTESIAN_POINT('Ctrl Pts',(-1.96229379940136,1.,0.164816568920269));
#32719=CARTESIAN_POINT('Ctrl Pts',(-1.9564675971873,1.,0.166093592002812));
#32720=CARTESIAN_POINT('Ctrl Pts',(-1.95069027794294,1.,0.167307501784475));
#32721=CARTESIAN_POINT('Ctrl Pts',(-1.94493757756931,1.,0.168455741607556));
#32722=CARTESIAN_POINT('Ctrl Pts',(-1.93915639211581,1.,0.169534904817491));
#32723=CARTESIAN_POINT('Ctrl Pts',(-1.93329183155539,1.,0.170541253116201));
#32724=CARTESIAN_POINT('Ctrl Pts',(-1.92731093582036,1.,0.171471191532988));
#32725=CARTESIAN_POINT('Ctrl Pts',(-1.9212233439798,1.,0.172321621259514));
#32726=CARTESIAN_POINT('Ctrl Pts',(-1.91511429159527,1.,0.173090695383496));
#32727=CARTESIAN_POINT('Ctrl Pts',(-1.90911693975267,1.,0.173776635257817));
#32728=CARTESIAN_POINT('Ctrl Pts',(-1.90335253862834,1.,0.174375518661085));
#32729=CARTESIAN_POINT('Ctrl Pts',(-1.89788101117132,1.,0.174879405091263));
#32730=CARTESIAN_POINT('Ctrl Pts',(-1.892646301985,1.,0.175274276190844));
#32731=CARTESIAN_POINT('Ctrl Pts',(-1.88742606273259,1.,0.175538155840648));
#32732=CARTESIAN_POINT('Ctrl Pts',(-1.88188663145367,1.,0.175644148889698));
#32733=CARTESIAN_POINT('Ctrl Pts',(-1.87563767773588,1.,0.175563480746485));
#32734=CARTESIAN_POINT('Ctrl Pts',(-1.86828349694799,1.,0.175268337590758));
#32735=CARTESIAN_POINT('Ctrl Pts',(-1.85948367088837,1.,0.17473525927603));
#32736=CARTESIAN_POINT('Ctrl Pts',(-1.8489811319852,1.,0.173946627587731));
#32737=CARTESIAN_POINT('Ctrl Pts',(-1.83658380527692,1.,0.1728894428919));
#32738=CARTESIAN_POINT('Ctrl Pts',(-1.82215766811545,1.,0.171554770204119));
#32739=CARTESIAN_POINT('Ctrl Pts',(-1.80561530629706,1.,0.169936923904608));
#32740=CARTESIAN_POINT('Ctrl Pts',(-1.7869064998507,1.,0.168032772805197));
#32741=CARTESIAN_POINT('Ctrl Pts',(-1.77018771684844,1.,0.1662793551464));
#32742=CARTESIAN_POINT('Ctrl Pts',(-1.75666056638427,1.,0.164834765707158));
#32743=CARTESIAN_POINT('Ctrl Pts',(-1.7472034950333,1.,0.163814161002002));
#32744=CARTESIAN_POINT('Ctrl Pts',(-1.74236521665491,1.,0.163289472382896));
#32745=CARTESIAN_POINT('',(-2.19890268624765,0.,0.069476445021958));
#32746=CARTESIAN_POINT('Origin',(-2.19890268624765,0.,-0.0694764450219585));
#32747=CARTESIAN_POINT('',(-2.19890268624765,1.,-0.0694764450219585));
#32748=CARTESIAN_POINT('',(-2.19890268624765,1.,0.069476445021958));
#32749=CARTESIAN_POINT('',(-2.19890268624765,0.,-0.0694764450219585));
#32750=CARTESIAN_POINT('Ctrl Pts',(-1.74236521665491,-1.,-0.163289472382896));
#32751=CARTESIAN_POINT('Ctrl Pts',(-1.74236521665491,1.,-0.163289472382896));
#32752=CARTESIAN_POINT('Ctrl Pts',(-1.74720349503904,-1.,-0.163814161002474));
#32753=CARTESIAN_POINT('Ctrl Pts',(-1.74720349503904,1.,-0.163814161002474));
#32754=CARTESIAN_POINT('Ctrl Pts',(-1.75666056640041,-1.,-0.164834765708484));
#32755=CARTESIAN_POINT('Ctrl Pts',(-1.75666056640041,1.,-0.164834765708484));
#32756=CARTESIAN_POINT('Ctrl Pts',(-1.77018771687692,-1.,-0.166279355148738));
#32757=CARTESIAN_POINT('Ctrl Pts',(-1.77018771687692,1.,-0.166279355148738));
#32758=CARTESIAN_POINT('Ctrl Pts',(-1.78690649988931,-1.,-0.16803277280837));
#32759=CARTESIAN_POINT('Ctrl Pts',(-1.78690649988931,1.,-0.16803277280837));
#32760=CARTESIAN_POINT('Ctrl Pts',(-1.80561530633924,-1.,-0.169936923908078));
#32761=CARTESIAN_POINT('Ctrl Pts',(-1.80561530633924,1.,-0.169936923908078));
#32762=CARTESIAN_POINT('Ctrl Pts',(-1.82215766815414,-1.,-0.171554770207306));
#32763=CARTESIAN_POINT('Ctrl Pts',(-1.82215766815414,1.,-0.171554770207306));
#32764=CARTESIAN_POINT('Ctrl Pts',(-1.83658380530747,-1.,-0.17288944289442));
#32765=CARTESIAN_POINT('Ctrl Pts',(-1.83658380530747,1.,-0.17288944289442));
#32766=CARTESIAN_POINT('Ctrl Pts',(-1.84898113200543,-1.,-0.173946627589401));
#32767=CARTESIAN_POINT('Ctrl Pts',(-1.84898113200543,1.,-0.173946627589401));
#32768=CARTESIAN_POINT('Ctrl Pts',(-1.85948367089838,-1.,-0.174735259276856));
#32769=CARTESIAN_POINT('Ctrl Pts',(-1.85948367089838,1.,-0.174735259276856));
#32770=CARTESIAN_POINT('Ctrl Pts',(-1.86828349694972,-1.,-0.175268337590901));
#32771=CARTESIAN_POINT('Ctrl Pts',(-1.86828349694972,1.,-0.175268337590901));
#32772=CARTESIAN_POINT('Ctrl Pts',(-1.87563767773249,-1.,-0.175563480746205));
#32773=CARTESIAN_POINT('Ctrl Pts',(-1.87563767773249,1.,-0.175563480746205));
#32774=CARTESIAN_POINT('Ctrl Pts',(-1.88188663144846,-1.,-0.175644148889271));
#32775=CARTESIAN_POINT('Ctrl Pts',(-1.88188663144846,1.,-0.175644148889271));
#32776=CARTESIAN_POINT('Ctrl Pts',(-1.88742606272818,-1.,-0.175538155840286));
#32777=CARTESIAN_POINT('Ctrl Pts',(-1.88742606272818,1.,-0.175538155840286));
#32778=CARTESIAN_POINT('Ctrl Pts',(-1.89264630198279,-1.,-0.175274276190664));
#32779=CARTESIAN_POINT('Ctrl Pts',(-1.89264630198279,1.,-0.175274276190664));
#32780=CARTESIAN_POINT('Ctrl Pts',(-1.89788101117148,-1.,-0.174879405091277));
#32781=CARTESIAN_POINT('Ctrl Pts',(-1.89788101117148,1.,-0.174879405091277));
#32782=CARTESIAN_POINT('Ctrl Pts',(-1.90335253863003,-1.,-0.174375518661222));
#32783=CARTESIAN_POINT('Ctrl Pts',(-1.90335253863003,1.,-0.174375518661222));
#32784=CARTESIAN_POINT('Ctrl Pts',(-1.90911693975475,-1.,-0.173776635257984));
#32785=CARTESIAN_POINT('Ctrl Pts',(-1.90911693975475,1.,-0.173776635257984));
#32786=CARTESIAN_POINT('Ctrl Pts',(-1.91511429159681,-1.,-0.173090695383619));
#32787=CARTESIAN_POINT('Ctrl Pts',(-1.91511429159681,1.,-0.173090695383619));
#32788=CARTESIAN_POINT('Ctrl Pts',(-1.92122334398034,-1.,-0.172321621259557));
#32789=CARTESIAN_POINT('Ctrl Pts',(-1.92122334398034,1.,-0.172321621259557));
#32790=CARTESIAN_POINT('Ctrl Pts',(-1.92731093582,-1.,-0.17147119153296));
#32791=CARTESIAN_POINT('Ctrl Pts',(-1.92731093582,1.,-0.17147119153296));
#32792=CARTESIAN_POINT('Ctrl Pts',(-1.93329183155455,-1.,-0.170541253116136));
#32793=CARTESIAN_POINT('Ctrl Pts',(-1.93329183155455,1.,-0.170541253116136));
#32794=CARTESIAN_POINT('Ctrl Pts',(-1.93915639211497,-1.,-0.169534904817425));
#32795=CARTESIAN_POINT('Ctrl Pts',(-1.93915639211497,1.,-0.169534904817425));
#32796=CARTESIAN_POINT('Ctrl Pts',(-1.94493757756879,-1.,-0.168455741607516));
#32797=CARTESIAN_POINT('Ctrl Pts',(-1.94493757756879,1.,-0.168455741607516));
#32798=CARTESIAN_POINT('Ctrl Pts',(-1.95069027794286,-1.,-0.167307501784469));
#32799=CARTESIAN_POINT('Ctrl Pts',(-1.95069027794286,1.,-0.167307501784469));
#32800=CARTESIAN_POINT('Ctrl Pts',(-1.95646759718755,-1.,-0.166093592002833));
#32801=CARTESIAN_POINT('Ctrl Pts',(-1.95646759718755,1.,-0.166093592002833));
#32802=CARTESIAN_POINT('Ctrl Pts',(-1.96229379940174,-1.,-0.1648165689203));
#32803=CARTESIAN_POINT('Ctrl Pts',(-1.96229379940174,1.,-0.1648165689203));
#32804=CARTESIAN_POINT('Ctrl Pts',(-1.96816512678,-1.,-0.16347818545776));
#32805=CARTESIAN_POINT('Ctrl Pts',(-1.96816512678,1.,-0.16347818545776));
#32806=CARTESIAN_POINT('Ctrl Pts',(-1.97406280235204,-1.,-0.162079693556302));
#32807=CARTESIAN_POINT('Ctrl Pts',(-1.97406280235204,1.,-0.162079693556302));
#32808=CARTESIAN_POINT('Ctrl Pts',(-1.97996195437557,-1.,-0.16062206078461));
#32809=CARTESIAN_POINT('Ctrl Pts',(-1.97996195437557,1.,-0.16062206078461));
#32810=CARTESIAN_POINT('Ctrl Pts',(-1.98584238283279,-1.,-0.159106226437289));
#32811=CARTESIAN_POINT('Ctrl Pts',(-1.98584238283279,1.,-0.159106226437289));
#32812=CARTESIAN_POINT('Ctrl Pts',(-1.99169810931893,-1.,-0.157533331459215));
#32813=CARTESIAN_POINT('Ctrl Pts',(-1.99169810931893,1.,-0.157533331459215));
#32814=CARTESIAN_POINT('Ctrl Pts',(-1.99753284771487,-1.,-0.155904629548775));
#32815=CARTESIAN_POINT('Ctrl Pts',(-1.99753284771487,1.,-0.155904629548775));
#32816=CARTESIAN_POINT('Ctrl Pts',(-2.00335565310539,-1.,-0.154221403049719));
#32817=CARTESIAN_POINT('Ctrl Pts',(-2.00335565310539,1.,-0.154221403049719));
#32818=CARTESIAN_POINT('Ctrl Pts',(-2.00917680318426,-1.,-0.152484883621452));
#32819=CARTESIAN_POINT('Ctrl Pts',(-2.00917680318426,1.,-0.152484883621452));
#32820=CARTESIAN_POINT('Ctrl Pts',(-2.01500291940243,-1.,-0.150696157673084));
#32821=CARTESIAN_POINT('Ctrl Pts',(-2.01500291940243,1.,-0.150696157673084));
#32822=CARTESIAN_POINT('Ctrl Pts',(-2.02083464969897,-1.,-0.148856124775343));
#32823=CARTESIAN_POINT('Ctrl Pts',(-2.02083464969897,1.,-0.148856124775343));
#32824=CARTESIAN_POINT('Ctrl Pts',(-2.02666926182017,-1.,-0.146965557332586));
#32825=CARTESIAN_POINT('Ctrl Pts',(-2.02666926182017,1.,-0.146965557332586));
#32826=CARTESIAN_POINT('Ctrl Pts',(-2.03250223739941,-1.,-0.145025140186058));
#32827=CARTESIAN_POINT('Ctrl Pts',(-2.03250223739941,1.,-0.145025140186058));
#32828=CARTESIAN_POINT('Ctrl Pts',(-2.03832911025913,-1.,-0.143035515058208));
#32829=CARTESIAN_POINT('Ctrl Pts',(-2.03832911025913,1.,-0.143035515058208));
#32830=CARTESIAN_POINT('Ctrl Pts',(-2.04414757947919,-1.,-0.140997332152545));
#32831=CARTESIAN_POINT('Ctrl Pts',(-2.04414757947919,1.,-0.140997332152545));
#32832=CARTESIAN_POINT('Ctrl Pts',(-2.04995762001333,-1.,-0.138911255368966));
#32833=CARTESIAN_POINT('Ctrl Pts',(-2.04995762001333,1.,-0.138911255368966));
#32834=CARTESIAN_POINT('Ctrl Pts',(-2.0557604441427,-1.,-0.136777941218044));
#32835=CARTESIAN_POINT('Ctrl Pts',(-2.0557604441427,1.,-0.136777941218044));
#32836=CARTESIAN_POINT('Ctrl Pts',(-2.06155781517844,-1.,-0.134598026192107));
#32837=CARTESIAN_POINT('Ctrl Pts',(-2.06155781517844,1.,-0.134598026192107));
#32838=CARTESIAN_POINT('Ctrl Pts',(-2.06735123910319,-1.,-0.13237211154771));
#32839=CARTESIAN_POINT('Ctrl Pts',(-2.06735123910319,1.,-0.13237211154771));
#32840=CARTESIAN_POINT('Ctrl Pts',(-2.07314114713047,-1.,-0.130100748328401));
#32841=CARTESIAN_POINT('Ctrl Pts',(-2.07314114713047,1.,-0.130100748328401));
#32842=CARTESIAN_POINT('Ctrl Pts',(-2.07892715110967,-1.,-0.127784445276116));
#32843=CARTESIAN_POINT('Ctrl Pts',(-2.07892715110967,1.,-0.127784445276116));
#32844=CARTESIAN_POINT('Ctrl Pts',(-2.08470840653628,-1.,-0.125423679412058));
#32845=CARTESIAN_POINT('Ctrl Pts',(-2.08470840653628,1.,-0.125423679412058));
#32846=CARTESIAN_POINT('Ctrl Pts',(-2.09048392424826,-1.,-0.123018905621083));
#32847=CARTESIAN_POINT('Ctrl Pts',(-2.09048392424826,1.,-0.123018905621083));
#32848=CARTESIAN_POINT('Ctrl Pts',(-2.09625292867756,-1.,-0.120570567965129));
#32849=CARTESIAN_POINT('Ctrl Pts',(-2.09625292867756,1.,-0.120570567965129));
#32850=CARTESIAN_POINT('Ctrl Pts',(-2.10201512132945,-1.,-0.118079107988368));
#32851=CARTESIAN_POINT('Ctrl Pts',(-2.10201512132945,1.,-0.118079107988368));
#32852=CARTESIAN_POINT('Ctrl Pts',(-2.10777050261359,-1.,-0.11554495768794));
#32853=CARTESIAN_POINT('Ctrl Pts',(-2.10777050261359,1.,-0.11554495768794));
#32854=CARTESIAN_POINT('Ctrl Pts',(-2.11351924490335,-1.,-0.112968534419746));
#32855=CARTESIAN_POINT('Ctrl Pts',(-2.11351924490335,1.,-0.112968534419746));
#32856=CARTESIAN_POINT('Ctrl Pts',(-2.11926155590849,-1.,-0.11035023613502));
#32857=CARTESIAN_POINT('Ctrl Pts',(-2.11926155590849,1.,-0.11035023613502));
#32858=CARTESIAN_POINT('Ctrl Pts',(-2.12499752306927,-1.,-0.107690435231068));
#32859=CARTESIAN_POINT('Ctrl Pts',(-2.12499752306927,1.,-0.107690435231068));
#32860=CARTESIAN_POINT('Ctrl Pts',(-2.1307270488718,-1.,-0.104989479152703));
#32861=CARTESIAN_POINT('Ctrl Pts',(-2.1307270488718,1.,-0.104989479152703));
#32862=CARTESIAN_POINT('Ctrl Pts',(-2.13644992667052,-1.,-0.102247700556064));
#32863=CARTESIAN_POINT('Ctrl Pts',(-2.13644992667052,1.,-0.102247700556064));
#32864=CARTESIAN_POINT('Ctrl Pts',(-2.14216588395974,-1.,-0.0994654261990744));
#32865=CARTESIAN_POINT('Ctrl Pts',(-2.14216588395974,1.,-0.0994654261990744));
#32866=CARTESIAN_POINT('Ctrl Pts',(-2.14787463531864,-1.,-0.096642985230569));
#32867=CARTESIAN_POINT('Ctrl Pts',(-2.14787463531864,1.,-0.096642985230569));
#32868=CARTESIAN_POINT('Ctrl Pts',(-2.15357593978377,-1.,-0.0937807218868346));
#32869=CARTESIAN_POINT('Ctrl Pts',(-2.15357593978377,1.,-0.0937807218868346));
#32870=CARTESIAN_POINT('Ctrl Pts',(-2.15926961544808,-1.,-0.0908789888108267));
#32871=CARTESIAN_POINT('Ctrl Pts',(-2.15926961544808,1.,-0.0908789888108267));
#32872=CARTESIAN_POINT('Ctrl Pts',(-2.16495552645275,-1.,-0.0879381291387824));
#32873=CARTESIAN_POINT('Ctrl Pts',(-2.16495552645275,1.,-0.0879381291387824));
#32874=CARTESIAN_POINT('Ctrl Pts',(-2.17063357871031,-1.,-0.0849584620835644));
#32875=CARTESIAN_POINT('Ctrl Pts',(-2.17063357871031,1.,-0.0849584620835644));
#32876=CARTESIAN_POINT('Ctrl Pts',(-2.1763037121106,-1.,-0.0819402680871941));
#32877=CARTESIAN_POINT('Ctrl Pts',(-2.1763037121106,1.,-0.0819402680871941));
#32878=CARTESIAN_POINT('Ctrl Pts',(-2.18196589448304,-1.,-0.0788837727683229));
#32879=CARTESIAN_POINT('Ctrl Pts',(-2.18196589448304,1.,-0.0788837727683229));
#32880=CARTESIAN_POINT('Ctrl Pts',(-2.1876201139874,-1.,-0.0757891465833413));
#32881=CARTESIAN_POINT('Ctrl Pts',(-2.1876201139874,1.,-0.0757891465833413));
#32882=CARTESIAN_POINT('Ctrl Pts',(-2.19213712012956,-1.,-0.0732830357304277));
#32883=CARTESIAN_POINT('Ctrl Pts',(-2.19213712012956,1.,-0.0732830357304277));
#32884=CARTESIAN_POINT('Ctrl Pts',(-2.19552129483562,-1.,-0.0713863779524629));
#32885=CARTESIAN_POINT('Ctrl Pts',(-2.19552129483562,1.,-0.0713863779524629));
#32886=CARTESIAN_POINT('Ctrl Pts',(-2.19777582085261,-1.,-0.0701143536324927));
#32887=CARTESIAN_POINT('Ctrl Pts',(-2.19777582085261,1.,-0.0701143536324927));
#32888=CARTESIAN_POINT('Ctrl Pts',(-2.19890268624765,-1.,-0.0694764450219585));
#32889=CARTESIAN_POINT('Ctrl Pts',(-2.19890268624765,1.,-0.0694764450219585));
#32890=CARTESIAN_POINT('',(-1.74236521665491,1.,-0.163289472382896));
#32891=CARTESIAN_POINT('Ctrl Pts',(-1.74236521665491,1.,-0.163289472382896));
#32892=CARTESIAN_POINT('Ctrl Pts',(-1.74720349503904,1.,-0.163814161002474));
#32893=CARTESIAN_POINT('Ctrl Pts',(-1.75666056640041,1.,-0.164834765708484));
#32894=CARTESIAN_POINT('Ctrl Pts',(-1.77018771687692,1.,-0.166279355148738));
#32895=CARTESIAN_POINT('Ctrl Pts',(-1.78690649988931,1.,-0.16803277280837));
#32896=CARTESIAN_POINT('Ctrl Pts',(-1.80561530633924,1.,-0.169936923908078));
#32897=CARTESIAN_POINT('Ctrl Pts',(-1.82215766815414,1.,-0.171554770207306));
#32898=CARTESIAN_POINT('Ctrl Pts',(-1.83658380530747,1.,-0.17288944289442));
#32899=CARTESIAN_POINT('Ctrl Pts',(-1.84898113200543,1.,-0.173946627589401));
#32900=CARTESIAN_POINT('Ctrl Pts',(-1.85948367089838,1.,-0.174735259276856));
#32901=CARTESIAN_POINT('Ctrl Pts',(-1.86828349694972,1.,-0.175268337590901));
#32902=CARTESIAN_POINT('Ctrl Pts',(-1.87563767773249,1.,-0.175563480746205));
#32903=CARTESIAN_POINT('Ctrl Pts',(-1.88188663144846,1.,-0.175644148889271));
#32904=CARTESIAN_POINT('Ctrl Pts',(-1.88742606272818,1.,-0.175538155840286));
#32905=CARTESIAN_POINT('Ctrl Pts',(-1.89264630198279,1.,-0.175274276190664));
#32906=CARTESIAN_POINT('Ctrl Pts',(-1.89788101117148,1.,-0.174879405091277));
#32907=CARTESIAN_POINT('Ctrl Pts',(-1.90335253863003,1.,-0.174375518661222));
#32908=CARTESIAN_POINT('Ctrl Pts',(-1.90911693975475,1.,-0.173776635257984));
#32909=CARTESIAN_POINT('Ctrl Pts',(-1.91511429159681,1.,-0.173090695383619));
#32910=CARTESIAN_POINT('Ctrl Pts',(-1.92122334398034,1.,-0.172321621259557));
#32911=CARTESIAN_POINT('Ctrl Pts',(-1.92731093582,1.,-0.17147119153296));
#32912=CARTESIAN_POINT('Ctrl Pts',(-1.93329183155455,1.,-0.170541253116136));
#32913=CARTESIAN_POINT('Ctrl Pts',(-1.93915639211497,1.,-0.169534904817425));
#32914=CARTESIAN_POINT('Ctrl Pts',(-1.94493757756879,1.,-0.168455741607516));
#32915=CARTESIAN_POINT('Ctrl Pts',(-1.95069027794286,1.,-0.167307501784469));
#32916=CARTESIAN_POINT('Ctrl Pts',(-1.95646759718755,1.,-0.166093592002833));
#32917=CARTESIAN_POINT('Ctrl Pts',(-1.96229379940174,1.,-0.1648165689203));
#32918=CARTESIAN_POINT('Ctrl Pts',(-1.96816512678,1.,-0.16347818545776));
#32919=CARTESIAN_POINT('Ctrl Pts',(-1.97406280235204,1.,-0.162079693556302));
#32920=CARTESIAN_POINT('Ctrl Pts',(-1.97996195437557,1.,-0.16062206078461));
#32921=CARTESIAN_POINT('Ctrl Pts',(-1.98584238283279,1.,-0.159106226437289));
#32922=CARTESIAN_POINT('Ctrl Pts',(-1.99169810931893,1.,-0.157533331459215));
#32923=CARTESIAN_POINT('Ctrl Pts',(-1.99753284771487,1.,-0.155904629548775));
#32924=CARTESIAN_POINT('Ctrl Pts',(-2.00335565310539,1.,-0.154221403049719));
#32925=CARTESIAN_POINT('Ctrl Pts',(-2.00917680318426,1.,-0.152484883621452));
#32926=CARTESIAN_POINT('Ctrl Pts',(-2.01500291940243,1.,-0.150696157673084));
#32927=CARTESIAN_POINT('Ctrl Pts',(-2.02083464969897,1.,-0.148856124775343));
#32928=CARTESIAN_POINT('Ctrl Pts',(-2.02666926182017,1.,-0.146965557332586));
#32929=CARTESIAN_POINT('Ctrl Pts',(-2.03250223739941,1.,-0.145025140186058));
#32930=CARTESIAN_POINT('Ctrl Pts',(-2.03832911025913,1.,-0.143035515058208));
#32931=CARTESIAN_POINT('Ctrl Pts',(-2.04414757947919,1.,-0.140997332152545));
#32932=CARTESIAN_POINT('Ctrl Pts',(-2.04995762001333,1.,-0.138911255368966));
#32933=CARTESIAN_POINT('Ctrl Pts',(-2.0557604441427,1.,-0.136777941218044));
#32934=CARTESIAN_POINT('Ctrl Pts',(-2.06155781517844,1.,-0.134598026192107));
#32935=CARTESIAN_POINT('Ctrl Pts',(-2.06735123910319,1.,-0.13237211154771));
#32936=CARTESIAN_POINT('Ctrl Pts',(-2.07314114713047,1.,-0.130100748328401));
#32937=CARTESIAN_POINT('Ctrl Pts',(-2.07892715110967,1.,-0.127784445276116));
#32938=CARTESIAN_POINT('Ctrl Pts',(-2.08470840653628,1.,-0.125423679412058));
#32939=CARTESIAN_POINT('Ctrl Pts',(-2.09048392424826,1.,-0.123018905621083));
#32940=CARTESIAN_POINT('Ctrl Pts',(-2.09625292867756,1.,-0.120570567965129));
#32941=CARTESIAN_POINT('Ctrl Pts',(-2.10201512132945,1.,-0.118079107988368));
#32942=CARTESIAN_POINT('Ctrl Pts',(-2.10777050261359,1.,-0.11554495768794));
#32943=CARTESIAN_POINT('Ctrl Pts',(-2.11351924490335,1.,-0.112968534419746));
#32944=CARTESIAN_POINT('Ctrl Pts',(-2.11926155590849,1.,-0.11035023613502));
#32945=CARTESIAN_POINT('Ctrl Pts',(-2.12499752306927,1.,-0.107690435231068));
#32946=CARTESIAN_POINT('Ctrl Pts',(-2.1307270488718,1.,-0.104989479152703));
#32947=CARTESIAN_POINT('Ctrl Pts',(-2.13644992667052,1.,-0.102247700556064));
#32948=CARTESIAN_POINT('Ctrl Pts',(-2.14216588395974,1.,-0.0994654261990744));
#32949=CARTESIAN_POINT('Ctrl Pts',(-2.14787463531864,1.,-0.096642985230569));
#32950=CARTESIAN_POINT('Ctrl Pts',(-2.15357593978377,1.,-0.0937807218868346));
#32951=CARTESIAN_POINT('Ctrl Pts',(-2.15926961544808,1.,-0.0908789888108267));
#32952=CARTESIAN_POINT('Ctrl Pts',(-2.16495552645275,1.,-0.0879381291387824));
#32953=CARTESIAN_POINT('Ctrl Pts',(-2.17063357871031,1.,-0.0849584620835644));
#32954=CARTESIAN_POINT('Ctrl Pts',(-2.1763037121106,1.,-0.0819402680871941));
#32955=CARTESIAN_POINT('Ctrl Pts',(-2.18196589448304,1.,-0.0788837727683229));
#32956=CARTESIAN_POINT('Ctrl Pts',(-2.1876201139874,1.,-0.0757891465833413));
#32957=CARTESIAN_POINT('Ctrl Pts',(-2.19213712012956,1.,-0.0732830357304277));
#32958=CARTESIAN_POINT('Ctrl Pts',(-2.19552129483562,1.,-0.0713863779524629));
#32959=CARTESIAN_POINT('Ctrl Pts',(-2.19777582085261,1.,-0.0701143536324927));
#32960=CARTESIAN_POINT('Ctrl Pts',(-2.19890268624765,1.,-0.0694764450219585));
#32961=CARTESIAN_POINT('',(-1.74236521665491,0.,-0.163289472382896));
#32962=CARTESIAN_POINT('Origin',(0.,0.,0.));
#32963=CARTESIAN_POINT('',(-1.7075470150345,1.,-0.383122945602004));
#32964=CARTESIAN_POINT('Origin',(0.,1.,0.));
#32965=CARTESIAN_POINT('',(-1.7075470150345,0.,-0.383122945602004));
#32966=CARTESIAN_POINT('Ctrl Pts',(-2.11275013067528,-1.,-0.61342227326009));
#32967=CARTESIAN_POINT('Ctrl Pts',(-2.11275013067528,1.,-0.61342227326009));
#32968=CARTESIAN_POINT('Ctrl Pts',(-2.11187554260142,-1.,-0.61246736556225));
#32969=CARTESIAN_POINT('Ctrl Pts',(-2.11187554260142,1.,-0.61246736556225));
#32970=CARTESIAN_POINT('Ctrl Pts',(-2.11012443807661,-1.,-0.610560911691113));
#32971=CARTESIAN_POINT('Ctrl Pts',(-2.11012443807661,1.,-0.610560911691113));
#32972=CARTESIAN_POINT('Ctrl Pts',(-2.10749199615859,-1.,-0.607711315456826));
#32973=CARTESIAN_POINT('Ctrl Pts',(-2.10749199615859,1.,-0.607711315456826));
#32974=CARTESIAN_POINT('Ctrl Pts',(-2.10397049887709,-1.,-0.603932030738212));
#32975=CARTESIAN_POINT('Ctrl Pts',(-2.10397049887709,1.,-0.603932030738212));
#32976=CARTESIAN_POINT('Ctrl Pts',(-2.09954930865331,-1.,-0.599241616422144));
#32977=CARTESIAN_POINT('Ctrl Pts',(-2.09954930865331,1.,-0.599241616422144));
#32978=CARTESIAN_POINT('Ctrl Pts',(-2.09510876220501,-1.,-0.594585006052823));
#32979=CARTESIAN_POINT('Ctrl Pts',(-2.09510876220501,1.,-0.594585006052823));
#32980=CARTESIAN_POINT('Ctrl Pts',(-2.09064881812053,-1.,-0.589962365403189));
#32981=CARTESIAN_POINT('Ctrl Pts',(-2.09064881812053,1.,-0.589962365403189));
#32982=CARTESIAN_POINT('Ctrl Pts',(-2.086169437277,-1.,-0.585373918990895));
#32983=CARTESIAN_POINT('Ctrl Pts',(-2.086169437277,1.,-0.585373918990895));
#32984=CARTESIAN_POINT('Ctrl Pts',(-2.08167059018138,-1.,-0.580819952107257));
#32985=CARTESIAN_POINT('Ctrl Pts',(-2.08167059018138,1.,-0.580819952107257));
#32986=CARTESIAN_POINT('Ctrl Pts',(-2.07715226767361,-1.,-0.576300797416274));
#32987=CARTESIAN_POINT('Ctrl Pts',(-2.07715226767361,1.,-0.576300797416274));
#32988=CARTESIAN_POINT('Ctrl Pts',(-2.07261449292757,-1.,-0.571816823242411));
#32989=CARTESIAN_POINT('Ctrl Pts',(-2.07261449292757,1.,-0.571816823242411));
#32990=CARTESIAN_POINT('Ctrl Pts',(-2.06805732997383,-1.,-0.567368421181229));
#32991=CARTESIAN_POINT('Ctrl Pts',(-2.06805732997383,1.,-0.567368421181229));
#32992=CARTESIAN_POINT('Ctrl Pts',(-2.06348090160697,-1.,-0.562955993082574));
#32993=CARTESIAN_POINT('Ctrl Pts',(-2.06348090160697,1.,-0.562955993082574));
#32994=CARTESIAN_POINT('Ctrl Pts',(-2.05888537756571,-1.,-0.558579940185467));
#32995=CARTESIAN_POINT('Ctrl Pts',(-2.05888537756571,1.,-0.558579940185467));
#32996=CARTESIAN_POINT('Ctrl Pts',(-2.05427091604482,-1.,-0.554240657464109));
#32997=CARTESIAN_POINT('Ctrl Pts',(-2.05427091604482,1.,-0.554240657464109));
#32998=CARTESIAN_POINT('Ctrl Pts',(-2.04963761077974,-1.,-0.549938525150342));
#32999=CARTESIAN_POINT('Ctrl Pts',(-2.04963761077974,1.,-0.549938525150342));
#33000=CARTESIAN_POINT('Ctrl Pts',(-2.0449854471456,-1.,-0.545673903817348));
#33001=CARTESIAN_POINT('Ctrl Pts',(-2.0449854471456,1.,-0.545673903817348));
#33002=CARTESIAN_POINT('Ctrl Pts',(-2.0403142269048,-1.,-0.54144712061552));
#33003=CARTESIAN_POINT('Ctrl Pts',(-2.0403142269048,1.,-0.54144712061552));
#33004=CARTESIAN_POINT('Ctrl Pts',(-2.03562362953993,-1.,-0.537258489833134));
#33005=CARTESIAN_POINT('Ctrl Pts',(-2.03562362953993,1.,-0.537258489833134));
#33006=CARTESIAN_POINT('Ctrl Pts',(-2.03091336214401,-1.,-0.533108355132905));
#33007=CARTESIAN_POINT('Ctrl Pts',(-2.03091336214401,1.,-0.533108355132905));
#33008=CARTESIAN_POINT('Ctrl Pts',(-2.02618329083289,-1.,-0.52899712724191));
#33009=CARTESIAN_POINT('Ctrl Pts',(-2.02618329083289,1.,-0.52899712724191));
#33010=CARTESIAN_POINT('Ctrl Pts',(-2.02143356304712,-1.,-0.524925318333518));
#33011=CARTESIAN_POINT('Ctrl Pts',(-2.02143356304712,1.,-0.524925318333518));
#33012=CARTESIAN_POINT('Ctrl Pts',(-2.01666477917305,-1.,-0.520893590399428));
#33013=CARTESIAN_POINT('Ctrl Pts',(-2.01666477917305,1.,-0.520893590399428));
#33014=CARTESIAN_POINT('Ctrl Pts',(-2.01187773939257,-1.,-0.516902681728733));
#33015=CARTESIAN_POINT('Ctrl Pts',(-2.01187773939257,1.,-0.516902681728733));
#33016=CARTESIAN_POINT('Ctrl Pts',(-2.00707309946955,-1.,-0.512953306961813));
#33017=CARTESIAN_POINT('Ctrl Pts',(-2.00707309946955,1.,-0.512953306961813));
#33018=CARTESIAN_POINT('Ctrl Pts',(-2.00225107134733,-1.,-0.509046069886152));
#33019=CARTESIAN_POINT('Ctrl Pts',(-2.00225107134733,1.,-0.509046069886152));
#33020=CARTESIAN_POINT('Ctrl Pts',(-1.99741107463567,-1.,-0.505181361323011));
#33021=CARTESIAN_POINT('Ctrl Pts',(-1.99741107463567,1.,-0.505181361323011));
#33022=CARTESIAN_POINT('Ctrl Pts',(-1.9925514912615,-1.,-0.501359287727129));
#33023=CARTESIAN_POINT('Ctrl Pts',(-1.9925514912615,1.,-0.501359287727129));
#33024=CARTESIAN_POINT('Ctrl Pts',(-1.98767044752929,-1.,-0.497579909545564));
#33025=CARTESIAN_POINT('Ctrl Pts',(-1.98767044752929,1.,-0.497579909545564));
#33026=CARTESIAN_POINT('Ctrl Pts',(-1.9827665876182,-1.,-0.493843476541492));
#33027=CARTESIAN_POINT('Ctrl Pts',(-1.9827665876182,1.,-0.493843476541492));
#33028=CARTESIAN_POINT('Ctrl Pts',(-1.97783973019229,-1.,-0.490150627860955));
#33029=CARTESIAN_POINT('Ctrl Pts',(-1.97783973019229,1.,-0.490150627860955));
#33030=CARTESIAN_POINT('Ctrl Pts',(-1.97289186263272,-1.,-0.486502692907661));
#33031=CARTESIAN_POINT('Ctrl Pts',(-1.97289186263272,1.,-0.486502692907661));
#33032=CARTESIAN_POINT('Ctrl Pts',(-1.96792703422358,-1.,-0.482901662120686));
#33033=CARTESIAN_POINT('Ctrl Pts',(-1.96792703422358,1.,-0.482901662120686));
#33034=CARTESIAN_POINT('Ctrl Pts',(-1.96294933055938,-1.,-0.479349583074846));
#33035=CARTESIAN_POINT('Ctrl Pts',(-1.96294933055938,1.,-0.479349583074846));
#33036=CARTESIAN_POINT('Ctrl Pts',(-1.95796111148175,-1.,-0.475848034683171));
#33037=CARTESIAN_POINT('Ctrl Pts',(-1.95796111148175,1.,-0.475848034683171));
#33038=CARTESIAN_POINT('Ctrl Pts',(-1.95296148278136,-1.,-0.472397672264079));
#33039=CARTESIAN_POINT('Ctrl Pts',(-1.95296148278136,1.,-0.472397672264079));
#33040=CARTESIAN_POINT('Ctrl Pts',(-1.94794381136524,-1.,-0.468997482913158));
#33041=CARTESIAN_POINT('Ctrl Pts',(-1.94794381136524,1.,-0.468997482913158));
#33042=CARTESIAN_POINT('Ctrl Pts',(-1.94289794196205,-1.,-0.465645462026064));
#33043=CARTESIAN_POINT('Ctrl Pts',(-1.94289794196205,1.,-0.465645462026064));
#33044=CARTESIAN_POINT('Ctrl Pts',(-1.93781486640834,-1.,-0.462340031009087));
#33045=CARTESIAN_POINT('Ctrl Pts',(-1.93781486640834,1.,-0.462340031009087));
#33046=CARTESIAN_POINT('Ctrl Pts',(-1.93269066517936,-1.,-0.459081234547931));
#33047=CARTESIAN_POINT('Ctrl Pts',(-1.93269066517936,1.,-0.459081234547931));
#33048=CARTESIAN_POINT('Ctrl Pts',(-1.92753067150461,-1.,-0.455872005174335));
#33049=CARTESIAN_POINT('Ctrl Pts',(-1.92753067150461,1.,-0.455872005174335));
#33050=CARTESIAN_POINT('Ctrl Pts',(-1.9223538064847,-1.,-0.452719478359356));
#33051=CARTESIAN_POINT('Ctrl Pts',(-1.9223538064847,1.,-0.452719478359356));
#33052=CARTESIAN_POINT('Ctrl Pts',(-1.91718342555717,-1.,-0.449632260106572));
#33053=CARTESIAN_POINT('Ctrl Pts',(-1.91718342555717,1.,-0.449632260106572));
#33054=CARTESIAN_POINT('Ctrl Pts',(-1.91203699981095,-1.,-0.446617343485651));
#33055=CARTESIAN_POINT('Ctrl Pts',(-1.91203699981095,1.,-0.446617343485651));
#33056=CARTESIAN_POINT('Ctrl Pts',(-1.90691756144906,-1.,-0.44367755684917));
#33057=CARTESIAN_POINT('Ctrl Pts',(-1.90691756144906,1.,-0.44367755684917));
#33058=CARTESIAN_POINT('Ctrl Pts',(-1.90180124389137,-1.,-0.44080783370416));
#33059=CARTESIAN_POINT('Ctrl Pts',(-1.90180124389137,1.,-0.44080783370416));
#33060=CARTESIAN_POINT('Ctrl Pts',(-1.89663648956549,-1.,-0.437995003948443));
#33061=CARTESIAN_POINT('Ctrl Pts',(-1.89663648956549,1.,-0.437995003948443));
#33062=CARTESIAN_POINT('Ctrl Pts',(-1.89136993975585,-1.,-0.43522566096358));
#33063=CARTESIAN_POINT('Ctrl Pts',(-1.89136993975585,1.,-0.43522566096358));
#33064=CARTESIAN_POINT('Ctrl Pts',(-1.88596913666828,-1.,-0.432493038548833));
#33065=CARTESIAN_POINT('Ctrl Pts',(-1.88596913666828,1.,-0.432493038548833));
#33066=CARTESIAN_POINT('Ctrl Pts',(-1.88044229001778,-1.,-0.429803062482217));
#33067=CARTESIAN_POINT('Ctrl Pts',(-1.88044229001778,1.,-0.429803062482217));
#33068=CARTESIAN_POINT('Ctrl Pts',(-1.87486989291333,-1.,-0.427183828518743));
#33069=CARTESIAN_POINT('Ctrl Pts',(-1.87486989291333,1.,-0.427183828518743));
#33070=CARTESIAN_POINT('Ctrl Pts',(-1.8693780394412,-1.,-0.424678177290876));
#33071=CARTESIAN_POINT('Ctrl Pts',(-1.8693780394412,1.,-0.424678177290876));
#33072=CARTESIAN_POINT('Ctrl Pts',(-1.86408083333863,-1.,-0.422327307417884));
#33073=CARTESIAN_POINT('Ctrl Pts',(-1.86408083333863,1.,-0.422327307417884));
#33074=CARTESIAN_POINT('Ctrl Pts',(-1.8590328109667,-1.,-0.420157287975583));
#33075=CARTESIAN_POINT('Ctrl Pts',(-1.8590328109667,1.,-0.420157287975583));
#33076=CARTESIAN_POINT('Ctrl Pts',(-1.8541763285645,-1.,-0.418164129144045));
#33077=CARTESIAN_POINT('Ctrl Pts',(-1.8541763285645,1.,-0.418164129144045));
#33078=CARTESIAN_POINT('Ctrl Pts',(-1.84929312930314,-1.,-0.416300022039885));
#33079=CARTESIAN_POINT('Ctrl Pts',(-1.84929312930314,1.,-0.416300022039885));
#33080=CARTESIAN_POINT('Ctrl Pts',(-1.84405757074218,-1.,-0.414487438255542));
#33081=CARTESIAN_POINT('Ctrl Pts',(-1.84405757074218,1.,-0.414487438255542));
#33082=CARTESIAN_POINT('Ctrl Pts',(-1.8380895347617,-1.,-0.412633125322945));
#33083=CARTESIAN_POINT('Ctrl Pts',(-1.8380895347617,1.,-0.412633125322945));
#33084=CARTESIAN_POINT('Ctrl Pts',(-1.83100408895047,-1.,-0.410641256301276));
#33085=CARTESIAN_POINT('Ctrl Pts',(-1.83100408895047,1.,-0.410641256301276));
#33086=CARTESIAN_POINT('Ctrl Pts',(-1.82247022677562,-1.,-0.408428948106227));
#33087=CARTESIAN_POINT('Ctrl Pts',(-1.82247022677562,1.,-0.408428948106227));
#33088=CARTESIAN_POINT('Ctrl Pts',(-1.81223801812013,-1.,-0.405933518407175));
#33089=CARTESIAN_POINT('Ctrl Pts',(-1.81223801812013,1.,-0.405933518407175));
#33090=CARTESIAN_POINT('Ctrl Pts',(-1.80012077173238,-1.,-0.403107976163396));
#33091=CARTESIAN_POINT('Ctrl Pts',(-1.80012077173238,1.,-0.403107976163396));
#33092=CARTESIAN_POINT('Ctrl Pts',(-1.78598826343754,-1.,-0.399919403774155));
#33093=CARTESIAN_POINT('Ctrl Pts',(-1.78598826343754,1.,-0.399919403774155));
#33094=CARTESIAN_POINT('Ctrl Pts',(-1.76975560043442,-1.,-0.396346196110688));
#33095=CARTESIAN_POINT('Ctrl Pts',(-1.76975560043442,1.,-0.396346196110688));
#33096=CARTESIAN_POINT('Ctrl Pts',(-1.75137405310193,-1.,-0.392375812285395));
#33097=CARTESIAN_POINT('Ctrl Pts',(-1.75137405310193,1.,-0.392375812285395));
#33098=CARTESIAN_POINT('Ctrl Pts',(-1.73493170972829,-1.,-0.388877023502615));
#33099=CARTESIAN_POINT('Ctrl Pts',(-1.73493170972829,1.,-0.388877023502615));
#33100=CARTESIAN_POINT('Ctrl Pts',(-1.72162022244582,-1.,-0.386070790323281));
#33101=CARTESIAN_POINT('Ctrl Pts',(-1.72162022244582,1.,-0.386070790323281));
#33102=CARTESIAN_POINT('Ctrl Pts',(-1.71231062891398,-1.,-0.384119047314215));
#33103=CARTESIAN_POINT('Ctrl Pts',(-1.71231062891398,1.,-0.384119047314215));
#33104=CARTESIAN_POINT('Ctrl Pts',(-1.7075470150345,-1.,-0.383122945602004));
#33105=CARTESIAN_POINT('Ctrl Pts',(-1.7075470150345,1.,-0.383122945602004));
#33106=CARTESIAN_POINT('',(-2.11275013067528,1.,-0.61342227326009));
#33107=CARTESIAN_POINT('Ctrl Pts',(-2.11275013067528,1.,-0.61342227326009));
#33108=CARTESIAN_POINT('Ctrl Pts',(-2.11187554260142,1.,-0.61246736556225));
#33109=CARTESIAN_POINT('Ctrl Pts',(-2.11012443807661,1.,-0.610560911691113));
#33110=CARTESIAN_POINT('Ctrl Pts',(-2.10749199615859,1.,-0.607711315456826));
#33111=CARTESIAN_POINT('Ctrl Pts',(-2.10397049887709,1.,-0.603932030738212));
#33112=CARTESIAN_POINT('Ctrl Pts',(-2.09954930865331,1.,-0.599241616422144));
#33113=CARTESIAN_POINT('Ctrl Pts',(-2.09510876220501,1.,-0.594585006052823));
#33114=CARTESIAN_POINT('Ctrl Pts',(-2.09064881812053,1.,-0.589962365403189));
#33115=CARTESIAN_POINT('Ctrl Pts',(-2.086169437277,1.,-0.585373918990895));
#33116=CARTESIAN_POINT('Ctrl Pts',(-2.08167059018138,1.,-0.580819952107257));
#33117=CARTESIAN_POINT('Ctrl Pts',(-2.07715226767361,1.,-0.576300797416274));
#33118=CARTESIAN_POINT('Ctrl Pts',(-2.07261449292757,1.,-0.571816823242411));
#33119=CARTESIAN_POINT('Ctrl Pts',(-2.06805732997383,1.,-0.567368421181229));
#33120=CARTESIAN_POINT('Ctrl Pts',(-2.06348090160697,1.,-0.562955993082574));
#33121=CARTESIAN_POINT('Ctrl Pts',(-2.05888537756571,1.,-0.558579940185467));
#33122=CARTESIAN_POINT('Ctrl Pts',(-2.05427091604482,1.,-0.554240657464109));
#33123=CARTESIAN_POINT('Ctrl Pts',(-2.04963761077974,1.,-0.549938525150342));
#33124=CARTESIAN_POINT('Ctrl Pts',(-2.0449854471456,1.,-0.545673903817348));
#33125=CARTESIAN_POINT('Ctrl Pts',(-2.0403142269048,1.,-0.54144712061552));
#33126=CARTESIAN_POINT('Ctrl Pts',(-2.03562362953993,1.,-0.537258489833134));
#33127=CARTESIAN_POINT('Ctrl Pts',(-2.03091336214401,1.,-0.533108355132905));
#33128=CARTESIAN_POINT('Ctrl Pts',(-2.02618329083289,1.,-0.52899712724191));
#33129=CARTESIAN_POINT('Ctrl Pts',(-2.02143356304712,1.,-0.524925318333518));
#33130=CARTESIAN_POINT('Ctrl Pts',(-2.01666477917305,1.,-0.520893590399428));
#33131=CARTESIAN_POINT('Ctrl Pts',(-2.01187773939257,1.,-0.516902681728733));
#33132=CARTESIAN_POINT('Ctrl Pts',(-2.00707309946955,1.,-0.512953306961813));
#33133=CARTESIAN_POINT('Ctrl Pts',(-2.00225107134733,1.,-0.509046069886152));
#33134=CARTESIAN_POINT('Ctrl Pts',(-1.99741107463567,1.,-0.505181361323011));
#33135=CARTESIAN_POINT('Ctrl Pts',(-1.9925514912615,1.,-0.501359287727129));
#33136=CARTESIAN_POINT('Ctrl Pts',(-1.98767044752929,1.,-0.497579909545564));
#33137=CARTESIAN_POINT('Ctrl Pts',(-1.9827665876182,1.,-0.493843476541492));
#33138=CARTESIAN_POINT('Ctrl Pts',(-1.97783973019229,1.,-0.490150627860955));
#33139=CARTESIAN_POINT('Ctrl Pts',(-1.97289186263272,1.,-0.486502692907661));
#33140=CARTESIAN_POINT('Ctrl Pts',(-1.96792703422358,1.,-0.482901662120686));
#33141=CARTESIAN_POINT('Ctrl Pts',(-1.96294933055938,1.,-0.479349583074846));
#33142=CARTESIAN_POINT('Ctrl Pts',(-1.95796111148175,1.,-0.475848034683171));
#33143=CARTESIAN_POINT('Ctrl Pts',(-1.95296148278136,1.,-0.472397672264079));
#33144=CARTESIAN_POINT('Ctrl Pts',(-1.94794381136524,1.,-0.468997482913158));
#33145=CARTESIAN_POINT('Ctrl Pts',(-1.94289794196205,1.,-0.465645462026064));
#33146=CARTESIAN_POINT('Ctrl Pts',(-1.93781486640834,1.,-0.462340031009087));
#33147=CARTESIAN_POINT('Ctrl Pts',(-1.93269066517936,1.,-0.459081234547931));
#33148=CARTESIAN_POINT('Ctrl Pts',(-1.92753067150461,1.,-0.455872005174335));
#33149=CARTESIAN_POINT('Ctrl Pts',(-1.9223538064847,1.,-0.452719478359356));
#33150=CARTESIAN_POINT('Ctrl Pts',(-1.91718342555717,1.,-0.449632260106572));
#33151=CARTESIAN_POINT('Ctrl Pts',(-1.91203699981095,1.,-0.446617343485651));
#33152=CARTESIAN_POINT('Ctrl Pts',(-1.90691756144906,1.,-0.44367755684917));
#33153=CARTESIAN_POINT('Ctrl Pts',(-1.90180124389137,1.,-0.44080783370416));
#33154=CARTESIAN_POINT('Ctrl Pts',(-1.89663648956549,1.,-0.437995003948443));
#33155=CARTESIAN_POINT('Ctrl Pts',(-1.89136993975585,1.,-0.43522566096358));
#33156=CARTESIAN_POINT('Ctrl Pts',(-1.88596913666828,1.,-0.432493038548833));
#33157=CARTESIAN_POINT('Ctrl Pts',(-1.88044229001778,1.,-0.429803062482217));
#33158=CARTESIAN_POINT('Ctrl Pts',(-1.87486989291333,1.,-0.427183828518743));
#33159=CARTESIAN_POINT('Ctrl Pts',(-1.8693780394412,1.,-0.424678177290876));
#33160=CARTESIAN_POINT('Ctrl Pts',(-1.86408083333863,1.,-0.422327307417884));
#33161=CARTESIAN_POINT('Ctrl Pts',(-1.8590328109667,1.,-0.420157287975583));
#33162=CARTESIAN_POINT('Ctrl Pts',(-1.8541763285645,1.,-0.418164129144045));
#33163=CARTESIAN_POINT('Ctrl Pts',(-1.84929312930314,1.,-0.416300022039885));
#33164=CARTESIAN_POINT('Ctrl Pts',(-1.84405757074218,1.,-0.414487438255542));
#33165=CARTESIAN_POINT('Ctrl Pts',(-1.8380895347617,1.,-0.412633125322945));
#33166=CARTESIAN_POINT('Ctrl Pts',(-1.83100408895047,1.,-0.410641256301276));
#33167=CARTESIAN_POINT('Ctrl Pts',(-1.82247022677562,1.,-0.408428948106227));
#33168=CARTESIAN_POINT('Ctrl Pts',(-1.81223801812013,1.,-0.405933518407175));
#33169=CARTESIAN_POINT('Ctrl Pts',(-1.80012077173238,1.,-0.403107976163396));
#33170=CARTESIAN_POINT('Ctrl Pts',(-1.78598826343754,1.,-0.399919403774155));
#33171=CARTESIAN_POINT('Ctrl Pts',(-1.76975560043442,1.,-0.396346196110688));
#33172=CARTESIAN_POINT('Ctrl Pts',(-1.75137405310193,1.,-0.392375812285395));
#33173=CARTESIAN_POINT('Ctrl Pts',(-1.73493170972829,1.,-0.388877023502615));
#33174=CARTESIAN_POINT('Ctrl Pts',(-1.72162022244582,1.,-0.386070790323281));
#33175=CARTESIAN_POINT('Ctrl Pts',(-1.71231062891398,1.,-0.384119047314215));
#33176=CARTESIAN_POINT('Ctrl Pts',(-1.7075470150345,1.,-0.383122945602004));
#33177=CARTESIAN_POINT('',(-2.11275013067528,0.,-0.61342227326009));
#33178=CARTESIAN_POINT('Origin',(-2.0698113262342,0.,-0.745574324794401));
#33179=CARTESIAN_POINT('',(-2.0698113262342,1.,-0.745574324794401));
#33180=CARTESIAN_POINT('',(-2.11275013067528,1.,-0.61342227326009));
#33181=CARTESIAN_POINT('',(-2.0698113262342,0.,-0.745574324794401));
#33182=CARTESIAN_POINT('Ctrl Pts',(-1.60662857109684,-1.,-0.693717979106306));
#33183=CARTESIAN_POINT('Ctrl Pts',(-1.60662857109684,1.,-0.693717979106306));
#33184=CARTESIAN_POINT('Ctrl Pts',(-1.61106790958151,-1.,-0.695712097881194));
#33185=CARTESIAN_POINT('Ctrl Pts',(-1.61106790958151,1.,-0.695712097881194));
#33186=CARTESIAN_POINT('Ctrl Pts',(-1.61974673472612,-1.,-0.699605146405088));
#33187=CARTESIAN_POINT('Ctrl Pts',(-1.61974673472612,1.,-0.699605146405088));
#33188=CARTESIAN_POINT('Ctrl Pts',(-1.63216541664676,-1.,-0.705159151988319));
#33189=CARTESIAN_POINT('Ctrl Pts',(-1.63216541664676,1.,-0.705159151988319));
#33190=CARTESIAN_POINT('Ctrl Pts',(-1.64752408832016,-1.,-0.711993139355394));
#33191=CARTESIAN_POINT('Ctrl Pts',(-1.64752408832016,1.,-0.711993139355394));
#33192=CARTESIAN_POINT('Ctrl Pts',(-1.6647288055568,-1.,-0.719585433804282));
#33193=CARTESIAN_POINT('Ctrl Pts',(-1.6647288055568,1.,-0.719585433804282));
#33194=CARTESIAN_POINT('Ctrl Pts',(-1.67996158455503,-1.,-0.726235967997433));
#33195=CARTESIAN_POINT('Ctrl Pts',(-1.67996158455503,1.,-0.726235967997433));
#33196=CARTESIAN_POINT('Ctrl Pts',(-1.69326921975743,-1.,-0.731963238697195));
#33197=CARTESIAN_POINT('Ctrl Pts',(-1.69326921975743,1.,-0.731963238697195));
#33198=CARTESIAN_POINT('Ctrl Pts',(-1.70473309006121,-1.,-0.736799665724771));
#33199=CARTESIAN_POINT('Ctrl Pts',(-1.70473309006121,1.,-0.736799665724771));
#33200=CARTESIAN_POINT('Ctrl Pts',(-1.71447789751927,-1.,-0.740795162032087));
#33201=CARTESIAN_POINT('Ctrl Pts',(-1.71447789751927,1.,-0.740795162032087));
#33202=CARTESIAN_POINT('Ctrl Pts',(-1.7226822991693,-1.,-0.744021445433764));
#33203=CARTESIAN_POINT('Ctrl Pts',(-1.7226822991693,1.,-0.744021445433764));
#33204=CARTESIAN_POINT('Ctrl Pts',(-1.72958533647399,-1.,-0.746574710096436));
#33205=CARTESIAN_POINT('Ctrl Pts',(-1.72958533647399,1.,-0.746574710096436));
#33206=CARTESIAN_POINT('Ctrl Pts',(-1.73550351679848,-1.,-0.748582462954854));
#33207=CARTESIAN_POINT('Ctrl Pts',(-1.73550351679848,1.,-0.748582462954854));
#33208=CARTESIAN_POINT('Ctrl Pts',(-1.74080458266705,-1.,-0.75019343597954));
#33209=CARTESIAN_POINT('Ctrl Pts',(-1.74080458266705,1.,-0.75019343597954));
#33210=CARTESIAN_POINT('Ctrl Pts',(-1.74585086852298,-1.,-0.751555614163629));
#33211=CARTESIAN_POINT('Ctrl Pts',(-1.74585086852298,1.,-0.751555614163629));
#33212=CARTESIAN_POINT('Ctrl Pts',(-1.75095139468809,-1.,-0.752797683531377));
#33213=CARTESIAN_POINT('Ctrl Pts',(-1.75095139468809,1.,-0.752797683531377));
#33214=CARTESIAN_POINT('Ctrl Pts',(-1.75631083600175,-1.,-0.75400925402848));
#33215=CARTESIAN_POINT('Ctrl Pts',(-1.75631083600175,1.,-0.75400925402848));
#33216=CARTESIAN_POINT('Ctrl Pts',(-1.7619781724032,-1.,-0.755220979975262));
#33217=CARTESIAN_POINT('Ctrl Pts',(-1.7619781724032,1.,-0.755220979975262));
#33218=CARTESIAN_POINT('Ctrl Pts',(-1.76789396003141,-1.,-0.756421896028403));
#33219=CARTESIAN_POINT('Ctrl Pts',(-1.76789396003141,1.,-0.756421896028403));
#33220=CARTESIAN_POINT('Ctrl Pts',(-1.77394167108342,-1.,-0.757578264077238));
#33221=CARTESIAN_POINT('Ctrl Pts',(-1.77394167108342,1.,-0.757578264077238));
#33222=CARTESIAN_POINT('Ctrl Pts',(-1.77999411220912,-1.,-0.75865062667738));
#33223=CARTESIAN_POINT('Ctrl Pts',(-1.77999411220912,1.,-0.75865062667738));
#33224=CARTESIAN_POINT('Ctrl Pts',(-1.78596964884526,-1.,-0.759614401109868));
#33225=CARTESIAN_POINT('Ctrl Pts',(-1.78596964884526,1.,-0.759614401109868));
#33226=CARTESIAN_POINT('Ctrl Pts',(-1.79185815610802,-1.,-0.760469555880425));
#33227=CARTESIAN_POINT('Ctrl Pts',(-1.79185815610802,1.,-0.760469555880425));
#33228=CARTESIAN_POINT('Ctrl Pts',(-1.79768986997735,-1.,-0.761229695230359));
#33229=CARTESIAN_POINT('Ctrl Pts',(-1.79768986997735,1.,-0.761229695230359));
#33230=CARTESIAN_POINT('Ctrl Pts',(-1.80351583877334,-1.,-0.761915336443515));
#33231=CARTESIAN_POINT('Ctrl Pts',(-1.80351583877334,1.,-0.761915336443515));
#33232=CARTESIAN_POINT('Ctrl Pts',(-1.80938551463989,-1.,-0.762546129464036));
#33233=CARTESIAN_POINT('Ctrl Pts',(-1.80938551463989,1.,-0.762546129464036));
#33234=CARTESIAN_POINT('Ctrl Pts',(-1.81532118405566,-1.,-0.763132003836783));
#33235=CARTESIAN_POINT('Ctrl Pts',(-1.81532118405566,1.,-0.763132003836783));
#33236=CARTESIAN_POINT('Ctrl Pts',(-1.82131873145297,-1.,-0.763673465462854));
#33237=CARTESIAN_POINT('Ctrl Pts',(-1.82131873145297,1.,-0.763673465462854));
#33238=CARTESIAN_POINT('Ctrl Pts',(-1.8273599120008,-1.,-0.764165902606055));
#33239=CARTESIAN_POINT('Ctrl Pts',(-1.8273599120008,1.,-0.764165902606055));
#33240=CARTESIAN_POINT('Ctrl Pts',(-1.8334207722714,-1.,-0.764602549687845));
#33241=CARTESIAN_POINT('Ctrl Pts',(-1.8334207722714,1.,-0.764602549687845));
#33242=CARTESIAN_POINT('Ctrl Pts',(-1.83948181064823,-1.,-0.764978057881687));
#33243=CARTESIAN_POINT('Ctrl Pts',(-1.83948181064823,1.,-0.764978057881687));
#33244=CARTESIAN_POINT('Ctrl Pts',(-1.8455369887591,-1.,-0.765291664861971));
#33245=CARTESIAN_POINT('Ctrl Pts',(-1.8455369887591,1.,-0.765291664861971));
#33246=CARTESIAN_POINT('Ctrl Pts',(-1.85158945130054,-1.,-0.765545710619023));
#33247=CARTESIAN_POINT('Ctrl Pts',(-1.85158945130054,1.,-0.765545710619023));
#33248=CARTESIAN_POINT('Ctrl Pts',(-1.85764741390391,-1.,-0.765744212909305));
#33249=CARTESIAN_POINT('Ctrl Pts',(-1.85764741390391,1.,-0.765744212909305));
#33250=CARTESIAN_POINT('Ctrl Pts',(-1.86372027063314,-1.,-0.765891519092557));
#33251=CARTESIAN_POINT('Ctrl Pts',(-1.86372027063314,1.,-0.765891519092557));
#33252=CARTESIAN_POINT('Ctrl Pts',(-1.86981398314345,-1.,-0.765990708546111));
#33253=CARTESIAN_POINT('Ctrl Pts',(-1.86981398314345,1.,-0.765990708546111));
#33254=CARTESIAN_POINT('Ctrl Pts',(-1.87592888967886,-1.,-0.766042837036759));
#33255=CARTESIAN_POINT('Ctrl Pts',(-1.87592888967886,1.,-0.766042837036759));
#33256=CARTESIAN_POINT('Ctrl Pts',(-1.88206215302561,-1.,-0.766047794851868));
#33257=CARTESIAN_POINT('Ctrl Pts',(-1.88206215302561,1.,-0.766047794851868));
#33258=CARTESIAN_POINT('Ctrl Pts',(-1.88820926433409,-1.,-0.76600483706209));
#33259=CARTESIAN_POINT('Ctrl Pts',(-1.88820926433409,1.,-0.76600483706209));
#33260=CARTESIAN_POINT('Ctrl Pts',(-1.89436577771389,-1.,-0.765913193856979));
#33261=CARTESIAN_POINT('Ctrl Pts',(-1.89436577771389,1.,-0.765913193856979));
#33262=CARTESIAN_POINT('Ctrl Pts',(-1.90052930393599,-1.,-0.765772772593395));
#33263=CARTESIAN_POINT('Ctrl Pts',(-1.90052930393599,1.,-0.765772772593395));
#33264=CARTESIAN_POINT('Ctrl Pts',(-1.90669961402362,-1.,-0.765584196937936));
#33265=CARTESIAN_POINT('Ctrl Pts',(-1.90669961402362,1.,-0.765584196937936));
#33266=CARTESIAN_POINT('Ctrl Pts',(-1.91287765805174,-1.,-0.765348465884739));
#33267=CARTESIAN_POINT('Ctrl Pts',(-1.91287765805174,1.,-0.765348465884739));
#33268=CARTESIAN_POINT('Ctrl Pts',(-1.91906491634197,-1.,-0.765066729667095));
#33269=CARTESIAN_POINT('Ctrl Pts',(-1.91906491634197,1.,-0.765066729667095));
#33270=CARTESIAN_POINT('Ctrl Pts',(-1.92526263537041,-1.,-0.764740025488189));
#33271=CARTESIAN_POINT('Ctrl Pts',(-1.92526263537041,1.,-0.764740025488189));
#33272=CARTESIAN_POINT('Ctrl Pts',(-1.93147105496367,-1.,-0.764369010673889));
#33273=CARTESIAN_POINT('Ctrl Pts',(-1.93147105496367,1.,-0.764369010673889));
#33274=CARTESIAN_POINT('Ctrl Pts',(-1.93768964875867,-1.,-0.763954049121393));
#33275=CARTESIAN_POINT('Ctrl Pts',(-1.93768964875867,1.,-0.763954049121393));
#33276=CARTESIAN_POINT('Ctrl Pts',(-1.94391746617626,-1.,-0.76349533353858));
#33277=CARTESIAN_POINT('Ctrl Pts',(-1.94391746617626,1.,-0.76349533353858));
#33278=CARTESIAN_POINT('Ctrl Pts',(-1.95015342590025,-1.,-0.762992990878774));
#33279=CARTESIAN_POINT('Ctrl Pts',(-1.95015342590025,1.,-0.762992990878774));
#33280=CARTESIAN_POINT('Ctrl Pts',(-1.95639665309893,-1.,-0.762447203806263));
#33281=CARTESIAN_POINT('Ctrl Pts',(-1.95639665309893,1.,-0.762447203806263));
#33282=CARTESIAN_POINT('Ctrl Pts',(-1.96264672744229,-1.,-0.761858300014575));
#33283=CARTESIAN_POINT('Ctrl Pts',(-1.96264672744229,1.,-0.761858300014575));
#33284=CARTESIAN_POINT('Ctrl Pts',(-1.96890351582545,-1.,-0.761226690483986));
#33285=CARTESIAN_POINT('Ctrl Pts',(-1.96890351582545,1.,-0.761226690483986));
#33286=CARTESIAN_POINT('Ctrl Pts',(-1.97516705321521,-1.,-0.760552825409855));
#33287=CARTESIAN_POINT('Ctrl Pts',(-1.97516705321521,1.,-0.760552825409855));
#33288=CARTESIAN_POINT('Ctrl Pts',(-1.98143741418156,-1.,-0.759837147452135));
#33289=CARTESIAN_POINT('Ctrl Pts',(-1.98143741418156,1.,-0.759837147452135));
#33290=CARTESIAN_POINT('Ctrl Pts',(-1.98771456680806,-1.,-0.759080037802242));
#33291=CARTESIAN_POINT('Ctrl Pts',(-1.98771456680806,1.,-0.759080037802242));
#33292=CARTESIAN_POINT('Ctrl Pts',(-1.9939983109871,-1.,-0.758281796766377));
#33293=CARTESIAN_POINT('Ctrl Pts',(-1.9939983109871,1.,-0.758281796766377));
#33294=CARTESIAN_POINT('Ctrl Pts',(-2.00028834739072,-1.,-0.757442676862341));
#33295=CARTESIAN_POINT('Ctrl Pts',(-2.00028834739072,1.,-0.757442676862341));
#33296=CARTESIAN_POINT('Ctrl Pts',(-2.00658431587682,-1.,-0.756562904646496));
#33297=CARTESIAN_POINT('Ctrl Pts',(-2.00658431587682,1.,-0.756562904646496));
#33298=CARTESIAN_POINT('Ctrl Pts',(-2.01288584328149,-1.,-0.7556427049581));
#33299=CARTESIAN_POINT('Ctrl Pts',(-2.01288584328149,1.,-0.7556427049581));
#33300=CARTESIAN_POINT('Ctrl Pts',(-2.01919259406003,-1.,-0.75468233072352));
#33301=CARTESIAN_POINT('Ctrl Pts',(-2.01919259406003,1.,-0.75468233072352));
#33302=CARTESIAN_POINT('Ctrl Pts',(-2.02550428623587,-1.,-0.753682061113765));
#33303=CARTESIAN_POINT('Ctrl Pts',(-2.02550428623587,1.,-0.753682061113765));
#33304=CARTESIAN_POINT('Ctrl Pts',(-2.03182068456467,-1.,-0.752642180488104));
#33305=CARTESIAN_POINT('Ctrl Pts',(-2.03182068456467,1.,-0.752642180488104));
#33306=CARTESIAN_POINT('Ctrl Pts',(-2.03814160092173,-1.,-0.751562963361383));
#33307=CARTESIAN_POINT('Ctrl Pts',(-2.03814160092173,1.,-0.751562963361383));
#33308=CARTESIAN_POINT('Ctrl Pts',(-2.04446689147754,-1.,-0.750444657874758));
#33309=CARTESIAN_POINT('Ctrl Pts',(-2.04446689147754,1.,-0.750444657874758));
#33310=CARTESIAN_POINT('Ctrl Pts',(-2.05079645591606,-1.,-0.749287468663053));
#33311=CARTESIAN_POINT('Ctrl Pts',(-2.05079645591606,1.,-0.749287468663053));
#33312=CARTESIAN_POINT('Ctrl Pts',(-2.05713023030263,-1.,-0.748091554181101));
#33313=CARTESIAN_POINT('Ctrl Pts',(-2.05713023030263,1.,-0.748091554181101));
#33314=CARTESIAN_POINT('Ctrl Pts',(-2.06220058927162,-1.,-0.747103932785504));
#33315=CARTESIAN_POINT('Ctrl Pts',(-2.06220058927162,1.,-0.747103932785504));
#33316=CARTESIAN_POINT('Ctrl Pts',(-2.06600523016401,-1.,-0.746345871542695));
#33317=CARTESIAN_POINT('Ctrl Pts',(-2.06600523016401,1.,-0.746345871542695));
#33318=CARTESIAN_POINT('Ctrl Pts',(-2.06854248895575,-1.,-0.74583279137781));
#33319=CARTESIAN_POINT('Ctrl Pts',(-2.06854248895575,1.,-0.74583279137781));
#33320=CARTESIAN_POINT('Ctrl Pts',(-2.0698113262342,-1.,-0.745574324794401));
#33321=CARTESIAN_POINT('Ctrl Pts',(-2.0698113262342,1.,-0.745574324794401));
#33322=CARTESIAN_POINT('',(-1.60662857109684,1.,-0.693717979106306));
#33323=CARTESIAN_POINT('Ctrl Pts',(-1.60662857109684,1.,-0.693717979106306));
#33324=CARTESIAN_POINT('Ctrl Pts',(-1.61106790958151,1.,-0.695712097881194));
#33325=CARTESIAN_POINT('Ctrl Pts',(-1.61974673472612,1.,-0.699605146405088));
#33326=CARTESIAN_POINT('Ctrl Pts',(-1.63216541664676,1.,-0.705159151988319));
#33327=CARTESIAN_POINT('Ctrl Pts',(-1.64752408832016,1.,-0.711993139355394));
#33328=CARTESIAN_POINT('Ctrl Pts',(-1.6647288055568,1.,-0.719585433804282));
#33329=CARTESIAN_POINT('Ctrl Pts',(-1.67996158455503,1.,-0.726235967997433));
#33330=CARTESIAN_POINT('Ctrl Pts',(-1.69326921975743,1.,-0.731963238697195));
#33331=CARTESIAN_POINT('Ctrl Pts',(-1.70473309006121,1.,-0.736799665724771));
#33332=CARTESIAN_POINT('Ctrl Pts',(-1.71447789751927,1.,-0.740795162032087));
#33333=CARTESIAN_POINT('Ctrl Pts',(-1.7226822991693,1.,-0.744021445433764));
#33334=CARTESIAN_POINT('Ctrl Pts',(-1.72958533647399,1.,-0.746574710096436));
#33335=CARTESIAN_POINT('Ctrl Pts',(-1.73550351679848,1.,-0.748582462954854));
#33336=CARTESIAN_POINT('Ctrl Pts',(-1.74080458266705,1.,-0.75019343597954));
#33337=CARTESIAN_POINT('Ctrl Pts',(-1.74585086852298,1.,-0.751555614163629));
#33338=CARTESIAN_POINT('Ctrl Pts',(-1.75095139468809,1.,-0.752797683531377));
#33339=CARTESIAN_POINT('Ctrl Pts',(-1.75631083600175,1.,-0.75400925402848));
#33340=CARTESIAN_POINT('Ctrl Pts',(-1.7619781724032,1.,-0.755220979975262));
#33341=CARTESIAN_POINT('Ctrl Pts',(-1.76789396003141,1.,-0.756421896028403));
#33342=CARTESIAN_POINT('Ctrl Pts',(-1.77394167108342,1.,-0.757578264077238));
#33343=CARTESIAN_POINT('Ctrl Pts',(-1.77999411220912,1.,-0.75865062667738));
#33344=CARTESIAN_POINT('Ctrl Pts',(-1.78596964884526,1.,-0.759614401109868));
#33345=CARTESIAN_POINT('Ctrl Pts',(-1.79185815610802,1.,-0.760469555880425));
#33346=CARTESIAN_POINT('Ctrl Pts',(-1.79768986997735,1.,-0.761229695230359));
#33347=CARTESIAN_POINT('Ctrl Pts',(-1.80351583877334,1.,-0.761915336443515));
#33348=CARTESIAN_POINT('Ctrl Pts',(-1.80938551463989,1.,-0.762546129464036));
#33349=CARTESIAN_POINT('Ctrl Pts',(-1.81532118405566,1.,-0.763132003836783));
#33350=CARTESIAN_POINT('Ctrl Pts',(-1.82131873145297,1.,-0.763673465462854));
#33351=CARTESIAN_POINT('Ctrl Pts',(-1.8273599120008,1.,-0.764165902606055));
#33352=CARTESIAN_POINT('Ctrl Pts',(-1.8334207722714,1.,-0.764602549687845));
#33353=CARTESIAN_POINT('Ctrl Pts',(-1.83948181064823,1.,-0.764978057881687));
#33354=CARTESIAN_POINT('Ctrl Pts',(-1.8455369887591,1.,-0.765291664861971));
#33355=CARTESIAN_POINT('Ctrl Pts',(-1.85158945130054,1.,-0.765545710619023));
#33356=CARTESIAN_POINT('Ctrl Pts',(-1.85764741390391,1.,-0.765744212909305));
#33357=CARTESIAN_POINT('Ctrl Pts',(-1.86372027063314,1.,-0.765891519092557));
#33358=CARTESIAN_POINT('Ctrl Pts',(-1.86981398314345,1.,-0.765990708546111));
#33359=CARTESIAN_POINT('Ctrl Pts',(-1.87592888967886,1.,-0.766042837036759));
#33360=CARTESIAN_POINT('Ctrl Pts',(-1.88206215302561,1.,-0.766047794851868));
#33361=CARTESIAN_POINT('Ctrl Pts',(-1.88820926433409,1.,-0.76600483706209));
#33362=CARTESIAN_POINT('Ctrl Pts',(-1.89436577771389,1.,-0.765913193856979));
#33363=CARTESIAN_POINT('Ctrl Pts',(-1.90052930393599,1.,-0.765772772593395));
#33364=CARTESIAN_POINT('Ctrl Pts',(-1.90669961402362,1.,-0.765584196937936));
#33365=CARTESIAN_POINT('Ctrl Pts',(-1.91287765805174,1.,-0.765348465884739));
#33366=CARTESIAN_POINT('Ctrl Pts',(-1.91906491634197,1.,-0.765066729667095));
#33367=CARTESIAN_POINT('Ctrl Pts',(-1.92526263537041,1.,-0.764740025488189));
#33368=CARTESIAN_POINT('Ctrl Pts',(-1.93147105496367,1.,-0.764369010673889));
#33369=CARTESIAN_POINT('Ctrl Pts',(-1.93768964875867,1.,-0.763954049121393));
#33370=CARTESIAN_POINT('Ctrl Pts',(-1.94391746617626,1.,-0.76349533353858));
#33371=CARTESIAN_POINT('Ctrl Pts',(-1.95015342590025,1.,-0.762992990878774));
#33372=CARTESIAN_POINT('Ctrl Pts',(-1.95639665309893,1.,-0.762447203806263));
#33373=CARTESIAN_POINT('Ctrl Pts',(-1.96264672744229,1.,-0.761858300014575));
#33374=CARTESIAN_POINT('Ctrl Pts',(-1.96890351582545,1.,-0.761226690483986));
#33375=CARTESIAN_POINT('Ctrl Pts',(-1.97516705321521,1.,-0.760552825409855));
#33376=CARTESIAN_POINT('Ctrl Pts',(-1.98143741418156,1.,-0.759837147452135));
#33377=CARTESIAN_POINT('Ctrl Pts',(-1.98771456680806,1.,-0.759080037802242));
#33378=CARTESIAN_POINT('Ctrl Pts',(-1.9939983109871,1.,-0.758281796766377));
#33379=CARTESIAN_POINT('Ctrl Pts',(-2.00028834739072,1.,-0.757442676862341));
#33380=CARTESIAN_POINT('Ctrl Pts',(-2.00658431587682,1.,-0.756562904646496));
#33381=CARTESIAN_POINT('Ctrl Pts',(-2.01288584328149,1.,-0.7556427049581));
#33382=CARTESIAN_POINT('Ctrl Pts',(-2.01919259406003,1.,-0.75468233072352));
#33383=CARTESIAN_POINT('Ctrl Pts',(-2.02550428623587,1.,-0.753682061113765));
#33384=CARTESIAN_POINT('Ctrl Pts',(-2.03182068456467,1.,-0.752642180488104));
#33385=CARTESIAN_POINT('Ctrl Pts',(-2.03814160092173,1.,-0.751562963361383));
#33386=CARTESIAN_POINT('Ctrl Pts',(-2.04446689147754,1.,-0.750444657874758));
#33387=CARTESIAN_POINT('Ctrl Pts',(-2.05079645591606,1.,-0.749287468663053));
#33388=CARTESIAN_POINT('Ctrl Pts',(-2.05713023030263,1.,-0.748091554181101));
#33389=CARTESIAN_POINT('Ctrl Pts',(-2.06220058927162,1.,-0.747103932785504));
#33390=CARTESIAN_POINT('Ctrl Pts',(-2.06600523016401,1.,-0.746345871542695));
#33391=CARTESIAN_POINT('Ctrl Pts',(-2.06854248895575,1.,-0.74583279137781));
#33392=CARTESIAN_POINT('Ctrl Pts',(-2.0698113262342,1.,-0.745574324794401));
#33393=CARTESIAN_POINT('',(-1.60662857109684,0.,-0.693717979106306));
#33394=CARTESIAN_POINT('Origin',(0.,0.,0.));
#33395=CARTESIAN_POINT('',(-1.5055822144029,1.,-0.892032620296855));
#33396=CARTESIAN_POINT('Origin',(0.,1.,0.));
#33397=CARTESIAN_POINT('',(-1.5055822144029,0.,-0.892032620296855));
#33398=CARTESIAN_POINT('Ctrl Pts',(-1.81978687191668,-1.,-1.23627494547115));
#33399=CARTESIAN_POINT('Ctrl Pts',(-1.81978687191668,1.,-1.23627494547115));
#33400=CARTESIAN_POINT('Ctrl Pts',(-1.81925017193666,-1.,-1.23509651170476));
#33401=CARTESIAN_POINT('Ctrl Pts',(-1.81925017193666,1.,-1.23509651170476));
#33402=CARTESIAN_POINT('Ctrl Pts',(-1.81817389921279,-1.,-1.2327422452705));
#33403=CARTESIAN_POINT('Ctrl Pts',(-1.81817389921279,1.,-1.2327422452705));
#33404=CARTESIAN_POINT('Ctrl Pts',(-1.8165508718364,-1.,-1.2292186489137));
#33405=CARTESIAN_POINT('Ctrl Pts',(-1.8165508718364,1.,-1.2292186489137));
#33406=CARTESIAN_POINT('Ctrl Pts',(-1.81436959210434,-1.,-1.2245361330495));
#33407=CARTESIAN_POINT('Ctrl Pts',(-1.81436959210434,1.,-1.2245361330495));
#33408=CARTESIAN_POINT('Ctrl Pts',(-1.81161420806656,-1.,-1.21870906103557));
#33409=CARTESIAN_POINT('Ctrl Pts',(-1.81161420806656,1.,-1.21870906103557));
#33410=CARTESIAN_POINT('Ctrl Pts',(-1.80882996917129,-1.,-1.21290815708314));
#33411=CARTESIAN_POINT('Ctrl Pts',(-1.80882996917129,1.,-1.21290815708314));
#33412=CARTESIAN_POINT('Ctrl Pts',(-1.80601678480707,-1.,-1.20713356605475));
#33413=CARTESIAN_POINT('Ctrl Pts',(-1.80601678480707,1.,-1.20713356605475));
#33414=CARTESIAN_POINT('Ctrl Pts',(-1.80317454838603,-1.,-1.20138548938974));
#33415=CARTESIAN_POINT('Ctrl Pts',(-1.80317454838603,1.,-1.20138548938974));
#33416=CARTESIAN_POINT('Ctrl Pts',(-1.80030314369879,-1.,-1.19566418930242));
#33417=CARTESIAN_POINT('Ctrl Pts',(-1.80030314369879,1.,-1.19566418930242));
#33418=CARTESIAN_POINT('Ctrl Pts',(-1.79740245923478,-1.,-1.18996997934445));
#33419=CARTESIAN_POINT('Ctrl Pts',(-1.79740245923478,1.,-1.18996997934445));
#33420=CARTESIAN_POINT('Ctrl Pts',(-1.79447240321515,-1.,-1.18430321697432));
#33421=CARTESIAN_POINT('Ctrl Pts',(-1.79447240321515,1.,-1.18430321697432));
#33422=CARTESIAN_POINT('Ctrl Pts',(-1.79151291552689,-1.,-1.17866429440809));
#33423=CARTESIAN_POINT('Ctrl Pts',(-1.79151291552689,1.,-1.17866429440809));
#33424=CARTESIAN_POINT('Ctrl Pts',(-1.78852398877616,-1.,-1.17305363177328));
#33425=CARTESIAN_POINT('Ctrl Pts',(-1.78852398877616,1.,-1.17305363177328));
#33426=CARTESIAN_POINT('Ctrl Pts',(-1.78550566040443,-1.,-1.16747166312303));
#33427=CARTESIAN_POINT('Ctrl Pts',(-1.78550566040443,1.,-1.16747166312303));
#33428=CARTESIAN_POINT('Ctrl Pts',(-1.78245795881009,-1.,-1.16191881298499));
#33429=CARTESIAN_POINT('Ctrl Pts',(-1.78245795881009,1.,-1.16191881298499));
#33430=CARTESIAN_POINT('Ctrl Pts',(-1.77938085564275,-1.,-1.15639547194698));
#33431=CARTESIAN_POINT('Ctrl Pts',(-1.77938085564275,1.,-1.15639547194698));
#33432=CARTESIAN_POINT('Ctrl Pts',(-1.7762742255701,-1.,-1.15090197841515));
#33433=CARTESIAN_POINT('Ctrl Pts',(-1.7762742255701,1.,-1.15090197841515));
#33434=CARTESIAN_POINT('Ctrl Pts',(-1.77313777896194,-1.,-1.1454385822692));
#33435=CARTESIAN_POINT('Ctrl Pts',(-1.77313777896194,1.,-1.1454385822692));
#33436=CARTESIAN_POINT('Ctrl Pts',(-1.76997111386769,-1.,-1.14000548336975));
#33437=CARTESIAN_POINT('Ctrl Pts',(-1.76997111386769,1.,-1.14000548336975));
#33438=CARTESIAN_POINT('Ctrl Pts',(-1.76677384551862,-1.,-1.1346029180462));
#33439=CARTESIAN_POINT('Ctrl Pts',(-1.76677384551862,1.,-1.1346029180462));
#33440=CARTESIAN_POINT('Ctrl Pts',(-1.7635457196617,-1.,-1.12923123555075));
#33441=CARTESIAN_POINT('Ctrl Pts',(-1.7635457196617,1.,-1.12923123555075));
#33442=CARTESIAN_POINT('Ctrl Pts',(-1.76028671825096,-1.,-1.12389096855086));
#33443=CARTESIAN_POINT('Ctrl Pts',(-1.76028671825096,1.,-1.12389096855086));
#33444=CARTESIAN_POINT('Ctrl Pts',(-1.75699720772105,-1.,-1.11858293216763));
#33445=CARTESIAN_POINT('Ctrl Pts',(-1.75699720772105,1.,-1.11858293216763));
#33446=CARTESIAN_POINT('Ctrl Pts',(-1.7536777209463,-1.,-1.11330807582551));
#33447=CARTESIAN_POINT('Ctrl Pts',(-1.7536777209463,1.,-1.11330807582551));
#33448=CARTESIAN_POINT('Ctrl Pts',(-1.7503286607592,-1.,-1.10806728183007));
#33449=CARTESIAN_POINT('Ctrl Pts',(-1.7503286607592,1.,-1.10806728183007));
#33450=CARTESIAN_POINT('Ctrl Pts',(-1.74695004214923,-1.,-1.10286118991143));
#33451=CARTESIAN_POINT('Ctrl Pts',(-1.74695004214923,1.,-1.10286118991143));
#33452=CARTESIAN_POINT('Ctrl Pts',(-1.74354119236208,-1.,-1.09768999241225));
#33453=CARTESIAN_POINT('Ctrl Pts',(-1.74354119236208,1.,-1.09768999241225));
#33454=CARTESIAN_POINT('Ctrl Pts',(-1.74010053962247,-1.,-1.09255329056493));
#33455=CARTESIAN_POINT('Ctrl Pts',(-1.74010053962247,1.,-1.09255329056493));
#33456=CARTESIAN_POINT('Ctrl Pts',(-1.73662628326091,-1.,-1.08745056285427));
#33457=CARTESIAN_POINT('Ctrl Pts',(-1.73662628326091,1.,-1.08745056285427));
#33458=CARTESIAN_POINT('Ctrl Pts',(-1.73311705663407,-1.,-1.08238162784749));
#33459=CARTESIAN_POINT('Ctrl Pts',(-1.73311705663407,1.,-1.08238162784749));
#33460=CARTESIAN_POINT('Ctrl Pts',(-1.72957248977424,-1.,-1.0773470373727));
#33461=CARTESIAN_POINT('Ctrl Pts',(-1.72957248977424,1.,-1.0773470373727));
#33462=CARTESIAN_POINT('Ctrl Pts',(-1.72599406198488,-1.,-1.07234866990252));
#33463=CARTESIAN_POINT('Ctrl Pts',(-1.72599406198488,1.,-1.07234866990252));
#33464=CARTESIAN_POINT('Ctrl Pts',(-1.72238500928453,-1.,-1.06738966975462));
#33465=CARTESIAN_POINT('Ctrl Pts',(-1.72238500928453,1.,-1.06738966975462));
#33466=CARTESIAN_POINT('Ctrl Pts',(-1.71874858456904,-1.,-1.06247324680647));
#33467=CARTESIAN_POINT('Ctrl Pts',(-1.71874858456904,1.,-1.06247324680647));
#33468=CARTESIAN_POINT('Ctrl Pts',(-1.7150865442702,-1.,-1.05760163192479));
#33469=CARTESIAN_POINT('Ctrl Pts',(-1.7150865442702,1.,-1.05760163192479));
#33470=CARTESIAN_POINT('Ctrl Pts',(-1.71139783543989,-1.,-1.05277517202855));
#33471=CARTESIAN_POINT('Ctrl Pts',(-1.71139783543989,1.,-1.05277517202855));
#33472=CARTESIAN_POINT('Ctrl Pts',(-1.70767646263649,-1.,-1.04799085404995));
#33473=CARTESIAN_POINT('Ctrl Pts',(-1.70767646263649,1.,-1.04799085404995));
#33474=CARTESIAN_POINT('Ctrl Pts',(-1.70391338707982,-1.,-1.04324363334554));
#33475=CARTESIAN_POINT('Ctrl Pts',(-1.70391338707982,1.,-1.04324363334554));
#33476=CARTESIAN_POINT('Ctrl Pts',(-1.70010052930962,-1.,-1.03852922490789));
#33477=CARTESIAN_POINT('Ctrl Pts',(-1.70010052930962,1.,-1.03852922490789));
#33478=CARTESIAN_POINT('Ctrl Pts',(-1.69623414782771,-1.,-1.03384646003588));
#33479=CARTESIAN_POINT('Ctrl Pts',(-1.69623414782771,1.,-1.03384646003588));
#33480=CARTESIAN_POINT('Ctrl Pts',(-1.69231840863458,-1.,-1.02919977579147));
#33481=CARTESIAN_POINT('Ctrl Pts',(-1.69231840863458,1.,-1.02919977579147));
#33482=CARTESIAN_POINT('Ctrl Pts',(-1.68836910178447,-1.,-1.02460180535255));
#33483=CARTESIAN_POINT('Ctrl Pts',(-1.68836910178447,1.,-1.02460180535255));
#33484=CARTESIAN_POINT('Ctrl Pts',(-1.68440578021706,-1.,-1.02006795074201));
#33485=CARTESIAN_POINT('Ctrl Pts',(-1.68440578021706,1.,-1.02006795074201));
#33486=CARTESIAN_POINT('Ctrl Pts',(-1.68044289894798,-1.,-1.01561026162773));
#33487=CARTESIAN_POINT('Ctrl Pts',(-1.68044289894798,1.,-1.01561026162773));
#33488=CARTESIAN_POINT('Ctrl Pts',(-1.67648246776464,-1.,-1.01123236493511));
#33489=CARTESIAN_POINT('Ctrl Pts',(-1.67648246776464,1.,-1.01123236493511));
#33490=CARTESIAN_POINT('Ctrl Pts',(-1.67250335383293,-1.,-1.00692206696414));
#33491=CARTESIAN_POINT('Ctrl Pts',(-1.67250335383293,1.,-1.00692206696414));
#33492=CARTESIAN_POINT('Ctrl Pts',(-1.66846059277303,-1.,-1.00265091003727));
#33493=CARTESIAN_POINT('Ctrl Pts',(-1.66846059277303,1.,-1.00265091003727));
#33494=CARTESIAN_POINT('Ctrl Pts',(-1.66430758030376,-1.,-0.998389654952758));
#33495=CARTESIAN_POINT('Ctrl Pts',(-1.66430758030376,1.,-0.998389654952758));
#33496=CARTESIAN_POINT('Ctrl Pts',(-1.66001553809947,-1.,-0.994121836661306));
#33497=CARTESIAN_POINT('Ctrl Pts',(-1.66001553809947,1.,-0.994121836661306));
#33498=CARTESIAN_POINT('Ctrl Pts',(-1.65559044289699,-1.,-0.989855627854165));
#33499=CARTESIAN_POINT('Ctrl Pts',(-1.65559044289699,1.,-0.989855627854165));
#33500=CARTESIAN_POINT('Ctrl Pts',(-1.65110016612638,-1.,-0.985642622920821));
#33501=CARTESIAN_POINT('Ctrl Pts',(-1.65110016612638,1.,-0.985642622920821));
#33502=CARTESIAN_POINT('Ctrl Pts',(-1.64665139190656,-1.,-0.981562530939489));
#33503=CARTESIAN_POINT('Ctrl Pts',(-1.64665139190656,1.,-0.981562530939489));
#33504=CARTESIAN_POINT('Ctrl Pts',(-1.64233990826687,-1.,-0.977689794119416));
#33505=CARTESIAN_POINT('Ctrl Pts',(-1.64233990826687,1.,-0.977689794119416));
#33506=CARTESIAN_POINT('Ctrl Pts',(-1.63820952658144,-1.,-0.974066058287418));
#33507=CARTESIAN_POINT('Ctrl Pts',(-1.63820952658144,1.,-0.974066058287418));
#33508=CARTESIAN_POINT('Ctrl Pts',(-1.63420665729798,-1.,-0.970669715997509));
#33509=CARTESIAN_POINT('Ctrl Pts',(-1.63420665729798,1.,-0.970669715997509));
#33510=CARTESIAN_POINT('Ctrl Pts',(-1.63013849959461,-1.,-0.967387853230345));
#33511=CARTESIAN_POINT('Ctrl Pts',(-1.63013849959461,1.,-0.967387853230345));
#33512=CARTESIAN_POINT('Ctrl Pts',(-1.62571930670187,-1.,-0.964046107040536));
#33513=CARTESIAN_POINT('Ctrl Pts',(-1.62571930670187,1.,-0.964046107040536));
#33514=CARTESIAN_POINT('Ctrl Pts',(-1.62061638140221,-1.,-0.960438326101729));
#33515=CARTESIAN_POINT('Ctrl Pts',(-1.62061638140221,1.,-0.960438326101729));
#33516=CARTESIAN_POINT('Ctrl Pts',(-1.61449324337085,-1.,-0.956354422920671));
#33517=CARTESIAN_POINT('Ctrl Pts',(-1.61449324337085,1.,-0.956354422920671));
#33518=CARTESIAN_POINT('Ctrl Pts',(-1.60706069896936,-1.,-0.951613284356035));
#33519=CARTESIAN_POINT('Ctrl Pts',(-1.60706069896936,1.,-0.951613284356035));
#33520=CARTESIAN_POINT('Ctrl Pts',(-1.59810042043673,-1.,-0.946078063315257));
#33521=CARTESIAN_POINT('Ctrl Pts',(-1.59810042043673,1.,-0.946078063315257));
#33522=CARTESIAN_POINT('Ctrl Pts',(-1.58744937487176,-1.,-0.939646377893399));
#33523=CARTESIAN_POINT('Ctrl Pts',(-1.58744937487176,1.,-0.939646377893399));
#33524=CARTESIAN_POINT('Ctrl Pts',(-1.57499388382243,-1.,-0.932246680108685));
#33525=CARTESIAN_POINT('Ctrl Pts',(-1.57499388382243,1.,-0.932246680108685));
#33526=CARTESIAN_POINT('Ctrl Pts',(-1.56065988578893,-1.,-0.923832188944341));
#33527=CARTESIAN_POINT('Ctrl Pts',(-1.56065988578893,1.,-0.923832188944341));
#33528=CARTESIAN_POINT('Ctrl Pts',(-1.54440491149498,-1.,-0.914375919026456));
#33529=CARTESIAN_POINT('Ctrl Pts',(-1.54440491149498,1.,-0.914375919026456));
#33530=CARTESIAN_POINT('Ctrl Pts',(-1.52984849887993,-1.,-0.905967409625651));
#33531=CARTESIAN_POINT('Ctrl Pts',(-1.52984849887993,1.,-0.905967409625651));
#33532=CARTESIAN_POINT('Ctrl Pts',(-1.51805569590094,-1.,-0.899185047483511));
#33533=CARTESIAN_POINT('Ctrl Pts',(-1.51805569590094,1.,-0.899185047483511));
#33534=CARTESIAN_POINT('Ctrl Pts',(-1.50980486806688,-1.,-0.894452006964543));
#33535=CARTESIAN_POINT('Ctrl Pts',(-1.50980486806688,1.,-0.894452006964543));
#33536=CARTESIAN_POINT('Ctrl Pts',(-1.5055822144029,-1.,-0.892032620296855));
#33537=CARTESIAN_POINT('Ctrl Pts',(-1.5055822144029,1.,-0.892032620296855));
#33538=CARTESIAN_POINT('',(-1.81978687191668,1.,-1.23627494547115));
#33539=CARTESIAN_POINT('Ctrl Pts',(-1.81978687191668,1.,-1.23627494547115));
#33540=CARTESIAN_POINT('Ctrl Pts',(-1.81925017193666,1.,-1.23509651170476));
#33541=CARTESIAN_POINT('Ctrl Pts',(-1.81817389921279,1.,-1.2327422452705));
#33542=CARTESIAN_POINT('Ctrl Pts',(-1.8165508718364,1.,-1.2292186489137));
#33543=CARTESIAN_POINT('Ctrl Pts',(-1.81436959210434,1.,-1.2245361330495));
#33544=CARTESIAN_POINT('Ctrl Pts',(-1.81161420806656,1.,-1.21870906103557));
#33545=CARTESIAN_POINT('Ctrl Pts',(-1.80882996917129,1.,-1.21290815708314));
#33546=CARTESIAN_POINT('Ctrl Pts',(-1.80601678480707,1.,-1.20713356605475));
#33547=CARTESIAN_POINT('Ctrl Pts',(-1.80317454838603,1.,-1.20138548938974));
#33548=CARTESIAN_POINT('Ctrl Pts',(-1.80030314369879,1.,-1.19566418930242));
#33549=CARTESIAN_POINT('Ctrl Pts',(-1.79740245923478,1.,-1.18996997934445));
#33550=CARTESIAN_POINT('Ctrl Pts',(-1.79447240321515,1.,-1.18430321697432));
#33551=CARTESIAN_POINT('Ctrl Pts',(-1.79151291552689,1.,-1.17866429440809));
#33552=CARTESIAN_POINT('Ctrl Pts',(-1.78852398877616,1.,-1.17305363177328));
#33553=CARTESIAN_POINT('Ctrl Pts',(-1.78550566040443,1.,-1.16747166312303));
#33554=CARTESIAN_POINT('Ctrl Pts',(-1.78245795881009,1.,-1.16191881298499));
#33555=CARTESIAN_POINT('Ctrl Pts',(-1.77938085564275,1.,-1.15639547194698));
#33556=CARTESIAN_POINT('Ctrl Pts',(-1.7762742255701,1.,-1.15090197841515));
#33557=CARTESIAN_POINT('Ctrl Pts',(-1.77313777896194,1.,-1.1454385822692));
#33558=CARTESIAN_POINT('Ctrl Pts',(-1.76997111386769,1.,-1.14000548336975));
#33559=CARTESIAN_POINT('Ctrl Pts',(-1.76677384551862,1.,-1.1346029180462));
#33560=CARTESIAN_POINT('Ctrl Pts',(-1.7635457196617,1.,-1.12923123555075));
#33561=CARTESIAN_POINT('Ctrl Pts',(-1.76028671825096,1.,-1.12389096855086));
#33562=CARTESIAN_POINT('Ctrl Pts',(-1.75699720772105,1.,-1.11858293216763));
#33563=CARTESIAN_POINT('Ctrl Pts',(-1.7536777209463,1.,-1.11330807582551));
#33564=CARTESIAN_POINT('Ctrl Pts',(-1.7503286607592,1.,-1.10806728183007));
#33565=CARTESIAN_POINT('Ctrl Pts',(-1.74695004214923,1.,-1.10286118991143));
#33566=CARTESIAN_POINT('Ctrl Pts',(-1.74354119236208,1.,-1.09768999241225));
#33567=CARTESIAN_POINT('Ctrl Pts',(-1.74010053962247,1.,-1.09255329056493));
#33568=CARTESIAN_POINT('Ctrl Pts',(-1.73662628326091,1.,-1.08745056285427));
#33569=CARTESIAN_POINT('Ctrl Pts',(-1.73311705663407,1.,-1.08238162784749));
#33570=CARTESIAN_POINT('Ctrl Pts',(-1.72957248977424,1.,-1.0773470373727));
#33571=CARTESIAN_POINT('Ctrl Pts',(-1.72599406198488,1.,-1.07234866990252));
#33572=CARTESIAN_POINT('Ctrl Pts',(-1.72238500928453,1.,-1.06738966975462));
#33573=CARTESIAN_POINT('Ctrl Pts',(-1.71874858456904,1.,-1.06247324680647));
#33574=CARTESIAN_POINT('Ctrl Pts',(-1.7150865442702,1.,-1.05760163192479));
#33575=CARTESIAN_POINT('Ctrl Pts',(-1.71139783543989,1.,-1.05277517202855));
#33576=CARTESIAN_POINT('Ctrl Pts',(-1.70767646263649,1.,-1.04799085404995));
#33577=CARTESIAN_POINT('Ctrl Pts',(-1.70391338707982,1.,-1.04324363334554));
#33578=CARTESIAN_POINT('Ctrl Pts',(-1.70010052930962,1.,-1.03852922490789));
#33579=CARTESIAN_POINT('Ctrl Pts',(-1.69623414782771,1.,-1.03384646003588));
#33580=CARTESIAN_POINT('Ctrl Pts',(-1.69231840863458,1.,-1.02919977579147));
#33581=CARTESIAN_POINT('Ctrl Pts',(-1.68836910178447,1.,-1.02460180535255));
#33582=CARTESIAN_POINT('Ctrl Pts',(-1.68440578021706,1.,-1.02006795074201));
#33583=CARTESIAN_POINT('Ctrl Pts',(-1.68044289894798,1.,-1.01561026162773));
#33584=CARTESIAN_POINT('Ctrl Pts',(-1.67648246776464,1.,-1.01123236493511));
#33585=CARTESIAN_POINT('Ctrl Pts',(-1.67250335383293,1.,-1.00692206696414));
#33586=CARTESIAN_POINT('Ctrl Pts',(-1.66846059277303,1.,-1.00265091003727));
#33587=CARTESIAN_POINT('Ctrl Pts',(-1.66430758030376,1.,-0.998389654952758));
#33588=CARTESIAN_POINT('Ctrl Pts',(-1.66001553809947,1.,-0.994121836661306));
#33589=CARTESIAN_POINT('Ctrl Pts',(-1.65559044289699,1.,-0.989855627854165));
#33590=CARTESIAN_POINT('Ctrl Pts',(-1.65110016612638,1.,-0.985642622920821));
#33591=CARTESIAN_POINT('Ctrl Pts',(-1.64665139190656,1.,-0.981562530939489));
#33592=CARTESIAN_POINT('Ctrl Pts',(-1.64233990826687,1.,-0.977689794119416));
#33593=CARTESIAN_POINT('Ctrl Pts',(-1.63820952658144,1.,-0.974066058287418));
#33594=CARTESIAN_POINT('Ctrl Pts',(-1.63420665729798,1.,-0.970669715997509));
#33595=CARTESIAN_POINT('Ctrl Pts',(-1.63013849959461,1.,-0.967387853230345));
#33596=CARTESIAN_POINT('Ctrl Pts',(-1.62571930670187,1.,-0.964046107040536));
#33597=CARTESIAN_POINT('Ctrl Pts',(-1.62061638140221,1.,-0.960438326101729));
#33598=CARTESIAN_POINT('Ctrl Pts',(-1.61449324337085,1.,-0.956354422920671));
#33599=CARTESIAN_POINT('Ctrl Pts',(-1.60706069896936,1.,-0.951613284356035));
#33600=CARTESIAN_POINT('Ctrl Pts',(-1.59810042043673,1.,-0.946078063315257));
#33601=CARTESIAN_POINT('Ctrl Pts',(-1.58744937487176,1.,-0.939646377893399));
#33602=CARTESIAN_POINT('Ctrl Pts',(-1.57499388382243,1.,-0.932246680108685));
#33603=CARTESIAN_POINT('Ctrl Pts',(-1.56065988578893,1.,-0.923832188944341));
#33604=CARTESIAN_POINT('Ctrl Pts',(-1.54440491149498,1.,-0.914375919026456));
#33605=CARTESIAN_POINT('Ctrl Pts',(-1.52984849887993,1.,-0.905967409625651));
#33606=CARTESIAN_POINT('Ctrl Pts',(-1.51805569590094,1.,-0.899185047483511));
#33607=CARTESIAN_POINT('Ctrl Pts',(-1.50980486806688,1.,-0.894452006964543));
#33608=CARTESIAN_POINT('Ctrl Pts',(-1.5055822144029,1.,-0.892032620296855));
#33609=CARTESIAN_POINT('',(-1.81978687191668,0.,-1.23627494547115));
#33610=CARTESIAN_POINT('Origin',(-1.73811241238545,0.,-1.34869019493419));
#33611=CARTESIAN_POINT('',(-1.73811241238545,1.,-1.34869019493419));
#33612=CARTESIAN_POINT('',(-1.81978687191668,1.,-1.23627494547115));
#33613=CARTESIAN_POINT('',(-1.73811241238545,0.,-1.34869019493419));
#33614=CARTESIAN_POINT('Ctrl Pts',(-1.31362392696032,-1.,-1.15624053661742));
#33615=CARTESIAN_POINT('Ctrl Pts',(-1.31362392696032,1.,-1.15624053661742));
#33616=CARTESIAN_POINT('Ctrl Pts',(-1.31722977216397,-1.,-1.15950888730809));
#33617=CARTESIAN_POINT('Ctrl Pts',(-1.31722977216397,1.,-1.15950888730809));
#33618=CARTESIAN_POINT('Ctrl Pts',(-1.32428080721772,-1.,-1.16589330093588));
#33619=CARTESIAN_POINT('Ctrl Pts',(-1.32428080721772,1.,-1.16589330093588));
#33620=CARTESIAN_POINT('Ctrl Pts',(-1.33437539347008,-1.,-1.17501305789857));
#33621=CARTESIAN_POINT('Ctrl Pts',(-1.33437539347008,1.,-1.17501305789857));
#33622=CARTESIAN_POINT('Ctrl Pts',(-1.34687054001093,-1.,-1.18625865667441));
#33623=CARTESIAN_POINT('Ctrl Pts',(-1.34687054001093,1.,-1.18625865667441));
#33624=CARTESIAN_POINT('Ctrl Pts',(-1.36088705043885,-1.,-1.1987959077932));
#33625=CARTESIAN_POINT('Ctrl Pts',(-1.36088705043885,1.,-1.1987959077932));
#33626=CARTESIAN_POINT('Ctrl Pts',(-1.37331915607905,-1.,-1.20982812925645));
#33627=CARTESIAN_POINT('Ctrl Pts',(-1.37331915607905,1.,-1.20982812925645));
#33628=CARTESIAN_POINT('Ctrl Pts',(-1.38420564527715,-1.,-1.21938737280852));
#33629=CARTESIAN_POINT('Ctrl Pts',(-1.38420564527715,1.,-1.21938737280852));
#33630=CARTESIAN_POINT('Ctrl Pts',(-1.39361389568796,-1.,-1.22752961899387));
#33631=CARTESIAN_POINT('Ctrl Pts',(-1.39361389568796,1.,-1.22752961899387));
#33632=CARTESIAN_POINT('Ctrl Pts',(-1.40164708206106,-1.,-1.23434087290423));
#33633=CARTESIAN_POINT('Ctrl Pts',(-1.40164708206106,1.,-1.23434087290423));
#33634=CARTESIAN_POINT('Ctrl Pts',(-1.40845295531283,-1.,-1.23994455029534));
#33635=CARTESIAN_POINT('Ctrl Pts',(-1.40845295531283,1.,-1.23994455029534));
#33636=CARTESIAN_POINT('Ctrl Pts',(-1.41422913175179,-1.,-1.24450600513056));
#33637=CARTESIAN_POINT('Ctrl Pts',(-1.41422913175179,1.,-1.24450600513056));
#33638=CARTESIAN_POINT('Ctrl Pts',(-1.41923722596025,-1.,-1.24824430986571));
#33639=CARTESIAN_POINT('Ctrl Pts',(-1.41923722596025,1.,-1.24824430986571));
#33640=CARTESIAN_POINT('Ctrl Pts',(-1.42378102115575,-1.,-1.2514145557001));
#33641=CARTESIAN_POINT('Ctrl Pts',(-1.42378102115575,1.,-1.2514145557001));
#33642=CARTESIAN_POINT('Ctrl Pts',(-1.42815938799387,-1.,-1.25426945222639));
#33643=CARTESIAN_POINT('Ctrl Pts',(-1.42815938799387,1.,-1.25426945222639));
#33644=CARTESIAN_POINT('Ctrl Pts',(-1.43262645609691,-1.,-1.25702687965755));
#33645=CARTESIAN_POINT('Ctrl Pts',(-1.43262645609691,1.,-1.25702687965755));
#33646=CARTESIAN_POINT('Ctrl Pts',(-1.43734919180848,-1.,-1.25983531012005));
#33647=CARTESIAN_POINT('Ctrl Pts',(-1.43734919180848,1.,-1.25983531012005));
#33648=CARTESIAN_POINT('Ctrl Pts',(-1.44236470511303,-1.,-1.26273903323859));
#33649=CARTESIAN_POINT('Ctrl Pts',(-1.44236470511303,1.,-1.26273903323859));
#33650=CARTESIAN_POINT('Ctrl Pts',(-1.44761985001662,-1.,-1.26570925118868));
#33651=CARTESIAN_POINT('Ctrl Pts',(-1.44761985001662,1.,-1.26570925118868));
#33652=CARTESIAN_POINT('Ctrl Pts',(-1.45301422764247,-1.,-1.2686778680489));
#33653=CARTESIAN_POINT('Ctrl Pts',(-1.45301422764247,1.,-1.2686778680489));
#33654=CARTESIAN_POINT('Ctrl Pts',(-1.45843906294697,-1.,-1.27156805265289));
#33655=CARTESIAN_POINT('Ctrl Pts',(-1.45843906294697,1.,-1.27156805265289));
#33656=CARTESIAN_POINT('Ctrl Pts',(-1.46382431332476,-1.,-1.27433119897822));
#33657=CARTESIAN_POINT('Ctrl Pts',(-1.46382431332476,1.,-1.27433119897822));
#33658=CARTESIAN_POINT('Ctrl Pts',(-1.46916035917133,-1.,-1.27696414831089));
#33659=CARTESIAN_POINT('Ctrl Pts',(-1.46916035917133,1.,-1.27696414831089));
#33660=CARTESIAN_POINT('Ctrl Pts',(-1.4744717526707,-1.,-1.2794891824849));
#33661=CARTESIAN_POINT('Ctrl Pts',(-1.4744717526707,1.,-1.2794891824849));
#33662=CARTESIAN_POINT('Ctrl Pts',(-1.47980070347095,-1.,-1.28194158939517));
#33663=CARTESIAN_POINT('Ctrl Pts',(-1.47980070347095,1.,-1.28194158939517));
#33664=CARTESIAN_POINT('Ctrl Pts',(-1.4851881711891,-1.,-1.28435533880201));
#33665=CARTESIAN_POINT('Ctrl Pts',(-1.4851881711891,1.,-1.28435533880201));
#33666=CARTESIAN_POINT('Ctrl Pts',(-1.4906522831278,-1.,-1.2867467611644));
#33667=CARTESIAN_POINT('Ctrl Pts',(-1.4906522831278,1.,-1.2867467611644));
#33668=CARTESIAN_POINT('Ctrl Pts',(-1.49618896881754,-1.,-1.28911506584254));
#33669=CARTESIAN_POINT('Ctrl Pts',(-1.49618896881754,1.,-1.28911506584254));
#33670=CARTESIAN_POINT('Ctrl Pts',(-1.50178230149776,-1.,-1.29145022885181));
#33671=CARTESIAN_POINT('Ctrl Pts',(-1.50178230149776,1.,-1.29145022885181));
#33672=CARTESIAN_POINT('Ctrl Pts',(-1.50741159078365,-1.,-1.29373841372842));
#33673=CARTESIAN_POINT('Ctrl Pts',(-1.50741159078365,1.,-1.29373841372842));
#33674=CARTESIAN_POINT('Ctrl Pts',(-1.51305994241402,-1.,-1.29596850710509));
#33675=CARTESIAN_POINT('Ctrl Pts',(-1.51305994241402,1.,-1.29596850710509));
#33676=CARTESIAN_POINT('Ctrl Pts',(-1.51872184912724,-1.,-1.29813791800747));
#33677=CARTESIAN_POINT('Ctrl Pts',(-1.51872184912724,1.,-1.29813791800747));
#33678=CARTESIAN_POINT('Ctrl Pts',(-1.52439957861062,-1.,-1.30024984366328));
#33679=CARTESIAN_POINT('Ctrl Pts',(-1.52439957861062,1.,-1.30024984366328));
#33680=CARTESIAN_POINT('Ctrl Pts',(-1.53009970283891,-1.,-1.30231064395568));
#33681=CARTESIAN_POINT('Ctrl Pts',(-1.53009970283891,1.,-1.30231064395568));
#33682=CARTESIAN_POINT('Ctrl Pts',(-1.53582981268977,-1.,-1.30432735639489));
#33683=CARTESIAN_POINT('Ctrl Pts',(-1.53582981268977,1.,-1.30432735639489));
#33684=CARTESIAN_POINT('Ctrl Pts',(-1.54159462645432,-1.,-1.30630475189556));
#33685=CARTESIAN_POINT('Ctrl Pts',(-1.54159462645432,1.,-1.30630475189556));
#33686=CARTESIAN_POINT('Ctrl Pts',(-1.54739413957185,-1.,-1.30824393907473));
#33687=CARTESIAN_POINT('Ctrl Pts',(-1.54739413957185,1.,-1.30824393907473));
#33688=CARTESIAN_POINT('Ctrl Pts',(-1.55322568759481,-1.,-1.31014393684222));
#33689=CARTESIAN_POINT('Ctrl Pts',(-1.55322568759481,1.,-1.31014393684222));
#33690=CARTESIAN_POINT('Ctrl Pts',(-1.55908521254821,-1.,-1.31200264341696));
#33691=CARTESIAN_POINT('Ctrl Pts',(-1.55908521254821,1.,-1.31200264341696));
#33692=CARTESIAN_POINT('Ctrl Pts',(-1.56496872402353,-1.,-1.31381795281002));
#33693=CARTESIAN_POINT('Ctrl Pts',(-1.56496872402353,1.,-1.31381795281002));
#33694=CARTESIAN_POINT('Ctrl Pts',(-1.57087397835723,-1.,-1.31558903860016));
#33695=CARTESIAN_POINT('Ctrl Pts',(-1.57087397835723,1.,-1.31558903860016));
#33696=CARTESIAN_POINT('Ctrl Pts',(-1.5768005650559,-1.,-1.31731642317187));
#33697=CARTESIAN_POINT('Ctrl Pts',(-1.5768005650559,1.,-1.31731642317187));
#33698=CARTESIAN_POINT('Ctrl Pts',(-1.58274907898834,-1.,-1.31900135021432));
#33699=CARTESIAN_POINT('Ctrl Pts',(-1.58274907898834,1.,-1.31900135021432));
#33700=CARTESIAN_POINT('Ctrl Pts',(-1.58872057258245,-1.,-1.32064537110892));
#33701=CARTESIAN_POINT('Ctrl Pts',(-1.58872057258245,1.,-1.32064537110892));
#33702=CARTESIAN_POINT('Ctrl Pts',(-1.59471591079403,-1.,-1.32224985747682));
#33703=CARTESIAN_POINT('Ctrl Pts',(-1.59471591079403,1.,-1.32224985747682));
#33704=CARTESIAN_POINT('Ctrl Pts',(-1.60073511858687,-1.,-1.32381550858256));
#33705=CARTESIAN_POINT('Ctrl Pts',(-1.60073511858687,1.,-1.32381550858256));
#33706=CARTESIAN_POINT('Ctrl Pts',(-1.60677758290954,-1.,-1.32534250785782));
#33707=CARTESIAN_POINT('Ctrl Pts',(-1.60677758290954,1.,-1.32534250785782));
#33708=CARTESIAN_POINT('Ctrl Pts',(-1.6128423401575,-1.,-1.32683074483356));
#33709=CARTESIAN_POINT('Ctrl Pts',(-1.6128423401575,1.,-1.32683074483356));
#33710=CARTESIAN_POINT('Ctrl Pts',(-1.61892832270724,-1.,-1.32828000610449));
#33711=CARTESIAN_POINT('Ctrl Pts',(-1.61892832270724,1.,-1.32828000610449));
#33712=CARTESIAN_POINT('Ctrl Pts',(-1.62503464209797,-1.,-1.3296901950568));
#33713=CARTESIAN_POINT('Ctrl Pts',(-1.62503464209797,1.,-1.3296901950568));
#33714=CARTESIAN_POINT('Ctrl Pts',(-1.63116079730923,-1.,-1.33106149345645));
#33715=CARTESIAN_POINT('Ctrl Pts',(-1.63116079730923,1.,-1.33106149345645));
#33716=CARTESIAN_POINT('Ctrl Pts',(-1.63730653475089,-1.,-1.33239425103724));
#33717=CARTESIAN_POINT('Ctrl Pts',(-1.63730653475089,1.,-1.33239425103724));
#33718=CARTESIAN_POINT('Ctrl Pts',(-1.6434717485603,-1.,-1.33368890676572));
#33719=CARTESIAN_POINT('Ctrl Pts',(-1.6434717485603,1.,-1.33368890676572));
#33720=CARTESIAN_POINT('Ctrl Pts',(-1.6496563728683,-1.,-1.33494590467993));
#33721=CARTESIAN_POINT('Ctrl Pts',(-1.6496563728683,1.,-1.33494590467993));
#33722=CARTESIAN_POINT('Ctrl Pts',(-1.65586025952593,-1.,-1.33616559745172));
#33723=CARTESIAN_POINT('Ctrl Pts',(-1.65586025952593,1.,-1.33616559745172));
#33724=CARTESIAN_POINT('Ctrl Pts',(-1.66208312541983,-1.,-1.33734820885262));
#33725=CARTESIAN_POINT('Ctrl Pts',(-1.66208312541983,1.,-1.33734820885262));
#33726=CARTESIAN_POINT('Ctrl Pts',(-1.66832460783989,-1.,-1.33849388654388));
#33727=CARTESIAN_POINT('Ctrl Pts',(-1.66832460783989,1.,-1.33849388654388));
#33728=CARTESIAN_POINT('Ctrl Pts',(-1.67458429426086,-1.,-1.3396027347034));
#33729=CARTESIAN_POINT('Ctrl Pts',(-1.67458429426086,1.,-1.3396027347034));
#33730=CARTESIAN_POINT('Ctrl Pts',(-1.68086176030362,-1.,-1.34067485185203));
#33731=CARTESIAN_POINT('Ctrl Pts',(-1.68086176030362,1.,-1.34067485185203));
#33732=CARTESIAN_POINT('Ctrl Pts',(-1.68715660868764,-1.,-1.341710374848));
#33733=CARTESIAN_POINT('Ctrl Pts',(-1.68715660868764,1.,-1.341710374848));
#33734=CARTESIAN_POINT('Ctrl Pts',(-1.6934684849687,-1.,-1.34270948206319));
#33735=CARTESIAN_POINT('Ctrl Pts',(-1.6934684849687,1.,-1.34270948206319));
#33736=CARTESIAN_POINT('Ctrl Pts',(-1.69979707754427,-1.,-1.34367237124483));
#33737=CARTESIAN_POINT('Ctrl Pts',(-1.69979707754427,1.,-1.34367237124483));
#33738=CARTESIAN_POINT('Ctrl Pts',(-1.70614212266738,-1.,-1.34459924533831));
#33739=CARTESIAN_POINT('Ctrl Pts',(-1.70614212266738,1.,-1.34459924533831));
#33740=CARTESIAN_POINT('Ctrl Pts',(-1.71250340686822,-1.,-1.34549029589416));
#33741=CARTESIAN_POINT('Ctrl Pts',(-1.71250340686822,1.,-1.34549029589416));
#33742=CARTESIAN_POINT('Ctrl Pts',(-1.7188807715049,-1.,-1.34634568653227));
#33743=CARTESIAN_POINT('Ctrl Pts',(-1.7188807715049,1.,-1.34634568653227));
#33744=CARTESIAN_POINT('Ctrl Pts',(-1.72527410680674,-1.,-1.34716554819527));
#33745=CARTESIAN_POINT('Ctrl Pts',(-1.72527410680674,1.,-1.34716554819527));
#33746=CARTESIAN_POINT('Ctrl Pts',(-1.7304014965394,-1.,-1.34779309152035));
#33747=CARTESIAN_POINT('Ctrl Pts',(-1.7304014965394,1.,-1.34779309152035));
#33748=CARTESIAN_POINT('Ctrl Pts',(-1.73425417885907,-1.,-1.34824783112887));
#33749=CARTESIAN_POINT('Ctrl Pts',(-1.73425417885907,1.,-1.34824783112887));
#33750=CARTESIAN_POINT('Ctrl Pts',(-1.73682580585691,-1.,-1.34854391898045));
#33751=CARTESIAN_POINT('Ctrl Pts',(-1.73682580585691,1.,-1.34854391898045));
#33752=CARTESIAN_POINT('Ctrl Pts',(-1.73811241238545,-1.,-1.34869019493419));
#33753=CARTESIAN_POINT('Ctrl Pts',(-1.73811241238545,1.,-1.34869019493419));
#33754=CARTESIAN_POINT('',(-1.31362392696032,1.,-1.15624053661742));
#33755=CARTESIAN_POINT('Ctrl Pts',(-1.31362392696032,1.,-1.15624053661742));
#33756=CARTESIAN_POINT('Ctrl Pts',(-1.31722977216397,1.,-1.15950888730809));
#33757=CARTESIAN_POINT('Ctrl Pts',(-1.32428080721772,1.,-1.16589330093588));
#33758=CARTESIAN_POINT('Ctrl Pts',(-1.33437539347008,1.,-1.17501305789857));
#33759=CARTESIAN_POINT('Ctrl Pts',(-1.34687054001093,1.,-1.18625865667441));
#33760=CARTESIAN_POINT('Ctrl Pts',(-1.36088705043885,1.,-1.1987959077932));
#33761=CARTESIAN_POINT('Ctrl Pts',(-1.37331915607905,1.,-1.20982812925645));
#33762=CARTESIAN_POINT('Ctrl Pts',(-1.38420564527715,1.,-1.21938737280852));
#33763=CARTESIAN_POINT('Ctrl Pts',(-1.39361389568796,1.,-1.22752961899387));
#33764=CARTESIAN_POINT('Ctrl Pts',(-1.40164708206106,1.,-1.23434087290423));
#33765=CARTESIAN_POINT('Ctrl Pts',(-1.40845295531283,1.,-1.23994455029534));
#33766=CARTESIAN_POINT('Ctrl Pts',(-1.41422913175179,1.,-1.24450600513056));
#33767=CARTESIAN_POINT('Ctrl Pts',(-1.41923722596025,1.,-1.24824430986571));
#33768=CARTESIAN_POINT('Ctrl Pts',(-1.42378102115575,1.,-1.2514145557001));
#33769=CARTESIAN_POINT('Ctrl Pts',(-1.42815938799387,1.,-1.25426945222639));
#33770=CARTESIAN_POINT('Ctrl Pts',(-1.43262645609691,1.,-1.25702687965755));
#33771=CARTESIAN_POINT('Ctrl Pts',(-1.43734919180848,1.,-1.25983531012005));
#33772=CARTESIAN_POINT('Ctrl Pts',(-1.44236470511303,1.,-1.26273903323859));
#33773=CARTESIAN_POINT('Ctrl Pts',(-1.44761985001662,1.,-1.26570925118868));
#33774=CARTESIAN_POINT('Ctrl Pts',(-1.45301422764247,1.,-1.2686778680489));
#33775=CARTESIAN_POINT('Ctrl Pts',(-1.45843906294697,1.,-1.27156805265289));
#33776=CARTESIAN_POINT('Ctrl Pts',(-1.46382431332476,1.,-1.27433119897822));
#33777=CARTESIAN_POINT('Ctrl Pts',(-1.46916035917133,1.,-1.27696414831089));
#33778=CARTESIAN_POINT('Ctrl Pts',(-1.4744717526707,1.,-1.2794891824849));
#33779=CARTESIAN_POINT('Ctrl Pts',(-1.47980070347095,1.,-1.28194158939517));
#33780=CARTESIAN_POINT('Ctrl Pts',(-1.4851881711891,1.,-1.28435533880201));
#33781=CARTESIAN_POINT('Ctrl Pts',(-1.4906522831278,1.,-1.2867467611644));
#33782=CARTESIAN_POINT('Ctrl Pts',(-1.49618896881754,1.,-1.28911506584254));
#33783=CARTESIAN_POINT('Ctrl Pts',(-1.50178230149776,1.,-1.29145022885181));
#33784=CARTESIAN_POINT('Ctrl Pts',(-1.50741159078365,1.,-1.29373841372842));
#33785=CARTESIAN_POINT('Ctrl Pts',(-1.51305994241402,1.,-1.29596850710509));
#33786=CARTESIAN_POINT('Ctrl Pts',(-1.51872184912724,1.,-1.29813791800747));
#33787=CARTESIAN_POINT('Ctrl Pts',(-1.52439957861062,1.,-1.30024984366328));
#33788=CARTESIAN_POINT('Ctrl Pts',(-1.53009970283891,1.,-1.30231064395568));
#33789=CARTESIAN_POINT('Ctrl Pts',(-1.53582981268977,1.,-1.30432735639489));
#33790=CARTESIAN_POINT('Ctrl Pts',(-1.54159462645432,1.,-1.30630475189556));
#33791=CARTESIAN_POINT('Ctrl Pts',(-1.54739413957185,1.,-1.30824393907473));
#33792=CARTESIAN_POINT('Ctrl Pts',(-1.55322568759481,1.,-1.31014393684222));
#33793=CARTESIAN_POINT('Ctrl Pts',(-1.55908521254821,1.,-1.31200264341696));
#33794=CARTESIAN_POINT('Ctrl Pts',(-1.56496872402353,1.,-1.31381795281002));
#33795=CARTESIAN_POINT('Ctrl Pts',(-1.57087397835723,1.,-1.31558903860016));
#33796=CARTESIAN_POINT('Ctrl Pts',(-1.5768005650559,1.,-1.31731642317187));
#33797=CARTESIAN_POINT('Ctrl Pts',(-1.58274907898834,1.,-1.31900135021432));
#33798=CARTESIAN_POINT('Ctrl Pts',(-1.58872057258245,1.,-1.32064537110892));
#33799=CARTESIAN_POINT('Ctrl Pts',(-1.59471591079403,1.,-1.32224985747682));
#33800=CARTESIAN_POINT('Ctrl Pts',(-1.60073511858687,1.,-1.32381550858256));
#33801=CARTESIAN_POINT('Ctrl Pts',(-1.60677758290954,1.,-1.32534250785782));
#33802=CARTESIAN_POINT('Ctrl Pts',(-1.6128423401575,1.,-1.32683074483356));
#33803=CARTESIAN_POINT('Ctrl Pts',(-1.61892832270724,1.,-1.32828000610449));
#33804=CARTESIAN_POINT('Ctrl Pts',(-1.62503464209797,1.,-1.3296901950568));
#33805=CARTESIAN_POINT('Ctrl Pts',(-1.63116079730923,1.,-1.33106149345645));
#33806=CARTESIAN_POINT('Ctrl Pts',(-1.63730653475089,1.,-1.33239425103724));
#33807=CARTESIAN_POINT('Ctrl Pts',(-1.6434717485603,1.,-1.33368890676572));
#33808=CARTESIAN_POINT('Ctrl Pts',(-1.6496563728683,1.,-1.33494590467993));
#33809=CARTESIAN_POINT('Ctrl Pts',(-1.65586025952593,1.,-1.33616559745172));
#33810=CARTESIAN_POINT('Ctrl Pts',(-1.66208312541983,1.,-1.33734820885262));
#33811=CARTESIAN_POINT('Ctrl Pts',(-1.66832460783989,1.,-1.33849388654388));
#33812=CARTESIAN_POINT('Ctrl Pts',(-1.67458429426086,1.,-1.3396027347034));
#33813=CARTESIAN_POINT('Ctrl Pts',(-1.68086176030362,1.,-1.34067485185203));
#33814=CARTESIAN_POINT('Ctrl Pts',(-1.68715660868764,1.,-1.341710374848));
#33815=CARTESIAN_POINT('Ctrl Pts',(-1.6934684849687,1.,-1.34270948206319));
#33816=CARTESIAN_POINT('Ctrl Pts',(-1.69979707754427,1.,-1.34367237124483));
#33817=CARTESIAN_POINT('Ctrl Pts',(-1.70614212266738,1.,-1.34459924533831));
#33818=CARTESIAN_POINT('Ctrl Pts',(-1.71250340686822,1.,-1.34549029589416));
#33819=CARTESIAN_POINT('Ctrl Pts',(-1.7188807715049,1.,-1.34634568653227));
#33820=CARTESIAN_POINT('Ctrl Pts',(-1.72527410680674,1.,-1.34716554819527));
#33821=CARTESIAN_POINT('Ctrl Pts',(-1.7304014965394,1.,-1.34779309152035));
#33822=CARTESIAN_POINT('Ctrl Pts',(-1.73425417885907,1.,-1.34824783112887));
#33823=CARTESIAN_POINT('Ctrl Pts',(-1.73682580585691,1.,-1.34854391898045));
#33824=CARTESIAN_POINT('Ctrl Pts',(-1.73811241238545,1.,-1.34869019493419));
#33825=CARTESIAN_POINT('',(-1.31362392696032,0.,-1.15624053661742));
#33826=CARTESIAN_POINT('Origin',(0.,0.,0.));
#33827=CARTESIAN_POINT('',(-1.15624053661742,1.,-1.31362392696033));
#33828=CARTESIAN_POINT('Origin',(0.,1.,0.));
#33829=CARTESIAN_POINT('',(-1.15624053661742,0.,-1.31362392696033));
#33830=CARTESIAN_POINT('Ctrl Pts',(-1.34869019493419,-1.,-1.73811241238545));
#33831=CARTESIAN_POINT('Ctrl Pts',(-1.34869019493419,1.,-1.73811241238545));
#33832=CARTESIAN_POINT('Ctrl Pts',(-1.34854391898145,-1.,-1.73682580585819));
#33833=CARTESIAN_POINT('Ctrl Pts',(-1.34854391898145,1.,-1.73682580585819));
#33834=CARTESIAN_POINT('Ctrl Pts',(-1.34824783113158,-1.,-1.73425417886255));
#33835=CARTESIAN_POINT('Ctrl Pts',(-1.34824783113158,1.,-1.73425417886255));
#33836=CARTESIAN_POINT('Ctrl Pts',(-1.3477930915247,-1.,-1.73040149654497));
#33837=CARTESIAN_POINT('Ctrl Pts',(-1.3477930915247,1.,-1.73040149654497));
#33838=CARTESIAN_POINT('Ctrl Pts',(-1.34716554820013,-1.,-1.72527410681298));
#33839=CARTESIAN_POINT('Ctrl Pts',(-1.34716554820013,1.,-1.72527410681298));
#33840=CARTESIAN_POINT('Ctrl Pts',(-1.34634568653586,-1.,-1.7188807715095));
#33841=CARTESIAN_POINT('Ctrl Pts',(-1.34634568653586,1.,-1.7188807715095));
#33842=CARTESIAN_POINT('Ctrl Pts',(-1.34549029589563,-1.,-1.71250340687011));
#33843=CARTESIAN_POINT('Ctrl Pts',(-1.34549029589563,1.,-1.71250340687011));
#33844=CARTESIAN_POINT('Ctrl Pts',(-1.34459924533783,-1.,-1.70614212266676));
#33845=CARTESIAN_POINT('Ctrl Pts',(-1.34459924533783,1.,-1.70614212266676));
#33846=CARTESIAN_POINT('Ctrl Pts',(-1.34367237124322,-1.,-1.69979707754221));
#33847=CARTESIAN_POINT('Ctrl Pts',(-1.34367237124322,1.,-1.69979707754221));
#33848=CARTESIAN_POINT('Ctrl Pts',(-1.34270948206139,-1.,-1.6934684849664));
#33849=CARTESIAN_POINT('Ctrl Pts',(-1.34270948206139,1.,-1.6934684849664));
#33850=CARTESIAN_POINT('Ctrl Pts',(-1.34171037484673,-1.,-1.68715660868602));
#33851=CARTESIAN_POINT('Ctrl Pts',(-1.34171037484673,1.,-1.68715660868602));
#33852=CARTESIAN_POINT('Ctrl Pts',(-1.3406748518516,-1.,-1.68086176030308));
#33853=CARTESIAN_POINT('Ctrl Pts',(-1.3406748518516,1.,-1.68086176030308));
#33854=CARTESIAN_POINT('Ctrl Pts',(-1.33960273470372,-1.,-1.67458429426126));
#33855=CARTESIAN_POINT('Ctrl Pts',(-1.33960273470372,1.,-1.67458429426126));
#33856=CARTESIAN_POINT('Ctrl Pts',(-1.33849388654458,-1.,-1.66832460784078));
#33857=CARTESIAN_POINT('Ctrl Pts',(-1.33849388654458,1.,-1.66832460784078));
#33858=CARTESIAN_POINT('Ctrl Pts',(-1.33734820885331,-1.,-1.66208312542073));
#33859=CARTESIAN_POINT('Ctrl Pts',(-1.33734820885331,1.,-1.66208312542073));
#33860=CARTESIAN_POINT('Ctrl Pts',(-1.33616559745217,-1.,-1.65586025952651));
#33861=CARTESIAN_POINT('Ctrl Pts',(-1.33616559745217,1.,-1.65586025952651));
#33862=CARTESIAN_POINT('Ctrl Pts',(-1.33494590468003,-1.,-1.64965637286843));
#33863=CARTESIAN_POINT('Ctrl Pts',(-1.33494590468003,1.,-1.64965637286843));
#33864=CARTESIAN_POINT('Ctrl Pts',(-1.33368890676554,-1.,-1.64347174856007));
#33865=CARTESIAN_POINT('Ctrl Pts',(-1.33368890676554,1.,-1.64347174856007));
#33866=CARTESIAN_POINT('Ctrl Pts',(-1.33239425103694,-1.,-1.6373065347505));
#33867=CARTESIAN_POINT('Ctrl Pts',(-1.33239425103694,1.,-1.6373065347505));
#33868=CARTESIAN_POINT('Ctrl Pts',(-1.33106149345618,-1.,-1.63116079730887));
#33869=CARTESIAN_POINT('Ctrl Pts',(-1.33106149345618,1.,-1.63116079730887));
#33870=CARTESIAN_POINT('Ctrl Pts',(-1.32969019505665,-1.,-1.62503464209777));
#33871=CARTESIAN_POINT('Ctrl Pts',(-1.32969019505665,1.,-1.62503464209777));
#33872=CARTESIAN_POINT('Ctrl Pts',(-1.32828000610448,-1.,-1.61892832270723));
#33873=CARTESIAN_POINT('Ctrl Pts',(-1.32828000610448,1.,-1.61892832270723));
#33874=CARTESIAN_POINT('Ctrl Pts',(-1.32683074483365,-1.,-1.61284234015762));
#33875=CARTESIAN_POINT('Ctrl Pts',(-1.32683074483365,1.,-1.61284234015762));
#33876=CARTESIAN_POINT('Ctrl Pts',(-1.32534250785794,-1.,-1.6067775829097));
#33877=CARTESIAN_POINT('Ctrl Pts',(-1.32534250785794,1.,-1.6067775829097));
#33878=CARTESIAN_POINT('Ctrl Pts',(-1.32381550858266,-1.,-1.600735118587));
#33879=CARTESIAN_POINT('Ctrl Pts',(-1.32381550858266,1.,-1.600735118587));
#33880=CARTESIAN_POINT('Ctrl Pts',(-1.32224985747686,-1.,-1.59471591079408));
#33881=CARTESIAN_POINT('Ctrl Pts',(-1.32224985747686,1.,-1.59471591079408));
#33882=CARTESIAN_POINT('Ctrl Pts',(-1.32064537110891,-1.,-1.58872057258244));
#33883=CARTESIAN_POINT('Ctrl Pts',(-1.32064537110891,1.,-1.58872057258244));
#33884=CARTESIAN_POINT('Ctrl Pts',(-1.31900135021428,-1.,-1.58274907898829));
#33885=CARTESIAN_POINT('Ctrl Pts',(-1.31900135021428,1.,-1.58274907898829));
#33886=CARTESIAN_POINT('Ctrl Pts',(-1.31731642317183,-1.,-1.57680056505585));
#33887=CARTESIAN_POINT('Ctrl Pts',(-1.31731642317183,1.,-1.57680056505585));
#33888=CARTESIAN_POINT('Ctrl Pts',(-1.31558903860015,-1.,-1.57087397835721));
#33889=CARTESIAN_POINT('Ctrl Pts',(-1.31558903860015,1.,-1.57087397835721));
#33890=CARTESIAN_POINT('Ctrl Pts',(-1.31381795281002,-1.,-1.56496872402352));
#33891=CARTESIAN_POINT('Ctrl Pts',(-1.31381795281002,1.,-1.56496872402352));
#33892=CARTESIAN_POINT('Ctrl Pts',(-1.31200264341696,-1.,-1.55908521254822));
#33893=CARTESIAN_POINT('Ctrl Pts',(-1.31200264341696,1.,-1.55908521254822));
#33894=CARTESIAN_POINT('Ctrl Pts',(-1.31014393684221,-1.,-1.55322568759481));
#33895=CARTESIAN_POINT('Ctrl Pts',(-1.31014393684221,1.,-1.55322568759481));
#33896=CARTESIAN_POINT('Ctrl Pts',(-1.30824393907471,-1.,-1.54739413957183));
#33897=CARTESIAN_POINT('Ctrl Pts',(-1.30824393907471,1.,-1.54739413957183));
#33898=CARTESIAN_POINT('Ctrl Pts',(-1.30630475189553,-1.,-1.54159462645428));
#33899=CARTESIAN_POINT('Ctrl Pts',(-1.30630475189553,1.,-1.54159462645428));
#33900=CARTESIAN_POINT('Ctrl Pts',(-1.30432735639487,-1.,-1.53582981268976));
#33901=CARTESIAN_POINT('Ctrl Pts',(-1.30432735639487,1.,-1.53582981268976));
#33902=CARTESIAN_POINT('Ctrl Pts',(-1.3023106439557,-1.,-1.53009970283893));
#33903=CARTESIAN_POINT('Ctrl Pts',(-1.3023106439557,1.,-1.53009970283893));
#33904=CARTESIAN_POINT('Ctrl Pts',(-1.30024984366334,-1.,-1.5243995786107));
#33905=CARTESIAN_POINT('Ctrl Pts',(-1.30024984366334,1.,-1.5243995786107));
#33906=CARTESIAN_POINT('Ctrl Pts',(-1.29813791800757,-1.,-1.51872184912735));
#33907=CARTESIAN_POINT('Ctrl Pts',(-1.29813791800757,1.,-1.51872184912735));
#33908=CARTESIAN_POINT('Ctrl Pts',(-1.29596850710518,-1.,-1.51305994241412));
#33909=CARTESIAN_POINT('Ctrl Pts',(-1.29596850710518,1.,-1.51305994241412));
#33910=CARTESIAN_POINT('Ctrl Pts',(-1.29373841372843,-1.,-1.50741159078367));
#33911=CARTESIAN_POINT('Ctrl Pts',(-1.29373841372843,1.,-1.50741159078367));
#33912=CARTESIAN_POINT('Ctrl Pts',(-1.29145022885171,-1.,-1.50178230149764));
#33913=CARTESIAN_POINT('Ctrl Pts',(-1.29145022885171,1.,-1.50178230149764));
#33914=CARTESIAN_POINT('Ctrl Pts',(-1.28911506584232,-1.,-1.49618896881729));
#33915=CARTESIAN_POINT('Ctrl Pts',(-1.28911506584232,1.,-1.49618896881729));
#33916=CARTESIAN_POINT('Ctrl Pts',(-1.28674676116415,-1.,-1.4906522831275));
#33917=CARTESIAN_POINT('Ctrl Pts',(-1.28674676116415,1.,-1.4906522831275));
#33918=CARTESIAN_POINT('Ctrl Pts',(-1.28435533880184,-1.,-1.48518817118891));
#33919=CARTESIAN_POINT('Ctrl Pts',(-1.28435533880184,1.,-1.48518817118891));
#33920=CARTESIAN_POINT('Ctrl Pts',(-1.28194158939522,-1.,-1.47980070347102));
#33921=CARTESIAN_POINT('Ctrl Pts',(-1.28194158939522,1.,-1.47980070347102));
#33922=CARTESIAN_POINT('Ctrl Pts',(-1.27948918248524,-1.,-1.4744717526711));
#33923=CARTESIAN_POINT('Ctrl Pts',(-1.27948918248524,1.,-1.4744717526711));
#33924=CARTESIAN_POINT('Ctrl Pts',(-1.27696414831144,-1.,-1.46916035917197));
#33925=CARTESIAN_POINT('Ctrl Pts',(-1.27696414831144,1.,-1.46916035917197));
#33926=CARTESIAN_POINT('Ctrl Pts',(-1.27433119897877,-1.,-1.4638243133254));
#33927=CARTESIAN_POINT('Ctrl Pts',(-1.27433119897877,1.,-1.4638243133254));
#33928=CARTESIAN_POINT('Ctrl Pts',(-1.27156805265312,-1.,-1.45843906294725));
#33929=CARTESIAN_POINT('Ctrl Pts',(-1.27156805265312,1.,-1.45843906294725));
#33930=CARTESIAN_POINT('Ctrl Pts',(-1.26867786804854,-1.,-1.45301422764205));
#33931=CARTESIAN_POINT('Ctrl Pts',(-1.26867786804854,1.,-1.45301422764205));
#33932=CARTESIAN_POINT('Ctrl Pts',(-1.26570925118767,-1.,-1.44761985001544));
#33933=CARTESIAN_POINT('Ctrl Pts',(-1.26570925118767,1.,-1.44761985001544));
#33934=CARTESIAN_POINT('Ctrl Pts',(-1.26273903323723,-1.,-1.44236470511145));
#33935=CARTESIAN_POINT('Ctrl Pts',(-1.26273903323723,1.,-1.44236470511145));
#33936=CARTESIAN_POINT('Ctrl Pts',(-1.25983531011894,-1.,-1.43734919180719));
#33937=CARTESIAN_POINT('Ctrl Pts',(-1.25983531011894,1.,-1.43734919180719));
#33938=CARTESIAN_POINT('Ctrl Pts',(-1.25702687965744,-1.,-1.43262645609679));
#33939=CARTESIAN_POINT('Ctrl Pts',(-1.25702687965744,1.,-1.43262645609679));
#33940=CARTESIAN_POINT('Ctrl Pts',(-1.25426945222783,-1.,-1.42815938799555));
#33941=CARTESIAN_POINT('Ctrl Pts',(-1.25426945222783,1.,-1.42815938799555));
#33942=CARTESIAN_POINT('Ctrl Pts',(-1.25141455570299,-1.,-1.42378102115911));
#33943=CARTESIAN_POINT('Ctrl Pts',(-1.25141455570299,1.,-1.42378102115911));
#33944=CARTESIAN_POINT('Ctrl Pts',(-1.24824430986911,-1.,-1.41923722596421));
#33945=CARTESIAN_POINT('Ctrl Pts',(-1.24824430986911,1.,-1.41923722596421));
#33946=CARTESIAN_POINT('Ctrl Pts',(-1.24450600513278,-1.,-1.41422913175437));
#33947=CARTESIAN_POINT('Ctrl Pts',(-1.24450600513278,1.,-1.41422913175437));
#33948=CARTESIAN_POINT('Ctrl Pts',(-1.23994455029421,-1.,-1.40845295531151));
#33949=CARTESIAN_POINT('Ctrl Pts',(-1.23994455029421,1.,-1.40845295531151));
#33950=CARTESIAN_POINT('Ctrl Pts',(-1.23434087289768,-1.,-1.40164708205345));
#33951=CARTESIAN_POINT('Ctrl Pts',(-1.23434087289768,1.,-1.40164708205345));
#33952=CARTESIAN_POINT('Ctrl Pts',(-1.22752961898063,-1.,-1.39361389567257));
#33953=CARTESIAN_POINT('Ctrl Pts',(-1.22752961898063,1.,-1.39361389567257));
#33954=CARTESIAN_POINT('Ctrl Pts',(-1.21938737278853,-1.,-1.38420564525391));
#33955=CARTESIAN_POINT('Ctrl Pts',(-1.21938737278853,1.,-1.38420564525391));
#33956=CARTESIAN_POINT('Ctrl Pts',(-1.20982812923113,-1.,-1.37331915604962));
#33957=CARTESIAN_POINT('Ctrl Pts',(-1.20982812923113,1.,-1.37331915604962));
#33958=CARTESIAN_POINT('Ctrl Pts',(-1.1987959077656,-1.,-1.36088705040677));
#33959=CARTESIAN_POINT('Ctrl Pts',(-1.1987959077656,1.,-1.36088705040677));
#33960=CARTESIAN_POINT('Ctrl Pts',(-1.18625865664915,-1.,-1.34687053998157));
#33961=CARTESIAN_POINT('Ctrl Pts',(-1.18625865664915,1.,-1.34687053998157));
#33962=CARTESIAN_POINT('Ctrl Pts',(-1.17501305787994,-1.,-1.33437539344842));
#33963=CARTESIAN_POINT('Ctrl Pts',(-1.17501305787994,1.,-1.33437539344842));
#33964=CARTESIAN_POINT('Ctrl Pts',(-1.16589330092532,-1.,-1.32428080720544));
#33965=CARTESIAN_POINT('Ctrl Pts',(-1.16589330092532,1.,-1.32428080720544));
#33966=CARTESIAN_POINT('Ctrl Pts',(-1.15950888730433,-1.,-1.3172297721596));
#33967=CARTESIAN_POINT('Ctrl Pts',(-1.15950888730433,1.,-1.3172297721596));
#33968=CARTESIAN_POINT('Ctrl Pts',(-1.15624053661742,-1.,-1.31362392696033));
#33969=CARTESIAN_POINT('Ctrl Pts',(-1.15624053661742,1.,-1.31362392696033));
#33970=CARTESIAN_POINT('',(-1.34869019493419,1.,-1.73811241238545));
#33971=CARTESIAN_POINT('Ctrl Pts',(-1.34869019493419,1.,-1.73811241238545));
#33972=CARTESIAN_POINT('Ctrl Pts',(-1.34854391898145,1.,-1.73682580585819));
#33973=CARTESIAN_POINT('Ctrl Pts',(-1.34824783113158,1.,-1.73425417886255));
#33974=CARTESIAN_POINT('Ctrl Pts',(-1.3477930915247,1.,-1.73040149654497));
#33975=CARTESIAN_POINT('Ctrl Pts',(-1.34716554820013,1.,-1.72527410681298));
#33976=CARTESIAN_POINT('Ctrl Pts',(-1.34634568653586,1.,-1.7188807715095));
#33977=CARTESIAN_POINT('Ctrl Pts',(-1.34549029589563,1.,-1.71250340687011));
#33978=CARTESIAN_POINT('Ctrl Pts',(-1.34459924533783,1.,-1.70614212266676));
#33979=CARTESIAN_POINT('Ctrl Pts',(-1.34367237124322,1.,-1.69979707754221));
#33980=CARTESIAN_POINT('Ctrl Pts',(-1.34270948206139,1.,-1.6934684849664));
#33981=CARTESIAN_POINT('Ctrl Pts',(-1.34171037484673,1.,-1.68715660868602));
#33982=CARTESIAN_POINT('Ctrl Pts',(-1.3406748518516,1.,-1.68086176030308));
#33983=CARTESIAN_POINT('Ctrl Pts',(-1.33960273470372,1.,-1.67458429426126));
#33984=CARTESIAN_POINT('Ctrl Pts',(-1.33849388654458,1.,-1.66832460784078));
#33985=CARTESIAN_POINT('Ctrl Pts',(-1.33734820885331,1.,-1.66208312542073));
#33986=CARTESIAN_POINT('Ctrl Pts',(-1.33616559745217,1.,-1.65586025952651));
#33987=CARTESIAN_POINT('Ctrl Pts',(-1.33494590468003,1.,-1.64965637286843));
#33988=CARTESIAN_POINT('Ctrl Pts',(-1.33368890676554,1.,-1.64347174856007));
#33989=CARTESIAN_POINT('Ctrl Pts',(-1.33239425103694,1.,-1.6373065347505));
#33990=CARTESIAN_POINT('Ctrl Pts',(-1.33106149345618,1.,-1.63116079730887));
#33991=CARTESIAN_POINT('Ctrl Pts',(-1.32969019505665,1.,-1.62503464209777));
#33992=CARTESIAN_POINT('Ctrl Pts',(-1.32828000610448,1.,-1.61892832270723));
#33993=CARTESIAN_POINT('Ctrl Pts',(-1.32683074483365,1.,-1.61284234015762));
#33994=CARTESIAN_POINT('Ctrl Pts',(-1.32534250785794,1.,-1.6067775829097));
#33995=CARTESIAN_POINT('Ctrl Pts',(-1.32381550858266,1.,-1.600735118587));
#33996=CARTESIAN_POINT('Ctrl Pts',(-1.32224985747686,1.,-1.59471591079408));
#33997=CARTESIAN_POINT('Ctrl Pts',(-1.32064537110891,1.,-1.58872057258244));
#33998=CARTESIAN_POINT('Ctrl Pts',(-1.31900135021428,1.,-1.58274907898829));
#33999=CARTESIAN_POINT('Ctrl Pts',(-1.31731642317183,1.,-1.57680056505585));
#34000=CARTESIAN_POINT('Ctrl Pts',(-1.31558903860015,1.,-1.57087397835721));
#34001=CARTESIAN_POINT('Ctrl Pts',(-1.31381795281002,1.,-1.56496872402352));
#34002=CARTESIAN_POINT('Ctrl Pts',(-1.31200264341696,1.,-1.55908521254822));
#34003=CARTESIAN_POINT('Ctrl Pts',(-1.31014393684221,1.,-1.55322568759481));
#34004=CARTESIAN_POINT('Ctrl Pts',(-1.30824393907471,1.,-1.54739413957183));
#34005=CARTESIAN_POINT('Ctrl Pts',(-1.30630475189553,1.,-1.54159462645428));
#34006=CARTESIAN_POINT('Ctrl Pts',(-1.30432735639487,1.,-1.53582981268976));
#34007=CARTESIAN_POINT('Ctrl Pts',(-1.3023106439557,1.,-1.53009970283893));
#34008=CARTESIAN_POINT('Ctrl Pts',(-1.30024984366334,1.,-1.5243995786107));
#34009=CARTESIAN_POINT('Ctrl Pts',(-1.29813791800757,1.,-1.51872184912735));
#34010=CARTESIAN_POINT('Ctrl Pts',(-1.29596850710518,1.,-1.51305994241412));
#34011=CARTESIAN_POINT('Ctrl Pts',(-1.29373841372843,1.,-1.50741159078367));
#34012=CARTESIAN_POINT('Ctrl Pts',(-1.29145022885171,1.,-1.50178230149764));
#34013=CARTESIAN_POINT('Ctrl Pts',(-1.28911506584232,1.,-1.49618896881729));
#34014=CARTESIAN_POINT('Ctrl Pts',(-1.28674676116415,1.,-1.4906522831275));
#34015=CARTESIAN_POINT('Ctrl Pts',(-1.28435533880184,1.,-1.48518817118891));
#34016=CARTESIAN_POINT('Ctrl Pts',(-1.28194158939522,1.,-1.47980070347102));
#34017=CARTESIAN_POINT('Ctrl Pts',(-1.27948918248524,1.,-1.4744717526711));
#34018=CARTESIAN_POINT('Ctrl Pts',(-1.27696414831144,1.,-1.46916035917197));
#34019=CARTESIAN_POINT('Ctrl Pts',(-1.27433119897877,1.,-1.4638243133254));
#34020=CARTESIAN_POINT('Ctrl Pts',(-1.27156805265312,1.,-1.45843906294725));
#34021=CARTESIAN_POINT('Ctrl Pts',(-1.26867786804854,1.,-1.45301422764205));
#34022=CARTESIAN_POINT('Ctrl Pts',(-1.26570925118767,1.,-1.44761985001544));
#34023=CARTESIAN_POINT('Ctrl Pts',(-1.26273903323723,1.,-1.44236470511145));
#34024=CARTESIAN_POINT('Ctrl Pts',(-1.25983531011894,1.,-1.43734919180719));
#34025=CARTESIAN_POINT('Ctrl Pts',(-1.25702687965744,1.,-1.43262645609679));
#34026=CARTESIAN_POINT('Ctrl Pts',(-1.25426945222783,1.,-1.42815938799555));
#34027=CARTESIAN_POINT('Ctrl Pts',(-1.25141455570299,1.,-1.42378102115911));
#34028=CARTESIAN_POINT('Ctrl Pts',(-1.24824430986911,1.,-1.41923722596421));
#34029=CARTESIAN_POINT('Ctrl Pts',(-1.24450600513278,1.,-1.41422913175437));
#34030=CARTESIAN_POINT('Ctrl Pts',(-1.23994455029421,1.,-1.40845295531151));
#34031=CARTESIAN_POINT('Ctrl Pts',(-1.23434087289768,1.,-1.40164708205345));
#34032=CARTESIAN_POINT('Ctrl Pts',(-1.22752961898063,1.,-1.39361389567257));
#34033=CARTESIAN_POINT('Ctrl Pts',(-1.21938737278853,1.,-1.38420564525391));
#34034=CARTESIAN_POINT('Ctrl Pts',(-1.20982812923113,1.,-1.37331915604962));
#34035=CARTESIAN_POINT('Ctrl Pts',(-1.1987959077656,1.,-1.36088705040677));
#34036=CARTESIAN_POINT('Ctrl Pts',(-1.18625865664915,1.,-1.34687053998157));
#34037=CARTESIAN_POINT('Ctrl Pts',(-1.17501305787994,1.,-1.33437539344842));
#34038=CARTESIAN_POINT('Ctrl Pts',(-1.16589330092532,1.,-1.32428080720544));
#34039=CARTESIAN_POINT('Ctrl Pts',(-1.15950888730433,1.,-1.3172297721596));
#34040=CARTESIAN_POINT('Ctrl Pts',(-1.15624053661742,1.,-1.31362392696033));
#34041=CARTESIAN_POINT('',(-1.34869019493419,0.,-1.73811241238545));
#34042=CARTESIAN_POINT('Origin',(-1.23627494547115,0.,-1.81978687191668));
#34043=CARTESIAN_POINT('',(-1.23627494547115,1.,-1.81978687191668));
#34044=CARTESIAN_POINT('',(-1.34869019493419,1.,-1.73811241238545));
#34045=CARTESIAN_POINT('',(-1.23627494547115,0.,-1.81978687191668));
#34046=CARTESIAN_POINT('Ctrl Pts',(-0.892032620296855,-1.,-1.5055822144029));
#34047=CARTESIAN_POINT('Ctrl Pts',(-0.892032620296855,1.,-1.5055822144029));
#34048=CARTESIAN_POINT('Ctrl Pts',(-0.894452006967538,-1.,-1.50980486807181));
#34049=CARTESIAN_POINT('Ctrl Pts',(-0.894452006967538,1.,-1.50980486807181));
#34050=CARTESIAN_POINT('Ctrl Pts',(-0.89918504749193,-1.,-1.51805569591479));
#34051=CARTESIAN_POINT('Ctrl Pts',(-0.89918504749193,1.,-1.51805569591479));
#34052=CARTESIAN_POINT('Ctrl Pts',(-0.905967409640499,-1.,-1.52984849890434));
#34053=CARTESIAN_POINT('Ctrl Pts',(-0.905967409640499,1.,-1.52984849890434));
#34054=CARTESIAN_POINT('Ctrl Pts',(-0.91437591904658,-1.,-1.54440491152808));
#34055=CARTESIAN_POINT('Ctrl Pts',(-0.91437591904658,1.,-1.54440491152808));
#34056=CARTESIAN_POINT('Ctrl Pts',(-0.923832188966322,-1.,-1.56065988582509));
#34057=CARTESIAN_POINT('Ctrl Pts',(-0.923832188966322,1.,-1.56065988582509));
#34058=CARTESIAN_POINT('Ctrl Pts',(-0.932246680128849,-1.,-1.57499388385561));
#34059=CARTESIAN_POINT('Ctrl Pts',(-0.932246680128849,1.,-1.57499388385561));
#34060=CARTESIAN_POINT('Ctrl Pts',(-0.939646377909319,-1.,-1.58744937489796));
#34061=CARTESIAN_POINT('Ctrl Pts',(-0.939646377909319,1.,-1.58744937489796));
#34062=CARTESIAN_POINT('Ctrl Pts',(-0.946078063325796,-1.,-1.59810042045408));
#34063=CARTESIAN_POINT('Ctrl Pts',(-0.946078063325796,1.,-1.59810042045408));
#34064=CARTESIAN_POINT('Ctrl Pts',(-0.951613284361248,-1.,-1.60706069897794));
#34065=CARTESIAN_POINT('Ctrl Pts',(-0.951613284361248,1.,-1.60706069897794));
#34066=CARTESIAN_POINT('Ctrl Pts',(-0.956354422921573,-1.,-1.61449324337233));
#34067=CARTESIAN_POINT('Ctrl Pts',(-0.956354422921573,1.,-1.61449324337233));
#34068=CARTESIAN_POINT('Ctrl Pts',(-0.960438326099958,-1.,-1.62061638139929));
#34069=CARTESIAN_POINT('Ctrl Pts',(-0.960438326099958,1.,-1.62061638139929));
#34070=CARTESIAN_POINT('Ctrl Pts',(-0.964046107037821,-1.,-1.6257193066974));
#34071=CARTESIAN_POINT('Ctrl Pts',(-0.964046107037821,1.,-1.6257193066974));
#34072=CARTESIAN_POINT('Ctrl Pts',(-0.967387853228041,-1.,-1.63013849959083));
#34073=CARTESIAN_POINT('Ctrl Pts',(-0.967387853228041,1.,-1.63013849959083));
#34074=CARTESIAN_POINT('Ctrl Pts',(-0.970669715996356,-1.,-1.63420665729609));
#34075=CARTESIAN_POINT('Ctrl Pts',(-0.970669715996356,1.,-1.63420665729609));
#34076=CARTESIAN_POINT('Ctrl Pts',(-0.974066058287501,-1.,-1.63820952658157));
#34077=CARTESIAN_POINT('Ctrl Pts',(-0.974066058287501,1.,-1.63820952658157));
#34078=CARTESIAN_POINT('Ctrl Pts',(-0.977689794120297,-1.,-1.64233990826831));
#34079=CARTESIAN_POINT('Ctrl Pts',(-0.977689794120297,1.,-1.64233990826831));
#34080=CARTESIAN_POINT('Ctrl Pts',(-0.981562530940574,-1.,-1.64665139190834));
#34081=CARTESIAN_POINT('Ctrl Pts',(-0.981562530940574,1.,-1.64665139190834));
#34082=CARTESIAN_POINT('Ctrl Pts',(-0.985642622921626,-1.,-1.6511001661277));
#34083=CARTESIAN_POINT('Ctrl Pts',(-0.985642622921626,1.,-1.6511001661277));
#34084=CARTESIAN_POINT('Ctrl Pts',(-0.98985562785445,-1.,-1.65559044289746));
#34085=CARTESIAN_POINT('Ctrl Pts',(-0.98985562785445,1.,-1.65559044289746));
#34086=CARTESIAN_POINT('Ctrl Pts',(-0.994121836661116,-1.,-1.66001553809916));
#34087=CARTESIAN_POINT('Ctrl Pts',(-0.994121836661116,1.,-1.66001553809916));
#34088=CARTESIAN_POINT('Ctrl Pts',(-0.998389654952317,-1.,-1.66430758030304));
#34089=CARTESIAN_POINT('Ctrl Pts',(-0.998389654952317,1.,-1.66430758030304));
#34090=CARTESIAN_POINT('Ctrl Pts',(-1.00265091003682,-1.,-1.66846059277231));
#34091=CARTESIAN_POINT('Ctrl Pts',(-1.00265091003682,1.,-1.66846059277231));
#34092=CARTESIAN_POINT('Ctrl Pts',(-1.00692206696387,-1.,-1.67250335383248));
#34093=CARTESIAN_POINT('Ctrl Pts',(-1.00692206696387,1.,-1.67250335383248));
#34094=CARTESIAN_POINT('Ctrl Pts',(-1.01123236493507,-1.,-1.67648246776457));
#34095=CARTESIAN_POINT('Ctrl Pts',(-1.01123236493507,1.,-1.67648246776457));
#34096=CARTESIAN_POINT('Ctrl Pts',(-1.01561026162787,-1.,-1.6804428989482));
#34097=CARTESIAN_POINT('Ctrl Pts',(-1.01561026162787,1.,-1.6804428989482));
#34098=CARTESIAN_POINT('Ctrl Pts',(-1.02006795074222,-1.,-1.68440578021739));
#34099=CARTESIAN_POINT('Ctrl Pts',(-1.02006795074222,1.,-1.68440578021739));
#34100=CARTESIAN_POINT('Ctrl Pts',(-1.02460180535272,-1.,-1.68836910178475));
#34101=CARTESIAN_POINT('Ctrl Pts',(-1.02460180535272,1.,-1.68836910178475));
#34102=CARTESIAN_POINT('Ctrl Pts',(-1.02919977579155,-1.,-1.69231840863471));
#34103=CARTESIAN_POINT('Ctrl Pts',(-1.02919977579155,1.,-1.69231840863471));
#34104=CARTESIAN_POINT('Ctrl Pts',(-1.03384646003587,-1.,-1.69623414782769));
#34105=CARTESIAN_POINT('Ctrl Pts',(-1.03384646003587,1.,-1.69623414782769));
#34106=CARTESIAN_POINT('Ctrl Pts',(-1.03852922490782,-1.,-1.70010052930951));
#34107=CARTESIAN_POINT('Ctrl Pts',(-1.03852922490782,1.,-1.70010052930951));
#34108=CARTESIAN_POINT('Ctrl Pts',(-1.04324363334546,-1.,-1.70391338707969));
#34109=CARTESIAN_POINT('Ctrl Pts',(-1.04324363334546,1.,-1.70391338707969));
#34110=CARTESIAN_POINT('Ctrl Pts',(-1.0479908540499,-1.,-1.70767646263641));
#34111=CARTESIAN_POINT('Ctrl Pts',(-1.0479908540499,1.,-1.70767646263641));
#34112=CARTESIAN_POINT('Ctrl Pts',(-1.05277517202854,-1.,-1.71139783543986));
#34113=CARTESIAN_POINT('Ctrl Pts',(-1.05277517202854,1.,-1.71139783543986));
#34114=CARTESIAN_POINT('Ctrl Pts',(-1.05760163192481,-1.,-1.71508654427022));
#34115=CARTESIAN_POINT('Ctrl Pts',(-1.05760163192481,1.,-1.71508654427022));
#34116=CARTESIAN_POINT('Ctrl Pts',(-1.0624732468065,-1.,-1.71874858456908));
#34117=CARTESIAN_POINT('Ctrl Pts',(-1.0624732468065,1.,-1.71874858456908));
#34118=CARTESIAN_POINT('Ctrl Pts',(-1.06738966975463,-1.,-1.72238500928456));
#34119=CARTESIAN_POINT('Ctrl Pts',(-1.06738966975463,1.,-1.72238500928456));
#34120=CARTESIAN_POINT('Ctrl Pts',(-1.07234866990252,-1.,-1.72599406198489));
#34121=CARTESIAN_POINT('Ctrl Pts',(-1.07234866990252,1.,-1.72599406198489));
#34122=CARTESIAN_POINT('Ctrl Pts',(-1.0773470373727,-1.,-1.72957248977424));
#34123=CARTESIAN_POINT('Ctrl Pts',(-1.0773470373727,1.,-1.72957248977424));
#34124=CARTESIAN_POINT('Ctrl Pts',(-1.08238162784749,-1.,-1.73311705663407));
#34125=CARTESIAN_POINT('Ctrl Pts',(-1.08238162784749,1.,-1.73311705663407));
#34126=CARTESIAN_POINT('Ctrl Pts',(-1.08745056285429,-1.,-1.73662628326093));
#34127=CARTESIAN_POINT('Ctrl Pts',(-1.08745056285429,1.,-1.73662628326093));
#34128=CARTESIAN_POINT('Ctrl Pts',(-1.09255329056496,-1.,-1.74010053962252));
#34129=CARTESIAN_POINT('Ctrl Pts',(-1.09255329056496,1.,-1.74010053962252));
#34130=CARTESIAN_POINT('Ctrl Pts',(-1.09768999241229,-1.,-1.74354119236212));
#34131=CARTESIAN_POINT('Ctrl Pts',(-1.09768999241229,1.,-1.74354119236212));
#34132=CARTESIAN_POINT('Ctrl Pts',(-1.10286118991144,-1.,-1.74695004214924));
#34133=CARTESIAN_POINT('Ctrl Pts',(-1.10286118991144,1.,-1.74695004214924));
#34134=CARTESIAN_POINT('Ctrl Pts',(-1.10806728183003,-1.,-1.75032866075914));
#34135=CARTESIAN_POINT('Ctrl Pts',(-1.10806728183003,1.,-1.75032866075914));
#34136=CARTESIAN_POINT('Ctrl Pts',(-1.11330807582542,-1.,-1.75367772094617));
#34137=CARTESIAN_POINT('Ctrl Pts',(-1.11330807582542,1.,-1.75367772094617));
#34138=CARTESIAN_POINT('Ctrl Pts',(-1.11858293216752,-1.,-1.75699720772089));
#34139=CARTESIAN_POINT('Ctrl Pts',(-1.11858293216752,1.,-1.75699720772089));
#34140=CARTESIAN_POINT('Ctrl Pts',(-1.12389096855078,-1.,-1.76028671825084));
#34141=CARTESIAN_POINT('Ctrl Pts',(-1.12389096855078,1.,-1.76028671825084));
#34142=CARTESIAN_POINT('Ctrl Pts',(-1.12923123555076,-1.,-1.76354571966171));
#34143=CARTESIAN_POINT('Ctrl Pts',(-1.12923123555076,1.,-1.76354571966171));
#34144=CARTESIAN_POINT('Ctrl Pts',(-1.13460291804635,-1.,-1.76677384551883));
#34145=CARTESIAN_POINT('Ctrl Pts',(-1.13460291804635,1.,-1.76677384551883));
#34146=CARTESIAN_POINT('Ctrl Pts',(-1.14000548337,-1.,-1.76997111386806));
#34147=CARTESIAN_POINT('Ctrl Pts',(-1.14000548337,1.,-1.76997111386806));
#34148=CARTESIAN_POINT('Ctrl Pts',(-1.14543858226948,-1.,-1.77313777896234));
#34149=CARTESIAN_POINT('Ctrl Pts',(-1.14543858226948,1.,-1.77313777896234));
#34150=CARTESIAN_POINT('Ctrl Pts',(-1.15090197841531,-1.,-1.77627422557034));
#34151=CARTESIAN_POINT('Ctrl Pts',(-1.15090197841531,1.,-1.77627422557034));
#34152=CARTESIAN_POINT('Ctrl Pts',(-1.15639547194689,-1.,-1.77938085564261));
#34153=CARTESIAN_POINT('Ctrl Pts',(-1.15639547194689,1.,-1.77938085564261));
#34154=CARTESIAN_POINT('Ctrl Pts',(-1.16191881298458,-1.,-1.78245795880949));
#34155=CARTESIAN_POINT('Ctrl Pts',(-1.16191881298458,1.,-1.78245795880949));
#34156=CARTESIAN_POINT('Ctrl Pts',(-1.16747166312239,-1.,-1.78550566040349));
#34157=CARTESIAN_POINT('Ctrl Pts',(-1.16747166312239,1.,-1.78550566040349));
#34158=CARTESIAN_POINT('Ctrl Pts',(-1.17305363177265,-1.,-1.78852398877523));
#34159=CARTESIAN_POINT('Ctrl Pts',(-1.17305363177265,1.,-1.78852398877523));
#34160=CARTESIAN_POINT('Ctrl Pts',(-1.17866429440781,-1.,-1.79151291552646));
#34161=CARTESIAN_POINT('Ctrl Pts',(-1.17866429440781,1.,-1.79151291552646));
#34162=CARTESIAN_POINT('Ctrl Pts',(-1.18430321697471,-1.,-1.79447240321572));
#34163=CARTESIAN_POINT('Ctrl Pts',(-1.18430321697471,1.,-1.79447240321572));
#34164=CARTESIAN_POINT('Ctrl Pts',(-1.1899699793456,-1.,-1.79740245923649));
#34165=CARTESIAN_POINT('Ctrl Pts',(-1.1899699793456,1.,-1.79740245923649));
#34166=CARTESIAN_POINT('Ctrl Pts',(-1.19566418930405,-1.,-1.80030314370121));
#34167=CARTESIAN_POINT('Ctrl Pts',(-1.19566418930405,1.,-1.80030314370121));
#34168=CARTESIAN_POINT('Ctrl Pts',(-1.2013854893912,-1.,-1.8031745483882));
#34169=CARTESIAN_POINT('Ctrl Pts',(-1.2013854893912,1.,-1.8031745483882));
#34170=CARTESIAN_POINT('Ctrl Pts',(-1.20713356605519,-1.,-1.80601678480772));
#34171=CARTESIAN_POINT('Ctrl Pts',(-1.20713356605519,1.,-1.80601678480772));
#34172=CARTESIAN_POINT('Ctrl Pts',(-1.2129081570818,-1.,-1.80882996916931));
#34173=CARTESIAN_POINT('Ctrl Pts',(-1.2129081570818,1.,-1.80882996916931));
#34174=CARTESIAN_POINT('Ctrl Pts',(-1.2187090610323,-1.,-1.81161420806172));
#34175=CARTESIAN_POINT('Ctrl Pts',(-1.2187090610323,1.,-1.81161420806172));
#34176=CARTESIAN_POINT('Ctrl Pts',(-1.22453613304507,-1.,-1.81436959209778));
#34177=CARTESIAN_POINT('Ctrl Pts',(-1.22453613304507,1.,-1.81436959209778));
#34178=CARTESIAN_POINT('Ctrl Pts',(-1.22921864890975,-1.,-1.81655087183054));
#34179=CARTESIAN_POINT('Ctrl Pts',(-1.22921864890975,1.,-1.81655087183054));
#34180=CARTESIAN_POINT('Ctrl Pts',(-1.23274224526804,-1.,-1.81817389920914));
#34181=CARTESIAN_POINT('Ctrl Pts',(-1.23274224526804,1.,-1.81817389920914));
#34182=CARTESIAN_POINT('Ctrl Pts',(-1.23509651170384,-1.,-1.81925017193531));
#34183=CARTESIAN_POINT('Ctrl Pts',(-1.23509651170384,1.,-1.81925017193531));
#34184=CARTESIAN_POINT('Ctrl Pts',(-1.23627494547115,-1.,-1.81978687191668));
#34185=CARTESIAN_POINT('Ctrl Pts',(-1.23627494547115,1.,-1.81978687191668));
#34186=CARTESIAN_POINT('',(-0.892032620296855,1.,-1.5055822144029));
#34187=CARTESIAN_POINT('Ctrl Pts',(-0.892032620296855,1.,-1.5055822144029));
#34188=CARTESIAN_POINT('Ctrl Pts',(-0.894452006967538,1.,-1.50980486807181));
#34189=CARTESIAN_POINT('Ctrl Pts',(-0.89918504749193,1.,-1.51805569591479));
#34190=CARTESIAN_POINT('Ctrl Pts',(-0.905967409640499,1.,-1.52984849890434));
#34191=CARTESIAN_POINT('Ctrl Pts',(-0.91437591904658,1.,-1.54440491152808));
#34192=CARTESIAN_POINT('Ctrl Pts',(-0.923832188966322,1.,-1.56065988582509));
#34193=CARTESIAN_POINT('Ctrl Pts',(-0.932246680128849,1.,-1.57499388385561));
#34194=CARTESIAN_POINT('Ctrl Pts',(-0.939646377909319,1.,-1.58744937489796));
#34195=CARTESIAN_POINT('Ctrl Pts',(-0.946078063325796,1.,-1.59810042045408));
#34196=CARTESIAN_POINT('Ctrl Pts',(-0.951613284361248,1.,-1.60706069897794));
#34197=CARTESIAN_POINT('Ctrl Pts',(-0.956354422921573,1.,-1.61449324337233));
#34198=CARTESIAN_POINT('Ctrl Pts',(-0.960438326099958,1.,-1.62061638139929));
#34199=CARTESIAN_POINT('Ctrl Pts',(-0.964046107037821,1.,-1.6257193066974));
#34200=CARTESIAN_POINT('Ctrl Pts',(-0.967387853228041,1.,-1.63013849959083));
#34201=CARTESIAN_POINT('Ctrl Pts',(-0.970669715996356,1.,-1.63420665729609));
#34202=CARTESIAN_POINT('Ctrl Pts',(-0.974066058287501,1.,-1.63820952658157));
#34203=CARTESIAN_POINT('Ctrl Pts',(-0.977689794120297,1.,-1.64233990826831));
#34204=CARTESIAN_POINT('Ctrl Pts',(-0.981562530940574,1.,-1.64665139190834));
#34205=CARTESIAN_POINT('Ctrl Pts',(-0.985642622921626,1.,-1.6511001661277));
#34206=CARTESIAN_POINT('Ctrl Pts',(-0.98985562785445,1.,-1.65559044289746));
#34207=CARTESIAN_POINT('Ctrl Pts',(-0.994121836661116,1.,-1.66001553809916));
#34208=CARTESIAN_POINT('Ctrl Pts',(-0.998389654952317,1.,-1.66430758030304));
#34209=CARTESIAN_POINT('Ctrl Pts',(-1.00265091003682,1.,-1.66846059277231));
#34210=CARTESIAN_POINT('Ctrl Pts',(-1.00692206696387,1.,-1.67250335383248));
#34211=CARTESIAN_POINT('Ctrl Pts',(-1.01123236493507,1.,-1.67648246776457));
#34212=CARTESIAN_POINT('Ctrl Pts',(-1.01561026162787,1.,-1.6804428989482));
#34213=CARTESIAN_POINT('Ctrl Pts',(-1.02006795074222,1.,-1.68440578021739));
#34214=CARTESIAN_POINT('Ctrl Pts',(-1.02460180535272,1.,-1.68836910178475));
#34215=CARTESIAN_POINT('Ctrl Pts',(-1.02919977579155,1.,-1.69231840863471));
#34216=CARTESIAN_POINT('Ctrl Pts',(-1.03384646003587,1.,-1.69623414782769));
#34217=CARTESIAN_POINT('Ctrl Pts',(-1.03852922490782,1.,-1.70010052930951));
#34218=CARTESIAN_POINT('Ctrl Pts',(-1.04324363334546,1.,-1.70391338707969));
#34219=CARTESIAN_POINT('Ctrl Pts',(-1.0479908540499,1.,-1.70767646263641));
#34220=CARTESIAN_POINT('Ctrl Pts',(-1.05277517202854,1.,-1.71139783543986));
#34221=CARTESIAN_POINT('Ctrl Pts',(-1.05760163192481,1.,-1.71508654427022));
#34222=CARTESIAN_POINT('Ctrl Pts',(-1.0624732468065,1.,-1.71874858456908));
#34223=CARTESIAN_POINT('Ctrl Pts',(-1.06738966975463,1.,-1.72238500928456));
#34224=CARTESIAN_POINT('Ctrl Pts',(-1.07234866990252,1.,-1.72599406198489));
#34225=CARTESIAN_POINT('Ctrl Pts',(-1.0773470373727,1.,-1.72957248977424));
#34226=CARTESIAN_POINT('Ctrl Pts',(-1.08238162784749,1.,-1.73311705663407));
#34227=CARTESIAN_POINT('Ctrl Pts',(-1.08745056285429,1.,-1.73662628326093));
#34228=CARTESIAN_POINT('Ctrl Pts',(-1.09255329056496,1.,-1.74010053962252));
#34229=CARTESIAN_POINT('Ctrl Pts',(-1.09768999241229,1.,-1.74354119236212));
#34230=CARTESIAN_POINT('Ctrl Pts',(-1.10286118991144,1.,-1.74695004214924));
#34231=CARTESIAN_POINT('Ctrl Pts',(-1.10806728183003,1.,-1.75032866075914));
#34232=CARTESIAN_POINT('Ctrl Pts',(-1.11330807582542,1.,-1.75367772094617));
#34233=CARTESIAN_POINT('Ctrl Pts',(-1.11858293216752,1.,-1.75699720772089));
#34234=CARTESIAN_POINT('Ctrl Pts',(-1.12389096855078,1.,-1.76028671825084));
#34235=CARTESIAN_POINT('Ctrl Pts',(-1.12923123555076,1.,-1.76354571966171));
#34236=CARTESIAN_POINT('Ctrl Pts',(-1.13460291804635,1.,-1.76677384551883));
#34237=CARTESIAN_POINT('Ctrl Pts',(-1.14000548337,1.,-1.76997111386806));
#34238=CARTESIAN_POINT('Ctrl Pts',(-1.14543858226948,1.,-1.77313777896234));
#34239=CARTESIAN_POINT('Ctrl Pts',(-1.15090197841531,1.,-1.77627422557034));
#34240=CARTESIAN_POINT('Ctrl Pts',(-1.15639547194689,1.,-1.77938085564261));
#34241=CARTESIAN_POINT('Ctrl Pts',(-1.16191881298458,1.,-1.78245795880949));
#34242=CARTESIAN_POINT('Ctrl Pts',(-1.16747166312239,1.,-1.78550566040349));
#34243=CARTESIAN_POINT('Ctrl Pts',(-1.17305363177265,1.,-1.78852398877523));
#34244=CARTESIAN_POINT('Ctrl Pts',(-1.17866429440781,1.,-1.79151291552646));
#34245=CARTESIAN_POINT('Ctrl Pts',(-1.18430321697471,1.,-1.79447240321572));
#34246=CARTESIAN_POINT('Ctrl Pts',(-1.1899699793456,1.,-1.79740245923649));
#34247=CARTESIAN_POINT('Ctrl Pts',(-1.19566418930405,1.,-1.80030314370121));
#34248=CARTESIAN_POINT('Ctrl Pts',(-1.2013854893912,1.,-1.8031745483882));
#34249=CARTESIAN_POINT('Ctrl Pts',(-1.20713356605519,1.,-1.80601678480772));
#34250=CARTESIAN_POINT('Ctrl Pts',(-1.2129081570818,1.,-1.80882996916931));
#34251=CARTESIAN_POINT('Ctrl Pts',(-1.2187090610323,1.,-1.81161420806172));
#34252=CARTESIAN_POINT('Ctrl Pts',(-1.22453613304507,1.,-1.81436959209778));
#34253=CARTESIAN_POINT('Ctrl Pts',(-1.22921864890975,1.,-1.81655087183054));
#34254=CARTESIAN_POINT('Ctrl Pts',(-1.23274224526804,1.,-1.81817389920914));
#34255=CARTESIAN_POINT('Ctrl Pts',(-1.23509651170384,1.,-1.81925017193531));
#34256=CARTESIAN_POINT('Ctrl Pts',(-1.23627494547115,1.,-1.81978687191668));
#34257=CARTESIAN_POINT('',(-0.892032620296856,0.,-1.5055822144029));
#34258=CARTESIAN_POINT('Origin',(0.,0.,0.));
#34259=CARTESIAN_POINT('',(-0.693717979106305,1.,-1.60662857109684));
#34260=CARTESIAN_POINT('Origin',(0.,1.,0.));
#34261=CARTESIAN_POINT('',(-0.693717979106306,0.,-1.60662857109684));
#34262=CARTESIAN_POINT('Ctrl Pts',(-0.745574324794401,-1.,-2.0698113262342));
#34263=CARTESIAN_POINT('Ctrl Pts',(-0.745574324794401,1.,-2.0698113262342));
#34264=CARTESIAN_POINT('Ctrl Pts',(-0.745832791378367,-1.,-2.06854248895728));
#34265=CARTESIAN_POINT('Ctrl Pts',(-0.745832791378367,1.,-2.06854248895728));
#34266=CARTESIAN_POINT('Ctrl Pts',(-0.7463458715442,-1.,-2.06600523016815));
#34267=CARTESIAN_POINT('Ctrl Pts',(-0.7463458715442,1.,-2.06600523016815));
#34268=CARTESIAN_POINT('Ctrl Pts',(-0.747103932787919,-1.,-2.06220058927826));
#34269=CARTESIAN_POINT('Ctrl Pts',(-0.747103932787919,1.,-2.06220058927826));
#34270=CARTESIAN_POINT('Ctrl Pts',(-0.748091554183802,-1.,-2.05713023031006));
#34271=CARTESIAN_POINT('Ctrl Pts',(-0.748091554183802,1.,-2.05713023031006));
#34272=CARTESIAN_POINT('Ctrl Pts',(-0.749287468665046,-1.,-2.05079645592154));
#34273=CARTESIAN_POINT('Ctrl Pts',(-0.749287468665046,1.,-2.05079645592154));
#34274=CARTESIAN_POINT('Ctrl Pts',(-0.750444657875576,-1.,-2.04446689147979));
#34275=CARTESIAN_POINT('Ctrl Pts',(-0.750444657875576,1.,-2.04446689147979));
#34276=CARTESIAN_POINT('Ctrl Pts',(-0.751562963361115,-1.,-2.03814160092099));
#34277=CARTESIAN_POINT('Ctrl Pts',(-0.751562963361115,1.,-2.03814160092099));
#34278=CARTESIAN_POINT('Ctrl Pts',(-0.752642180487211,-1.,-2.03182068456221));
#34279=CARTESIAN_POINT('Ctrl Pts',(-0.752642180487211,1.,-2.03182068456221));
#34280=CARTESIAN_POINT('Ctrl Pts',(-0.753682061112768,-1.,-2.02550428623313));
#34281=CARTESIAN_POINT('Ctrl Pts',(-0.753682061112768,1.,-2.02550428623313));
#34282=CARTESIAN_POINT('Ctrl Pts',(-0.754682330722816,-1.,-2.01919259405809));
#34283=CARTESIAN_POINT('Ctrl Pts',(-0.754682330722816,1.,-2.01919259405809));
#34284=CARTESIAN_POINT('Ctrl Pts',(-0.755642704957865,-1.,-2.01288584328084));
#34285=CARTESIAN_POINT('Ctrl Pts',(-0.755642704957865,1.,-2.01288584328084));
#34286=CARTESIAN_POINT('Ctrl Pts',(-0.75656290464667,-1.,-2.0065843158773));
#34287=CARTESIAN_POINT('Ctrl Pts',(-0.75656290464667,1.,-2.0065843158773));
#34288=CARTESIAN_POINT('Ctrl Pts',(-0.757442676862724,-1.,-2.00028834739178));
#34289=CARTESIAN_POINT('Ctrl Pts',(-0.757442676862724,1.,-2.00028834739178));
#34290=CARTESIAN_POINT('Ctrl Pts',(-0.758281796766761,-1.,-1.99399831098817));
#34291=CARTESIAN_POINT('Ctrl Pts',(-0.758281796766761,1.,-1.99399831098817));
#34292=CARTESIAN_POINT('Ctrl Pts',(-0.759080037802488,-1.,-1.98771456680874));
#34293=CARTESIAN_POINT('Ctrl Pts',(-0.759080037802488,1.,-1.98771456680874));
#34294=CARTESIAN_POINT('Ctrl Pts',(-0.75983714745219,-1.,-1.98143741418172));
#34295=CARTESIAN_POINT('Ctrl Pts',(-0.75983714745219,1.,-1.98143741418172));
#34296=CARTESIAN_POINT('Ctrl Pts',(-0.760552825409757,-1.,-1.97516705321494));
#34297=CARTESIAN_POINT('Ctrl Pts',(-0.760552825409757,1.,-1.97516705321494));
#34298=CARTESIAN_POINT('Ctrl Pts',(-0.76122669048382,-1.,-1.96890351582499));
#34299=CARTESIAN_POINT('Ctrl Pts',(-0.76122669048382,1.,-1.96890351582499));
#34300=CARTESIAN_POINT('Ctrl Pts',(-0.761858300014423,-1.,-1.96264672744186));
#34301=CARTESIAN_POINT('Ctrl Pts',(-0.761858300014423,1.,-1.96264672744186));
#34302=CARTESIAN_POINT('Ctrl Pts',(-0.762447203806179,-1.,-1.95639665309869));
#34303=CARTESIAN_POINT('Ctrl Pts',(-0.762447203806179,1.,-1.95639665309869));
#34304=CARTESIAN_POINT('Ctrl Pts',(-0.762992990878769,-1.,-1.95015342590024));
#34305=CARTESIAN_POINT('Ctrl Pts',(-0.762992990878769,1.,-1.95015342590024));
#34306=CARTESIAN_POINT('Ctrl Pts',(-0.763495333538629,-1.,-1.9439174661764));
#34307=CARTESIAN_POINT('Ctrl Pts',(-0.763495333538629,1.,-1.9439174661764));
#34308=CARTESIAN_POINT('Ctrl Pts',(-0.763954049121458,-1.,-1.93768964875886));
#34309=CARTESIAN_POINT('Ctrl Pts',(-0.763954049121458,1.,-1.93768964875886));
#34310=CARTESIAN_POINT('Ctrl Pts',(-0.764369010673941,-1.,-1.93147105496382));
#34311=CARTESIAN_POINT('Ctrl Pts',(-0.764369010673941,1.,-1.93147105496382));
#34312=CARTESIAN_POINT('Ctrl Pts',(-0.764740025488211,-1.,-1.92526263537048));
#34313=CARTESIAN_POINT('Ctrl Pts',(-0.764740025488211,1.,-1.92526263537048));
#34314=CARTESIAN_POINT('Ctrl Pts',(-0.765066729667088,-1.,-1.91906491634196));
#34315=CARTESIAN_POINT('Ctrl Pts',(-0.765066729667088,1.,-1.91906491634196));
#34316=CARTESIAN_POINT('Ctrl Pts',(-0.765348465884722,-1.,-1.91287765805169));
#34317=CARTESIAN_POINT('Ctrl Pts',(-0.765348465884722,1.,-1.91287765805169));
#34318=CARTESIAN_POINT('Ctrl Pts',(-0.765584196937919,-1.,-1.90669961402356));
#34319=CARTESIAN_POINT('Ctrl Pts',(-0.765584196937919,1.,-1.90669961402356));
#34320=CARTESIAN_POINT('Ctrl Pts',(-0.765772772593386,-1.,-1.90052930393596));
#34321=CARTESIAN_POINT('Ctrl Pts',(-0.765772772593386,1.,-1.90052930393596));
#34322=CARTESIAN_POINT('Ctrl Pts',(-0.765913193856978,-1.,-1.89436577771388));
#34323=CARTESIAN_POINT('Ctrl Pts',(-0.765913193856978,1.,-1.89436577771388));
#34324=CARTESIAN_POINT('Ctrl Pts',(-0.766004837062091,-1.,-1.88820926433409));
#34325=CARTESIAN_POINT('Ctrl Pts',(-0.766004837062091,1.,-1.88820926433409));
#34326=CARTESIAN_POINT('Ctrl Pts',(-0.766047794851865,-1.,-1.88206215302561));
#34327=CARTESIAN_POINT('Ctrl Pts',(-0.766047794851865,1.,-1.88206215302561));
#34328=CARTESIAN_POINT('Ctrl Pts',(-0.766042837036744,-1.,-1.87592888967883));
#34329=CARTESIAN_POINT('Ctrl Pts',(-0.766042837036744,1.,-1.87592888967883));
#34330=CARTESIAN_POINT('Ctrl Pts',(-0.765990708546091,-1.,-1.86981398314341));
#34331=CARTESIAN_POINT('Ctrl Pts',(-0.765990708546091,1.,-1.86981398314341));
#34332=CARTESIAN_POINT('Ctrl Pts',(-0.765891519092547,-1.,-1.86372027063312));
#34333=CARTESIAN_POINT('Ctrl Pts',(-0.765891519092547,1.,-1.86372027063312));
#34334=CARTESIAN_POINT('Ctrl Pts',(-0.765744212909318,-1.,-1.85764741390394));
#34335=CARTESIAN_POINT('Ctrl Pts',(-0.765744212909318,1.,-1.85764741390394));
#34336=CARTESIAN_POINT('Ctrl Pts',(-0.765545710619062,-1.,-1.85158945130063));
#34337=CARTESIAN_POINT('Ctrl Pts',(-0.765545710619062,1.,-1.85158945130063));
#34338=CARTESIAN_POINT('Ctrl Pts',(-0.765291664862029,-1.,-1.84553698875924));
#34339=CARTESIAN_POINT('Ctrl Pts',(-0.765291664862029,1.,-1.84553698875924));
#34340=CARTESIAN_POINT('Ctrl Pts',(-0.764978057881737,-1.,-1.83948181064835));
#34341=CARTESIAN_POINT('Ctrl Pts',(-0.764978057881737,1.,-1.83948181064835));
#34342=CARTESIAN_POINT('Ctrl Pts',(-0.764602549687853,-1.,-1.83342077227142));
#34343=CARTESIAN_POINT('Ctrl Pts',(-0.764602549687853,1.,-1.83342077227142));
#34344=CARTESIAN_POINT('Ctrl Pts',(-0.764165902605995,-1.,-1.82735991200065));
#34345=CARTESIAN_POINT('Ctrl Pts',(-0.764165902605995,1.,-1.82735991200065));
#34346=CARTESIAN_POINT('Ctrl Pts',(-0.763673465462726,-1.,-1.82131873145266));
#34347=CARTESIAN_POINT('Ctrl Pts',(-0.763673465462726,1.,-1.82131873145266));
#34348=CARTESIAN_POINT('Ctrl Pts',(-0.763132003836634,-1.,-1.8153211840553));
#34349=CARTESIAN_POINT('Ctrl Pts',(-0.763132003836634,1.,-1.8153211840553));
#34350=CARTESIAN_POINT('Ctrl Pts',(-0.762546129463938,-1.,-1.80938551463965));
#34351=CARTESIAN_POINT('Ctrl Pts',(-0.762546129463938,1.,-1.80938551463965));
#34352=CARTESIAN_POINT('Ctrl Pts',(-0.761915336443547,-1.,-1.80351583877342));
#34353=CARTESIAN_POINT('Ctrl Pts',(-0.761915336443547,1.,-1.80351583877342));
#34354=CARTESIAN_POINT('Ctrl Pts',(-0.761229695230558,-1.,-1.79768986997783));
#34355=CARTESIAN_POINT('Ctrl Pts',(-0.761229695230558,1.,-1.79768986997783));
#34356=CARTESIAN_POINT('Ctrl Pts',(-0.760469555880749,-1.,-1.7918581561088));
#34357=CARTESIAN_POINT('Ctrl Pts',(-0.760469555880749,1.,-1.7918581561088));
#34358=CARTESIAN_POINT('Ctrl Pts',(-0.759614401110189,-1.,-1.78596964884604));
#34359=CARTESIAN_POINT('Ctrl Pts',(-0.759614401110189,1.,-1.78596964884604));
#34360=CARTESIAN_POINT('Ctrl Pts',(-0.758650626677518,-1.,-1.77999411220945));
#34361=CARTESIAN_POINT('Ctrl Pts',(-0.758650626677518,1.,-1.77999411220945));
#34362=CARTESIAN_POINT('Ctrl Pts',(-0.757578264077029,-1.,-1.77394167108292));
#34363=CARTESIAN_POINT('Ctrl Pts',(-0.757578264077029,1.,-1.77394167108292));
#34364=CARTESIAN_POINT('Ctrl Pts',(-0.75642189602781,-1.,-1.76789396002998));
#34365=CARTESIAN_POINT('Ctrl Pts',(-0.75642189602781,1.,-1.76789396002998));
#34366=CARTESIAN_POINT('Ctrl Pts',(-0.755220979974461,-1.,-1.76197817240128));
#34367=CARTESIAN_POINT('Ctrl Pts',(-0.755220979974461,1.,-1.76197817240128));
#34368=CARTESIAN_POINT('Ctrl Pts',(-0.754009254027829,-1.,-1.75631083600019));
#34369=CARTESIAN_POINT('Ctrl Pts',(-0.754009254027829,1.,-1.75631083600019));
#34370=CARTESIAN_POINT('Ctrl Pts',(-0.752797683531314,-1.,-1.75095139468794));
#34371=CARTESIAN_POINT('Ctrl Pts',(-0.752797683531314,1.,-1.75095139468794));
#34372=CARTESIAN_POINT('Ctrl Pts',(-0.751555614164482,-1.,-1.74585086852502));
#34373=CARTESIAN_POINT('Ctrl Pts',(-0.751555614164482,1.,-1.74585086852502));
#34374=CARTESIAN_POINT('Ctrl Pts',(-0.750193435981249,-1.,-1.74080458267114));
#34375=CARTESIAN_POINT('Ctrl Pts',(-0.750193435981249,1.,-1.74080458267114));
#34376=CARTESIAN_POINT('Ctrl Pts',(-0.74858246295687,-1.,-1.7355035168033));
#34377=CARTESIAN_POINT('Ctrl Pts',(-0.74858246295687,1.,-1.7355035168033));
#34378=CARTESIAN_POINT('Ctrl Pts',(-0.746574710097752,-1.,-1.72958533647714));
#34379=CARTESIAN_POINT('Ctrl Pts',(-0.746574710097752,1.,-1.72958533647714));
#34380=CARTESIAN_POINT('Ctrl Pts',(-0.744021445433093,-1.,-1.72268229916769));
#34381=CARTESIAN_POINT('Ctrl Pts',(-0.744021445433093,1.,-1.72268229916769));
#34382=CARTESIAN_POINT('Ctrl Pts',(-0.74079516202821,-1.,-1.71447789751001));
#34383=CARTESIAN_POINT('Ctrl Pts',(-0.74079516202821,1.,-1.71447789751001));
#34384=CARTESIAN_POINT('Ctrl Pts',(-0.736799665716932,-1.,-1.70473309004249));
#34385=CARTESIAN_POINT('Ctrl Pts',(-0.736799665716932,1.,-1.70473309004249));
#34386=CARTESIAN_POINT('Ctrl Pts',(-0.731963238685357,-1.,-1.69326921972915));
#34387=CARTESIAN_POINT('Ctrl Pts',(-0.731963238685357,1.,-1.69326921972915));
#34388=CARTESIAN_POINT('Ctrl Pts',(-0.726235967982445,-1.,-1.67996158451922));
#34389=CARTESIAN_POINT('Ctrl Pts',(-0.726235967982445,1.,-1.67996158451922));
#34390=CARTESIAN_POINT('Ctrl Pts',(-0.71958543378795,-1.,-1.66472880551777));
#34391=CARTESIAN_POINT('Ctrl Pts',(-0.71958543378795,1.,-1.66472880551777));
#34392=CARTESIAN_POINT('Ctrl Pts',(-0.711993139340447,-1.,-1.64752408828442));
#34393=CARTESIAN_POINT('Ctrl Pts',(-0.711993139340447,1.,-1.64752408828442));
#34394=CARTESIAN_POINT('Ctrl Pts',(-0.705159151977294,-1.,-1.6321654166204));
#34395=CARTESIAN_POINT('Ctrl Pts',(-0.705159151977294,1.,-1.6321654166204));
#34396=CARTESIAN_POINT('Ctrl Pts',(-0.699605146398837,-1.,-1.61974673471117));
#34397=CARTESIAN_POINT('Ctrl Pts',(-0.699605146398837,1.,-1.61974673471117));
#34398=CARTESIAN_POINT('Ctrl Pts',(-0.69571209787897,-1.,-1.61106790957619));
#34399=CARTESIAN_POINT('Ctrl Pts',(-0.69571209787897,1.,-1.61106790957619));
#34400=CARTESIAN_POINT('Ctrl Pts',(-0.693717979106305,-1.,-1.60662857109684));
#34401=CARTESIAN_POINT('Ctrl Pts',(-0.693717979106305,1.,-1.60662857109684));
#34402=CARTESIAN_POINT('',(-0.745574324794401,1.,-2.0698113262342));
#34403=CARTESIAN_POINT('Ctrl Pts',(-0.745574324794401,1.,-2.0698113262342));
#34404=CARTESIAN_POINT('Ctrl Pts',(-0.745832791378367,1.,-2.06854248895728));
#34405=CARTESIAN_POINT('Ctrl Pts',(-0.7463458715442,1.,-2.06600523016815));
#34406=CARTESIAN_POINT('Ctrl Pts',(-0.747103932787919,1.,-2.06220058927826));
#34407=CARTESIAN_POINT('Ctrl Pts',(-0.748091554183802,1.,-2.05713023031006));
#34408=CARTESIAN_POINT('Ctrl Pts',(-0.749287468665046,1.,-2.05079645592154));
#34409=CARTESIAN_POINT('Ctrl Pts',(-0.750444657875576,1.,-2.04446689147979));
#34410=CARTESIAN_POINT('Ctrl Pts',(-0.751562963361115,1.,-2.03814160092099));
#34411=CARTESIAN_POINT('Ctrl Pts',(-0.752642180487211,1.,-2.03182068456221));
#34412=CARTESIAN_POINT('Ctrl Pts',(-0.753682061112768,1.,-2.02550428623313));
#34413=CARTESIAN_POINT('Ctrl Pts',(-0.754682330722816,1.,-2.01919259405809));
#34414=CARTESIAN_POINT('Ctrl Pts',(-0.755642704957865,1.,-2.01288584328084));
#34415=CARTESIAN_POINT('Ctrl Pts',(-0.75656290464667,1.,-2.0065843158773));
#34416=CARTESIAN_POINT('Ctrl Pts',(-0.757442676862724,1.,-2.00028834739178));
#34417=CARTESIAN_POINT('Ctrl Pts',(-0.758281796766761,1.,-1.99399831098817));
#34418=CARTESIAN_POINT('Ctrl Pts',(-0.759080037802488,1.,-1.98771456680874));
#34419=CARTESIAN_POINT('Ctrl Pts',(-0.75983714745219,1.,-1.98143741418172));
#34420=CARTESIAN_POINT('Ctrl Pts',(-0.760552825409757,1.,-1.97516705321494));
#34421=CARTESIAN_POINT('Ctrl Pts',(-0.76122669048382,1.,-1.96890351582499));
#34422=CARTESIAN_POINT('Ctrl Pts',(-0.761858300014423,1.,-1.96264672744186));
#34423=CARTESIAN_POINT('Ctrl Pts',(-0.762447203806179,1.,-1.95639665309869));
#34424=CARTESIAN_POINT('Ctrl Pts',(-0.762992990878769,1.,-1.95015342590024));
#34425=CARTESIAN_POINT('Ctrl Pts',(-0.763495333538629,1.,-1.9439174661764));
#34426=CARTESIAN_POINT('Ctrl Pts',(-0.763954049121458,1.,-1.93768964875886));
#34427=CARTESIAN_POINT('Ctrl Pts',(-0.764369010673941,1.,-1.93147105496382));
#34428=CARTESIAN_POINT('Ctrl Pts',(-0.764740025488211,1.,-1.92526263537048));
#34429=CARTESIAN_POINT('Ctrl Pts',(-0.765066729667088,1.,-1.91906491634196));
#34430=CARTESIAN_POINT('Ctrl Pts',(-0.765348465884722,1.,-1.91287765805169));
#34431=CARTESIAN_POINT('Ctrl Pts',(-0.765584196937919,1.,-1.90669961402356));
#34432=CARTESIAN_POINT('Ctrl Pts',(-0.765772772593386,1.,-1.90052930393596));
#34433=CARTESIAN_POINT('Ctrl Pts',(-0.765913193856978,1.,-1.89436577771388));
#34434=CARTESIAN_POINT('Ctrl Pts',(-0.766004837062091,1.,-1.88820926433409));
#34435=CARTESIAN_POINT('Ctrl Pts',(-0.766047794851865,1.,-1.88206215302561));
#34436=CARTESIAN_POINT('Ctrl Pts',(-0.766042837036744,1.,-1.87592888967883));
#34437=CARTESIAN_POINT('Ctrl Pts',(-0.765990708546091,1.,-1.86981398314341));
#34438=CARTESIAN_POINT('Ctrl Pts',(-0.765891519092547,1.,-1.86372027063312));
#34439=CARTESIAN_POINT('Ctrl Pts',(-0.765744212909318,1.,-1.85764741390394));
#34440=CARTESIAN_POINT('Ctrl Pts',(-0.765545710619062,1.,-1.85158945130063));
#34441=CARTESIAN_POINT('Ctrl Pts',(-0.765291664862029,1.,-1.84553698875924));
#34442=CARTESIAN_POINT('Ctrl Pts',(-0.764978057881737,1.,-1.83948181064835));
#34443=CARTESIAN_POINT('Ctrl Pts',(-0.764602549687853,1.,-1.83342077227142));
#34444=CARTESIAN_POINT('Ctrl Pts',(-0.764165902605995,1.,-1.82735991200065));
#34445=CARTESIAN_POINT('Ctrl Pts',(-0.763673465462726,1.,-1.82131873145266));
#34446=CARTESIAN_POINT('Ctrl Pts',(-0.763132003836634,1.,-1.8153211840553));
#34447=CARTESIAN_POINT('Ctrl Pts',(-0.762546129463938,1.,-1.80938551463965));
#34448=CARTESIAN_POINT('Ctrl Pts',(-0.761915336443547,1.,-1.80351583877342));
#34449=CARTESIAN_POINT('Ctrl Pts',(-0.761229695230558,1.,-1.79768986997783));
#34450=CARTESIAN_POINT('Ctrl Pts',(-0.760469555880749,1.,-1.7918581561088));
#34451=CARTESIAN_POINT('Ctrl Pts',(-0.759614401110189,1.,-1.78596964884604));
#34452=CARTESIAN_POINT('Ctrl Pts',(-0.758650626677518,1.,-1.77999411220945));
#34453=CARTESIAN_POINT('Ctrl Pts',(-0.757578264077029,1.,-1.77394167108292));
#34454=CARTESIAN_POINT('Ctrl Pts',(-0.75642189602781,1.,-1.76789396002998));
#34455=CARTESIAN_POINT('Ctrl Pts',(-0.755220979974461,1.,-1.76197817240128));
#34456=CARTESIAN_POINT('Ctrl Pts',(-0.754009254027829,1.,-1.75631083600019));
#34457=CARTESIAN_POINT('Ctrl Pts',(-0.752797683531314,1.,-1.75095139468794));
#34458=CARTESIAN_POINT('Ctrl Pts',(-0.751555614164482,1.,-1.74585086852502));
#34459=CARTESIAN_POINT('Ctrl Pts',(-0.750193435981249,1.,-1.74080458267114));
#34460=CARTESIAN_POINT('Ctrl Pts',(-0.74858246295687,1.,-1.7355035168033));
#34461=CARTESIAN_POINT('Ctrl Pts',(-0.746574710097752,1.,-1.72958533647714));
#34462=CARTESIAN_POINT('Ctrl Pts',(-0.744021445433093,1.,-1.72268229916769));
#34463=CARTESIAN_POINT('Ctrl Pts',(-0.74079516202821,1.,-1.71447789751001));
#34464=CARTESIAN_POINT('Ctrl Pts',(-0.736799665716932,1.,-1.70473309004249));
#34465=CARTESIAN_POINT('Ctrl Pts',(-0.731963238685357,1.,-1.69326921972915));
#34466=CARTESIAN_POINT('Ctrl Pts',(-0.726235967982445,1.,-1.67996158451922));
#34467=CARTESIAN_POINT('Ctrl Pts',(-0.71958543378795,1.,-1.66472880551777));
#34468=CARTESIAN_POINT('Ctrl Pts',(-0.711993139340447,1.,-1.64752408828442));
#34469=CARTESIAN_POINT('Ctrl Pts',(-0.705159151977294,1.,-1.6321654166204));
#34470=CARTESIAN_POINT('Ctrl Pts',(-0.699605146398837,1.,-1.61974673471117));
#34471=CARTESIAN_POINT('Ctrl Pts',(-0.69571209787897,1.,-1.61106790957619));
#34472=CARTESIAN_POINT('Ctrl Pts',(-0.693717979106305,1.,-1.60662857109684));
#34473=CARTESIAN_POINT('',(-0.745574324794401,0.,-2.0698113262342));
#34474=CARTESIAN_POINT('Origin',(-0.61342227326009,0.,-2.11275013067528));
#34475=CARTESIAN_POINT('',(-0.61342227326009,1.,-2.11275013067528));
#34476=CARTESIAN_POINT('',(-0.745574324794401,1.,-2.0698113262342));
#34477=CARTESIAN_POINT('',(-0.61342227326009,0.,-2.11275013067528));
#34478=CARTESIAN_POINT('Ctrl Pts',(-0.383122945602004,-1.,-1.7075470150345));
#34479=CARTESIAN_POINT('Ctrl Pts',(-0.383122945602004,1.,-1.7075470150345));
#34480=CARTESIAN_POINT('Ctrl Pts',(-0.384119047315542,-1.,-1.71231062891958));
#34481=CARTESIAN_POINT('Ctrl Pts',(-0.384119047315542,1.,-1.71231062891958));
#34482=CARTESIAN_POINT('Ctrl Pts',(-0.38607079032701,-1.,-1.72162022246158));
#34483=CARTESIAN_POINT('Ctrl Pts',(-0.38607079032701,1.,-1.72162022246158));
#34484=CARTESIAN_POINT('Ctrl Pts',(-0.388877023509191,-1.,-1.7349317097561));
#34485=CARTESIAN_POINT('Ctrl Pts',(-0.388877023509191,1.,-1.7349317097561));
#34486=CARTESIAN_POINT('Ctrl Pts',(-0.392375812294307,-1.,-1.75137405313962));
#34487=CARTESIAN_POINT('Ctrl Pts',(-0.392375812294307,1.,-1.75137405313962));
#34488=CARTESIAN_POINT('Ctrl Pts',(-0.39634619612042,-1.,-1.7697556004756));
#34489=CARTESIAN_POINT('Ctrl Pts',(-0.39634619612042,1.,-1.7697556004756));
#34490=CARTESIAN_POINT('Ctrl Pts',(-0.39991940378308,-1.,-1.78598826347533));
#34491=CARTESIAN_POINT('Ctrl Pts',(-0.39991940378308,1.,-1.78598826347533));
#34492=CARTESIAN_POINT('Ctrl Pts',(-0.403107976170441,-1.,-1.80012077176221));
#34493=CARTESIAN_POINT('Ctrl Pts',(-0.403107976170441,1.,-1.80012077176221));
#34494=CARTESIAN_POINT('Ctrl Pts',(-0.405933518411838,-1.,-1.81223801813988));
#34495=CARTESIAN_POINT('Ctrl Pts',(-0.405933518411838,1.,-1.81223801813988));
#34496=CARTESIAN_POINT('Ctrl Pts',(-0.408428948108533,-1.,-1.8224702267854));
#34497=CARTESIAN_POINT('Ctrl Pts',(-0.408428948108533,1.,-1.8224702267854));
#34498=CARTESIAN_POINT('Ctrl Pts',(-0.410641256301675,-1.,-1.83100408895216));
#34499=CARTESIAN_POINT('Ctrl Pts',(-0.410641256301675,1.,-1.83100408895216));
#34500=CARTESIAN_POINT('Ctrl Pts',(-0.412633125322162,-1.,-1.83808953475839));
#34501=CARTESIAN_POINT('Ctrl Pts',(-0.412633125322162,1.,-1.83808953475839));
#34502=CARTESIAN_POINT('Ctrl Pts',(-0.41448743825434,-1.,-1.8440575707371));
#34503=CARTESIAN_POINT('Ctrl Pts',(-0.41448743825434,1.,-1.8440575707371));
#34504=CARTESIAN_POINT('Ctrl Pts',(-0.416300022038864,-1.,-1.84929312929882));
#34505=CARTESIAN_POINT('Ctrl Pts',(-0.416300022038864,1.,-1.84929312929882));
#34506=CARTESIAN_POINT('Ctrl Pts',(-0.418164129143534,-1.,-1.85417632856234));
#34507=CARTESIAN_POINT('Ctrl Pts',(-0.418164129143534,1.,-1.85417632856234));
#34508=CARTESIAN_POINT('Ctrl Pts',(-0.420157287975619,-1.,-1.85903281096686));
#34509=CARTESIAN_POINT('Ctrl Pts',(-0.420157287975619,1.,-1.85903281096686));
#34510=CARTESIAN_POINT('Ctrl Pts',(-0.422327307418275,-1.,-1.86408083334028));
#34511=CARTESIAN_POINT('Ctrl Pts',(-0.422327307418275,1.,-1.86408083334028));
#34512=CARTESIAN_POINT('Ctrl Pts',(-0.424678177291359,-1.,-1.86937803944323));
#34513=CARTESIAN_POINT('Ctrl Pts',(-0.424678177291359,1.,-1.86937803944323));
#34514=CARTESIAN_POINT('Ctrl Pts',(-0.427183828519102,-1.,-1.87486989291484));
#34515=CARTESIAN_POINT('Ctrl Pts',(-0.427183828519102,1.,-1.87486989291484));
#34516=CARTESIAN_POINT('Ctrl Pts',(-0.429803062482344,-1.,-1.88044229001832));
#34517=CARTESIAN_POINT('Ctrl Pts',(-0.429803062482344,1.,-1.88044229001832));
#34518=CARTESIAN_POINT('Ctrl Pts',(-0.432493038548748,-1.,-1.88596913666793));
#34519=CARTESIAN_POINT('Ctrl Pts',(-0.432493038548748,1.,-1.88596913666793));
#34520=CARTESIAN_POINT('Ctrl Pts',(-0.435225660963383,-1.,-1.89136993975504));
#34521=CARTESIAN_POINT('Ctrl Pts',(-0.435225660963383,1.,-1.89136993975504));
#34522=CARTESIAN_POINT('Ctrl Pts',(-0.437995003948244,-1.,-1.89663648956466));
#34523=CARTESIAN_POINT('Ctrl Pts',(-0.437995003948244,1.,-1.89663648956466));
#34524=CARTESIAN_POINT('Ctrl Pts',(-0.440807833704038,-1.,-1.90180124389086));
#34525=CARTESIAN_POINT('Ctrl Pts',(-0.440807833704038,1.,-1.90180124389086));
#34526=CARTESIAN_POINT('Ctrl Pts',(-0.443677556849151,-1.,-1.90691756144898));
#34527=CARTESIAN_POINT('Ctrl Pts',(-0.443677556849151,1.,-1.90691756144898));
#34528=CARTESIAN_POINT('Ctrl Pts',(-0.446617343485711,-1.,-1.9120369998112));
#34529=CARTESIAN_POINT('Ctrl Pts',(-0.446617343485711,1.,-1.9120369998112));
#34530=CARTESIAN_POINT('Ctrl Pts',(-0.449632260106662,-1.,-1.91718342555755));
#34531=CARTESIAN_POINT('Ctrl Pts',(-0.449632260106662,1.,-1.91718342555755));
#34532=CARTESIAN_POINT('Ctrl Pts',(-0.452719478359432,-1.,-1.92235380648502));
#34533=CARTESIAN_POINT('Ctrl Pts',(-0.452719478359432,1.,-1.92235380648502));
#34534=CARTESIAN_POINT('Ctrl Pts',(-0.455872005174371,-1.,-1.92753067150476));
#34535=CARTESIAN_POINT('Ctrl Pts',(-0.455872005174371,1.,-1.92753067150476));
#34536=CARTESIAN_POINT('Ctrl Pts',(-0.459081234547926,-1.,-1.93269066517934));
#34537=CARTESIAN_POINT('Ctrl Pts',(-0.459081234547926,1.,-1.93269066517934));
#34538=CARTESIAN_POINT('Ctrl Pts',(-0.462340031009056,-1.,-1.93781486640821));
#34539=CARTESIAN_POINT('Ctrl Pts',(-0.462340031009056,1.,-1.93781486640821));
#34540=CARTESIAN_POINT('Ctrl Pts',(-0.46564546202603,-1.,-1.9428979419619));
#34541=CARTESIAN_POINT('Ctrl Pts',(-0.46564546202603,1.,-1.9428979419619));
#34542=CARTESIAN_POINT('Ctrl Pts',(-0.468997482913135,-1.,-1.94794381136514));
#34543=CARTESIAN_POINT('Ctrl Pts',(-0.468997482913135,1.,-1.94794381136514));
#34544=CARTESIAN_POINT('Ctrl Pts',(-0.472397672264072,-1.,-1.95296148278133));
#34545=CARTESIAN_POINT('Ctrl Pts',(-0.472397672264072,1.,-1.95296148278133));
#34546=CARTESIAN_POINT('Ctrl Pts',(-0.475848034683176,-1.,-1.95796111148177));
#34547=CARTESIAN_POINT('Ctrl Pts',(-0.475848034683176,1.,-1.95796111148177));
#34548=CARTESIAN_POINT('Ctrl Pts',(-0.479349583074855,-1.,-1.96294933055943));
#34549=CARTESIAN_POINT('Ctrl Pts',(-0.479349583074855,1.,-1.96294933055943));
#34550=CARTESIAN_POINT('Ctrl Pts',(-0.482901662120691,-1.,-1.96792703422362));
#34551=CARTESIAN_POINT('Ctrl Pts',(-0.482901662120691,1.,-1.96792703422362));
#34552=CARTESIAN_POINT('Ctrl Pts',(-0.486502692907659,-1.,-1.97289186263272));
#34553=CARTESIAN_POINT('Ctrl Pts',(-0.486502692907659,1.,-1.97289186263272));
#34554=CARTESIAN_POINT('Ctrl Pts',(-0.490150627860952,-1.,-1.97783973019229));
#34555=CARTESIAN_POINT('Ctrl Pts',(-0.490150627860952,1.,-1.97783973019229));
#34556=CARTESIAN_POINT('Ctrl Pts',(-0.493843476541495,-1.,-1.98276658761821));
#34557=CARTESIAN_POINT('Ctrl Pts',(-0.493843476541495,1.,-1.98276658761821));
#34558=CARTESIAN_POINT('Ctrl Pts',(-0.497579909545574,-1.,-1.98767044752932));
#34559=CARTESIAN_POINT('Ctrl Pts',(-0.497579909545574,1.,-1.98767044752932));
#34560=CARTESIAN_POINT('Ctrl Pts',(-0.501359287727146,-1.,-1.99255149126155));
#34561=CARTESIAN_POINT('Ctrl Pts',(-0.501359287727146,1.,-1.99255149126155));
#34562=CARTESIAN_POINT('Ctrl Pts',(-0.505181361323026,-1.,-1.99741107463572));
#34563=CARTESIAN_POINT('Ctrl Pts',(-0.505181361323026,1.,-1.99741107463572));
#34564=CARTESIAN_POINT('Ctrl Pts',(-0.509046069886157,-1.,-2.00225107134734));
#34565=CARTESIAN_POINT('Ctrl Pts',(-0.509046069886157,1.,-2.00225107134734));
#34566=CARTESIAN_POINT('Ctrl Pts',(-0.512953306961792,-1.,-2.00707309946949));
#34567=CARTESIAN_POINT('Ctrl Pts',(-0.512953306961792,1.,-2.00707309946949));
#34568=CARTESIAN_POINT('Ctrl Pts',(-0.516902681728687,-1.,-2.01187773939242));
#34569=CARTESIAN_POINT('Ctrl Pts',(-0.516902681728687,1.,-2.01187773939242));
#34570=CARTESIAN_POINT('Ctrl Pts',(-0.52089359039937,-1.,-2.01666477917286));
#34571=CARTESIAN_POINT('Ctrl Pts',(-0.52089359039937,1.,-2.01666477917286));
#34572=CARTESIAN_POINT('Ctrl Pts',(-0.524925318333476,-1.,-2.02143356304698));
#34573=CARTESIAN_POINT('Ctrl Pts',(-0.524925318333476,1.,-2.02143356304698));
#34574=CARTESIAN_POINT('Ctrl Pts',(-0.528997127241914,-1.,-2.0261832908329));
#34575=CARTESIAN_POINT('Ctrl Pts',(-0.528997127241914,1.,-2.0261832908329));
#34576=CARTESIAN_POINT('Ctrl Pts',(-0.533108355132977,-1.,-2.03091336214426));
#34577=CARTESIAN_POINT('Ctrl Pts',(-0.533108355132977,1.,-2.03091336214426));
#34578=CARTESIAN_POINT('Ctrl Pts',(-0.537258489833262,-1.,-2.03562362954037));
#34579=CARTESIAN_POINT('Ctrl Pts',(-0.537258489833262,1.,-2.03562362954037));
#34580=CARTESIAN_POINT('Ctrl Pts',(-0.541447120615659,-1.,-2.04031422690527));
#34581=CARTESIAN_POINT('Ctrl Pts',(-0.541447120615659,1.,-2.04031422690527));
#34582=CARTESIAN_POINT('Ctrl Pts',(-0.54567390381743,-1.,-2.04498544714588));
#34583=CARTESIAN_POINT('Ctrl Pts',(-0.54567390381743,1.,-2.04498544714588));
#34584=CARTESIAN_POINT('Ctrl Pts',(-0.549938525150295,-1.,-2.04963761077958));
#34585=CARTESIAN_POINT('Ctrl Pts',(-0.549938525150295,1.,-2.04963761077958));
#34586=CARTESIAN_POINT('Ctrl Pts',(-0.554240657463906,-1.,-2.05427091604413));
#34587=CARTESIAN_POINT('Ctrl Pts',(-0.554240657463906,1.,-2.05427091604413));
#34588=CARTESIAN_POINT('Ctrl Pts',(-0.558579940185151,-1.,-2.05888537756462));
#34589=CARTESIAN_POINT('Ctrl Pts',(-0.558579940185151,1.,-2.05888537756462));
#34590=CARTESIAN_POINT('Ctrl Pts',(-0.562955993082261,-1.,-2.06348090160589));
#34591=CARTESIAN_POINT('Ctrl Pts',(-0.562955993082261,1.,-2.06348090160589));
#34592=CARTESIAN_POINT('Ctrl Pts',(-0.567368421181087,-1.,-2.06805732997334));
#34593=CARTESIAN_POINT('Ctrl Pts',(-0.567368421181087,1.,-2.06805732997334));
#34594=CARTESIAN_POINT('Ctrl Pts',(-0.571816823242603,-1.,-2.07261449292824));
#34595=CARTESIAN_POINT('Ctrl Pts',(-0.571816823242603,1.,-2.07261449292824));
#34596=CARTESIAN_POINT('Ctrl Pts',(-0.576300797416844,-1.,-2.07715226767559));
#34597=CARTESIAN_POINT('Ctrl Pts',(-0.576300797416844,1.,-2.07715226767559));
#34598=CARTESIAN_POINT('Ctrl Pts',(-0.580819952108063,-1.,-2.08167059018418));
#34599=CARTESIAN_POINT('Ctrl Pts',(-0.580819952108063,1.,-2.08167059018418));
#34600=CARTESIAN_POINT('Ctrl Pts',(-0.585373918991617,-1.,-2.08616943727951));
#34601=CARTESIAN_POINT('Ctrl Pts',(-0.585373918991617,1.,-2.08616943727951));
#34602=CARTESIAN_POINT('Ctrl Pts',(-0.589962365403406,-1.,-2.09064881812129));
#34603=CARTESIAN_POINT('Ctrl Pts',(-0.589962365403406,1.,-2.09064881812129));
#34604=CARTESIAN_POINT('Ctrl Pts',(-0.594585006052162,-1.,-2.0951087622027));
#34605=CARTESIAN_POINT('Ctrl Pts',(-0.594585006052162,1.,-2.0951087622027));
#34606=CARTESIAN_POINT('Ctrl Pts',(-0.599241616420533,-1.,-2.0995493086477));
#34607=CARTESIAN_POINT('Ctrl Pts',(-0.599241616420533,1.,-2.0995493086477));
#34608=CARTESIAN_POINT('Ctrl Pts',(-0.60393203073603,-1.,-2.10397049886949));
#34609=CARTESIAN_POINT('Ctrl Pts',(-0.60393203073603,1.,-2.10397049886949));
#34610=CARTESIAN_POINT('Ctrl Pts',(-0.607711315454876,-1.,-2.1074919961518));
#34611=CARTESIAN_POINT('Ctrl Pts',(-0.607711315454876,1.,-2.1074919961518));
#34612=CARTESIAN_POINT('Ctrl Pts',(-0.610560911689899,-1.,-2.11012443807238));
#34613=CARTESIAN_POINT('Ctrl Pts',(-0.610560911689899,1.,-2.11012443807238));
#34614=CARTESIAN_POINT('Ctrl Pts',(-0.6124673655618,-1.,-2.11187554259986));
#34615=CARTESIAN_POINT('Ctrl Pts',(-0.6124673655618,1.,-2.11187554259986));
#34616=CARTESIAN_POINT('Ctrl Pts',(-0.61342227326009,-1.,-2.11275013067528));
#34617=CARTESIAN_POINT('Ctrl Pts',(-0.61342227326009,1.,-2.11275013067528));
#34618=CARTESIAN_POINT('',(-0.383122945602004,1.,-1.7075470150345));
#34619=CARTESIAN_POINT('Ctrl Pts',(-0.383122945602004,1.,-1.7075470150345));
#34620=CARTESIAN_POINT('Ctrl Pts',(-0.384119047315542,1.,-1.71231062891958));
#34621=CARTESIAN_POINT('Ctrl Pts',(-0.38607079032701,1.,-1.72162022246158));
#34622=CARTESIAN_POINT('Ctrl Pts',(-0.388877023509191,1.,-1.7349317097561));
#34623=CARTESIAN_POINT('Ctrl Pts',(-0.392375812294307,1.,-1.75137405313962));
#34624=CARTESIAN_POINT('Ctrl Pts',(-0.39634619612042,1.,-1.7697556004756));
#34625=CARTESIAN_POINT('Ctrl Pts',(-0.39991940378308,1.,-1.78598826347533));
#34626=CARTESIAN_POINT('Ctrl Pts',(-0.403107976170441,1.,-1.80012077176221));
#34627=CARTESIAN_POINT('Ctrl Pts',(-0.405933518411838,1.,-1.81223801813988));
#34628=CARTESIAN_POINT('Ctrl Pts',(-0.408428948108533,1.,-1.8224702267854));
#34629=CARTESIAN_POINT('Ctrl Pts',(-0.410641256301675,1.,-1.83100408895216));
#34630=CARTESIAN_POINT('Ctrl Pts',(-0.412633125322162,1.,-1.83808953475839));
#34631=CARTESIAN_POINT('Ctrl Pts',(-0.41448743825434,1.,-1.8440575707371));
#34632=CARTESIAN_POINT('Ctrl Pts',(-0.416300022038864,1.,-1.84929312929882));
#34633=CARTESIAN_POINT('Ctrl Pts',(-0.418164129143534,1.,-1.85417632856234));
#34634=CARTESIAN_POINT('Ctrl Pts',(-0.420157287975619,1.,-1.85903281096686));
#34635=CARTESIAN_POINT('Ctrl Pts',(-0.422327307418275,1.,-1.86408083334028));
#34636=CARTESIAN_POINT('Ctrl Pts',(-0.424678177291359,1.,-1.86937803944323));
#34637=CARTESIAN_POINT('Ctrl Pts',(-0.427183828519102,1.,-1.87486989291484));
#34638=CARTESIAN_POINT('Ctrl Pts',(-0.429803062482344,1.,-1.88044229001832));
#34639=CARTESIAN_POINT('Ctrl Pts',(-0.432493038548748,1.,-1.88596913666793));
#34640=CARTESIAN_POINT('Ctrl Pts',(-0.435225660963383,1.,-1.89136993975504));
#34641=CARTESIAN_POINT('Ctrl Pts',(-0.437995003948244,1.,-1.89663648956466));
#34642=CARTESIAN_POINT('Ctrl Pts',(-0.440807833704038,1.,-1.90180124389086));
#34643=CARTESIAN_POINT('Ctrl Pts',(-0.443677556849151,1.,-1.90691756144898));
#34644=CARTESIAN_POINT('Ctrl Pts',(-0.446617343485711,1.,-1.9120369998112));
#34645=CARTESIAN_POINT('Ctrl Pts',(-0.449632260106662,1.,-1.91718342555755));
#34646=CARTESIAN_POINT('Ctrl Pts',(-0.452719478359432,1.,-1.92235380648502));
#34647=CARTESIAN_POINT('Ctrl Pts',(-0.455872005174371,1.,-1.92753067150476));
#34648=CARTESIAN_POINT('Ctrl Pts',(-0.459081234547926,1.,-1.93269066517934));
#34649=CARTESIAN_POINT('Ctrl Pts',(-0.462340031009056,1.,-1.93781486640821));
#34650=CARTESIAN_POINT('Ctrl Pts',(-0.46564546202603,1.,-1.9428979419619));
#34651=CARTESIAN_POINT('Ctrl Pts',(-0.468997482913135,1.,-1.94794381136514));
#34652=CARTESIAN_POINT('Ctrl Pts',(-0.472397672264072,1.,-1.95296148278133));
#34653=CARTESIAN_POINT('Ctrl Pts',(-0.475848034683176,1.,-1.95796111148177));
#34654=CARTESIAN_POINT('Ctrl Pts',(-0.479349583074855,1.,-1.96294933055943));
#34655=CARTESIAN_POINT('Ctrl Pts',(-0.482901662120691,1.,-1.96792703422362));
#34656=CARTESIAN_POINT('Ctrl Pts',(-0.486502692907659,1.,-1.97289186263272));
#34657=CARTESIAN_POINT('Ctrl Pts',(-0.490150627860952,1.,-1.97783973019229));
#34658=CARTESIAN_POINT('Ctrl Pts',(-0.493843476541495,1.,-1.98276658761821));
#34659=CARTESIAN_POINT('Ctrl Pts',(-0.497579909545574,1.,-1.98767044752932));
#34660=CARTESIAN_POINT('Ctrl Pts',(-0.501359287727146,1.,-1.99255149126155));
#34661=CARTESIAN_POINT('Ctrl Pts',(-0.505181361323026,1.,-1.99741107463572));
#34662=CARTESIAN_POINT('Ctrl Pts',(-0.509046069886157,1.,-2.00225107134734));
#34663=CARTESIAN_POINT('Ctrl Pts',(-0.512953306961792,1.,-2.00707309946949));
#34664=CARTESIAN_POINT('Ctrl Pts',(-0.516902681728687,1.,-2.01187773939242));
#34665=CARTESIAN_POINT('Ctrl Pts',(-0.52089359039937,1.,-2.01666477917286));
#34666=CARTESIAN_POINT('Ctrl Pts',(-0.524925318333476,1.,-2.02143356304698));
#34667=CARTESIAN_POINT('Ctrl Pts',(-0.528997127241914,1.,-2.0261832908329));
#34668=CARTESIAN_POINT('Ctrl Pts',(-0.533108355132977,1.,-2.03091336214426));
#34669=CARTESIAN_POINT('Ctrl Pts',(-0.537258489833262,1.,-2.03562362954037));
#34670=CARTESIAN_POINT('Ctrl Pts',(-0.541447120615659,1.,-2.04031422690527));
#34671=CARTESIAN_POINT('Ctrl Pts',(-0.54567390381743,1.,-2.04498544714588));
#34672=CARTESIAN_POINT('Ctrl Pts',(-0.549938525150295,1.,-2.04963761077958));
#34673=CARTESIAN_POINT('Ctrl Pts',(-0.554240657463906,1.,-2.05427091604413));
#34674=CARTESIAN_POINT('Ctrl Pts',(-0.558579940185151,1.,-2.05888537756462));
#34675=CARTESIAN_POINT('Ctrl Pts',(-0.562955993082261,1.,-2.06348090160589));
#34676=CARTESIAN_POINT('Ctrl Pts',(-0.567368421181087,1.,-2.06805732997334));
#34677=CARTESIAN_POINT('Ctrl Pts',(-0.571816823242603,1.,-2.07261449292824));
#34678=CARTESIAN_POINT('Ctrl Pts',(-0.576300797416844,1.,-2.07715226767559));
#34679=CARTESIAN_POINT('Ctrl Pts',(-0.580819952108063,1.,-2.08167059018418));
#34680=CARTESIAN_POINT('Ctrl Pts',(-0.585373918991617,1.,-2.08616943727951));
#34681=CARTESIAN_POINT('Ctrl Pts',(-0.589962365403406,1.,-2.09064881812129));
#34682=CARTESIAN_POINT('Ctrl Pts',(-0.594585006052162,1.,-2.0951087622027));
#34683=CARTESIAN_POINT('Ctrl Pts',(-0.599241616420533,1.,-2.0995493086477));
#34684=CARTESIAN_POINT('Ctrl Pts',(-0.60393203073603,1.,-2.10397049886949));
#34685=CARTESIAN_POINT('Ctrl Pts',(-0.607711315454876,1.,-2.1074919961518));
#34686=CARTESIAN_POINT('Ctrl Pts',(-0.610560911689899,1.,-2.11012443807238));
#34687=CARTESIAN_POINT('Ctrl Pts',(-0.6124673655618,1.,-2.11187554259986));
#34688=CARTESIAN_POINT('Ctrl Pts',(-0.61342227326009,1.,-2.11275013067528));
#34689=CARTESIAN_POINT('',(-0.383122945602003,0.,-1.7075470150345));
#34690=CARTESIAN_POINT('Origin',(0.,0.,0.));
#34691=CARTESIAN_POINT('',(-0.163289472382896,1.,-1.74236521665491));
#34692=CARTESIAN_POINT('Origin',(0.,1.,0.));
#34693=CARTESIAN_POINT('',(-0.163289472382896,0.,-1.74236521665491));
#34694=CARTESIAN_POINT('Ctrl Pts',(-0.0694764450219581,-1.,-2.19890268624765));
#34695=CARTESIAN_POINT('Ctrl Pts',(-0.0694764450219581,1.,-2.19890268624765));
#34696=CARTESIAN_POINT('Ctrl Pts',(-0.070114353632549,-1.,-2.19777582085423));
#34697=CARTESIAN_POINT('Ctrl Pts',(-0.070114353632549,1.,-2.19777582085423));
#34698=CARTESIAN_POINT('Ctrl Pts',(-0.0713863779526154,-1.,-2.19552129484002));
#34699=CARTESIAN_POINT('Ctrl Pts',(-0.0713863779526154,1.,-2.19552129484002));
#34700=CARTESIAN_POINT('Ctrl Pts',(-0.0732830357306725,-1.,-2.19213712013662));
#34701=CARTESIAN_POINT('Ctrl Pts',(-0.0732830357306725,1.,-2.19213712013662));
#34702=CARTESIAN_POINT('Ctrl Pts',(-0.0757891465836148,-1.,-2.1876201139953));
#34703=CARTESIAN_POINT('Ctrl Pts',(-0.0757891465836148,1.,-2.1876201139953));
#34704=CARTESIAN_POINT('Ctrl Pts',(-0.0788837727685243,-1.,-2.18196589448887));
#34705=CARTESIAN_POINT('Ctrl Pts',(-0.0788837727685243,1.,-2.18196589448887));
#34706=CARTESIAN_POINT('Ctrl Pts',(-0.0819402680872765,-1.,-2.176303712113));
#34707=CARTESIAN_POINT('Ctrl Pts',(-0.0819402680872765,1.,-2.176303712113));
#34708=CARTESIAN_POINT('Ctrl Pts',(-0.0849584620835372,-1.,-2.17063357870952));
#34709=CARTESIAN_POINT('Ctrl Pts',(-0.0849584620835372,1.,-2.17063357870952));
#34710=CARTESIAN_POINT('Ctrl Pts',(-0.0879381291386923,-1.,-2.16495552645014));
#34711=CARTESIAN_POINT('Ctrl Pts',(-0.0879381291386923,1.,-2.16495552645014));
#34712=CARTESIAN_POINT('Ctrl Pts',(-0.0908789888107265,-1.,-2.15926961544516));
#34713=CARTESIAN_POINT('Ctrl Pts',(-0.0908789888107265,1.,-2.15926961544516));
#34714=CARTESIAN_POINT('Ctrl Pts',(-0.0937807218867643,-1.,-2.1535759397817));
#34715=CARTESIAN_POINT('Ctrl Pts',(-0.0937807218867643,1.,-2.1535759397817));
#34716=CARTESIAN_POINT('Ctrl Pts',(-0.0966429852305459,-1.,-2.14787463531795));
#34717=CARTESIAN_POINT('Ctrl Pts',(-0.0966429852305459,1.,-2.14787463531795));
#34718=CARTESIAN_POINT('Ctrl Pts',(-0.0994654261990915,-1.,-2.14216588396025));
#34719=CARTESIAN_POINT('Ctrl Pts',(-0.0994654261990915,1.,-2.14216588396025));
#34720=CARTESIAN_POINT('Ctrl Pts',(-0.1022477005561,-1.,-2.13644992667165));
#34721=CARTESIAN_POINT('Ctrl Pts',(-0.1022477005561,1.,-2.13644992667165));
#34722=CARTESIAN_POINT('Ctrl Pts',(-0.104989479152739,-1.,-2.13072704887293));
#34723=CARTESIAN_POINT('Ctrl Pts',(-0.104989479152739,1.,-2.13072704887293));
#34724=CARTESIAN_POINT('Ctrl Pts',(-0.10769043523109,-1.,-2.12499752307));
#34725=CARTESIAN_POINT('Ctrl Pts',(-0.10769043523109,1.,-2.12499752307));
#34726=CARTESIAN_POINT('Ctrl Pts',(-0.110350236135025,-1.,-2.11926155590865));
#34727=CARTESIAN_POINT('Ctrl Pts',(-0.110350236135025,1.,-2.11926155590865));
#34728=CARTESIAN_POINT('Ctrl Pts',(-0.112968534419737,-1.,-2.11351924490306));
#34729=CARTESIAN_POINT('Ctrl Pts',(-0.112968534419737,1.,-2.11351924490306));
#34730=CARTESIAN_POINT('Ctrl Pts',(-0.115544957687926,-1.,-2.10777050261309));
#34731=CARTESIAN_POINT('Ctrl Pts',(-0.115544957687926,1.,-2.10777050261309));
#34732=CARTESIAN_POINT('Ctrl Pts',(-0.118079107988355,-1.,-2.102015121329));
#34733=CARTESIAN_POINT('Ctrl Pts',(-0.118079107988355,1.,-2.102015121329));
#34734=CARTESIAN_POINT('Ctrl Pts',(-0.120570567965122,-1.,-2.0962529286773));
#34735=CARTESIAN_POINT('Ctrl Pts',(-0.120570567965122,1.,-2.0962529286773));
#34736=CARTESIAN_POINT('Ctrl Pts',(-0.123018905621083,-1.,-2.09048392424825));
#34737=CARTESIAN_POINT('Ctrl Pts',(-0.123018905621083,1.,-2.09048392424825));
#34738=CARTESIAN_POINT('Ctrl Pts',(-0.125423679412061,-1.,-2.08470840653643));
#34739=CARTESIAN_POINT('Ctrl Pts',(-0.125423679412061,1.,-2.08470840653643));
#34740=CARTESIAN_POINT('Ctrl Pts',(-0.12778444527612,-1.,-2.07892715110987));
#34741=CARTESIAN_POINT('Ctrl Pts',(-0.12778444527612,1.,-2.07892715110987));
#34742=CARTESIAN_POINT('Ctrl Pts',(-0.130100748328403,-1.,-2.07314114713063));
#34743=CARTESIAN_POINT('Ctrl Pts',(-0.130100748328403,1.,-2.07314114713063));
#34744=CARTESIAN_POINT('Ctrl Pts',(-0.13237211154771,-1.,-2.06735123910326));
#34745=CARTESIAN_POINT('Ctrl Pts',(-0.13237211154771,1.,-2.06735123910326));
#34746=CARTESIAN_POINT('Ctrl Pts',(-0.134598026192106,-1.,-2.06155781517842));
#34747=CARTESIAN_POINT('Ctrl Pts',(-0.134598026192106,1.,-2.06155781517842));
#34748=CARTESIAN_POINT('Ctrl Pts',(-0.136777941218044,-1.,-2.05576044414264));
#34749=CARTESIAN_POINT('Ctrl Pts',(-0.136777941218044,1.,-2.05576044414264));
#34750=CARTESIAN_POINT('Ctrl Pts',(-0.138911255368966,-1.,-2.04995762001328));
#34751=CARTESIAN_POINT('Ctrl Pts',(-0.138911255368966,1.,-2.04995762001328));
#34752=CARTESIAN_POINT('Ctrl Pts',(-0.140997332152546,-1.,-2.04414757947916));
#34753=CARTESIAN_POINT('Ctrl Pts',(-0.140997332152546,1.,-2.04414757947916));
#34754=CARTESIAN_POINT('Ctrl Pts',(-0.143035515058209,-1.,-2.03832911025912));
#34755=CARTESIAN_POINT('Ctrl Pts',(-0.143035515058209,1.,-2.03832911025912));
#34756=CARTESIAN_POINT('Ctrl Pts',(-0.145025140186057,-1.,-2.03250223739942));
#34757=CARTESIAN_POINT('Ctrl Pts',(-0.145025140186057,1.,-2.03250223739942));
#34758=CARTESIAN_POINT('Ctrl Pts',(-0.146965557332583,-1.,-2.02666926182017));
#34759=CARTESIAN_POINT('Ctrl Pts',(-0.146965557332583,1.,-2.02666926182017));
#34760=CARTESIAN_POINT('Ctrl Pts',(-0.148856124775337,-1.,-2.02083464969894));
#34761=CARTESIAN_POINT('Ctrl Pts',(-0.148856124775337,1.,-2.02083464969894));
#34762=CARTESIAN_POINT('Ctrl Pts',(-0.150696157673078,-1.,-2.01500291940238));
#34763=CARTESIAN_POINT('Ctrl Pts',(-0.150696157673078,1.,-2.01500291940238));
#34764=CARTESIAN_POINT('Ctrl Pts',(-0.15248488362145,-1.,-2.00917680318424));
#34765=CARTESIAN_POINT('Ctrl Pts',(-0.15248488362145,1.,-2.00917680318424));
#34766=CARTESIAN_POINT('Ctrl Pts',(-0.154221403049722,-1.,-2.00335565310543));
#34767=CARTESIAN_POINT('Ctrl Pts',(-0.154221403049722,1.,-2.00335565310543));
#34768=CARTESIAN_POINT('Ctrl Pts',(-0.155904629548783,-1.,-1.99753284771497));
#34769=CARTESIAN_POINT('Ctrl Pts',(-0.155904629548783,1.,-1.99753284771497));
#34770=CARTESIAN_POINT('Ctrl Pts',(-0.157533331459227,-1.,-1.99169810931908));
#34771=CARTESIAN_POINT('Ctrl Pts',(-0.157533331459227,1.,-1.99169810931908));
#34772=CARTESIAN_POINT('Ctrl Pts',(-0.159106226437299,-1.,-1.98584238283292));
#34773=CARTESIAN_POINT('Ctrl Pts',(-0.159106226437299,1.,-1.98584238283292));
#34774=CARTESIAN_POINT('Ctrl Pts',(-0.160622060784611,-1.,-1.97996195437559));
#34775=CARTESIAN_POINT('Ctrl Pts',(-0.160622060784611,1.,-1.97996195437559));
#34776=CARTESIAN_POINT('Ctrl Pts',(-0.162079693556289,-1.,-1.97406280235188));
#34777=CARTESIAN_POINT('Ctrl Pts',(-0.162079693556289,1.,-1.97406280235188));
#34778=CARTESIAN_POINT('Ctrl Pts',(-0.163478185457734,-1.,-1.96816512677967));
#34779=CARTESIAN_POINT('Ctrl Pts',(-0.163478185457734,1.,-1.96816512677967));
#34780=CARTESIAN_POINT('Ctrl Pts',(-0.164816568920269,-1.,-1.96229379940136));
#34781=CARTESIAN_POINT('Ctrl Pts',(-0.164816568920269,1.,-1.96229379940136));
#34782=CARTESIAN_POINT('Ctrl Pts',(-0.166093592002812,-1.,-1.9564675971873));
#34783=CARTESIAN_POINT('Ctrl Pts',(-0.166093592002812,1.,-1.9564675971873));
#34784=CARTESIAN_POINT('Ctrl Pts',(-0.167307501784475,-1.,-1.95069027794294));
#34785=CARTESIAN_POINT('Ctrl Pts',(-0.167307501784475,1.,-1.95069027794294));
#34786=CARTESIAN_POINT('Ctrl Pts',(-0.168455741607556,-1.,-1.94493757756931));
#34787=CARTESIAN_POINT('Ctrl Pts',(-0.168455741607556,1.,-1.94493757756931));
#34788=CARTESIAN_POINT('Ctrl Pts',(-0.169534904817491,-1.,-1.93915639211581));
#34789=CARTESIAN_POINT('Ctrl Pts',(-0.169534904817491,1.,-1.93915639211581));
#34790=CARTESIAN_POINT('Ctrl Pts',(-0.170541253116202,-1.,-1.93329183155539));
#34791=CARTESIAN_POINT('Ctrl Pts',(-0.170541253116202,1.,-1.93329183155539));
#34792=CARTESIAN_POINT('Ctrl Pts',(-0.171471191532988,-1.,-1.92731093582036));
#34793=CARTESIAN_POINT('Ctrl Pts',(-0.171471191532988,1.,-1.92731093582036));
#34794=CARTESIAN_POINT('Ctrl Pts',(-0.172321621259514,-1.,-1.9212233439798));
#34795=CARTESIAN_POINT('Ctrl Pts',(-0.172321621259514,1.,-1.9212233439798));
#34796=CARTESIAN_POINT('Ctrl Pts',(-0.173090695383496,-1.,-1.91511429159527));
#34797=CARTESIAN_POINT('Ctrl Pts',(-0.173090695383496,1.,-1.91511429159527));
#34798=CARTESIAN_POINT('Ctrl Pts',(-0.173776635257817,-1.,-1.90911693975267));
#34799=CARTESIAN_POINT('Ctrl Pts',(-0.173776635257817,1.,-1.90911693975267));
#34800=CARTESIAN_POINT('Ctrl Pts',(-0.174375518661085,-1.,-1.90335253862834));
#34801=CARTESIAN_POINT('Ctrl Pts',(-0.174375518661085,1.,-1.90335253862834));
#34802=CARTESIAN_POINT('Ctrl Pts',(-0.174879405091263,-1.,-1.89788101117132));
#34803=CARTESIAN_POINT('Ctrl Pts',(-0.174879405091263,1.,-1.89788101117132));
#34804=CARTESIAN_POINT('Ctrl Pts',(-0.175274276190844,-1.,-1.892646301985));
#34805=CARTESIAN_POINT('Ctrl Pts',(-0.175274276190844,1.,-1.892646301985));
#34806=CARTESIAN_POINT('Ctrl Pts',(-0.175538155840648,-1.,-1.88742606273259));
#34807=CARTESIAN_POINT('Ctrl Pts',(-0.175538155840648,1.,-1.88742606273259));
#34808=CARTESIAN_POINT('Ctrl Pts',(-0.175644148889699,-1.,-1.88188663145367));
#34809=CARTESIAN_POINT('Ctrl Pts',(-0.175644148889699,1.,-1.88188663145367));
#34810=CARTESIAN_POINT('Ctrl Pts',(-0.175563480746485,-1.,-1.87563767773588));
#34811=CARTESIAN_POINT('Ctrl Pts',(-0.175563480746485,1.,-1.87563767773588));
#34812=CARTESIAN_POINT('Ctrl Pts',(-0.175268337590758,-1.,-1.86828349694799));
#34813=CARTESIAN_POINT('Ctrl Pts',(-0.175268337590758,1.,-1.86828349694799));
#34814=CARTESIAN_POINT('Ctrl Pts',(-0.17473525927603,-1.,-1.85948367088837));
#34815=CARTESIAN_POINT('Ctrl Pts',(-0.17473525927603,1.,-1.85948367088837));
#34816=CARTESIAN_POINT('Ctrl Pts',(-0.173946627587731,-1.,-1.8489811319852));
#34817=CARTESIAN_POINT('Ctrl Pts',(-0.173946627587731,1.,-1.8489811319852));
#34818=CARTESIAN_POINT('Ctrl Pts',(-0.1728894428919,-1.,-1.83658380527692));
#34819=CARTESIAN_POINT('Ctrl Pts',(-0.1728894428919,1.,-1.83658380527692));
#34820=CARTESIAN_POINT('Ctrl Pts',(-0.171554770204119,-1.,-1.82215766811545));
#34821=CARTESIAN_POINT('Ctrl Pts',(-0.171554770204119,1.,-1.82215766811545));
#34822=CARTESIAN_POINT('Ctrl Pts',(-0.169936923904608,-1.,-1.80561530629706));
#34823=CARTESIAN_POINT('Ctrl Pts',(-0.169936923904608,1.,-1.80561530629706));
#34824=CARTESIAN_POINT('Ctrl Pts',(-0.168032772805197,-1.,-1.7869064998507));
#34825=CARTESIAN_POINT('Ctrl Pts',(-0.168032772805197,1.,-1.7869064998507));
#34826=CARTESIAN_POINT('Ctrl Pts',(-0.1662793551464,-1.,-1.77018771684844));
#34827=CARTESIAN_POINT('Ctrl Pts',(-0.1662793551464,1.,-1.77018771684844));
#34828=CARTESIAN_POINT('Ctrl Pts',(-0.164834765707158,-1.,-1.75666056638427));
#34829=CARTESIAN_POINT('Ctrl Pts',(-0.164834765707158,1.,-1.75666056638427));
#34830=CARTESIAN_POINT('Ctrl Pts',(-0.163814161002002,-1.,-1.7472034950333));
#34831=CARTESIAN_POINT('Ctrl Pts',(-0.163814161002002,1.,-1.7472034950333));
#34832=CARTESIAN_POINT('Ctrl Pts',(-0.163289472382896,-1.,-1.74236521665491));
#34833=CARTESIAN_POINT('Ctrl Pts',(-0.163289472382896,1.,-1.74236521665491));
#34834=CARTESIAN_POINT('',(-0.0694764450219581,1.,-2.19890268624765));
#34835=CARTESIAN_POINT('Ctrl Pts',(-0.0694764450219581,1.,-2.19890268624765));
#34836=CARTESIAN_POINT('Ctrl Pts',(-0.070114353632549,1.,-2.19777582085423));
#34837=CARTESIAN_POINT('Ctrl Pts',(-0.0713863779526154,1.,-2.19552129484002));
#34838=CARTESIAN_POINT('Ctrl Pts',(-0.0732830357306725,1.,-2.19213712013662));
#34839=CARTESIAN_POINT('Ctrl Pts',(-0.0757891465836148,1.,-2.1876201139953));
#34840=CARTESIAN_POINT('Ctrl Pts',(-0.0788837727685243,1.,-2.18196589448887));
#34841=CARTESIAN_POINT('Ctrl Pts',(-0.0819402680872765,1.,-2.176303712113));
#34842=CARTESIAN_POINT('Ctrl Pts',(-0.0849584620835372,1.,-2.17063357870952));
#34843=CARTESIAN_POINT('Ctrl Pts',(-0.0879381291386923,1.,-2.16495552645014));
#34844=CARTESIAN_POINT('Ctrl Pts',(-0.0908789888107265,1.,-2.15926961544516));
#34845=CARTESIAN_POINT('Ctrl Pts',(-0.0937807218867643,1.,-2.1535759397817));
#34846=CARTESIAN_POINT('Ctrl Pts',(-0.0966429852305459,1.,-2.14787463531795));
#34847=CARTESIAN_POINT('Ctrl Pts',(-0.0994654261990915,1.,-2.14216588396025));
#34848=CARTESIAN_POINT('Ctrl Pts',(-0.1022477005561,1.,-2.13644992667165));
#34849=CARTESIAN_POINT('Ctrl Pts',(-0.104989479152739,1.,-2.13072704887293));
#34850=CARTESIAN_POINT('Ctrl Pts',(-0.10769043523109,1.,-2.12499752307));
#34851=CARTESIAN_POINT('Ctrl Pts',(-0.110350236135025,1.,-2.11926155590865));
#34852=CARTESIAN_POINT('Ctrl Pts',(-0.112968534419737,1.,-2.11351924490306));
#34853=CARTESIAN_POINT('Ctrl Pts',(-0.115544957687926,1.,-2.10777050261309));
#34854=CARTESIAN_POINT('Ctrl Pts',(-0.118079107988355,1.,-2.102015121329));
#34855=CARTESIAN_POINT('Ctrl Pts',(-0.120570567965122,1.,-2.0962529286773));
#34856=CARTESIAN_POINT('Ctrl Pts',(-0.123018905621083,1.,-2.09048392424825));
#34857=CARTESIAN_POINT('Ctrl Pts',(-0.125423679412061,1.,-2.08470840653643));
#34858=CARTESIAN_POINT('Ctrl Pts',(-0.12778444527612,1.,-2.07892715110987));
#34859=CARTESIAN_POINT('Ctrl Pts',(-0.130100748328403,1.,-2.07314114713063));
#34860=CARTESIAN_POINT('Ctrl Pts',(-0.13237211154771,1.,-2.06735123910326));
#34861=CARTESIAN_POINT('Ctrl Pts',(-0.134598026192106,1.,-2.06155781517842));
#34862=CARTESIAN_POINT('Ctrl Pts',(-0.136777941218044,1.,-2.05576044414264));
#34863=CARTESIAN_POINT('Ctrl Pts',(-0.138911255368966,1.,-2.04995762001328));
#34864=CARTESIAN_POINT('Ctrl Pts',(-0.140997332152546,1.,-2.04414757947916));
#34865=CARTESIAN_POINT('Ctrl Pts',(-0.143035515058209,1.,-2.03832911025912));
#34866=CARTESIAN_POINT('Ctrl Pts',(-0.145025140186057,1.,-2.03250223739942));
#34867=CARTESIAN_POINT('Ctrl Pts',(-0.146965557332583,1.,-2.02666926182017));
#34868=CARTESIAN_POINT('Ctrl Pts',(-0.148856124775337,1.,-2.02083464969894));
#34869=CARTESIAN_POINT('Ctrl Pts',(-0.150696157673078,1.,-2.01500291940238));
#34870=CARTESIAN_POINT('Ctrl Pts',(-0.15248488362145,1.,-2.00917680318424));
#34871=CARTESIAN_POINT('Ctrl Pts',(-0.154221403049722,1.,-2.00335565310543));
#34872=CARTESIAN_POINT('Ctrl Pts',(-0.155904629548783,1.,-1.99753284771497));
#34873=CARTESIAN_POINT('Ctrl Pts',(-0.157533331459227,1.,-1.99169810931908));
#34874=CARTESIAN_POINT('Ctrl Pts',(-0.159106226437299,1.,-1.98584238283292));
#34875=CARTESIAN_POINT('Ctrl Pts',(-0.160622060784611,1.,-1.97996195437559));
#34876=CARTESIAN_POINT('Ctrl Pts',(-0.162079693556289,1.,-1.97406280235188));
#34877=CARTESIAN_POINT('Ctrl Pts',(-0.163478185457734,1.,-1.96816512677967));
#34878=CARTESIAN_POINT('Ctrl Pts',(-0.164816568920269,1.,-1.96229379940136));
#34879=CARTESIAN_POINT('Ctrl Pts',(-0.166093592002812,1.,-1.9564675971873));
#34880=CARTESIAN_POINT('Ctrl Pts',(-0.167307501784475,1.,-1.95069027794294));
#34881=CARTESIAN_POINT('Ctrl Pts',(-0.168455741607556,1.,-1.94493757756931));
#34882=CARTESIAN_POINT('Ctrl Pts',(-0.169534904817491,1.,-1.93915639211581));
#34883=CARTESIAN_POINT('Ctrl Pts',(-0.170541253116202,1.,-1.93329183155539));
#34884=CARTESIAN_POINT('Ctrl Pts',(-0.171471191532988,1.,-1.92731093582036));
#34885=CARTESIAN_POINT('Ctrl Pts',(-0.172321621259514,1.,-1.9212233439798));
#34886=CARTESIAN_POINT('Ctrl Pts',(-0.173090695383496,1.,-1.91511429159527));
#34887=CARTESIAN_POINT('Ctrl Pts',(-0.173776635257817,1.,-1.90911693975267));
#34888=CARTESIAN_POINT('Ctrl Pts',(-0.174375518661085,1.,-1.90335253862834));
#34889=CARTESIAN_POINT('Ctrl Pts',(-0.174879405091263,1.,-1.89788101117132));
#34890=CARTESIAN_POINT('Ctrl Pts',(-0.175274276190844,1.,-1.892646301985));
#34891=CARTESIAN_POINT('Ctrl Pts',(-0.175538155840648,1.,-1.88742606273259));
#34892=CARTESIAN_POINT('Ctrl Pts',(-0.175644148889699,1.,-1.88188663145367));
#34893=CARTESIAN_POINT('Ctrl Pts',(-0.175563480746485,1.,-1.87563767773588));
#34894=CARTESIAN_POINT('Ctrl Pts',(-0.175268337590758,1.,-1.86828349694799));
#34895=CARTESIAN_POINT('Ctrl Pts',(-0.17473525927603,1.,-1.85948367088837));
#34896=CARTESIAN_POINT('Ctrl Pts',(-0.173946627587731,1.,-1.8489811319852));
#34897=CARTESIAN_POINT('Ctrl Pts',(-0.1728894428919,1.,-1.83658380527692));
#34898=CARTESIAN_POINT('Ctrl Pts',(-0.171554770204119,1.,-1.82215766811545));
#34899=CARTESIAN_POINT('Ctrl Pts',(-0.169936923904608,1.,-1.80561530629706));
#34900=CARTESIAN_POINT('Ctrl Pts',(-0.168032772805197,1.,-1.7869064998507));
#34901=CARTESIAN_POINT('Ctrl Pts',(-0.1662793551464,1.,-1.77018771684844));
#34902=CARTESIAN_POINT('Ctrl Pts',(-0.164834765707158,1.,-1.75666056638427));
#34903=CARTESIAN_POINT('Ctrl Pts',(-0.163814161002002,1.,-1.7472034950333));
#34904=CARTESIAN_POINT('Ctrl Pts',(-0.163289472382896,1.,-1.74236521665491));
#34905=CARTESIAN_POINT('',(-0.0694764450219581,0.,-2.19890268624765));
#34906=CARTESIAN_POINT('Origin',(0.0694764450219584,0.,-2.19890268624765));
#34907=CARTESIAN_POINT('',(0.0694764450219584,1.,-2.19890268624765));
#34908=CARTESIAN_POINT('',(-0.0694764450219581,1.,-2.19890268624765));
#34909=CARTESIAN_POINT('',(0.0694764450219584,0.,-2.19890268624765));
#34910=CARTESIAN_POINT('Ctrl Pts',(0.163289472382896,-1.,-1.74236521665491));
#34911=CARTESIAN_POINT('Ctrl Pts',(0.163289472382896,1.,-1.74236521665491));
#34912=CARTESIAN_POINT('Ctrl Pts',(0.163814161002474,-1.,-1.74720349503904));
#34913=CARTESIAN_POINT('Ctrl Pts',(0.163814161002474,1.,-1.74720349503904));
#34914=CARTESIAN_POINT('Ctrl Pts',(0.164834765708484,-1.,-1.75666056640041));
#34915=CARTESIAN_POINT('Ctrl Pts',(0.164834765708484,1.,-1.75666056640041));
#34916=CARTESIAN_POINT('Ctrl Pts',(0.166279355148738,-1.,-1.77018771687692));
#34917=CARTESIAN_POINT('Ctrl Pts',(0.166279355148738,1.,-1.77018771687692));
#34918=CARTESIAN_POINT('Ctrl Pts',(0.16803277280837,-1.,-1.78690649988931));
#34919=CARTESIAN_POINT('Ctrl Pts',(0.16803277280837,1.,-1.78690649988931));
#34920=CARTESIAN_POINT('Ctrl Pts',(0.169936923908078,-1.,-1.80561530633924));
#34921=CARTESIAN_POINT('Ctrl Pts',(0.169936923908078,1.,-1.80561530633924));
#34922=CARTESIAN_POINT('Ctrl Pts',(0.171554770207306,-1.,-1.82215766815414));
#34923=CARTESIAN_POINT('Ctrl Pts',(0.171554770207306,1.,-1.82215766815414));
#34924=CARTESIAN_POINT('Ctrl Pts',(0.17288944289442,-1.,-1.83658380530747));
#34925=CARTESIAN_POINT('Ctrl Pts',(0.17288944289442,1.,-1.83658380530747));
#34926=CARTESIAN_POINT('Ctrl Pts',(0.173946627589401,-1.,-1.84898113200543));
#34927=CARTESIAN_POINT('Ctrl Pts',(0.173946627589401,1.,-1.84898113200543));
#34928=CARTESIAN_POINT('Ctrl Pts',(0.174735259276856,-1.,-1.85948367089838));
#34929=CARTESIAN_POINT('Ctrl Pts',(0.174735259276856,1.,-1.85948367089838));
#34930=CARTESIAN_POINT('Ctrl Pts',(0.175268337590901,-1.,-1.86828349694972));
#34931=CARTESIAN_POINT('Ctrl Pts',(0.175268337590901,1.,-1.86828349694972));
#34932=CARTESIAN_POINT('Ctrl Pts',(0.175563480746205,-1.,-1.87563767773249));
#34933=CARTESIAN_POINT('Ctrl Pts',(0.175563480746205,1.,-1.87563767773249));
#34934=CARTESIAN_POINT('Ctrl Pts',(0.175644148889271,-1.,-1.88188663144846));
#34935=CARTESIAN_POINT('Ctrl Pts',(0.175644148889271,1.,-1.88188663144846));
#34936=CARTESIAN_POINT('Ctrl Pts',(0.175538155840286,-1.,-1.88742606272818));
#34937=CARTESIAN_POINT('Ctrl Pts',(0.175538155840286,1.,-1.88742606272818));
#34938=CARTESIAN_POINT('Ctrl Pts',(0.175274276190664,-1.,-1.89264630198279));
#34939=CARTESIAN_POINT('Ctrl Pts',(0.175274276190664,1.,-1.89264630198279));
#34940=CARTESIAN_POINT('Ctrl Pts',(0.174879405091277,-1.,-1.89788101117148));
#34941=CARTESIAN_POINT('Ctrl Pts',(0.174879405091277,1.,-1.89788101117148));
#34942=CARTESIAN_POINT('Ctrl Pts',(0.174375518661222,-1.,-1.90335253863003));
#34943=CARTESIAN_POINT('Ctrl Pts',(0.174375518661222,1.,-1.90335253863003));
#34944=CARTESIAN_POINT('Ctrl Pts',(0.173776635257984,-1.,-1.90911693975475));
#34945=CARTESIAN_POINT('Ctrl Pts',(0.173776635257984,1.,-1.90911693975475));
#34946=CARTESIAN_POINT('Ctrl Pts',(0.173090695383619,-1.,-1.91511429159681));
#34947=CARTESIAN_POINT('Ctrl Pts',(0.173090695383619,1.,-1.91511429159681));
#34948=CARTESIAN_POINT('Ctrl Pts',(0.172321621259557,-1.,-1.92122334398034));
#34949=CARTESIAN_POINT('Ctrl Pts',(0.172321621259557,1.,-1.92122334398034));
#34950=CARTESIAN_POINT('Ctrl Pts',(0.17147119153296,-1.,-1.92731093582));
#34951=CARTESIAN_POINT('Ctrl Pts',(0.17147119153296,1.,-1.92731093582));
#34952=CARTESIAN_POINT('Ctrl Pts',(0.170541253116136,-1.,-1.93329183155455));
#34953=CARTESIAN_POINT('Ctrl Pts',(0.170541253116136,1.,-1.93329183155455));
#34954=CARTESIAN_POINT('Ctrl Pts',(0.169534904817425,-1.,-1.93915639211497));
#34955=CARTESIAN_POINT('Ctrl Pts',(0.169534904817425,1.,-1.93915639211497));
#34956=CARTESIAN_POINT('Ctrl Pts',(0.168455741607516,-1.,-1.94493757756879));
#34957=CARTESIAN_POINT('Ctrl Pts',(0.168455741607516,1.,-1.94493757756879));
#34958=CARTESIAN_POINT('Ctrl Pts',(0.167307501784469,-1.,-1.95069027794286));
#34959=CARTESIAN_POINT('Ctrl Pts',(0.167307501784469,1.,-1.95069027794286));
#34960=CARTESIAN_POINT('Ctrl Pts',(0.166093592002833,-1.,-1.95646759718755));
#34961=CARTESIAN_POINT('Ctrl Pts',(0.166093592002833,1.,-1.95646759718755));
#34962=CARTESIAN_POINT('Ctrl Pts',(0.1648165689203,-1.,-1.96229379940174));
#34963=CARTESIAN_POINT('Ctrl Pts',(0.1648165689203,1.,-1.96229379940174));
#34964=CARTESIAN_POINT('Ctrl Pts',(0.16347818545776,-1.,-1.96816512678));
#34965=CARTESIAN_POINT('Ctrl Pts',(0.16347818545776,1.,-1.96816512678));
#34966=CARTESIAN_POINT('Ctrl Pts',(0.162079693556302,-1.,-1.97406280235204));
#34967=CARTESIAN_POINT('Ctrl Pts',(0.162079693556302,1.,-1.97406280235204));
#34968=CARTESIAN_POINT('Ctrl Pts',(0.16062206078461,-1.,-1.97996195437557));
#34969=CARTESIAN_POINT('Ctrl Pts',(0.16062206078461,1.,-1.97996195437557));
#34970=CARTESIAN_POINT('Ctrl Pts',(0.159106226437288,-1.,-1.98584238283279));
#34971=CARTESIAN_POINT('Ctrl Pts',(0.159106226437288,1.,-1.98584238283279));
#34972=CARTESIAN_POINT('Ctrl Pts',(0.157533331459215,-1.,-1.99169810931893));
#34973=CARTESIAN_POINT('Ctrl Pts',(0.157533331459215,1.,-1.99169810931893));
#34974=CARTESIAN_POINT('Ctrl Pts',(0.155904629548774,-1.,-1.99753284771487));
#34975=CARTESIAN_POINT('Ctrl Pts',(0.155904629548774,1.,-1.99753284771487));
#34976=CARTESIAN_POINT('Ctrl Pts',(0.154221403049719,-1.,-2.00335565310539));
#34977=CARTESIAN_POINT('Ctrl Pts',(0.154221403049719,1.,-2.00335565310539));
#34978=CARTESIAN_POINT('Ctrl Pts',(0.152484883621452,-1.,-2.00917680318426));
#34979=CARTESIAN_POINT('Ctrl Pts',(0.152484883621452,1.,-2.00917680318426));
#34980=CARTESIAN_POINT('Ctrl Pts',(0.150696157673084,-1.,-2.01500291940243));
#34981=CARTESIAN_POINT('Ctrl Pts',(0.150696157673084,1.,-2.01500291940243));
#34982=CARTESIAN_POINT('Ctrl Pts',(0.148856124775343,-1.,-2.02083464969897));
#34983=CARTESIAN_POINT('Ctrl Pts',(0.148856124775343,1.,-2.02083464969897));
#34984=CARTESIAN_POINT('Ctrl Pts',(0.146965557332586,-1.,-2.02666926182017));
#34985=CARTESIAN_POINT('Ctrl Pts',(0.146965557332586,1.,-2.02666926182017));
#34986=CARTESIAN_POINT('Ctrl Pts',(0.145025140186058,-1.,-2.03250223739941));
#34987=CARTESIAN_POINT('Ctrl Pts',(0.145025140186058,1.,-2.03250223739941));
#34988=CARTESIAN_POINT('Ctrl Pts',(0.143035515058208,-1.,-2.03832911025913));
#34989=CARTESIAN_POINT('Ctrl Pts',(0.143035515058208,1.,-2.03832911025913));
#34990=CARTESIAN_POINT('Ctrl Pts',(0.140997332152545,-1.,-2.04414757947919));
#34991=CARTESIAN_POINT('Ctrl Pts',(0.140997332152545,1.,-2.04414757947919));
#34992=CARTESIAN_POINT('Ctrl Pts',(0.138911255368966,-1.,-2.04995762001333));
#34993=CARTESIAN_POINT('Ctrl Pts',(0.138911255368966,1.,-2.04995762001333));
#34994=CARTESIAN_POINT('Ctrl Pts',(0.136777941218044,-1.,-2.0557604441427));
#34995=CARTESIAN_POINT('Ctrl Pts',(0.136777941218044,1.,-2.0557604441427));
#34996=CARTESIAN_POINT('Ctrl Pts',(0.134598026192107,-1.,-2.06155781517844));
#34997=CARTESIAN_POINT('Ctrl Pts',(0.134598026192107,1.,-2.06155781517844));
#34998=CARTESIAN_POINT('Ctrl Pts',(0.13237211154771,-1.,-2.06735123910319));
#34999=CARTESIAN_POINT('Ctrl Pts',(0.13237211154771,1.,-2.06735123910319));
#35000=CARTESIAN_POINT('Ctrl Pts',(0.1301007483284,-1.,-2.07314114713047));
#35001=CARTESIAN_POINT('Ctrl Pts',(0.1301007483284,1.,-2.07314114713047));
#35002=CARTESIAN_POINT('Ctrl Pts',(0.127784445276116,-1.,-2.07892715110967));
#35003=CARTESIAN_POINT('Ctrl Pts',(0.127784445276116,1.,-2.07892715110967));
#35004=CARTESIAN_POINT('Ctrl Pts',(0.125423679412058,-1.,-2.08470840653628));
#35005=CARTESIAN_POINT('Ctrl Pts',(0.125423679412058,1.,-2.08470840653628));
#35006=CARTESIAN_POINT('Ctrl Pts',(0.123018905621083,-1.,-2.09048392424826));
#35007=CARTESIAN_POINT('Ctrl Pts',(0.123018905621083,1.,-2.09048392424826));
#35008=CARTESIAN_POINT('Ctrl Pts',(0.120570567965129,-1.,-2.09625292867756));
#35009=CARTESIAN_POINT('Ctrl Pts',(0.120570567965129,1.,-2.09625292867756));
#35010=CARTESIAN_POINT('Ctrl Pts',(0.118079107988368,-1.,-2.10201512132945));
#35011=CARTESIAN_POINT('Ctrl Pts',(0.118079107988368,1.,-2.10201512132945));
#35012=CARTESIAN_POINT('Ctrl Pts',(0.11554495768794,-1.,-2.10777050261359));
#35013=CARTESIAN_POINT('Ctrl Pts',(0.11554495768794,1.,-2.10777050261359));
#35014=CARTESIAN_POINT('Ctrl Pts',(0.112968534419746,-1.,-2.11351924490335));
#35015=CARTESIAN_POINT('Ctrl Pts',(0.112968534419746,1.,-2.11351924490335));
#35016=CARTESIAN_POINT('Ctrl Pts',(0.11035023613502,-1.,-2.11926155590849));
#35017=CARTESIAN_POINT('Ctrl Pts',(0.11035023613502,1.,-2.11926155590849));
#35018=CARTESIAN_POINT('Ctrl Pts',(0.107690435231068,-1.,-2.12499752306927));
#35019=CARTESIAN_POINT('Ctrl Pts',(0.107690435231068,1.,-2.12499752306927));
#35020=CARTESIAN_POINT('Ctrl Pts',(0.104989479152703,-1.,-2.1307270488718));
#35021=CARTESIAN_POINT('Ctrl Pts',(0.104989479152703,1.,-2.1307270488718));
#35022=CARTESIAN_POINT('Ctrl Pts',(0.102247700556064,-1.,-2.13644992667052));
#35023=CARTESIAN_POINT('Ctrl Pts',(0.102247700556064,1.,-2.13644992667052));
#35024=CARTESIAN_POINT('Ctrl Pts',(0.0994654261990743,-1.,-2.14216588395974));
#35025=CARTESIAN_POINT('Ctrl Pts',(0.0994654261990743,1.,-2.14216588395974));
#35026=CARTESIAN_POINT('Ctrl Pts',(0.0966429852305689,-1.,-2.14787463531864));
#35027=CARTESIAN_POINT('Ctrl Pts',(0.0966429852305689,1.,-2.14787463531864));
#35028=CARTESIAN_POINT('Ctrl Pts',(0.0937807218868345,-1.,-2.15357593978377));
#35029=CARTESIAN_POINT('Ctrl Pts',(0.0937807218868345,1.,-2.15357593978377));
#35030=CARTESIAN_POINT('Ctrl Pts',(0.0908789888108266,-1.,-2.15926961544808));
#35031=CARTESIAN_POINT('Ctrl Pts',(0.0908789888108266,1.,-2.15926961544808));
#35032=CARTESIAN_POINT('Ctrl Pts',(0.0879381291387823,-1.,-2.16495552645275));
#35033=CARTESIAN_POINT('Ctrl Pts',(0.0879381291387823,1.,-2.16495552645275));
#35034=CARTESIAN_POINT('Ctrl Pts',(0.0849584620835643,-1.,-2.17063357871031));
#35035=CARTESIAN_POINT('Ctrl Pts',(0.0849584620835643,1.,-2.17063357871031));
#35036=CARTESIAN_POINT('Ctrl Pts',(0.0819402680871939,-1.,-2.1763037121106));
#35037=CARTESIAN_POINT('Ctrl Pts',(0.0819402680871939,1.,-2.1763037121106));
#35038=CARTESIAN_POINT('Ctrl Pts',(0.0788837727683228,-1.,-2.18196589448304));
#35039=CARTESIAN_POINT('Ctrl Pts',(0.0788837727683228,1.,-2.18196589448304));
#35040=CARTESIAN_POINT('Ctrl Pts',(0.0757891465833411,-1.,-2.1876201139874));
#35041=CARTESIAN_POINT('Ctrl Pts',(0.0757891465833411,1.,-2.1876201139874));
#35042=CARTESIAN_POINT('Ctrl Pts',(0.0732830357304276,-1.,-2.19213712012956));
#35043=CARTESIAN_POINT('Ctrl Pts',(0.0732830357304276,1.,-2.19213712012956));
#35044=CARTESIAN_POINT('Ctrl Pts',(0.0713863779524627,-1.,-2.19552129483562));
#35045=CARTESIAN_POINT('Ctrl Pts',(0.0713863779524627,1.,-2.19552129483562));
#35046=CARTESIAN_POINT('Ctrl Pts',(0.0701143536324926,-1.,-2.19777582085261));
#35047=CARTESIAN_POINT('Ctrl Pts',(0.0701143536324926,1.,-2.19777582085261));
#35048=CARTESIAN_POINT('Ctrl Pts',(0.0694764450219584,-1.,-2.19890268624765));
#35049=CARTESIAN_POINT('Ctrl Pts',(0.0694764450219584,1.,-2.19890268624765));
#35050=CARTESIAN_POINT('',(0.163289472382896,1.,-1.74236521665491));
#35051=CARTESIAN_POINT('Ctrl Pts',(0.163289472382896,1.,-1.74236521665491));
#35052=CARTESIAN_POINT('Ctrl Pts',(0.163814161002474,1.,-1.74720349503904));
#35053=CARTESIAN_POINT('Ctrl Pts',(0.164834765708484,1.,-1.75666056640041));
#35054=CARTESIAN_POINT('Ctrl Pts',(0.166279355148738,1.,-1.77018771687692));
#35055=CARTESIAN_POINT('Ctrl Pts',(0.16803277280837,1.,-1.78690649988931));
#35056=CARTESIAN_POINT('Ctrl Pts',(0.169936923908078,1.,-1.80561530633924));
#35057=CARTESIAN_POINT('Ctrl Pts',(0.171554770207306,1.,-1.82215766815414));
#35058=CARTESIAN_POINT('Ctrl Pts',(0.17288944289442,1.,-1.83658380530747));
#35059=CARTESIAN_POINT('Ctrl Pts',(0.173946627589401,1.,-1.84898113200543));
#35060=CARTESIAN_POINT('Ctrl Pts',(0.174735259276856,1.,-1.85948367089838));
#35061=CARTESIAN_POINT('Ctrl Pts',(0.175268337590901,1.,-1.86828349694972));
#35062=CARTESIAN_POINT('Ctrl Pts',(0.175563480746205,1.,-1.87563767773249));
#35063=CARTESIAN_POINT('Ctrl Pts',(0.175644148889271,1.,-1.88188663144846));
#35064=CARTESIAN_POINT('Ctrl Pts',(0.175538155840286,1.,-1.88742606272818));
#35065=CARTESIAN_POINT('Ctrl Pts',(0.175274276190664,1.,-1.89264630198279));
#35066=CARTESIAN_POINT('Ctrl Pts',(0.174879405091277,1.,-1.89788101117148));
#35067=CARTESIAN_POINT('Ctrl Pts',(0.174375518661222,1.,-1.90335253863003));
#35068=CARTESIAN_POINT('Ctrl Pts',(0.173776635257984,1.,-1.90911693975475));
#35069=CARTESIAN_POINT('Ctrl Pts',(0.173090695383619,1.,-1.91511429159681));
#35070=CARTESIAN_POINT('Ctrl Pts',(0.172321621259557,1.,-1.92122334398034));
#35071=CARTESIAN_POINT('Ctrl Pts',(0.17147119153296,1.,-1.92731093582));
#35072=CARTESIAN_POINT('Ctrl Pts',(0.170541253116136,1.,-1.93329183155455));
#35073=CARTESIAN_POINT('Ctrl Pts',(0.169534904817425,1.,-1.93915639211497));
#35074=CARTESIAN_POINT('Ctrl Pts',(0.168455741607516,1.,-1.94493757756879));
#35075=CARTESIAN_POINT('Ctrl Pts',(0.167307501784469,1.,-1.95069027794286));
#35076=CARTESIAN_POINT('Ctrl Pts',(0.166093592002833,1.,-1.95646759718755));
#35077=CARTESIAN_POINT('Ctrl Pts',(0.1648165689203,1.,-1.96229379940174));
#35078=CARTESIAN_POINT('Ctrl Pts',(0.16347818545776,1.,-1.96816512678));
#35079=CARTESIAN_POINT('Ctrl Pts',(0.162079693556302,1.,-1.97406280235204));
#35080=CARTESIAN_POINT('Ctrl Pts',(0.16062206078461,1.,-1.97996195437557));
#35081=CARTESIAN_POINT('Ctrl Pts',(0.159106226437288,1.,-1.98584238283279));
#35082=CARTESIAN_POINT('Ctrl Pts',(0.157533331459215,1.,-1.99169810931893));
#35083=CARTESIAN_POINT('Ctrl Pts',(0.155904629548774,1.,-1.99753284771487));
#35084=CARTESIAN_POINT('Ctrl Pts',(0.154221403049719,1.,-2.00335565310539));
#35085=CARTESIAN_POINT('Ctrl Pts',(0.152484883621452,1.,-2.00917680318426));
#35086=CARTESIAN_POINT('Ctrl Pts',(0.150696157673084,1.,-2.01500291940243));
#35087=CARTESIAN_POINT('Ctrl Pts',(0.148856124775343,1.,-2.02083464969897));
#35088=CARTESIAN_POINT('Ctrl Pts',(0.146965557332586,1.,-2.02666926182017));
#35089=CARTESIAN_POINT('Ctrl Pts',(0.145025140186058,1.,-2.03250223739941));
#35090=CARTESIAN_POINT('Ctrl Pts',(0.143035515058208,1.,-2.03832911025913));
#35091=CARTESIAN_POINT('Ctrl Pts',(0.140997332152545,1.,-2.04414757947919));
#35092=CARTESIAN_POINT('Ctrl Pts',(0.138911255368966,1.,-2.04995762001333));
#35093=CARTESIAN_POINT('Ctrl Pts',(0.136777941218044,1.,-2.0557604441427));
#35094=CARTESIAN_POINT('Ctrl Pts',(0.134598026192107,1.,-2.06155781517844));
#35095=CARTESIAN_POINT('Ctrl Pts',(0.13237211154771,1.,-2.06735123910319));
#35096=CARTESIAN_POINT('Ctrl Pts',(0.1301007483284,1.,-2.07314114713047));
#35097=CARTESIAN_POINT('Ctrl Pts',(0.127784445276116,1.,-2.07892715110967));
#35098=CARTESIAN_POINT('Ctrl Pts',(0.125423679412058,1.,-2.08470840653628));
#35099=CARTESIAN_POINT('Ctrl Pts',(0.123018905621083,1.,-2.09048392424826));
#35100=CARTESIAN_POINT('Ctrl Pts',(0.120570567965129,1.,-2.09625292867756));
#35101=CARTESIAN_POINT('Ctrl Pts',(0.118079107988368,1.,-2.10201512132945));
#35102=CARTESIAN_POINT('Ctrl Pts',(0.11554495768794,1.,-2.10777050261359));
#35103=CARTESIAN_POINT('Ctrl Pts',(0.112968534419746,1.,-2.11351924490335));
#35104=CARTESIAN_POINT('Ctrl Pts',(0.11035023613502,1.,-2.11926155590849));
#35105=CARTESIAN_POINT('Ctrl Pts',(0.107690435231068,1.,-2.12499752306927));
#35106=CARTESIAN_POINT('Ctrl Pts',(0.104989479152703,1.,-2.1307270488718));
#35107=CARTESIAN_POINT('Ctrl Pts',(0.102247700556064,1.,-2.13644992667052));
#35108=CARTESIAN_POINT('Ctrl Pts',(0.0994654261990743,1.,-2.14216588395974));
#35109=CARTESIAN_POINT('Ctrl Pts',(0.0966429852305689,1.,-2.14787463531864));
#35110=CARTESIAN_POINT('Ctrl Pts',(0.0937807218868345,1.,-2.15357593978377));
#35111=CARTESIAN_POINT('Ctrl Pts',(0.0908789888108266,1.,-2.15926961544808));
#35112=CARTESIAN_POINT('Ctrl Pts',(0.0879381291387823,1.,-2.16495552645275));
#35113=CARTESIAN_POINT('Ctrl Pts',(0.0849584620835643,1.,-2.17063357871031));
#35114=CARTESIAN_POINT('Ctrl Pts',(0.0819402680871939,1.,-2.1763037121106));
#35115=CARTESIAN_POINT('Ctrl Pts',(0.0788837727683228,1.,-2.18196589448304));
#35116=CARTESIAN_POINT('Ctrl Pts',(0.0757891465833411,1.,-2.1876201139874));
#35117=CARTESIAN_POINT('Ctrl Pts',(0.0732830357304276,1.,-2.19213712012956));
#35118=CARTESIAN_POINT('Ctrl Pts',(0.0713863779524627,1.,-2.19552129483562));
#35119=CARTESIAN_POINT('Ctrl Pts',(0.0701143536324926,1.,-2.19777582085261));
#35120=CARTESIAN_POINT('Ctrl Pts',(0.0694764450219584,1.,-2.19890268624765));
#35121=CARTESIAN_POINT('',(0.163289472382896,0.,-1.74236521665491));
#35122=CARTESIAN_POINT('Origin',(0.,0.,0.));
#35123=CARTESIAN_POINT('',(0.383122945602004,1.,-1.7075470150345));
#35124=CARTESIAN_POINT('Origin',(0.,1.,0.));
#35125=CARTESIAN_POINT('',(0.383122945602004,0.,-1.7075470150345));
#35126=CARTESIAN_POINT('Ctrl Pts',(0.61342227326009,-1.,-2.11275013067528));
#35127=CARTESIAN_POINT('Ctrl Pts',(0.61342227326009,1.,-2.11275013067528));
#35128=CARTESIAN_POINT('Ctrl Pts',(0.61246736556225,-1.,-2.11187554260142));
#35129=CARTESIAN_POINT('Ctrl Pts',(0.61246736556225,1.,-2.11187554260142));
#35130=CARTESIAN_POINT('Ctrl Pts',(0.610560911691113,-1.,-2.11012443807661));
#35131=CARTESIAN_POINT('Ctrl Pts',(0.610560911691113,1.,-2.11012443807661));
#35132=CARTESIAN_POINT('Ctrl Pts',(0.607711315456826,-1.,-2.10749199615859));
#35133=CARTESIAN_POINT('Ctrl Pts',(0.607711315456826,1.,-2.10749199615859));
#35134=CARTESIAN_POINT('Ctrl Pts',(0.603932030738212,-1.,-2.10397049887709));
#35135=CARTESIAN_POINT('Ctrl Pts',(0.603932030738212,1.,-2.10397049887709));
#35136=CARTESIAN_POINT('Ctrl Pts',(0.599241616422144,-1.,-2.09954930865331));
#35137=CARTESIAN_POINT('Ctrl Pts',(0.599241616422144,1.,-2.09954930865331));
#35138=CARTESIAN_POINT('Ctrl Pts',(0.594585006052823,-1.,-2.09510876220501));
#35139=CARTESIAN_POINT('Ctrl Pts',(0.594585006052823,1.,-2.09510876220501));
#35140=CARTESIAN_POINT('Ctrl Pts',(0.589962365403189,-1.,-2.09064881812053));
#35141=CARTESIAN_POINT('Ctrl Pts',(0.589962365403189,1.,-2.09064881812053));
#35142=CARTESIAN_POINT('Ctrl Pts',(0.585373918990895,-1.,-2.086169437277));
#35143=CARTESIAN_POINT('Ctrl Pts',(0.585373918990895,1.,-2.086169437277));
#35144=CARTESIAN_POINT('Ctrl Pts',(0.580819952107256,-1.,-2.08167059018138));
#35145=CARTESIAN_POINT('Ctrl Pts',(0.580819952107256,1.,-2.08167059018138));
#35146=CARTESIAN_POINT('Ctrl Pts',(0.576300797416274,-1.,-2.07715226767361));
#35147=CARTESIAN_POINT('Ctrl Pts',(0.576300797416274,1.,-2.07715226767361));
#35148=CARTESIAN_POINT('Ctrl Pts',(0.571816823242411,-1.,-2.07261449292758));
#35149=CARTESIAN_POINT('Ctrl Pts',(0.571816823242411,1.,-2.07261449292758));
#35150=CARTESIAN_POINT('Ctrl Pts',(0.567368421181229,-1.,-2.06805732997383));
#35151=CARTESIAN_POINT('Ctrl Pts',(0.567368421181229,1.,-2.06805732997383));
#35152=CARTESIAN_POINT('Ctrl Pts',(0.562955993082574,-1.,-2.06348090160697));
#35153=CARTESIAN_POINT('Ctrl Pts',(0.562955993082574,1.,-2.06348090160697));
#35154=CARTESIAN_POINT('Ctrl Pts',(0.558579940185467,-1.,-2.05888537756571));
#35155=CARTESIAN_POINT('Ctrl Pts',(0.558579940185467,1.,-2.05888537756571));
#35156=CARTESIAN_POINT('Ctrl Pts',(0.554240657464109,-1.,-2.05427091604482));
#35157=CARTESIAN_POINT('Ctrl Pts',(0.554240657464109,1.,-2.05427091604482));
#35158=CARTESIAN_POINT('Ctrl Pts',(0.549938525150342,-1.,-2.04963761077974));
#35159=CARTESIAN_POINT('Ctrl Pts',(0.549938525150342,1.,-2.04963761077974));
#35160=CARTESIAN_POINT('Ctrl Pts',(0.545673903817348,-1.,-2.0449854471456));
#35161=CARTESIAN_POINT('Ctrl Pts',(0.545673903817348,1.,-2.0449854471456));
#35162=CARTESIAN_POINT('Ctrl Pts',(0.54144712061552,-1.,-2.0403142269048));
#35163=CARTESIAN_POINT('Ctrl Pts',(0.54144712061552,1.,-2.0403142269048));
#35164=CARTESIAN_POINT('Ctrl Pts',(0.537258489833134,-1.,-2.03562362953993));
#35165=CARTESIAN_POINT('Ctrl Pts',(0.537258489833134,1.,-2.03562362953993));
#35166=CARTESIAN_POINT('Ctrl Pts',(0.533108355132905,-1.,-2.03091336214401));
#35167=CARTESIAN_POINT('Ctrl Pts',(0.533108355132905,1.,-2.03091336214401));
#35168=CARTESIAN_POINT('Ctrl Pts',(0.52899712724191,-1.,-2.02618329083289));
#35169=CARTESIAN_POINT('Ctrl Pts',(0.52899712724191,1.,-2.02618329083289));
#35170=CARTESIAN_POINT('Ctrl Pts',(0.524925318333518,-1.,-2.02143356304712));
#35171=CARTESIAN_POINT('Ctrl Pts',(0.524925318333518,1.,-2.02143356304712));
#35172=CARTESIAN_POINT('Ctrl Pts',(0.520893590399428,-1.,-2.01666477917306));
#35173=CARTESIAN_POINT('Ctrl Pts',(0.520893590399428,1.,-2.01666477917306));
#35174=CARTESIAN_POINT('Ctrl Pts',(0.516902681728733,-1.,-2.01187773939257));
#35175=CARTESIAN_POINT('Ctrl Pts',(0.516902681728733,1.,-2.01187773939257));
#35176=CARTESIAN_POINT('Ctrl Pts',(0.512953306961813,-1.,-2.00707309946955));
#35177=CARTESIAN_POINT('Ctrl Pts',(0.512953306961813,1.,-2.00707309946955));
#35178=CARTESIAN_POINT('Ctrl Pts',(0.509046069886152,-1.,-2.00225107134733));
#35179=CARTESIAN_POINT('Ctrl Pts',(0.509046069886152,1.,-2.00225107134733));
#35180=CARTESIAN_POINT('Ctrl Pts',(0.505181361323011,-1.,-1.99741107463567));
#35181=CARTESIAN_POINT('Ctrl Pts',(0.505181361323011,1.,-1.99741107463567));
#35182=CARTESIAN_POINT('Ctrl Pts',(0.501359287727129,-1.,-1.9925514912615));
#35183=CARTESIAN_POINT('Ctrl Pts',(0.501359287727129,1.,-1.9925514912615));
#35184=CARTESIAN_POINT('Ctrl Pts',(0.497579909545564,-1.,-1.98767044752929));
#35185=CARTESIAN_POINT('Ctrl Pts',(0.497579909545564,1.,-1.98767044752929));
#35186=CARTESIAN_POINT('Ctrl Pts',(0.493843476541492,-1.,-1.9827665876182));
#35187=CARTESIAN_POINT('Ctrl Pts',(0.493843476541492,1.,-1.9827665876182));
#35188=CARTESIAN_POINT('Ctrl Pts',(0.490150627860955,-1.,-1.97783973019229));
#35189=CARTESIAN_POINT('Ctrl Pts',(0.490150627860955,1.,-1.97783973019229));
#35190=CARTESIAN_POINT('Ctrl Pts',(0.486502692907661,-1.,-1.97289186263272));
#35191=CARTESIAN_POINT('Ctrl Pts',(0.486502692907661,1.,-1.97289186263272));
#35192=CARTESIAN_POINT('Ctrl Pts',(0.482901662120686,-1.,-1.96792703422358));
#35193=CARTESIAN_POINT('Ctrl Pts',(0.482901662120686,1.,-1.96792703422358));
#35194=CARTESIAN_POINT('Ctrl Pts',(0.479349583074846,-1.,-1.96294933055938));
#35195=CARTESIAN_POINT('Ctrl Pts',(0.479349583074846,1.,-1.96294933055938));
#35196=CARTESIAN_POINT('Ctrl Pts',(0.475848034683171,-1.,-1.95796111148175));
#35197=CARTESIAN_POINT('Ctrl Pts',(0.475848034683171,1.,-1.95796111148175));
#35198=CARTESIAN_POINT('Ctrl Pts',(0.472397672264079,-1.,-1.95296148278136));
#35199=CARTESIAN_POINT('Ctrl Pts',(0.472397672264079,1.,-1.95296148278136));
#35200=CARTESIAN_POINT('Ctrl Pts',(0.468997482913158,-1.,-1.94794381136524));
#35201=CARTESIAN_POINT('Ctrl Pts',(0.468997482913158,1.,-1.94794381136524));
#35202=CARTESIAN_POINT('Ctrl Pts',(0.465645462026064,-1.,-1.94289794196205));
#35203=CARTESIAN_POINT('Ctrl Pts',(0.465645462026064,1.,-1.94289794196205));
#35204=CARTESIAN_POINT('Ctrl Pts',(0.462340031009087,-1.,-1.93781486640834));
#35205=CARTESIAN_POINT('Ctrl Pts',(0.462340031009087,1.,-1.93781486640834));
#35206=CARTESIAN_POINT('Ctrl Pts',(0.459081234547931,-1.,-1.93269066517936));
#35207=CARTESIAN_POINT('Ctrl Pts',(0.459081234547931,1.,-1.93269066517936));
#35208=CARTESIAN_POINT('Ctrl Pts',(0.455872005174335,-1.,-1.92753067150461));
#35209=CARTESIAN_POINT('Ctrl Pts',(0.455872005174335,1.,-1.92753067150461));
#35210=CARTESIAN_POINT('Ctrl Pts',(0.452719478359356,-1.,-1.9223538064847));
#35211=CARTESIAN_POINT('Ctrl Pts',(0.452719478359356,1.,-1.9223538064847));
#35212=CARTESIAN_POINT('Ctrl Pts',(0.449632260106572,-1.,-1.91718342555717));
#35213=CARTESIAN_POINT('Ctrl Pts',(0.449632260106572,1.,-1.91718342555717));
#35214=CARTESIAN_POINT('Ctrl Pts',(0.446617343485651,-1.,-1.91203699981095));
#35215=CARTESIAN_POINT('Ctrl Pts',(0.446617343485651,1.,-1.91203699981095));
#35216=CARTESIAN_POINT('Ctrl Pts',(0.44367755684917,-1.,-1.90691756144906));
#35217=CARTESIAN_POINT('Ctrl Pts',(0.44367755684917,1.,-1.90691756144906));
#35218=CARTESIAN_POINT('Ctrl Pts',(0.44080783370416,-1.,-1.90180124389137));
#35219=CARTESIAN_POINT('Ctrl Pts',(0.44080783370416,1.,-1.90180124389137));
#35220=CARTESIAN_POINT('Ctrl Pts',(0.437995003948443,-1.,-1.89663648956549));
#35221=CARTESIAN_POINT('Ctrl Pts',(0.437995003948443,1.,-1.89663648956549));
#35222=CARTESIAN_POINT('Ctrl Pts',(0.43522566096358,-1.,-1.89136993975585));
#35223=CARTESIAN_POINT('Ctrl Pts',(0.43522566096358,1.,-1.89136993975585));
#35224=CARTESIAN_POINT('Ctrl Pts',(0.432493038548833,-1.,-1.88596913666828));
#35225=CARTESIAN_POINT('Ctrl Pts',(0.432493038548833,1.,-1.88596913666828));
#35226=CARTESIAN_POINT('Ctrl Pts',(0.429803062482217,-1.,-1.88044229001779));
#35227=CARTESIAN_POINT('Ctrl Pts',(0.429803062482217,1.,-1.88044229001779));
#35228=CARTESIAN_POINT('Ctrl Pts',(0.427183828518743,-1.,-1.87486989291334));
#35229=CARTESIAN_POINT('Ctrl Pts',(0.427183828518743,1.,-1.87486989291334));
#35230=CARTESIAN_POINT('Ctrl Pts',(0.424678177290876,-1.,-1.8693780394412));
#35231=CARTESIAN_POINT('Ctrl Pts',(0.424678177290876,1.,-1.8693780394412));
#35232=CARTESIAN_POINT('Ctrl Pts',(0.422327307417884,-1.,-1.86408083333863));
#35233=CARTESIAN_POINT('Ctrl Pts',(0.422327307417884,1.,-1.86408083333863));
#35234=CARTESIAN_POINT('Ctrl Pts',(0.420157287975583,-1.,-1.8590328109667));
#35235=CARTESIAN_POINT('Ctrl Pts',(0.420157287975583,1.,-1.8590328109667));
#35236=CARTESIAN_POINT('Ctrl Pts',(0.418164129144045,-1.,-1.8541763285645));
#35237=CARTESIAN_POINT('Ctrl Pts',(0.418164129144045,1.,-1.8541763285645));
#35238=CARTESIAN_POINT('Ctrl Pts',(0.416300022039885,-1.,-1.84929312930314));
#35239=CARTESIAN_POINT('Ctrl Pts',(0.416300022039885,1.,-1.84929312930314));
#35240=CARTESIAN_POINT('Ctrl Pts',(0.414487438255542,-1.,-1.84405757074218));
#35241=CARTESIAN_POINT('Ctrl Pts',(0.414487438255542,1.,-1.84405757074218));
#35242=CARTESIAN_POINT('Ctrl Pts',(0.412633125322945,-1.,-1.8380895347617));
#35243=CARTESIAN_POINT('Ctrl Pts',(0.412633125322945,1.,-1.8380895347617));
#35244=CARTESIAN_POINT('Ctrl Pts',(0.410641256301276,-1.,-1.83100408895047));
#35245=CARTESIAN_POINT('Ctrl Pts',(0.410641256301276,1.,-1.83100408895047));
#35246=CARTESIAN_POINT('Ctrl Pts',(0.408428948106227,-1.,-1.82247022677562));
#35247=CARTESIAN_POINT('Ctrl Pts',(0.408428948106227,1.,-1.82247022677562));
#35248=CARTESIAN_POINT('Ctrl Pts',(0.405933518407175,-1.,-1.81223801812013));
#35249=CARTESIAN_POINT('Ctrl Pts',(0.405933518407175,1.,-1.81223801812013));
#35250=CARTESIAN_POINT('Ctrl Pts',(0.403107976163396,-1.,-1.80012077173238));
#35251=CARTESIAN_POINT('Ctrl Pts',(0.403107976163396,1.,-1.80012077173238));
#35252=CARTESIAN_POINT('Ctrl Pts',(0.399919403774155,-1.,-1.78598826343754));
#35253=CARTESIAN_POINT('Ctrl Pts',(0.399919403774155,1.,-1.78598826343754));
#35254=CARTESIAN_POINT('Ctrl Pts',(0.396346196110688,-1.,-1.76975560043442));
#35255=CARTESIAN_POINT('Ctrl Pts',(0.396346196110688,1.,-1.76975560043442));
#35256=CARTESIAN_POINT('Ctrl Pts',(0.392375812285395,-1.,-1.75137405310193));
#35257=CARTESIAN_POINT('Ctrl Pts',(0.392375812285395,1.,-1.75137405310193));
#35258=CARTESIAN_POINT('Ctrl Pts',(0.388877023502615,-1.,-1.73493170972829));
#35259=CARTESIAN_POINT('Ctrl Pts',(0.388877023502615,1.,-1.73493170972829));
#35260=CARTESIAN_POINT('Ctrl Pts',(0.386070790323281,-1.,-1.72162022244582));
#35261=CARTESIAN_POINT('Ctrl Pts',(0.386070790323281,1.,-1.72162022244582));
#35262=CARTESIAN_POINT('Ctrl Pts',(0.384119047314215,-1.,-1.71231062891398));
#35263=CARTESIAN_POINT('Ctrl Pts',(0.384119047314215,1.,-1.71231062891398));
#35264=CARTESIAN_POINT('Ctrl Pts',(0.383122945602004,-1.,-1.7075470150345));
#35265=CARTESIAN_POINT('Ctrl Pts',(0.383122945602004,1.,-1.7075470150345));
#35266=CARTESIAN_POINT('',(0.61342227326009,1.,-2.11275013067528));
#35267=CARTESIAN_POINT('Ctrl Pts',(0.61342227326009,1.,-2.11275013067528));
#35268=CARTESIAN_POINT('Ctrl Pts',(0.61246736556225,1.,-2.11187554260142));
#35269=CARTESIAN_POINT('Ctrl Pts',(0.610560911691113,1.,-2.11012443807661));
#35270=CARTESIAN_POINT('Ctrl Pts',(0.607711315456826,1.,-2.10749199615859));
#35271=CARTESIAN_POINT('Ctrl Pts',(0.603932030738212,1.,-2.10397049887709));
#35272=CARTESIAN_POINT('Ctrl Pts',(0.599241616422144,1.,-2.09954930865331));
#35273=CARTESIAN_POINT('Ctrl Pts',(0.594585006052823,1.,-2.09510876220501));
#35274=CARTESIAN_POINT('Ctrl Pts',(0.589962365403189,1.,-2.09064881812053));
#35275=CARTESIAN_POINT('Ctrl Pts',(0.585373918990895,1.,-2.086169437277));
#35276=CARTESIAN_POINT('Ctrl Pts',(0.580819952107256,1.,-2.08167059018138));
#35277=CARTESIAN_POINT('Ctrl Pts',(0.576300797416274,1.,-2.07715226767361));
#35278=CARTESIAN_POINT('Ctrl Pts',(0.571816823242411,1.,-2.07261449292758));
#35279=CARTESIAN_POINT('Ctrl Pts',(0.567368421181229,1.,-2.06805732997383));
#35280=CARTESIAN_POINT('Ctrl Pts',(0.562955993082574,1.,-2.06348090160697));
#35281=CARTESIAN_POINT('Ctrl Pts',(0.558579940185467,1.,-2.05888537756571));
#35282=CARTESIAN_POINT('Ctrl Pts',(0.554240657464109,1.,-2.05427091604482));
#35283=CARTESIAN_POINT('Ctrl Pts',(0.549938525150342,1.,-2.04963761077974));
#35284=CARTESIAN_POINT('Ctrl Pts',(0.545673903817348,1.,-2.0449854471456));
#35285=CARTESIAN_POINT('Ctrl Pts',(0.54144712061552,1.,-2.0403142269048));
#35286=CARTESIAN_POINT('Ctrl Pts',(0.537258489833134,1.,-2.03562362953993));
#35287=CARTESIAN_POINT('Ctrl Pts',(0.533108355132905,1.,-2.03091336214401));
#35288=CARTESIAN_POINT('Ctrl Pts',(0.52899712724191,1.,-2.02618329083289));
#35289=CARTESIAN_POINT('Ctrl Pts',(0.524925318333518,1.,-2.02143356304712));
#35290=CARTESIAN_POINT('Ctrl Pts',(0.520893590399428,1.,-2.01666477917306));
#35291=CARTESIAN_POINT('Ctrl Pts',(0.516902681728733,1.,-2.01187773939257));
#35292=CARTESIAN_POINT('Ctrl Pts',(0.512953306961813,1.,-2.00707309946955));
#35293=CARTESIAN_POINT('Ctrl Pts',(0.509046069886152,1.,-2.00225107134733));
#35294=CARTESIAN_POINT('Ctrl Pts',(0.505181361323011,1.,-1.99741107463567));
#35295=CARTESIAN_POINT('Ctrl Pts',(0.501359287727129,1.,-1.9925514912615));
#35296=CARTESIAN_POINT('Ctrl Pts',(0.497579909545564,1.,-1.98767044752929));
#35297=CARTESIAN_POINT('Ctrl Pts',(0.493843476541492,1.,-1.9827665876182));
#35298=CARTESIAN_POINT('Ctrl Pts',(0.490150627860955,1.,-1.97783973019229));
#35299=CARTESIAN_POINT('Ctrl Pts',(0.486502692907661,1.,-1.97289186263272));
#35300=CARTESIAN_POINT('Ctrl Pts',(0.482901662120686,1.,-1.96792703422358));
#35301=CARTESIAN_POINT('Ctrl Pts',(0.479349583074846,1.,-1.96294933055938));
#35302=CARTESIAN_POINT('Ctrl Pts',(0.475848034683171,1.,-1.95796111148175));
#35303=CARTESIAN_POINT('Ctrl Pts',(0.472397672264079,1.,-1.95296148278136));
#35304=CARTESIAN_POINT('Ctrl Pts',(0.468997482913158,1.,-1.94794381136524));
#35305=CARTESIAN_POINT('Ctrl Pts',(0.465645462026064,1.,-1.94289794196205));
#35306=CARTESIAN_POINT('Ctrl Pts',(0.462340031009087,1.,-1.93781486640834));
#35307=CARTESIAN_POINT('Ctrl Pts',(0.459081234547931,1.,-1.93269066517936));
#35308=CARTESIAN_POINT('Ctrl Pts',(0.455872005174335,1.,-1.92753067150461));
#35309=CARTESIAN_POINT('Ctrl Pts',(0.452719478359356,1.,-1.9223538064847));
#35310=CARTESIAN_POINT('Ctrl Pts',(0.449632260106572,1.,-1.91718342555717));
#35311=CARTESIAN_POINT('Ctrl Pts',(0.446617343485651,1.,-1.91203699981095));
#35312=CARTESIAN_POINT('Ctrl Pts',(0.44367755684917,1.,-1.90691756144906));
#35313=CARTESIAN_POINT('Ctrl Pts',(0.44080783370416,1.,-1.90180124389137));
#35314=CARTESIAN_POINT('Ctrl Pts',(0.437995003948443,1.,-1.89663648956549));
#35315=CARTESIAN_POINT('Ctrl Pts',(0.43522566096358,1.,-1.89136993975585));
#35316=CARTESIAN_POINT('Ctrl Pts',(0.432493038548833,1.,-1.88596913666828));
#35317=CARTESIAN_POINT('Ctrl Pts',(0.429803062482217,1.,-1.88044229001779));
#35318=CARTESIAN_POINT('Ctrl Pts',(0.427183828518743,1.,-1.87486989291334));
#35319=CARTESIAN_POINT('Ctrl Pts',(0.424678177290876,1.,-1.8693780394412));
#35320=CARTESIAN_POINT('Ctrl Pts',(0.422327307417884,1.,-1.86408083333863));
#35321=CARTESIAN_POINT('Ctrl Pts',(0.420157287975583,1.,-1.8590328109667));
#35322=CARTESIAN_POINT('Ctrl Pts',(0.418164129144045,1.,-1.8541763285645));
#35323=CARTESIAN_POINT('Ctrl Pts',(0.416300022039885,1.,-1.84929312930314));
#35324=CARTESIAN_POINT('Ctrl Pts',(0.414487438255542,1.,-1.84405757074218));
#35325=CARTESIAN_POINT('Ctrl Pts',(0.412633125322945,1.,-1.8380895347617));
#35326=CARTESIAN_POINT('Ctrl Pts',(0.410641256301276,1.,-1.83100408895047));
#35327=CARTESIAN_POINT('Ctrl Pts',(0.408428948106227,1.,-1.82247022677562));
#35328=CARTESIAN_POINT('Ctrl Pts',(0.405933518407175,1.,-1.81223801812013));
#35329=CARTESIAN_POINT('Ctrl Pts',(0.403107976163396,1.,-1.80012077173238));
#35330=CARTESIAN_POINT('Ctrl Pts',(0.399919403774155,1.,-1.78598826343754));
#35331=CARTESIAN_POINT('Ctrl Pts',(0.396346196110688,1.,-1.76975560043442));
#35332=CARTESIAN_POINT('Ctrl Pts',(0.392375812285395,1.,-1.75137405310193));
#35333=CARTESIAN_POINT('Ctrl Pts',(0.388877023502615,1.,-1.73493170972829));
#35334=CARTESIAN_POINT('Ctrl Pts',(0.386070790323281,1.,-1.72162022244582));
#35335=CARTESIAN_POINT('Ctrl Pts',(0.384119047314215,1.,-1.71231062891398));
#35336=CARTESIAN_POINT('Ctrl Pts',(0.383122945602004,1.,-1.7075470150345));
#35337=CARTESIAN_POINT('',(0.61342227326009,0.,-2.11275013067528));
#35338=CARTESIAN_POINT('Origin',(0.745574324794401,0.,-2.0698113262342));
#35339=CARTESIAN_POINT('',(0.745574324794401,1.,-2.0698113262342));
#35340=CARTESIAN_POINT('',(0.61342227326009,1.,-2.11275013067528));
#35341=CARTESIAN_POINT('',(0.745574324794401,0.,-2.0698113262342));
#35342=CARTESIAN_POINT('Ctrl Pts',(0.693717979106306,-1.,-1.60662857109684));
#35343=CARTESIAN_POINT('Ctrl Pts',(0.693717979106306,1.,-1.60662857109684));
#35344=CARTESIAN_POINT('Ctrl Pts',(0.695712097881194,-1.,-1.61106790958151));
#35345=CARTESIAN_POINT('Ctrl Pts',(0.695712097881194,1.,-1.61106790958151));
#35346=CARTESIAN_POINT('Ctrl Pts',(0.699605146405088,-1.,-1.61974673472612));
#35347=CARTESIAN_POINT('Ctrl Pts',(0.699605146405088,1.,-1.61974673472612));
#35348=CARTESIAN_POINT('Ctrl Pts',(0.705159151988319,-1.,-1.63216541664676));
#35349=CARTESIAN_POINT('Ctrl Pts',(0.705159151988319,1.,-1.63216541664676));
#35350=CARTESIAN_POINT('Ctrl Pts',(0.711993139355394,-1.,-1.64752408832016));
#35351=CARTESIAN_POINT('Ctrl Pts',(0.711993139355394,1.,-1.64752408832016));
#35352=CARTESIAN_POINT('Ctrl Pts',(0.719585433804282,-1.,-1.6647288055568));
#35353=CARTESIAN_POINT('Ctrl Pts',(0.719585433804282,1.,-1.6647288055568));
#35354=CARTESIAN_POINT('Ctrl Pts',(0.726235967997433,-1.,-1.67996158455503));
#35355=CARTESIAN_POINT('Ctrl Pts',(0.726235967997433,1.,-1.67996158455503));
#35356=CARTESIAN_POINT('Ctrl Pts',(0.731963238697195,-1.,-1.69326921975743));
#35357=CARTESIAN_POINT('Ctrl Pts',(0.731963238697195,1.,-1.69326921975743));
#35358=CARTESIAN_POINT('Ctrl Pts',(0.736799665724771,-1.,-1.70473309006121));
#35359=CARTESIAN_POINT('Ctrl Pts',(0.736799665724771,1.,-1.70473309006121));
#35360=CARTESIAN_POINT('Ctrl Pts',(0.740795162032087,-1.,-1.71447789751927));
#35361=CARTESIAN_POINT('Ctrl Pts',(0.740795162032087,1.,-1.71447789751927));
#35362=CARTESIAN_POINT('Ctrl Pts',(0.744021445433764,-1.,-1.7226822991693));
#35363=CARTESIAN_POINT('Ctrl Pts',(0.744021445433764,1.,-1.7226822991693));
#35364=CARTESIAN_POINT('Ctrl Pts',(0.746574710096436,-1.,-1.72958533647399));
#35365=CARTESIAN_POINT('Ctrl Pts',(0.746574710096436,1.,-1.72958533647399));
#35366=CARTESIAN_POINT('Ctrl Pts',(0.748582462954854,-1.,-1.73550351679848));
#35367=CARTESIAN_POINT('Ctrl Pts',(0.748582462954854,1.,-1.73550351679848));
#35368=CARTESIAN_POINT('Ctrl Pts',(0.75019343597954,-1.,-1.74080458266705));
#35369=CARTESIAN_POINT('Ctrl Pts',(0.75019343597954,1.,-1.74080458266705));
#35370=CARTESIAN_POINT('Ctrl Pts',(0.751555614163629,-1.,-1.74585086852298));
#35371=CARTESIAN_POINT('Ctrl Pts',(0.751555614163629,1.,-1.74585086852298));
#35372=CARTESIAN_POINT('Ctrl Pts',(0.752797683531377,-1.,-1.75095139468809));
#35373=CARTESIAN_POINT('Ctrl Pts',(0.752797683531377,1.,-1.75095139468809));
#35374=CARTESIAN_POINT('Ctrl Pts',(0.75400925402848,-1.,-1.75631083600175));
#35375=CARTESIAN_POINT('Ctrl Pts',(0.75400925402848,1.,-1.75631083600175));
#35376=CARTESIAN_POINT('Ctrl Pts',(0.755220979975262,-1.,-1.7619781724032));
#35377=CARTESIAN_POINT('Ctrl Pts',(0.755220979975262,1.,-1.7619781724032));
#35378=CARTESIAN_POINT('Ctrl Pts',(0.756421896028403,-1.,-1.76789396003141));
#35379=CARTESIAN_POINT('Ctrl Pts',(0.756421896028403,1.,-1.76789396003141));
#35380=CARTESIAN_POINT('Ctrl Pts',(0.757578264077238,-1.,-1.77394167108342));
#35381=CARTESIAN_POINT('Ctrl Pts',(0.757578264077238,1.,-1.77394167108342));
#35382=CARTESIAN_POINT('Ctrl Pts',(0.75865062667738,-1.,-1.77999411220912));
#35383=CARTESIAN_POINT('Ctrl Pts',(0.75865062667738,1.,-1.77999411220912));
#35384=CARTESIAN_POINT('Ctrl Pts',(0.759614401109868,-1.,-1.78596964884527));
#35385=CARTESIAN_POINT('Ctrl Pts',(0.759614401109868,1.,-1.78596964884527));
#35386=CARTESIAN_POINT('Ctrl Pts',(0.760469555880425,-1.,-1.79185815610802));
#35387=CARTESIAN_POINT('Ctrl Pts',(0.760469555880425,1.,-1.79185815610802));
#35388=CARTESIAN_POINT('Ctrl Pts',(0.761229695230359,-1.,-1.79768986997735));
#35389=CARTESIAN_POINT('Ctrl Pts',(0.761229695230359,1.,-1.79768986997735));
#35390=CARTESIAN_POINT('Ctrl Pts',(0.761915336443515,-1.,-1.80351583877334));
#35391=CARTESIAN_POINT('Ctrl Pts',(0.761915336443515,1.,-1.80351583877334));
#35392=CARTESIAN_POINT('Ctrl Pts',(0.762546129464036,-1.,-1.80938551463989));
#35393=CARTESIAN_POINT('Ctrl Pts',(0.762546129464036,1.,-1.80938551463989));
#35394=CARTESIAN_POINT('Ctrl Pts',(0.763132003836783,-1.,-1.81532118405566));
#35395=CARTESIAN_POINT('Ctrl Pts',(0.763132003836783,1.,-1.81532118405566));
#35396=CARTESIAN_POINT('Ctrl Pts',(0.763673465462854,-1.,-1.82131873145297));
#35397=CARTESIAN_POINT('Ctrl Pts',(0.763673465462854,1.,-1.82131873145297));
#35398=CARTESIAN_POINT('Ctrl Pts',(0.764165902606055,-1.,-1.8273599120008));
#35399=CARTESIAN_POINT('Ctrl Pts',(0.764165902606055,1.,-1.8273599120008));
#35400=CARTESIAN_POINT('Ctrl Pts',(0.764602549687845,-1.,-1.8334207722714));
#35401=CARTESIAN_POINT('Ctrl Pts',(0.764602549687845,1.,-1.8334207722714));
#35402=CARTESIAN_POINT('Ctrl Pts',(0.764978057881687,-1.,-1.83948181064823));
#35403=CARTESIAN_POINT('Ctrl Pts',(0.764978057881687,1.,-1.83948181064823));
#35404=CARTESIAN_POINT('Ctrl Pts',(0.765291664861971,-1.,-1.84553698875911));
#35405=CARTESIAN_POINT('Ctrl Pts',(0.765291664861971,1.,-1.84553698875911));
#35406=CARTESIAN_POINT('Ctrl Pts',(0.765545710619023,-1.,-1.85158945130054));
#35407=CARTESIAN_POINT('Ctrl Pts',(0.765545710619023,1.,-1.85158945130054));
#35408=CARTESIAN_POINT('Ctrl Pts',(0.765744212909305,-1.,-1.85764741390391));
#35409=CARTESIAN_POINT('Ctrl Pts',(0.765744212909305,1.,-1.85764741390391));
#35410=CARTESIAN_POINT('Ctrl Pts',(0.765891519092557,-1.,-1.86372027063315));
#35411=CARTESIAN_POINT('Ctrl Pts',(0.765891519092557,1.,-1.86372027063315));
#35412=CARTESIAN_POINT('Ctrl Pts',(0.765990708546111,-1.,-1.86981398314345));
#35413=CARTESIAN_POINT('Ctrl Pts',(0.765990708546111,1.,-1.86981398314345));
#35414=CARTESIAN_POINT('Ctrl Pts',(0.766042837036759,-1.,-1.87592888967886));
#35415=CARTESIAN_POINT('Ctrl Pts',(0.766042837036759,1.,-1.87592888967886));
#35416=CARTESIAN_POINT('Ctrl Pts',(0.766047794851868,-1.,-1.88206215302561));
#35417=CARTESIAN_POINT('Ctrl Pts',(0.766047794851868,1.,-1.88206215302561));
#35418=CARTESIAN_POINT('Ctrl Pts',(0.76600483706209,-1.,-1.88820926433409));
#35419=CARTESIAN_POINT('Ctrl Pts',(0.76600483706209,1.,-1.88820926433409));
#35420=CARTESIAN_POINT('Ctrl Pts',(0.765913193856979,-1.,-1.89436577771389));
#35421=CARTESIAN_POINT('Ctrl Pts',(0.765913193856979,1.,-1.89436577771389));
#35422=CARTESIAN_POINT('Ctrl Pts',(0.765772772593395,-1.,-1.90052930393599));
#35423=CARTESIAN_POINT('Ctrl Pts',(0.765772772593395,1.,-1.90052930393599));
#35424=CARTESIAN_POINT('Ctrl Pts',(0.765584196937936,-1.,-1.90669961402362));
#35425=CARTESIAN_POINT('Ctrl Pts',(0.765584196937936,1.,-1.90669961402362));
#35426=CARTESIAN_POINT('Ctrl Pts',(0.765348465884739,-1.,-1.91287765805174));
#35427=CARTESIAN_POINT('Ctrl Pts',(0.765348465884739,1.,-1.91287765805174));
#35428=CARTESIAN_POINT('Ctrl Pts',(0.765066729667095,-1.,-1.91906491634197));
#35429=CARTESIAN_POINT('Ctrl Pts',(0.765066729667095,1.,-1.91906491634197));
#35430=CARTESIAN_POINT('Ctrl Pts',(0.764740025488189,-1.,-1.92526263537041));
#35431=CARTESIAN_POINT('Ctrl Pts',(0.764740025488189,1.,-1.92526263537041));
#35432=CARTESIAN_POINT('Ctrl Pts',(0.764369010673889,-1.,-1.93147105496367));
#35433=CARTESIAN_POINT('Ctrl Pts',(0.764369010673889,1.,-1.93147105496367));
#35434=CARTESIAN_POINT('Ctrl Pts',(0.763954049121393,-1.,-1.93768964875867));
#35435=CARTESIAN_POINT('Ctrl Pts',(0.763954049121393,1.,-1.93768964875867));
#35436=CARTESIAN_POINT('Ctrl Pts',(0.76349533353858,-1.,-1.94391746617626));
#35437=CARTESIAN_POINT('Ctrl Pts',(0.76349533353858,1.,-1.94391746617626));
#35438=CARTESIAN_POINT('Ctrl Pts',(0.762992990878774,-1.,-1.95015342590025));
#35439=CARTESIAN_POINT('Ctrl Pts',(0.762992990878774,1.,-1.95015342590025));
#35440=CARTESIAN_POINT('Ctrl Pts',(0.762447203806263,-1.,-1.95639665309893));
#35441=CARTESIAN_POINT('Ctrl Pts',(0.762447203806263,1.,-1.95639665309893));
#35442=CARTESIAN_POINT('Ctrl Pts',(0.761858300014575,-1.,-1.96264672744229));
#35443=CARTESIAN_POINT('Ctrl Pts',(0.761858300014575,1.,-1.96264672744229));
#35444=CARTESIAN_POINT('Ctrl Pts',(0.761226690483986,-1.,-1.96890351582545));
#35445=CARTESIAN_POINT('Ctrl Pts',(0.761226690483986,1.,-1.96890351582545));
#35446=CARTESIAN_POINT('Ctrl Pts',(0.760552825409855,-1.,-1.97516705321521));
#35447=CARTESIAN_POINT('Ctrl Pts',(0.760552825409855,1.,-1.97516705321521));
#35448=CARTESIAN_POINT('Ctrl Pts',(0.759837147452135,-1.,-1.98143741418156));
#35449=CARTESIAN_POINT('Ctrl Pts',(0.759837147452135,1.,-1.98143741418156));
#35450=CARTESIAN_POINT('Ctrl Pts',(0.759080037802242,-1.,-1.98771456680806));
#35451=CARTESIAN_POINT('Ctrl Pts',(0.759080037802242,1.,-1.98771456680806));
#35452=CARTESIAN_POINT('Ctrl Pts',(0.758281796766377,-1.,-1.9939983109871));
#35453=CARTESIAN_POINT('Ctrl Pts',(0.758281796766377,1.,-1.9939983109871));
#35454=CARTESIAN_POINT('Ctrl Pts',(0.757442676862341,-1.,-2.00028834739072));
#35455=CARTESIAN_POINT('Ctrl Pts',(0.757442676862341,1.,-2.00028834739072));
#35456=CARTESIAN_POINT('Ctrl Pts',(0.756562904646496,-1.,-2.00658431587682));
#35457=CARTESIAN_POINT('Ctrl Pts',(0.756562904646496,1.,-2.00658431587682));
#35458=CARTESIAN_POINT('Ctrl Pts',(0.7556427049581,-1.,-2.01288584328149));
#35459=CARTESIAN_POINT('Ctrl Pts',(0.7556427049581,1.,-2.01288584328149));
#35460=CARTESIAN_POINT('Ctrl Pts',(0.75468233072352,-1.,-2.01919259406003));
#35461=CARTESIAN_POINT('Ctrl Pts',(0.75468233072352,1.,-2.01919259406003));
#35462=CARTESIAN_POINT('Ctrl Pts',(0.753682061113765,-1.,-2.02550428623587));
#35463=CARTESIAN_POINT('Ctrl Pts',(0.753682061113765,1.,-2.02550428623587));
#35464=CARTESIAN_POINT('Ctrl Pts',(0.752642180488104,-1.,-2.03182068456467));
#35465=CARTESIAN_POINT('Ctrl Pts',(0.752642180488104,1.,-2.03182068456467));
#35466=CARTESIAN_POINT('Ctrl Pts',(0.751562963361383,-1.,-2.03814160092173));
#35467=CARTESIAN_POINT('Ctrl Pts',(0.751562963361383,1.,-2.03814160092173));
#35468=CARTESIAN_POINT('Ctrl Pts',(0.750444657874758,-1.,-2.04446689147754));
#35469=CARTESIAN_POINT('Ctrl Pts',(0.750444657874758,1.,-2.04446689147754));
#35470=CARTESIAN_POINT('Ctrl Pts',(0.749287468663053,-1.,-2.05079645591606));
#35471=CARTESIAN_POINT('Ctrl Pts',(0.749287468663053,1.,-2.05079645591606));
#35472=CARTESIAN_POINT('Ctrl Pts',(0.748091554181101,-1.,-2.05713023030263));
#35473=CARTESIAN_POINT('Ctrl Pts',(0.748091554181101,1.,-2.05713023030263));
#35474=CARTESIAN_POINT('Ctrl Pts',(0.747103932785504,-1.,-2.06220058927162));
#35475=CARTESIAN_POINT('Ctrl Pts',(0.747103932785504,1.,-2.06220058927162));
#35476=CARTESIAN_POINT('Ctrl Pts',(0.746345871542695,-1.,-2.06600523016401));
#35477=CARTESIAN_POINT('Ctrl Pts',(0.746345871542695,1.,-2.06600523016401));
#35478=CARTESIAN_POINT('Ctrl Pts',(0.74583279137781,-1.,-2.06854248895575));
#35479=CARTESIAN_POINT('Ctrl Pts',(0.74583279137781,1.,-2.06854248895575));
#35480=CARTESIAN_POINT('Ctrl Pts',(0.745574324794401,-1.,-2.0698113262342));
#35481=CARTESIAN_POINT('Ctrl Pts',(0.745574324794401,1.,-2.0698113262342));
#35482=CARTESIAN_POINT('',(0.693717979106306,1.,-1.60662857109684));
#35483=CARTESIAN_POINT('Ctrl Pts',(0.693717979106306,1.,-1.60662857109684));
#35484=CARTESIAN_POINT('Ctrl Pts',(0.695712097881194,1.,-1.61106790958151));
#35485=CARTESIAN_POINT('Ctrl Pts',(0.699605146405088,1.,-1.61974673472612));
#35486=CARTESIAN_POINT('Ctrl Pts',(0.705159151988319,1.,-1.63216541664676));
#35487=CARTESIAN_POINT('Ctrl Pts',(0.711993139355394,1.,-1.64752408832016));
#35488=CARTESIAN_POINT('Ctrl Pts',(0.719585433804282,1.,-1.6647288055568));
#35489=CARTESIAN_POINT('Ctrl Pts',(0.726235967997433,1.,-1.67996158455503));
#35490=CARTESIAN_POINT('Ctrl Pts',(0.731963238697195,1.,-1.69326921975743));
#35491=CARTESIAN_POINT('Ctrl Pts',(0.736799665724771,1.,-1.70473309006121));
#35492=CARTESIAN_POINT('Ctrl Pts',(0.740795162032087,1.,-1.71447789751927));
#35493=CARTESIAN_POINT('Ctrl Pts',(0.744021445433764,1.,-1.7226822991693));
#35494=CARTESIAN_POINT('Ctrl Pts',(0.746574710096436,1.,-1.72958533647399));
#35495=CARTESIAN_POINT('Ctrl Pts',(0.748582462954854,1.,-1.73550351679848));
#35496=CARTESIAN_POINT('Ctrl Pts',(0.75019343597954,1.,-1.74080458266705));
#35497=CARTESIAN_POINT('Ctrl Pts',(0.751555614163629,1.,-1.74585086852298));
#35498=CARTESIAN_POINT('Ctrl Pts',(0.752797683531377,1.,-1.75095139468809));
#35499=CARTESIAN_POINT('Ctrl Pts',(0.75400925402848,1.,-1.75631083600175));
#35500=CARTESIAN_POINT('Ctrl Pts',(0.755220979975262,1.,-1.7619781724032));
#35501=CARTESIAN_POINT('Ctrl Pts',(0.756421896028403,1.,-1.76789396003141));
#35502=CARTESIAN_POINT('Ctrl Pts',(0.757578264077238,1.,-1.77394167108342));
#35503=CARTESIAN_POINT('Ctrl Pts',(0.75865062667738,1.,-1.77999411220912));
#35504=CARTESIAN_POINT('Ctrl Pts',(0.759614401109868,1.,-1.78596964884527));
#35505=CARTESIAN_POINT('Ctrl Pts',(0.760469555880425,1.,-1.79185815610802));
#35506=CARTESIAN_POINT('Ctrl Pts',(0.761229695230359,1.,-1.79768986997735));
#35507=CARTESIAN_POINT('Ctrl Pts',(0.761915336443515,1.,-1.80351583877334));
#35508=CARTESIAN_POINT('Ctrl Pts',(0.762546129464036,1.,-1.80938551463989));
#35509=CARTESIAN_POINT('Ctrl Pts',(0.763132003836783,1.,-1.81532118405566));
#35510=CARTESIAN_POINT('Ctrl Pts',(0.763673465462854,1.,-1.82131873145297));
#35511=CARTESIAN_POINT('Ctrl Pts',(0.764165902606055,1.,-1.8273599120008));
#35512=CARTESIAN_POINT('Ctrl Pts',(0.764602549687845,1.,-1.8334207722714));
#35513=CARTESIAN_POINT('Ctrl Pts',(0.764978057881687,1.,-1.83948181064823));
#35514=CARTESIAN_POINT('Ctrl Pts',(0.765291664861971,1.,-1.84553698875911));
#35515=CARTESIAN_POINT('Ctrl Pts',(0.765545710619023,1.,-1.85158945130054));
#35516=CARTESIAN_POINT('Ctrl Pts',(0.765744212909305,1.,-1.85764741390391));
#35517=CARTESIAN_POINT('Ctrl Pts',(0.765891519092557,1.,-1.86372027063315));
#35518=CARTESIAN_POINT('Ctrl Pts',(0.765990708546111,1.,-1.86981398314345));
#35519=CARTESIAN_POINT('Ctrl Pts',(0.766042837036759,1.,-1.87592888967886));
#35520=CARTESIAN_POINT('Ctrl Pts',(0.766047794851868,1.,-1.88206215302561));
#35521=CARTESIAN_POINT('Ctrl Pts',(0.76600483706209,1.,-1.88820926433409));
#35522=CARTESIAN_POINT('Ctrl Pts',(0.765913193856979,1.,-1.89436577771389));
#35523=CARTESIAN_POINT('Ctrl Pts',(0.765772772593395,1.,-1.90052930393599));
#35524=CARTESIAN_POINT('Ctrl Pts',(0.765584196937936,1.,-1.90669961402362));
#35525=CARTESIAN_POINT('Ctrl Pts',(0.765348465884739,1.,-1.91287765805174));
#35526=CARTESIAN_POINT('Ctrl Pts',(0.765066729667095,1.,-1.91906491634197));
#35527=CARTESIAN_POINT('Ctrl Pts',(0.764740025488189,1.,-1.92526263537041));
#35528=CARTESIAN_POINT('Ctrl Pts',(0.764369010673889,1.,-1.93147105496367));
#35529=CARTESIAN_POINT('Ctrl Pts',(0.763954049121393,1.,-1.93768964875867));
#35530=CARTESIAN_POINT('Ctrl Pts',(0.76349533353858,1.,-1.94391746617626));
#35531=CARTESIAN_POINT('Ctrl Pts',(0.762992990878774,1.,-1.95015342590025));
#35532=CARTESIAN_POINT('Ctrl Pts',(0.762447203806263,1.,-1.95639665309893));
#35533=CARTESIAN_POINT('Ctrl Pts',(0.761858300014575,1.,-1.96264672744229));
#35534=CARTESIAN_POINT('Ctrl Pts',(0.761226690483986,1.,-1.96890351582545));
#35535=CARTESIAN_POINT('Ctrl Pts',(0.760552825409855,1.,-1.97516705321521));
#35536=CARTESIAN_POINT('Ctrl Pts',(0.759837147452135,1.,-1.98143741418156));
#35537=CARTESIAN_POINT('Ctrl Pts',(0.759080037802242,1.,-1.98771456680806));
#35538=CARTESIAN_POINT('Ctrl Pts',(0.758281796766377,1.,-1.9939983109871));
#35539=CARTESIAN_POINT('Ctrl Pts',(0.757442676862341,1.,-2.00028834739072));
#35540=CARTESIAN_POINT('Ctrl Pts',(0.756562904646496,1.,-2.00658431587682));
#35541=CARTESIAN_POINT('Ctrl Pts',(0.7556427049581,1.,-2.01288584328149));
#35542=CARTESIAN_POINT('Ctrl Pts',(0.75468233072352,1.,-2.01919259406003));
#35543=CARTESIAN_POINT('Ctrl Pts',(0.753682061113765,1.,-2.02550428623587));
#35544=CARTESIAN_POINT('Ctrl Pts',(0.752642180488104,1.,-2.03182068456467));
#35545=CARTESIAN_POINT('Ctrl Pts',(0.751562963361383,1.,-2.03814160092173));
#35546=CARTESIAN_POINT('Ctrl Pts',(0.750444657874758,1.,-2.04446689147754));
#35547=CARTESIAN_POINT('Ctrl Pts',(0.749287468663053,1.,-2.05079645591606));
#35548=CARTESIAN_POINT('Ctrl Pts',(0.748091554181101,1.,-2.05713023030263));
#35549=CARTESIAN_POINT('Ctrl Pts',(0.747103932785504,1.,-2.06220058927162));
#35550=CARTESIAN_POINT('Ctrl Pts',(0.746345871542695,1.,-2.06600523016401));
#35551=CARTESIAN_POINT('Ctrl Pts',(0.74583279137781,1.,-2.06854248895575));
#35552=CARTESIAN_POINT('Ctrl Pts',(0.745574324794401,1.,-2.0698113262342));
#35553=CARTESIAN_POINT('',(0.693717979106306,0.,-1.60662857109684));
#35554=CARTESIAN_POINT('Origin',(0.,0.,0.));
#35555=CARTESIAN_POINT('',(0.892032620296855,1.,-1.5055822144029));
#35556=CARTESIAN_POINT('Origin',(0.,1.,0.));
#35557=CARTESIAN_POINT('',(0.892032620296855,0.,-1.5055822144029));
#35558=CARTESIAN_POINT('Ctrl Pts',(1.23627494547115,-1.,-1.81978687191668));
#35559=CARTESIAN_POINT('Ctrl Pts',(1.23627494547115,1.,-1.81978687191668));
#35560=CARTESIAN_POINT('Ctrl Pts',(1.23509651170476,-1.,-1.81925017193666));
#35561=CARTESIAN_POINT('Ctrl Pts',(1.23509651170476,1.,-1.81925017193666));
#35562=CARTESIAN_POINT('Ctrl Pts',(1.2327422452705,-1.,-1.81817389921279));
#35563=CARTESIAN_POINT('Ctrl Pts',(1.2327422452705,1.,-1.81817389921279));
#35564=CARTESIAN_POINT('Ctrl Pts',(1.2292186489137,-1.,-1.8165508718364));
#35565=CARTESIAN_POINT('Ctrl Pts',(1.2292186489137,1.,-1.8165508718364));
#35566=CARTESIAN_POINT('Ctrl Pts',(1.2245361330495,-1.,-1.81436959210434));
#35567=CARTESIAN_POINT('Ctrl Pts',(1.2245361330495,1.,-1.81436959210434));
#35568=CARTESIAN_POINT('Ctrl Pts',(1.21870906103557,-1.,-1.81161420806656));
#35569=CARTESIAN_POINT('Ctrl Pts',(1.21870906103557,1.,-1.81161420806656));
#35570=CARTESIAN_POINT('Ctrl Pts',(1.21290815708314,-1.,-1.80882996917129));
#35571=CARTESIAN_POINT('Ctrl Pts',(1.21290815708314,1.,-1.80882996917129));
#35572=CARTESIAN_POINT('Ctrl Pts',(1.20713356605475,-1.,-1.80601678480707));
#35573=CARTESIAN_POINT('Ctrl Pts',(1.20713356605475,1.,-1.80601678480707));
#35574=CARTESIAN_POINT('Ctrl Pts',(1.20138548938974,-1.,-1.80317454838603));
#35575=CARTESIAN_POINT('Ctrl Pts',(1.20138548938974,1.,-1.80317454838603));
#35576=CARTESIAN_POINT('Ctrl Pts',(1.19566418930242,-1.,-1.80030314369879));
#35577=CARTESIAN_POINT('Ctrl Pts',(1.19566418930242,1.,-1.80030314369879));
#35578=CARTESIAN_POINT('Ctrl Pts',(1.18996997934445,-1.,-1.79740245923478));
#35579=CARTESIAN_POINT('Ctrl Pts',(1.18996997934445,1.,-1.79740245923478));
#35580=CARTESIAN_POINT('Ctrl Pts',(1.18430321697432,-1.,-1.79447240321515));
#35581=CARTESIAN_POINT('Ctrl Pts',(1.18430321697432,1.,-1.79447240321515));
#35582=CARTESIAN_POINT('Ctrl Pts',(1.17866429440809,-1.,-1.79151291552689));
#35583=CARTESIAN_POINT('Ctrl Pts',(1.17866429440809,1.,-1.79151291552689));
#35584=CARTESIAN_POINT('Ctrl Pts',(1.17305363177328,-1.,-1.78852398877617));
#35585=CARTESIAN_POINT('Ctrl Pts',(1.17305363177328,1.,-1.78852398877617));
#35586=CARTESIAN_POINT('Ctrl Pts',(1.16747166312303,-1.,-1.78550566040443));
#35587=CARTESIAN_POINT('Ctrl Pts',(1.16747166312303,1.,-1.78550566040443));
#35588=CARTESIAN_POINT('Ctrl Pts',(1.16191881298499,-1.,-1.78245795881009));
#35589=CARTESIAN_POINT('Ctrl Pts',(1.16191881298499,1.,-1.78245795881009));
#35590=CARTESIAN_POINT('Ctrl Pts',(1.15639547194698,-1.,-1.77938085564275));
#35591=CARTESIAN_POINT('Ctrl Pts',(1.15639547194698,1.,-1.77938085564275));
#35592=CARTESIAN_POINT('Ctrl Pts',(1.15090197841514,-1.,-1.7762742255701));
#35593=CARTESIAN_POINT('Ctrl Pts',(1.15090197841514,1.,-1.7762742255701));
#35594=CARTESIAN_POINT('Ctrl Pts',(1.1454385822692,-1.,-1.77313777896194));
#35595=CARTESIAN_POINT('Ctrl Pts',(1.1454385822692,1.,-1.77313777896194));
#35596=CARTESIAN_POINT('Ctrl Pts',(1.14000548336975,-1.,-1.76997111386769));
#35597=CARTESIAN_POINT('Ctrl Pts',(1.14000548336975,1.,-1.76997111386769));
#35598=CARTESIAN_POINT('Ctrl Pts',(1.1346029180462,-1.,-1.76677384551862));
#35599=CARTESIAN_POINT('Ctrl Pts',(1.1346029180462,1.,-1.76677384551862));
#35600=CARTESIAN_POINT('Ctrl Pts',(1.12923123555075,-1.,-1.7635457196617));
#35601=CARTESIAN_POINT('Ctrl Pts',(1.12923123555075,1.,-1.7635457196617));
#35602=CARTESIAN_POINT('Ctrl Pts',(1.12389096855086,-1.,-1.76028671825096));
#35603=CARTESIAN_POINT('Ctrl Pts',(1.12389096855086,1.,-1.76028671825096));
#35604=CARTESIAN_POINT('Ctrl Pts',(1.11858293216763,-1.,-1.75699720772105));
#35605=CARTESIAN_POINT('Ctrl Pts',(1.11858293216763,1.,-1.75699720772105));
#35606=CARTESIAN_POINT('Ctrl Pts',(1.11330807582551,-1.,-1.7536777209463));
#35607=CARTESIAN_POINT('Ctrl Pts',(1.11330807582551,1.,-1.7536777209463));
#35608=CARTESIAN_POINT('Ctrl Pts',(1.10806728183007,-1.,-1.7503286607592));
#35609=CARTESIAN_POINT('Ctrl Pts',(1.10806728183007,1.,-1.7503286607592));
#35610=CARTESIAN_POINT('Ctrl Pts',(1.10286118991143,-1.,-1.74695004214923));
#35611=CARTESIAN_POINT('Ctrl Pts',(1.10286118991143,1.,-1.74695004214923));
#35612=CARTESIAN_POINT('Ctrl Pts',(1.09768999241225,-1.,-1.74354119236208));
#35613=CARTESIAN_POINT('Ctrl Pts',(1.09768999241225,1.,-1.74354119236208));
#35614=CARTESIAN_POINT('Ctrl Pts',(1.09255329056493,-1.,-1.74010053962247));
#35615=CARTESIAN_POINT('Ctrl Pts',(1.09255329056493,1.,-1.74010053962247));
#35616=CARTESIAN_POINT('Ctrl Pts',(1.08745056285427,-1.,-1.73662628326091));
#35617=CARTESIAN_POINT('Ctrl Pts',(1.08745056285427,1.,-1.73662628326091));
#35618=CARTESIAN_POINT('Ctrl Pts',(1.08238162784749,-1.,-1.73311705663407));
#35619=CARTESIAN_POINT('Ctrl Pts',(1.08238162784749,1.,-1.73311705663407));
#35620=CARTESIAN_POINT('Ctrl Pts',(1.0773470373727,-1.,-1.72957248977424));
#35621=CARTESIAN_POINT('Ctrl Pts',(1.0773470373727,1.,-1.72957248977424));
#35622=CARTESIAN_POINT('Ctrl Pts',(1.07234866990252,-1.,-1.72599406198488));
#35623=CARTESIAN_POINT('Ctrl Pts',(1.07234866990252,1.,-1.72599406198488));
#35624=CARTESIAN_POINT('Ctrl Pts',(1.06738966975462,-1.,-1.72238500928453));
#35625=CARTESIAN_POINT('Ctrl Pts',(1.06738966975462,1.,-1.72238500928453));
#35626=CARTESIAN_POINT('Ctrl Pts',(1.06247324680647,-1.,-1.71874858456904));
#35627=CARTESIAN_POINT('Ctrl Pts',(1.06247324680647,1.,-1.71874858456904));
#35628=CARTESIAN_POINT('Ctrl Pts',(1.05760163192479,-1.,-1.7150865442702));
#35629=CARTESIAN_POINT('Ctrl Pts',(1.05760163192479,1.,-1.7150865442702));
#35630=CARTESIAN_POINT('Ctrl Pts',(1.05277517202855,-1.,-1.71139783543989));
#35631=CARTESIAN_POINT('Ctrl Pts',(1.05277517202855,1.,-1.71139783543989));
#35632=CARTESIAN_POINT('Ctrl Pts',(1.04799085404995,-1.,-1.70767646263649));
#35633=CARTESIAN_POINT('Ctrl Pts',(1.04799085404995,1.,-1.70767646263649));
#35634=CARTESIAN_POINT('Ctrl Pts',(1.04324363334554,-1.,-1.70391338707982));
#35635=CARTESIAN_POINT('Ctrl Pts',(1.04324363334554,1.,-1.70391338707982));
#35636=CARTESIAN_POINT('Ctrl Pts',(1.03852922490789,-1.,-1.70010052930962));
#35637=CARTESIAN_POINT('Ctrl Pts',(1.03852922490789,1.,-1.70010052930962));
#35638=CARTESIAN_POINT('Ctrl Pts',(1.03384646003588,-1.,-1.69623414782771));
#35639=CARTESIAN_POINT('Ctrl Pts',(1.03384646003588,1.,-1.69623414782771));
#35640=CARTESIAN_POINT('Ctrl Pts',(1.02919977579147,-1.,-1.69231840863458));
#35641=CARTESIAN_POINT('Ctrl Pts',(1.02919977579147,1.,-1.69231840863458));
#35642=CARTESIAN_POINT('Ctrl Pts',(1.02460180535255,-1.,-1.68836910178447));
#35643=CARTESIAN_POINT('Ctrl Pts',(1.02460180535255,1.,-1.68836910178447));
#35644=CARTESIAN_POINT('Ctrl Pts',(1.02006795074201,-1.,-1.68440578021706));
#35645=CARTESIAN_POINT('Ctrl Pts',(1.02006795074201,1.,-1.68440578021706));
#35646=CARTESIAN_POINT('Ctrl Pts',(1.01561026162773,-1.,-1.68044289894798));
#35647=CARTESIAN_POINT('Ctrl Pts',(1.01561026162773,1.,-1.68044289894798));
#35648=CARTESIAN_POINT('Ctrl Pts',(1.01123236493511,-1.,-1.67648246776464));
#35649=CARTESIAN_POINT('Ctrl Pts',(1.01123236493511,1.,-1.67648246776464));
#35650=CARTESIAN_POINT('Ctrl Pts',(1.00692206696414,-1.,-1.67250335383293));
#35651=CARTESIAN_POINT('Ctrl Pts',(1.00692206696414,1.,-1.67250335383293));
#35652=CARTESIAN_POINT('Ctrl Pts',(1.00265091003727,-1.,-1.66846059277303));
#35653=CARTESIAN_POINT('Ctrl Pts',(1.00265091003727,1.,-1.66846059277303));
#35654=CARTESIAN_POINT('Ctrl Pts',(0.998389654952757,-1.,-1.66430758030376));
#35655=CARTESIAN_POINT('Ctrl Pts',(0.998389654952757,1.,-1.66430758030376));
#35656=CARTESIAN_POINT('Ctrl Pts',(0.994121836661305,-1.,-1.66001553809947));
#35657=CARTESIAN_POINT('Ctrl Pts',(0.994121836661305,1.,-1.66001553809947));
#35658=CARTESIAN_POINT('Ctrl Pts',(0.989855627854164,-1.,-1.65559044289699));
#35659=CARTESIAN_POINT('Ctrl Pts',(0.989855627854164,1.,-1.65559044289699));
#35660=CARTESIAN_POINT('Ctrl Pts',(0.98564262292082,-1.,-1.65110016612638));
#35661=CARTESIAN_POINT('Ctrl Pts',(0.98564262292082,1.,-1.65110016612638));
#35662=CARTESIAN_POINT('Ctrl Pts',(0.981562530939489,-1.,-1.64665139190656));
#35663=CARTESIAN_POINT('Ctrl Pts',(0.981562530939489,1.,-1.64665139190656));
#35664=CARTESIAN_POINT('Ctrl Pts',(0.977689794119416,-1.,-1.64233990826687));
#35665=CARTESIAN_POINT('Ctrl Pts',(0.977689794119416,1.,-1.64233990826687));
#35666=CARTESIAN_POINT('Ctrl Pts',(0.974066058287418,-1.,-1.63820952658144));
#35667=CARTESIAN_POINT('Ctrl Pts',(0.974066058287418,1.,-1.63820952658144));
#35668=CARTESIAN_POINT('Ctrl Pts',(0.970669715997509,-1.,-1.63420665729798));
#35669=CARTESIAN_POINT('Ctrl Pts',(0.970669715997509,1.,-1.63420665729798));
#35670=CARTESIAN_POINT('Ctrl Pts',(0.967387853230345,-1.,-1.63013849959462));
#35671=CARTESIAN_POINT('Ctrl Pts',(0.967387853230345,1.,-1.63013849959462));
#35672=CARTESIAN_POINT('Ctrl Pts',(0.964046107040535,-1.,-1.62571930670187));
#35673=CARTESIAN_POINT('Ctrl Pts',(0.964046107040535,1.,-1.62571930670187));
#35674=CARTESIAN_POINT('Ctrl Pts',(0.960438326101728,-1.,-1.62061638140221));
#35675=CARTESIAN_POINT('Ctrl Pts',(0.960438326101728,1.,-1.62061638140221));
#35676=CARTESIAN_POINT('Ctrl Pts',(0.95635442292067,-1.,-1.61449324337085));
#35677=CARTESIAN_POINT('Ctrl Pts',(0.95635442292067,1.,-1.61449324337085));
#35678=CARTESIAN_POINT('Ctrl Pts',(0.951613284356035,-1.,-1.60706069896936));
#35679=CARTESIAN_POINT('Ctrl Pts',(0.951613284356035,1.,-1.60706069896936));
#35680=CARTESIAN_POINT('Ctrl Pts',(0.946078063315257,-1.,-1.59810042043673));
#35681=CARTESIAN_POINT('Ctrl Pts',(0.946078063315257,1.,-1.59810042043673));
#35682=CARTESIAN_POINT('Ctrl Pts',(0.939646377893399,-1.,-1.58744937487176));
#35683=CARTESIAN_POINT('Ctrl Pts',(0.939646377893399,1.,-1.58744937487176));
#35684=CARTESIAN_POINT('Ctrl Pts',(0.932246680108685,-1.,-1.57499388382243));
#35685=CARTESIAN_POINT('Ctrl Pts',(0.932246680108685,1.,-1.57499388382243));
#35686=CARTESIAN_POINT('Ctrl Pts',(0.923832188944341,-1.,-1.56065988578893));
#35687=CARTESIAN_POINT('Ctrl Pts',(0.923832188944341,1.,-1.56065988578893));
#35688=CARTESIAN_POINT('Ctrl Pts',(0.914375919026456,-1.,-1.54440491149498));
#35689=CARTESIAN_POINT('Ctrl Pts',(0.914375919026456,1.,-1.54440491149498));
#35690=CARTESIAN_POINT('Ctrl Pts',(0.905967409625651,-1.,-1.52984849887993));
#35691=CARTESIAN_POINT('Ctrl Pts',(0.905967409625651,1.,-1.52984849887993));
#35692=CARTESIAN_POINT('Ctrl Pts',(0.89918504748351,-1.,-1.51805569590094));
#35693=CARTESIAN_POINT('Ctrl Pts',(0.89918504748351,1.,-1.51805569590094));
#35694=CARTESIAN_POINT('Ctrl Pts',(0.894452006964543,-1.,-1.50980486806688));
#35695=CARTESIAN_POINT('Ctrl Pts',(0.894452006964543,1.,-1.50980486806688));
#35696=CARTESIAN_POINT('Ctrl Pts',(0.892032620296855,-1.,-1.5055822144029));
#35697=CARTESIAN_POINT('Ctrl Pts',(0.892032620296855,1.,-1.5055822144029));
#35698=CARTESIAN_POINT('',(1.23627494547115,1.,-1.81978687191668));
#35699=CARTESIAN_POINT('Ctrl Pts',(1.23627494547115,1.,-1.81978687191668));
#35700=CARTESIAN_POINT('Ctrl Pts',(1.23509651170476,1.,-1.81925017193666));
#35701=CARTESIAN_POINT('Ctrl Pts',(1.2327422452705,1.,-1.81817389921279));
#35702=CARTESIAN_POINT('Ctrl Pts',(1.2292186489137,1.,-1.8165508718364));
#35703=CARTESIAN_POINT('Ctrl Pts',(1.2245361330495,1.,-1.81436959210434));
#35704=CARTESIAN_POINT('Ctrl Pts',(1.21870906103557,1.,-1.81161420806656));
#35705=CARTESIAN_POINT('Ctrl Pts',(1.21290815708314,1.,-1.80882996917129));
#35706=CARTESIAN_POINT('Ctrl Pts',(1.20713356605475,1.,-1.80601678480707));
#35707=CARTESIAN_POINT('Ctrl Pts',(1.20138548938974,1.,-1.80317454838603));
#35708=CARTESIAN_POINT('Ctrl Pts',(1.19566418930242,1.,-1.80030314369879));
#35709=CARTESIAN_POINT('Ctrl Pts',(1.18996997934445,1.,-1.79740245923478));
#35710=CARTESIAN_POINT('Ctrl Pts',(1.18430321697432,1.,-1.79447240321515));
#35711=CARTESIAN_POINT('Ctrl Pts',(1.17866429440809,1.,-1.79151291552689));
#35712=CARTESIAN_POINT('Ctrl Pts',(1.17305363177328,1.,-1.78852398877617));
#35713=CARTESIAN_POINT('Ctrl Pts',(1.16747166312303,1.,-1.78550566040443));
#35714=CARTESIAN_POINT('Ctrl Pts',(1.16191881298499,1.,-1.78245795881009));
#35715=CARTESIAN_POINT('Ctrl Pts',(1.15639547194698,1.,-1.77938085564275));
#35716=CARTESIAN_POINT('Ctrl Pts',(1.15090197841514,1.,-1.7762742255701));
#35717=CARTESIAN_POINT('Ctrl Pts',(1.1454385822692,1.,-1.77313777896194));
#35718=CARTESIAN_POINT('Ctrl Pts',(1.14000548336975,1.,-1.76997111386769));
#35719=CARTESIAN_POINT('Ctrl Pts',(1.1346029180462,1.,-1.76677384551862));
#35720=CARTESIAN_POINT('Ctrl Pts',(1.12923123555075,1.,-1.7635457196617));
#35721=CARTESIAN_POINT('Ctrl Pts',(1.12389096855086,1.,-1.76028671825096));
#35722=CARTESIAN_POINT('Ctrl Pts',(1.11858293216763,1.,-1.75699720772105));
#35723=CARTESIAN_POINT('Ctrl Pts',(1.11330807582551,1.,-1.7536777209463));
#35724=CARTESIAN_POINT('Ctrl Pts',(1.10806728183007,1.,-1.7503286607592));
#35725=CARTESIAN_POINT('Ctrl Pts',(1.10286118991143,1.,-1.74695004214923));
#35726=CARTESIAN_POINT('Ctrl Pts',(1.09768999241225,1.,-1.74354119236208));
#35727=CARTESIAN_POINT('Ctrl Pts',(1.09255329056493,1.,-1.74010053962247));
#35728=CARTESIAN_POINT('Ctrl Pts',(1.08745056285427,1.,-1.73662628326091));
#35729=CARTESIAN_POINT('Ctrl Pts',(1.08238162784749,1.,-1.73311705663407));
#35730=CARTESIAN_POINT('Ctrl Pts',(1.0773470373727,1.,-1.72957248977424));
#35731=CARTESIAN_POINT('Ctrl Pts',(1.07234866990252,1.,-1.72599406198488));
#35732=CARTESIAN_POINT('Ctrl Pts',(1.06738966975462,1.,-1.72238500928453));
#35733=CARTESIAN_POINT('Ctrl Pts',(1.06247324680647,1.,-1.71874858456904));
#35734=CARTESIAN_POINT('Ctrl Pts',(1.05760163192479,1.,-1.7150865442702));
#35735=CARTESIAN_POINT('Ctrl Pts',(1.05277517202855,1.,-1.71139783543989));
#35736=CARTESIAN_POINT('Ctrl Pts',(1.04799085404995,1.,-1.70767646263649));
#35737=CARTESIAN_POINT('Ctrl Pts',(1.04324363334554,1.,-1.70391338707982));
#35738=CARTESIAN_POINT('Ctrl Pts',(1.03852922490789,1.,-1.70010052930962));
#35739=CARTESIAN_POINT('Ctrl Pts',(1.03384646003588,1.,-1.69623414782771));
#35740=CARTESIAN_POINT('Ctrl Pts',(1.02919977579147,1.,-1.69231840863458));
#35741=CARTESIAN_POINT('Ctrl Pts',(1.02460180535255,1.,-1.68836910178447));
#35742=CARTESIAN_POINT('Ctrl Pts',(1.02006795074201,1.,-1.68440578021706));
#35743=CARTESIAN_POINT('Ctrl Pts',(1.01561026162773,1.,-1.68044289894798));
#35744=CARTESIAN_POINT('Ctrl Pts',(1.01123236493511,1.,-1.67648246776464));
#35745=CARTESIAN_POINT('Ctrl Pts',(1.00692206696414,1.,-1.67250335383293));
#35746=CARTESIAN_POINT('Ctrl Pts',(1.00265091003727,1.,-1.66846059277303));
#35747=CARTESIAN_POINT('Ctrl Pts',(0.998389654952757,1.,-1.66430758030376));
#35748=CARTESIAN_POINT('Ctrl Pts',(0.994121836661305,1.,-1.66001553809947));
#35749=CARTESIAN_POINT('Ctrl Pts',(0.989855627854164,1.,-1.65559044289699));
#35750=CARTESIAN_POINT('Ctrl Pts',(0.98564262292082,1.,-1.65110016612638));
#35751=CARTESIAN_POINT('Ctrl Pts',(0.981562530939489,1.,-1.64665139190656));
#35752=CARTESIAN_POINT('Ctrl Pts',(0.977689794119416,1.,-1.64233990826687));
#35753=CARTESIAN_POINT('Ctrl Pts',(0.974066058287418,1.,-1.63820952658144));
#35754=CARTESIAN_POINT('Ctrl Pts',(0.970669715997509,1.,-1.63420665729798));
#35755=CARTESIAN_POINT('Ctrl Pts',(0.967387853230345,1.,-1.63013849959462));
#35756=CARTESIAN_POINT('Ctrl Pts',(0.964046107040535,1.,-1.62571930670187));
#35757=CARTESIAN_POINT('Ctrl Pts',(0.960438326101728,1.,-1.62061638140221));
#35758=CARTESIAN_POINT('Ctrl Pts',(0.95635442292067,1.,-1.61449324337085));
#35759=CARTESIAN_POINT('Ctrl Pts',(0.951613284356035,1.,-1.60706069896936));
#35760=CARTESIAN_POINT('Ctrl Pts',(0.946078063315257,1.,-1.59810042043673));
#35761=CARTESIAN_POINT('Ctrl Pts',(0.939646377893399,1.,-1.58744937487176));
#35762=CARTESIAN_POINT('Ctrl Pts',(0.932246680108685,1.,-1.57499388382243));
#35763=CARTESIAN_POINT('Ctrl Pts',(0.923832188944341,1.,-1.56065988578893));
#35764=CARTESIAN_POINT('Ctrl Pts',(0.914375919026456,1.,-1.54440491149498));
#35765=CARTESIAN_POINT('Ctrl Pts',(0.905967409625651,1.,-1.52984849887993));
#35766=CARTESIAN_POINT('Ctrl Pts',(0.89918504748351,1.,-1.51805569590094));
#35767=CARTESIAN_POINT('Ctrl Pts',(0.894452006964543,1.,-1.50980486806688));
#35768=CARTESIAN_POINT('Ctrl Pts',(0.892032620296855,1.,-1.5055822144029));
#35769=CARTESIAN_POINT('',(1.23627494547115,0.,-1.81978687191668));
#35770=CARTESIAN_POINT('Origin',(1.34869019493419,0.,-1.73811241238545));
#35771=CARTESIAN_POINT('',(1.34869019493419,1.,-1.73811241238545));
#35772=CARTESIAN_POINT('',(1.23627494547115,1.,-1.81978687191668));
#35773=CARTESIAN_POINT('',(1.34869019493419,0.,-1.73811241238545));
#35774=CARTESIAN_POINT('Ctrl Pts',(1.15624053661742,-1.,-1.31362392696032));
#35775=CARTESIAN_POINT('Ctrl Pts',(1.15624053661742,1.,-1.31362392696032));
#35776=CARTESIAN_POINT('Ctrl Pts',(1.15950888730809,-1.,-1.31722977216397));
#35777=CARTESIAN_POINT('Ctrl Pts',(1.15950888730809,1.,-1.31722977216397));
#35778=CARTESIAN_POINT('Ctrl Pts',(1.16589330093588,-1.,-1.32428080721772));
#35779=CARTESIAN_POINT('Ctrl Pts',(1.16589330093588,1.,-1.32428080721772));
#35780=CARTESIAN_POINT('Ctrl Pts',(1.17501305789857,-1.,-1.33437539347008));
#35781=CARTESIAN_POINT('Ctrl Pts',(1.17501305789857,1.,-1.33437539347008));
#35782=CARTESIAN_POINT('Ctrl Pts',(1.18625865667441,-1.,-1.34687054001093));
#35783=CARTESIAN_POINT('Ctrl Pts',(1.18625865667441,1.,-1.34687054001093));
#35784=CARTESIAN_POINT('Ctrl Pts',(1.1987959077932,-1.,-1.36088705043885));
#35785=CARTESIAN_POINT('Ctrl Pts',(1.1987959077932,1.,-1.36088705043885));
#35786=CARTESIAN_POINT('Ctrl Pts',(1.20982812925645,-1.,-1.37331915607905));
#35787=CARTESIAN_POINT('Ctrl Pts',(1.20982812925645,1.,-1.37331915607905));
#35788=CARTESIAN_POINT('Ctrl Pts',(1.21938737280852,-1.,-1.38420564527715));
#35789=CARTESIAN_POINT('Ctrl Pts',(1.21938737280852,1.,-1.38420564527715));
#35790=CARTESIAN_POINT('Ctrl Pts',(1.22752961899387,-1.,-1.39361389568796));
#35791=CARTESIAN_POINT('Ctrl Pts',(1.22752961899387,1.,-1.39361389568796));
#35792=CARTESIAN_POINT('Ctrl Pts',(1.23434087290423,-1.,-1.40164708206106));
#35793=CARTESIAN_POINT('Ctrl Pts',(1.23434087290423,1.,-1.40164708206106));
#35794=CARTESIAN_POINT('Ctrl Pts',(1.23994455029534,-1.,-1.40845295531283));
#35795=CARTESIAN_POINT('Ctrl Pts',(1.23994455029534,1.,-1.40845295531283));
#35796=CARTESIAN_POINT('Ctrl Pts',(1.24450600513056,-1.,-1.41422913175179));
#35797=CARTESIAN_POINT('Ctrl Pts',(1.24450600513056,1.,-1.41422913175179));
#35798=CARTESIAN_POINT('Ctrl Pts',(1.24824430986571,-1.,-1.41923722596025));
#35799=CARTESIAN_POINT('Ctrl Pts',(1.24824430986571,1.,-1.41923722596025));
#35800=CARTESIAN_POINT('Ctrl Pts',(1.2514145557001,-1.,-1.42378102115575));
#35801=CARTESIAN_POINT('Ctrl Pts',(1.2514145557001,1.,-1.42378102115575));
#35802=CARTESIAN_POINT('Ctrl Pts',(1.25426945222639,-1.,-1.42815938799387));
#35803=CARTESIAN_POINT('Ctrl Pts',(1.25426945222639,1.,-1.42815938799387));
#35804=CARTESIAN_POINT('Ctrl Pts',(1.25702687965755,-1.,-1.43262645609691));
#35805=CARTESIAN_POINT('Ctrl Pts',(1.25702687965755,1.,-1.43262645609691));
#35806=CARTESIAN_POINT('Ctrl Pts',(1.25983531012005,-1.,-1.43734919180848));
#35807=CARTESIAN_POINT('Ctrl Pts',(1.25983531012005,1.,-1.43734919180848));
#35808=CARTESIAN_POINT('Ctrl Pts',(1.26273903323858,-1.,-1.44236470511303));
#35809=CARTESIAN_POINT('Ctrl Pts',(1.26273903323858,1.,-1.44236470511303));
#35810=CARTESIAN_POINT('Ctrl Pts',(1.26570925118868,-1.,-1.44761985001662));
#35811=CARTESIAN_POINT('Ctrl Pts',(1.26570925118868,1.,-1.44761985001662));
#35812=CARTESIAN_POINT('Ctrl Pts',(1.2686778680489,-1.,-1.45301422764247));
#35813=CARTESIAN_POINT('Ctrl Pts',(1.2686778680489,1.,-1.45301422764247));
#35814=CARTESIAN_POINT('Ctrl Pts',(1.27156805265289,-1.,-1.45843906294697));
#35815=CARTESIAN_POINT('Ctrl Pts',(1.27156805265289,1.,-1.45843906294697));
#35816=CARTESIAN_POINT('Ctrl Pts',(1.27433119897822,-1.,-1.46382431332476));
#35817=CARTESIAN_POINT('Ctrl Pts',(1.27433119897822,1.,-1.46382431332476));
#35818=CARTESIAN_POINT('Ctrl Pts',(1.27696414831089,-1.,-1.46916035917133));
#35819=CARTESIAN_POINT('Ctrl Pts',(1.27696414831089,1.,-1.46916035917133));
#35820=CARTESIAN_POINT('Ctrl Pts',(1.2794891824849,-1.,-1.4744717526707));
#35821=CARTESIAN_POINT('Ctrl Pts',(1.2794891824849,1.,-1.4744717526707));
#35822=CARTESIAN_POINT('Ctrl Pts',(1.28194158939517,-1.,-1.47980070347096));
#35823=CARTESIAN_POINT('Ctrl Pts',(1.28194158939517,1.,-1.47980070347096));
#35824=CARTESIAN_POINT('Ctrl Pts',(1.28435533880201,-1.,-1.4851881711891));
#35825=CARTESIAN_POINT('Ctrl Pts',(1.28435533880201,1.,-1.4851881711891));
#35826=CARTESIAN_POINT('Ctrl Pts',(1.2867467611644,-1.,-1.4906522831278));
#35827=CARTESIAN_POINT('Ctrl Pts',(1.2867467611644,1.,-1.4906522831278));
#35828=CARTESIAN_POINT('Ctrl Pts',(1.28911506584254,-1.,-1.49618896881754));
#35829=CARTESIAN_POINT('Ctrl Pts',(1.28911506584254,1.,-1.49618896881754));
#35830=CARTESIAN_POINT('Ctrl Pts',(1.29145022885181,-1.,-1.50178230149776));
#35831=CARTESIAN_POINT('Ctrl Pts',(1.29145022885181,1.,-1.50178230149776));
#35832=CARTESIAN_POINT('Ctrl Pts',(1.29373841372842,-1.,-1.50741159078365));
#35833=CARTESIAN_POINT('Ctrl Pts',(1.29373841372842,1.,-1.50741159078365));
#35834=CARTESIAN_POINT('Ctrl Pts',(1.29596850710509,-1.,-1.51305994241402));
#35835=CARTESIAN_POINT('Ctrl Pts',(1.29596850710509,1.,-1.51305994241402));
#35836=CARTESIAN_POINT('Ctrl Pts',(1.29813791800747,-1.,-1.51872184912724));
#35837=CARTESIAN_POINT('Ctrl Pts',(1.29813791800747,1.,-1.51872184912724));
#35838=CARTESIAN_POINT('Ctrl Pts',(1.30024984366328,-1.,-1.52439957861062));
#35839=CARTESIAN_POINT('Ctrl Pts',(1.30024984366328,1.,-1.52439957861062));
#35840=CARTESIAN_POINT('Ctrl Pts',(1.30231064395568,-1.,-1.53009970283891));
#35841=CARTESIAN_POINT('Ctrl Pts',(1.30231064395568,1.,-1.53009970283891));
#35842=CARTESIAN_POINT('Ctrl Pts',(1.30432735639489,-1.,-1.53582981268977));
#35843=CARTESIAN_POINT('Ctrl Pts',(1.30432735639489,1.,-1.53582981268977));
#35844=CARTESIAN_POINT('Ctrl Pts',(1.30630475189556,-1.,-1.54159462645432));
#35845=CARTESIAN_POINT('Ctrl Pts',(1.30630475189556,1.,-1.54159462645432));
#35846=CARTESIAN_POINT('Ctrl Pts',(1.30824393907473,-1.,-1.54739413957185));
#35847=CARTESIAN_POINT('Ctrl Pts',(1.30824393907473,1.,-1.54739413957185));
#35848=CARTESIAN_POINT('Ctrl Pts',(1.31014393684222,-1.,-1.55322568759481));
#35849=CARTESIAN_POINT('Ctrl Pts',(1.31014393684222,1.,-1.55322568759481));
#35850=CARTESIAN_POINT('Ctrl Pts',(1.31200264341696,-1.,-1.55908521254821));
#35851=CARTESIAN_POINT('Ctrl Pts',(1.31200264341696,1.,-1.55908521254821));
#35852=CARTESIAN_POINT('Ctrl Pts',(1.31381795281002,-1.,-1.56496872402353));
#35853=CARTESIAN_POINT('Ctrl Pts',(1.31381795281002,1.,-1.56496872402353));
#35854=CARTESIAN_POINT('Ctrl Pts',(1.31558903860016,-1.,-1.57087397835723));
#35855=CARTESIAN_POINT('Ctrl Pts',(1.31558903860016,1.,-1.57087397835723));
#35856=CARTESIAN_POINT('Ctrl Pts',(1.31731642317187,-1.,-1.5768005650559));
#35857=CARTESIAN_POINT('Ctrl Pts',(1.31731642317187,1.,-1.5768005650559));
#35858=CARTESIAN_POINT('Ctrl Pts',(1.31900135021432,-1.,-1.58274907898834));
#35859=CARTESIAN_POINT('Ctrl Pts',(1.31900135021432,1.,-1.58274907898834));
#35860=CARTESIAN_POINT('Ctrl Pts',(1.32064537110892,-1.,-1.58872057258245));
#35861=CARTESIAN_POINT('Ctrl Pts',(1.32064537110892,1.,-1.58872057258245));
#35862=CARTESIAN_POINT('Ctrl Pts',(1.32224985747682,-1.,-1.59471591079403));
#35863=CARTESIAN_POINT('Ctrl Pts',(1.32224985747682,1.,-1.59471591079403));
#35864=CARTESIAN_POINT('Ctrl Pts',(1.32381550858256,-1.,-1.60073511858687));
#35865=CARTESIAN_POINT('Ctrl Pts',(1.32381550858256,1.,-1.60073511858687));
#35866=CARTESIAN_POINT('Ctrl Pts',(1.32534250785782,-1.,-1.60677758290954));
#35867=CARTESIAN_POINT('Ctrl Pts',(1.32534250785782,1.,-1.60677758290954));
#35868=CARTESIAN_POINT('Ctrl Pts',(1.32683074483356,-1.,-1.6128423401575));
#35869=CARTESIAN_POINT('Ctrl Pts',(1.32683074483356,1.,-1.6128423401575));
#35870=CARTESIAN_POINT('Ctrl Pts',(1.32828000610449,-1.,-1.61892832270724));
#35871=CARTESIAN_POINT('Ctrl Pts',(1.32828000610449,1.,-1.61892832270724));
#35872=CARTESIAN_POINT('Ctrl Pts',(1.3296901950568,-1.,-1.62503464209797));
#35873=CARTESIAN_POINT('Ctrl Pts',(1.3296901950568,1.,-1.62503464209797));
#35874=CARTESIAN_POINT('Ctrl Pts',(1.33106149345645,-1.,-1.63116079730923));
#35875=CARTESIAN_POINT('Ctrl Pts',(1.33106149345645,1.,-1.63116079730923));
#35876=CARTESIAN_POINT('Ctrl Pts',(1.33239425103724,-1.,-1.63730653475089));
#35877=CARTESIAN_POINT('Ctrl Pts',(1.33239425103724,1.,-1.63730653475089));
#35878=CARTESIAN_POINT('Ctrl Pts',(1.33368890676572,-1.,-1.6434717485603));
#35879=CARTESIAN_POINT('Ctrl Pts',(1.33368890676572,1.,-1.6434717485603));
#35880=CARTESIAN_POINT('Ctrl Pts',(1.33494590467993,-1.,-1.6496563728683));
#35881=CARTESIAN_POINT('Ctrl Pts',(1.33494590467993,1.,-1.6496563728683));
#35882=CARTESIAN_POINT('Ctrl Pts',(1.33616559745172,-1.,-1.65586025952593));
#35883=CARTESIAN_POINT('Ctrl Pts',(1.33616559745172,1.,-1.65586025952593));
#35884=CARTESIAN_POINT('Ctrl Pts',(1.33734820885262,-1.,-1.66208312541983));
#35885=CARTESIAN_POINT('Ctrl Pts',(1.33734820885262,1.,-1.66208312541983));
#35886=CARTESIAN_POINT('Ctrl Pts',(1.33849388654388,-1.,-1.66832460783989));
#35887=CARTESIAN_POINT('Ctrl Pts',(1.33849388654388,1.,-1.66832460783989));
#35888=CARTESIAN_POINT('Ctrl Pts',(1.3396027347034,-1.,-1.67458429426086));
#35889=CARTESIAN_POINT('Ctrl Pts',(1.3396027347034,1.,-1.67458429426086));
#35890=CARTESIAN_POINT('Ctrl Pts',(1.34067485185203,-1.,-1.68086176030362));
#35891=CARTESIAN_POINT('Ctrl Pts',(1.34067485185203,1.,-1.68086176030362));
#35892=CARTESIAN_POINT('Ctrl Pts',(1.341710374848,-1.,-1.68715660868764));
#35893=CARTESIAN_POINT('Ctrl Pts',(1.341710374848,1.,-1.68715660868764));
#35894=CARTESIAN_POINT('Ctrl Pts',(1.34270948206319,-1.,-1.6934684849687));
#35895=CARTESIAN_POINT('Ctrl Pts',(1.34270948206319,1.,-1.6934684849687));
#35896=CARTESIAN_POINT('Ctrl Pts',(1.34367237124483,-1.,-1.69979707754427));
#35897=CARTESIAN_POINT('Ctrl Pts',(1.34367237124483,1.,-1.69979707754427));
#35898=CARTESIAN_POINT('Ctrl Pts',(1.34459924533831,-1.,-1.70614212266738));
#35899=CARTESIAN_POINT('Ctrl Pts',(1.34459924533831,1.,-1.70614212266738));
#35900=CARTESIAN_POINT('Ctrl Pts',(1.34549029589416,-1.,-1.71250340686822));
#35901=CARTESIAN_POINT('Ctrl Pts',(1.34549029589416,1.,-1.71250340686822));
#35902=CARTESIAN_POINT('Ctrl Pts',(1.34634568653227,-1.,-1.7188807715049));
#35903=CARTESIAN_POINT('Ctrl Pts',(1.34634568653227,1.,-1.7188807715049));
#35904=CARTESIAN_POINT('Ctrl Pts',(1.34716554819527,-1.,-1.72527410680674));
#35905=CARTESIAN_POINT('Ctrl Pts',(1.34716554819527,1.,-1.72527410680674));
#35906=CARTESIAN_POINT('Ctrl Pts',(1.34779309152035,-1.,-1.7304014965394));
#35907=CARTESIAN_POINT('Ctrl Pts',(1.34779309152035,1.,-1.7304014965394));
#35908=CARTESIAN_POINT('Ctrl Pts',(1.34824783112887,-1.,-1.73425417885907));
#35909=CARTESIAN_POINT('Ctrl Pts',(1.34824783112887,1.,-1.73425417885907));
#35910=CARTESIAN_POINT('Ctrl Pts',(1.34854391898045,-1.,-1.73682580585691));
#35911=CARTESIAN_POINT('Ctrl Pts',(1.34854391898045,1.,-1.73682580585691));
#35912=CARTESIAN_POINT('Ctrl Pts',(1.34869019493419,-1.,-1.73811241238545));
#35913=CARTESIAN_POINT('Ctrl Pts',(1.34869019493419,1.,-1.73811241238545));
#35914=CARTESIAN_POINT('',(1.15624053661742,1.,-1.31362392696032));
#35915=CARTESIAN_POINT('Ctrl Pts',(1.15624053661742,1.,-1.31362392696032));
#35916=CARTESIAN_POINT('Ctrl Pts',(1.15950888730809,1.,-1.31722977216397));
#35917=CARTESIAN_POINT('Ctrl Pts',(1.16589330093588,1.,-1.32428080721772));
#35918=CARTESIAN_POINT('Ctrl Pts',(1.17501305789857,1.,-1.33437539347008));
#35919=CARTESIAN_POINT('Ctrl Pts',(1.18625865667441,1.,-1.34687054001093));
#35920=CARTESIAN_POINT('Ctrl Pts',(1.1987959077932,1.,-1.36088705043885));
#35921=CARTESIAN_POINT('Ctrl Pts',(1.20982812925645,1.,-1.37331915607905));
#35922=CARTESIAN_POINT('Ctrl Pts',(1.21938737280852,1.,-1.38420564527715));
#35923=CARTESIAN_POINT('Ctrl Pts',(1.22752961899387,1.,-1.39361389568796));
#35924=CARTESIAN_POINT('Ctrl Pts',(1.23434087290423,1.,-1.40164708206106));
#35925=CARTESIAN_POINT('Ctrl Pts',(1.23994455029534,1.,-1.40845295531283));
#35926=CARTESIAN_POINT('Ctrl Pts',(1.24450600513056,1.,-1.41422913175179));
#35927=CARTESIAN_POINT('Ctrl Pts',(1.24824430986571,1.,-1.41923722596025));
#35928=CARTESIAN_POINT('Ctrl Pts',(1.2514145557001,1.,-1.42378102115575));
#35929=CARTESIAN_POINT('Ctrl Pts',(1.25426945222639,1.,-1.42815938799387));
#35930=CARTESIAN_POINT('Ctrl Pts',(1.25702687965755,1.,-1.43262645609691));
#35931=CARTESIAN_POINT('Ctrl Pts',(1.25983531012005,1.,-1.43734919180848));
#35932=CARTESIAN_POINT('Ctrl Pts',(1.26273903323858,1.,-1.44236470511303));
#35933=CARTESIAN_POINT('Ctrl Pts',(1.26570925118868,1.,-1.44761985001662));
#35934=CARTESIAN_POINT('Ctrl Pts',(1.2686778680489,1.,-1.45301422764247));
#35935=CARTESIAN_POINT('Ctrl Pts',(1.27156805265289,1.,-1.45843906294697));
#35936=CARTESIAN_POINT('Ctrl Pts',(1.27433119897822,1.,-1.46382431332476));
#35937=CARTESIAN_POINT('Ctrl Pts',(1.27696414831089,1.,-1.46916035917133));
#35938=CARTESIAN_POINT('Ctrl Pts',(1.2794891824849,1.,-1.4744717526707));
#35939=CARTESIAN_POINT('Ctrl Pts',(1.28194158939517,1.,-1.47980070347096));
#35940=CARTESIAN_POINT('Ctrl Pts',(1.28435533880201,1.,-1.4851881711891));
#35941=CARTESIAN_POINT('Ctrl Pts',(1.2867467611644,1.,-1.4906522831278));
#35942=CARTESIAN_POINT('Ctrl Pts',(1.28911506584254,1.,-1.49618896881754));
#35943=CARTESIAN_POINT('Ctrl Pts',(1.29145022885181,1.,-1.50178230149776));
#35944=CARTESIAN_POINT('Ctrl Pts',(1.29373841372842,1.,-1.50741159078365));
#35945=CARTESIAN_POINT('Ctrl Pts',(1.29596850710509,1.,-1.51305994241402));
#35946=CARTESIAN_POINT('Ctrl Pts',(1.29813791800747,1.,-1.51872184912724));
#35947=CARTESIAN_POINT('Ctrl Pts',(1.30024984366328,1.,-1.52439957861062));
#35948=CARTESIAN_POINT('Ctrl Pts',(1.30231064395568,1.,-1.53009970283891));
#35949=CARTESIAN_POINT('Ctrl Pts',(1.30432735639489,1.,-1.53582981268977));
#35950=CARTESIAN_POINT('Ctrl Pts',(1.30630475189556,1.,-1.54159462645432));
#35951=CARTESIAN_POINT('Ctrl Pts',(1.30824393907473,1.,-1.54739413957185));
#35952=CARTESIAN_POINT('Ctrl Pts',(1.31014393684222,1.,-1.55322568759481));
#35953=CARTESIAN_POINT('Ctrl Pts',(1.31200264341696,1.,-1.55908521254821));
#35954=CARTESIAN_POINT('Ctrl Pts',(1.31381795281002,1.,-1.56496872402353));
#35955=CARTESIAN_POINT('Ctrl Pts',(1.31558903860016,1.,-1.57087397835723));
#35956=CARTESIAN_POINT('Ctrl Pts',(1.31731642317187,1.,-1.5768005650559));
#35957=CARTESIAN_POINT('Ctrl Pts',(1.31900135021432,1.,-1.58274907898834));
#35958=CARTESIAN_POINT('Ctrl Pts',(1.32064537110892,1.,-1.58872057258245));
#35959=CARTESIAN_POINT('Ctrl Pts',(1.32224985747682,1.,-1.59471591079403));
#35960=CARTESIAN_POINT('Ctrl Pts',(1.32381550858256,1.,-1.60073511858687));
#35961=CARTESIAN_POINT('Ctrl Pts',(1.32534250785782,1.,-1.60677758290954));
#35962=CARTESIAN_POINT('Ctrl Pts',(1.32683074483356,1.,-1.6128423401575));
#35963=CARTESIAN_POINT('Ctrl Pts',(1.32828000610449,1.,-1.61892832270724));
#35964=CARTESIAN_POINT('Ctrl Pts',(1.3296901950568,1.,-1.62503464209797));
#35965=CARTESIAN_POINT('Ctrl Pts',(1.33106149345645,1.,-1.63116079730923));
#35966=CARTESIAN_POINT('Ctrl Pts',(1.33239425103724,1.,-1.63730653475089));
#35967=CARTESIAN_POINT('Ctrl Pts',(1.33368890676572,1.,-1.6434717485603));
#35968=CARTESIAN_POINT('Ctrl Pts',(1.33494590467993,1.,-1.6496563728683));
#35969=CARTESIAN_POINT('Ctrl Pts',(1.33616559745172,1.,-1.65586025952593));
#35970=CARTESIAN_POINT('Ctrl Pts',(1.33734820885262,1.,-1.66208312541983));
#35971=CARTESIAN_POINT('Ctrl Pts',(1.33849388654388,1.,-1.66832460783989));
#35972=CARTESIAN_POINT('Ctrl Pts',(1.3396027347034,1.,-1.67458429426086));
#35973=CARTESIAN_POINT('Ctrl Pts',(1.34067485185203,1.,-1.68086176030362));
#35974=CARTESIAN_POINT('Ctrl Pts',(1.341710374848,1.,-1.68715660868764));
#35975=CARTESIAN_POINT('Ctrl Pts',(1.34270948206319,1.,-1.6934684849687));
#35976=CARTESIAN_POINT('Ctrl Pts',(1.34367237124483,1.,-1.69979707754427));
#35977=CARTESIAN_POINT('Ctrl Pts',(1.34459924533831,1.,-1.70614212266738));
#35978=CARTESIAN_POINT('Ctrl Pts',(1.34549029589416,1.,-1.71250340686822));
#35979=CARTESIAN_POINT('Ctrl Pts',(1.34634568653227,1.,-1.7188807715049));
#35980=CARTESIAN_POINT('Ctrl Pts',(1.34716554819527,1.,-1.72527410680674));
#35981=CARTESIAN_POINT('Ctrl Pts',(1.34779309152035,1.,-1.7304014965394));
#35982=CARTESIAN_POINT('Ctrl Pts',(1.34824783112887,1.,-1.73425417885907));
#35983=CARTESIAN_POINT('Ctrl Pts',(1.34854391898045,1.,-1.73682580585691));
#35984=CARTESIAN_POINT('Ctrl Pts',(1.34869019493419,1.,-1.73811241238545));
#35985=CARTESIAN_POINT('',(1.15624053661742,0.,-1.31362392696032));
#35986=CARTESIAN_POINT('Origin',(0.,0.,0.));
#35987=CARTESIAN_POINT('',(1.31362392696032,1.,-1.15624053661742));
#35988=CARTESIAN_POINT('Origin',(0.,1.,0.));
#35989=CARTESIAN_POINT('',(1.31362392696032,0.,-1.15624053661742));
#35990=CARTESIAN_POINT('Ctrl Pts',(1.73811241238545,-1.,-1.34869019493419));
#35991=CARTESIAN_POINT('Ctrl Pts',(1.73811241238545,1.,-1.34869019493419));
#35992=CARTESIAN_POINT('Ctrl Pts',(1.73682580585819,-1.,-1.34854391898145));
#35993=CARTESIAN_POINT('Ctrl Pts',(1.73682580585819,1.,-1.34854391898145));
#35994=CARTESIAN_POINT('Ctrl Pts',(1.73425417886254,-1.,-1.34824783113158));
#35995=CARTESIAN_POINT('Ctrl Pts',(1.73425417886254,1.,-1.34824783113158));
#35996=CARTESIAN_POINT('Ctrl Pts',(1.73040149654497,-1.,-1.3477930915247));
#35997=CARTESIAN_POINT('Ctrl Pts',(1.73040149654497,1.,-1.3477930915247));
#35998=CARTESIAN_POINT('Ctrl Pts',(1.72527410681298,-1.,-1.34716554820013));
#35999=CARTESIAN_POINT('Ctrl Pts',(1.72527410681298,1.,-1.34716554820013));
#36000=CARTESIAN_POINT('Ctrl Pts',(1.7188807715095,-1.,-1.34634568653586));
#36001=CARTESIAN_POINT('Ctrl Pts',(1.7188807715095,1.,-1.34634568653586));
#36002=CARTESIAN_POINT('Ctrl Pts',(1.71250340687011,-1.,-1.34549029589563));
#36003=CARTESIAN_POINT('Ctrl Pts',(1.71250340687011,1.,-1.34549029589563));
#36004=CARTESIAN_POINT('Ctrl Pts',(1.70614212266676,-1.,-1.34459924533783));
#36005=CARTESIAN_POINT('Ctrl Pts',(1.70614212266676,1.,-1.34459924533783));
#36006=CARTESIAN_POINT('Ctrl Pts',(1.69979707754221,-1.,-1.34367237124322));
#36007=CARTESIAN_POINT('Ctrl Pts',(1.69979707754221,1.,-1.34367237124322));
#36008=CARTESIAN_POINT('Ctrl Pts',(1.6934684849664,-1.,-1.34270948206139));
#36009=CARTESIAN_POINT('Ctrl Pts',(1.6934684849664,1.,-1.34270948206139));
#36010=CARTESIAN_POINT('Ctrl Pts',(1.68715660868602,-1.,-1.34171037484673));
#36011=CARTESIAN_POINT('Ctrl Pts',(1.68715660868602,1.,-1.34171037484673));
#36012=CARTESIAN_POINT('Ctrl Pts',(1.68086176030308,-1.,-1.3406748518516));
#36013=CARTESIAN_POINT('Ctrl Pts',(1.68086176030308,1.,-1.3406748518516));
#36014=CARTESIAN_POINT('Ctrl Pts',(1.67458429426126,-1.,-1.33960273470372));
#36015=CARTESIAN_POINT('Ctrl Pts',(1.67458429426126,1.,-1.33960273470372));
#36016=CARTESIAN_POINT('Ctrl Pts',(1.66832460784078,-1.,-1.33849388654458));
#36017=CARTESIAN_POINT('Ctrl Pts',(1.66832460784078,1.,-1.33849388654458));
#36018=CARTESIAN_POINT('Ctrl Pts',(1.66208312542073,-1.,-1.33734820885331));
#36019=CARTESIAN_POINT('Ctrl Pts',(1.66208312542073,1.,-1.33734820885331));
#36020=CARTESIAN_POINT('Ctrl Pts',(1.65586025952651,-1.,-1.33616559745217));
#36021=CARTESIAN_POINT('Ctrl Pts',(1.65586025952651,1.,-1.33616559745217));
#36022=CARTESIAN_POINT('Ctrl Pts',(1.64965637286843,-1.,-1.33494590468003));
#36023=CARTESIAN_POINT('Ctrl Pts',(1.64965637286843,1.,-1.33494590468003));
#36024=CARTESIAN_POINT('Ctrl Pts',(1.64347174856007,-1.,-1.33368890676554));
#36025=CARTESIAN_POINT('Ctrl Pts',(1.64347174856007,1.,-1.33368890676554));
#36026=CARTESIAN_POINT('Ctrl Pts',(1.63730653475049,-1.,-1.33239425103694));
#36027=CARTESIAN_POINT('Ctrl Pts',(1.63730653475049,1.,-1.33239425103694));
#36028=CARTESIAN_POINT('Ctrl Pts',(1.63116079730887,-1.,-1.33106149345618));
#36029=CARTESIAN_POINT('Ctrl Pts',(1.63116079730887,1.,-1.33106149345618));
#36030=CARTESIAN_POINT('Ctrl Pts',(1.62503464209777,-1.,-1.32969019505665));
#36031=CARTESIAN_POINT('Ctrl Pts',(1.62503464209777,1.,-1.32969019505665));
#36032=CARTESIAN_POINT('Ctrl Pts',(1.61892832270723,-1.,-1.32828000610448));
#36033=CARTESIAN_POINT('Ctrl Pts',(1.61892832270723,1.,-1.32828000610448));
#36034=CARTESIAN_POINT('Ctrl Pts',(1.61284234015762,-1.,-1.32683074483365));
#36035=CARTESIAN_POINT('Ctrl Pts',(1.61284234015762,1.,-1.32683074483365));
#36036=CARTESIAN_POINT('Ctrl Pts',(1.6067775829097,-1.,-1.32534250785794));
#36037=CARTESIAN_POINT('Ctrl Pts',(1.6067775829097,1.,-1.32534250785794));
#36038=CARTESIAN_POINT('Ctrl Pts',(1.600735118587,-1.,-1.32381550858266));
#36039=CARTESIAN_POINT('Ctrl Pts',(1.600735118587,1.,-1.32381550858266));
#36040=CARTESIAN_POINT('Ctrl Pts',(1.59471591079408,-1.,-1.32224985747686));
#36041=CARTESIAN_POINT('Ctrl Pts',(1.59471591079408,1.,-1.32224985747686));
#36042=CARTESIAN_POINT('Ctrl Pts',(1.58872057258244,-1.,-1.32064537110891));
#36043=CARTESIAN_POINT('Ctrl Pts',(1.58872057258244,1.,-1.32064537110891));
#36044=CARTESIAN_POINT('Ctrl Pts',(1.58274907898829,-1.,-1.31900135021428));
#36045=CARTESIAN_POINT('Ctrl Pts',(1.58274907898829,1.,-1.31900135021428));
#36046=CARTESIAN_POINT('Ctrl Pts',(1.57680056505585,-1.,-1.31731642317183));
#36047=CARTESIAN_POINT('Ctrl Pts',(1.57680056505585,1.,-1.31731642317183));
#36048=CARTESIAN_POINT('Ctrl Pts',(1.57087397835721,-1.,-1.31558903860015));
#36049=CARTESIAN_POINT('Ctrl Pts',(1.57087397835721,1.,-1.31558903860015));
#36050=CARTESIAN_POINT('Ctrl Pts',(1.56496872402352,-1.,-1.31381795281002));
#36051=CARTESIAN_POINT('Ctrl Pts',(1.56496872402352,1.,-1.31381795281002));
#36052=CARTESIAN_POINT('Ctrl Pts',(1.55908521254822,-1.,-1.31200264341696));
#36053=CARTESIAN_POINT('Ctrl Pts',(1.55908521254822,1.,-1.31200264341696));
#36054=CARTESIAN_POINT('Ctrl Pts',(1.55322568759481,-1.,-1.31014393684221));
#36055=CARTESIAN_POINT('Ctrl Pts',(1.55322568759481,1.,-1.31014393684221));
#36056=CARTESIAN_POINT('Ctrl Pts',(1.54739413957183,-1.,-1.30824393907471));
#36057=CARTESIAN_POINT('Ctrl Pts',(1.54739413957183,1.,-1.30824393907471));
#36058=CARTESIAN_POINT('Ctrl Pts',(1.54159462645428,-1.,-1.30630475189553));
#36059=CARTESIAN_POINT('Ctrl Pts',(1.54159462645428,1.,-1.30630475189553));
#36060=CARTESIAN_POINT('Ctrl Pts',(1.53582981268976,-1.,-1.30432735639487));
#36061=CARTESIAN_POINT('Ctrl Pts',(1.53582981268976,1.,-1.30432735639487));
#36062=CARTESIAN_POINT('Ctrl Pts',(1.53009970283893,-1.,-1.3023106439557));
#36063=CARTESIAN_POINT('Ctrl Pts',(1.53009970283893,1.,-1.3023106439557));
#36064=CARTESIAN_POINT('Ctrl Pts',(1.5243995786107,-1.,-1.30024984366334));
#36065=CARTESIAN_POINT('Ctrl Pts',(1.5243995786107,1.,-1.30024984366334));
#36066=CARTESIAN_POINT('Ctrl Pts',(1.51872184912735,-1.,-1.29813791800757));
#36067=CARTESIAN_POINT('Ctrl Pts',(1.51872184912735,1.,-1.29813791800757));
#36068=CARTESIAN_POINT('Ctrl Pts',(1.51305994241412,-1.,-1.29596850710518));
#36069=CARTESIAN_POINT('Ctrl Pts',(1.51305994241412,1.,-1.29596850710518));
#36070=CARTESIAN_POINT('Ctrl Pts',(1.50741159078367,-1.,-1.29373841372843));
#36071=CARTESIAN_POINT('Ctrl Pts',(1.50741159078367,1.,-1.29373841372843));
#36072=CARTESIAN_POINT('Ctrl Pts',(1.50178230149764,-1.,-1.29145022885171));
#36073=CARTESIAN_POINT('Ctrl Pts',(1.50178230149764,1.,-1.29145022885171));
#36074=CARTESIAN_POINT('Ctrl Pts',(1.49618896881729,-1.,-1.28911506584232));
#36075=CARTESIAN_POINT('Ctrl Pts',(1.49618896881729,1.,-1.28911506584232));
#36076=CARTESIAN_POINT('Ctrl Pts',(1.4906522831275,-1.,-1.28674676116415));
#36077=CARTESIAN_POINT('Ctrl Pts',(1.4906522831275,1.,-1.28674676116415));
#36078=CARTESIAN_POINT('Ctrl Pts',(1.48518817118891,-1.,-1.28435533880184));
#36079=CARTESIAN_POINT('Ctrl Pts',(1.48518817118891,1.,-1.28435533880184));
#36080=CARTESIAN_POINT('Ctrl Pts',(1.47980070347102,-1.,-1.28194158939522));
#36081=CARTESIAN_POINT('Ctrl Pts',(1.47980070347102,1.,-1.28194158939522));
#36082=CARTESIAN_POINT('Ctrl Pts',(1.4744717526711,-1.,-1.27948918248524));
#36083=CARTESIAN_POINT('Ctrl Pts',(1.4744717526711,1.,-1.27948918248524));
#36084=CARTESIAN_POINT('Ctrl Pts',(1.46916035917197,-1.,-1.27696414831144));
#36085=CARTESIAN_POINT('Ctrl Pts',(1.46916035917197,1.,-1.27696414831144));
#36086=CARTESIAN_POINT('Ctrl Pts',(1.4638243133254,-1.,-1.27433119897877));
#36087=CARTESIAN_POINT('Ctrl Pts',(1.4638243133254,1.,-1.27433119897877));
#36088=CARTESIAN_POINT('Ctrl Pts',(1.45843906294725,-1.,-1.27156805265312));
#36089=CARTESIAN_POINT('Ctrl Pts',(1.45843906294725,1.,-1.27156805265312));
#36090=CARTESIAN_POINT('Ctrl Pts',(1.45301422764205,-1.,-1.26867786804854));
#36091=CARTESIAN_POINT('Ctrl Pts',(1.45301422764205,1.,-1.26867786804854));
#36092=CARTESIAN_POINT('Ctrl Pts',(1.44761985001544,-1.,-1.26570925118767));
#36093=CARTESIAN_POINT('Ctrl Pts',(1.44761985001544,1.,-1.26570925118767));
#36094=CARTESIAN_POINT('Ctrl Pts',(1.44236470511145,-1.,-1.26273903323723));
#36095=CARTESIAN_POINT('Ctrl Pts',(1.44236470511145,1.,-1.26273903323723));
#36096=CARTESIAN_POINT('Ctrl Pts',(1.43734919180719,-1.,-1.25983531011894));
#36097=CARTESIAN_POINT('Ctrl Pts',(1.43734919180719,1.,-1.25983531011894));
#36098=CARTESIAN_POINT('Ctrl Pts',(1.43262645609679,-1.,-1.25702687965744));
#36099=CARTESIAN_POINT('Ctrl Pts',(1.43262645609679,1.,-1.25702687965744));
#36100=CARTESIAN_POINT('Ctrl Pts',(1.42815938799555,-1.,-1.25426945222783));
#36101=CARTESIAN_POINT('Ctrl Pts',(1.42815938799555,1.,-1.25426945222783));
#36102=CARTESIAN_POINT('Ctrl Pts',(1.42378102115911,-1.,-1.25141455570299));
#36103=CARTESIAN_POINT('Ctrl Pts',(1.42378102115911,1.,-1.25141455570299));
#36104=CARTESIAN_POINT('Ctrl Pts',(1.41923722596421,-1.,-1.24824430986911));
#36105=CARTESIAN_POINT('Ctrl Pts',(1.41923722596421,1.,-1.24824430986911));
#36106=CARTESIAN_POINT('Ctrl Pts',(1.41422913175437,-1.,-1.24450600513278));
#36107=CARTESIAN_POINT('Ctrl Pts',(1.41422913175437,1.,-1.24450600513278));
#36108=CARTESIAN_POINT('Ctrl Pts',(1.40845295531151,-1.,-1.23994455029421));
#36109=CARTESIAN_POINT('Ctrl Pts',(1.40845295531151,1.,-1.23994455029421));
#36110=CARTESIAN_POINT('Ctrl Pts',(1.40164708205345,-1.,-1.23434087289768));
#36111=CARTESIAN_POINT('Ctrl Pts',(1.40164708205345,1.,-1.23434087289768));
#36112=CARTESIAN_POINT('Ctrl Pts',(1.39361389567257,-1.,-1.22752961898063));
#36113=CARTESIAN_POINT('Ctrl Pts',(1.39361389567257,1.,-1.22752961898063));
#36114=CARTESIAN_POINT('Ctrl Pts',(1.38420564525391,-1.,-1.21938737278853));
#36115=CARTESIAN_POINT('Ctrl Pts',(1.38420564525391,1.,-1.21938737278853));
#36116=CARTESIAN_POINT('Ctrl Pts',(1.37331915604962,-1.,-1.20982812923113));
#36117=CARTESIAN_POINT('Ctrl Pts',(1.37331915604962,1.,-1.20982812923113));
#36118=CARTESIAN_POINT('Ctrl Pts',(1.36088705040677,-1.,-1.1987959077656));
#36119=CARTESIAN_POINT('Ctrl Pts',(1.36088705040677,1.,-1.1987959077656));
#36120=CARTESIAN_POINT('Ctrl Pts',(1.34687053998157,-1.,-1.18625865664915));
#36121=CARTESIAN_POINT('Ctrl Pts',(1.34687053998157,1.,-1.18625865664915));
#36122=CARTESIAN_POINT('Ctrl Pts',(1.33437539344842,-1.,-1.17501305787994));
#36123=CARTESIAN_POINT('Ctrl Pts',(1.33437539344842,1.,-1.17501305787994));
#36124=CARTESIAN_POINT('Ctrl Pts',(1.32428080720544,-1.,-1.16589330092532));
#36125=CARTESIAN_POINT('Ctrl Pts',(1.32428080720544,1.,-1.16589330092532));
#36126=CARTESIAN_POINT('Ctrl Pts',(1.3172297721596,-1.,-1.15950888730433));
#36127=CARTESIAN_POINT('Ctrl Pts',(1.3172297721596,1.,-1.15950888730433));
#36128=CARTESIAN_POINT('Ctrl Pts',(1.31362392696032,-1.,-1.15624053661742));
#36129=CARTESIAN_POINT('Ctrl Pts',(1.31362392696032,1.,-1.15624053661742));
#36130=CARTESIAN_POINT('',(1.73811241238545,1.,-1.34869019493419));
#36131=CARTESIAN_POINT('Ctrl Pts',(1.73811241238545,1.,-1.34869019493419));
#36132=CARTESIAN_POINT('Ctrl Pts',(1.73682580585819,1.,-1.34854391898145));
#36133=CARTESIAN_POINT('Ctrl Pts',(1.73425417886254,1.,-1.34824783113158));
#36134=CARTESIAN_POINT('Ctrl Pts',(1.73040149654497,1.,-1.3477930915247));
#36135=CARTESIAN_POINT('Ctrl Pts',(1.72527410681298,1.,-1.34716554820013));
#36136=CARTESIAN_POINT('Ctrl Pts',(1.7188807715095,1.,-1.34634568653586));
#36137=CARTESIAN_POINT('Ctrl Pts',(1.71250340687011,1.,-1.34549029589563));
#36138=CARTESIAN_POINT('Ctrl Pts',(1.70614212266676,1.,-1.34459924533783));
#36139=CARTESIAN_POINT('Ctrl Pts',(1.69979707754221,1.,-1.34367237124322));
#36140=CARTESIAN_POINT('Ctrl Pts',(1.6934684849664,1.,-1.34270948206139));
#36141=CARTESIAN_POINT('Ctrl Pts',(1.68715660868602,1.,-1.34171037484673));
#36142=CARTESIAN_POINT('Ctrl Pts',(1.68086176030308,1.,-1.3406748518516));
#36143=CARTESIAN_POINT('Ctrl Pts',(1.67458429426126,1.,-1.33960273470372));
#36144=CARTESIAN_POINT('Ctrl Pts',(1.66832460784078,1.,-1.33849388654458));
#36145=CARTESIAN_POINT('Ctrl Pts',(1.66208312542073,1.,-1.33734820885331));
#36146=CARTESIAN_POINT('Ctrl Pts',(1.65586025952651,1.,-1.33616559745217));
#36147=CARTESIAN_POINT('Ctrl Pts',(1.64965637286843,1.,-1.33494590468003));
#36148=CARTESIAN_POINT('Ctrl Pts',(1.64347174856007,1.,-1.33368890676554));
#36149=CARTESIAN_POINT('Ctrl Pts',(1.63730653475049,1.,-1.33239425103694));
#36150=CARTESIAN_POINT('Ctrl Pts',(1.63116079730887,1.,-1.33106149345618));
#36151=CARTESIAN_POINT('Ctrl Pts',(1.62503464209777,1.,-1.32969019505665));
#36152=CARTESIAN_POINT('Ctrl Pts',(1.61892832270723,1.,-1.32828000610448));
#36153=CARTESIAN_POINT('Ctrl Pts',(1.61284234015762,1.,-1.32683074483365));
#36154=CARTESIAN_POINT('Ctrl Pts',(1.6067775829097,1.,-1.32534250785794));
#36155=CARTESIAN_POINT('Ctrl Pts',(1.600735118587,1.,-1.32381550858266));
#36156=CARTESIAN_POINT('Ctrl Pts',(1.59471591079408,1.,-1.32224985747686));
#36157=CARTESIAN_POINT('Ctrl Pts',(1.58872057258244,1.,-1.32064537110891));
#36158=CARTESIAN_POINT('Ctrl Pts',(1.58274907898829,1.,-1.31900135021428));
#36159=CARTESIAN_POINT('Ctrl Pts',(1.57680056505585,1.,-1.31731642317183));
#36160=CARTESIAN_POINT('Ctrl Pts',(1.57087397835721,1.,-1.31558903860015));
#36161=CARTESIAN_POINT('Ctrl Pts',(1.56496872402352,1.,-1.31381795281002));
#36162=CARTESIAN_POINT('Ctrl Pts',(1.55908521254822,1.,-1.31200264341696));
#36163=CARTESIAN_POINT('Ctrl Pts',(1.55322568759481,1.,-1.31014393684221));
#36164=CARTESIAN_POINT('Ctrl Pts',(1.54739413957183,1.,-1.30824393907471));
#36165=CARTESIAN_POINT('Ctrl Pts',(1.54159462645428,1.,-1.30630475189553));
#36166=CARTESIAN_POINT('Ctrl Pts',(1.53582981268976,1.,-1.30432735639487));
#36167=CARTESIAN_POINT('Ctrl Pts',(1.53009970283893,1.,-1.3023106439557));
#36168=CARTESIAN_POINT('Ctrl Pts',(1.5243995786107,1.,-1.30024984366334));
#36169=CARTESIAN_POINT('Ctrl Pts',(1.51872184912735,1.,-1.29813791800757));
#36170=CARTESIAN_POINT('Ctrl Pts',(1.51305994241412,1.,-1.29596850710518));
#36171=CARTESIAN_POINT('Ctrl Pts',(1.50741159078367,1.,-1.29373841372843));
#36172=CARTESIAN_POINT('Ctrl Pts',(1.50178230149764,1.,-1.29145022885171));
#36173=CARTESIAN_POINT('Ctrl Pts',(1.49618896881729,1.,-1.28911506584232));
#36174=CARTESIAN_POINT('Ctrl Pts',(1.4906522831275,1.,-1.28674676116415));
#36175=CARTESIAN_POINT('Ctrl Pts',(1.48518817118891,1.,-1.28435533880184));
#36176=CARTESIAN_POINT('Ctrl Pts',(1.47980070347102,1.,-1.28194158939522));
#36177=CARTESIAN_POINT('Ctrl Pts',(1.4744717526711,1.,-1.27948918248524));
#36178=CARTESIAN_POINT('Ctrl Pts',(1.46916035917197,1.,-1.27696414831144));
#36179=CARTESIAN_POINT('Ctrl Pts',(1.4638243133254,1.,-1.27433119897877));
#36180=CARTESIAN_POINT('Ctrl Pts',(1.45843906294725,1.,-1.27156805265312));
#36181=CARTESIAN_POINT('Ctrl Pts',(1.45301422764205,1.,-1.26867786804854));
#36182=CARTESIAN_POINT('Ctrl Pts',(1.44761985001544,1.,-1.26570925118767));
#36183=CARTESIAN_POINT('Ctrl Pts',(1.44236470511145,1.,-1.26273903323723));
#36184=CARTESIAN_POINT('Ctrl Pts',(1.43734919180719,1.,-1.25983531011894));
#36185=CARTESIAN_POINT('Ctrl Pts',(1.43262645609679,1.,-1.25702687965744));
#36186=CARTESIAN_POINT('Ctrl Pts',(1.42815938799555,1.,-1.25426945222783));
#36187=CARTESIAN_POINT('Ctrl Pts',(1.42378102115911,1.,-1.25141455570299));
#36188=CARTESIAN_POINT('Ctrl Pts',(1.41923722596421,1.,-1.24824430986911));
#36189=CARTESIAN_POINT('Ctrl Pts',(1.41422913175437,1.,-1.24450600513278));
#36190=CARTESIAN_POINT('Ctrl Pts',(1.40845295531151,1.,-1.23994455029421));
#36191=CARTESIAN_POINT('Ctrl Pts',(1.40164708205345,1.,-1.23434087289768));
#36192=CARTESIAN_POINT('Ctrl Pts',(1.39361389567257,1.,-1.22752961898063));
#36193=CARTESIAN_POINT('Ctrl Pts',(1.38420564525391,1.,-1.21938737278853));
#36194=CARTESIAN_POINT('Ctrl Pts',(1.37331915604962,1.,-1.20982812923113));
#36195=CARTESIAN_POINT('Ctrl Pts',(1.36088705040677,1.,-1.1987959077656));
#36196=CARTESIAN_POINT('Ctrl Pts',(1.34687053998157,1.,-1.18625865664915));
#36197=CARTESIAN_POINT('Ctrl Pts',(1.33437539344842,1.,-1.17501305787994));
#36198=CARTESIAN_POINT('Ctrl Pts',(1.32428080720544,1.,-1.16589330092532));
#36199=CARTESIAN_POINT('Ctrl Pts',(1.3172297721596,1.,-1.15950888730433));
#36200=CARTESIAN_POINT('Ctrl Pts',(1.31362392696032,1.,-1.15624053661742));
#36201=CARTESIAN_POINT('',(1.73811241238545,0.,-1.34869019493419));
#36202=CARTESIAN_POINT('Origin',(1.81978687191668,0.,-1.23627494547115));
#36203=CARTESIAN_POINT('',(1.81978687191668,1.,-1.23627494547115));
#36204=CARTESIAN_POINT('',(1.73811241238545,1.,-1.34869019493419));
#36205=CARTESIAN_POINT('',(1.81978687191668,0.,-1.23627494547115));
#36206=CARTESIAN_POINT('Ctrl Pts',(1.5055822144029,-1.,-0.892032620296855));
#36207=CARTESIAN_POINT('Ctrl Pts',(1.5055822144029,1.,-0.892032620296855));
#36208=CARTESIAN_POINT('Ctrl Pts',(1.50980486807181,-1.,-0.894452006967538));
#36209=CARTESIAN_POINT('Ctrl Pts',(1.50980486807181,1.,-0.894452006967538));
#36210=CARTESIAN_POINT('Ctrl Pts',(1.51805569591479,-1.,-0.89918504749193));
#36211=CARTESIAN_POINT('Ctrl Pts',(1.51805569591479,1.,-0.89918504749193));
#36212=CARTESIAN_POINT('Ctrl Pts',(1.52984849890434,-1.,-0.905967409640499));
#36213=CARTESIAN_POINT('Ctrl Pts',(1.52984849890434,1.,-0.905967409640499));
#36214=CARTESIAN_POINT('Ctrl Pts',(1.54440491152807,-1.,-0.91437591904658));
#36215=CARTESIAN_POINT('Ctrl Pts',(1.54440491152807,1.,-0.91437591904658));
#36216=CARTESIAN_POINT('Ctrl Pts',(1.56065988582509,-1.,-0.923832188966322));
#36217=CARTESIAN_POINT('Ctrl Pts',(1.56065988582509,1.,-0.923832188966322));
#36218=CARTESIAN_POINT('Ctrl Pts',(1.57499388385561,-1.,-0.932246680128849));
#36219=CARTESIAN_POINT('Ctrl Pts',(1.57499388385561,1.,-0.932246680128849));
#36220=CARTESIAN_POINT('Ctrl Pts',(1.58744937489796,-1.,-0.939646377909319));
#36221=CARTESIAN_POINT('Ctrl Pts',(1.58744937489796,1.,-0.939646377909319));
#36222=CARTESIAN_POINT('Ctrl Pts',(1.59810042045408,-1.,-0.946078063325796));
#36223=CARTESIAN_POINT('Ctrl Pts',(1.59810042045408,1.,-0.946078063325796));
#36224=CARTESIAN_POINT('Ctrl Pts',(1.60706069897794,-1.,-0.951613284361248));
#36225=CARTESIAN_POINT('Ctrl Pts',(1.60706069897794,1.,-0.951613284361248));
#36226=CARTESIAN_POINT('Ctrl Pts',(1.61449324337233,-1.,-0.956354422921573));
#36227=CARTESIAN_POINT('Ctrl Pts',(1.61449324337233,1.,-0.956354422921573));
#36228=CARTESIAN_POINT('Ctrl Pts',(1.62061638139929,-1.,-0.960438326099958));
#36229=CARTESIAN_POINT('Ctrl Pts',(1.62061638139929,1.,-0.960438326099958));
#36230=CARTESIAN_POINT('Ctrl Pts',(1.6257193066974,-1.,-0.964046107037821));
#36231=CARTESIAN_POINT('Ctrl Pts',(1.6257193066974,1.,-0.964046107037821));
#36232=CARTESIAN_POINT('Ctrl Pts',(1.63013849959083,-1.,-0.967387853228041));
#36233=CARTESIAN_POINT('Ctrl Pts',(1.63013849959083,1.,-0.967387853228041));
#36234=CARTESIAN_POINT('Ctrl Pts',(1.63420665729609,-1.,-0.970669715996356));
#36235=CARTESIAN_POINT('Ctrl Pts',(1.63420665729609,1.,-0.970669715996356));
#36236=CARTESIAN_POINT('Ctrl Pts',(1.63820952658157,-1.,-0.974066058287501));
#36237=CARTESIAN_POINT('Ctrl Pts',(1.63820952658157,1.,-0.974066058287501));
#36238=CARTESIAN_POINT('Ctrl Pts',(1.64233990826831,-1.,-0.977689794120297));
#36239=CARTESIAN_POINT('Ctrl Pts',(1.64233990826831,1.,-0.977689794120297));
#36240=CARTESIAN_POINT('Ctrl Pts',(1.64665139190834,-1.,-0.981562530940574));
#36241=CARTESIAN_POINT('Ctrl Pts',(1.64665139190834,1.,-0.981562530940574));
#36242=CARTESIAN_POINT('Ctrl Pts',(1.6511001661277,-1.,-0.985642622921626));
#36243=CARTESIAN_POINT('Ctrl Pts',(1.6511001661277,1.,-0.985642622921626));
#36244=CARTESIAN_POINT('Ctrl Pts',(1.65559044289746,-1.,-0.98985562785445));
#36245=CARTESIAN_POINT('Ctrl Pts',(1.65559044289746,1.,-0.98985562785445));
#36246=CARTESIAN_POINT('Ctrl Pts',(1.66001553809916,-1.,-0.994121836661116));
#36247=CARTESIAN_POINT('Ctrl Pts',(1.66001553809916,1.,-0.994121836661116));
#36248=CARTESIAN_POINT('Ctrl Pts',(1.66430758030304,-1.,-0.998389654952317));
#36249=CARTESIAN_POINT('Ctrl Pts',(1.66430758030304,1.,-0.998389654952317));
#36250=CARTESIAN_POINT('Ctrl Pts',(1.66846059277231,-1.,-1.00265091003682));
#36251=CARTESIAN_POINT('Ctrl Pts',(1.66846059277231,1.,-1.00265091003682));
#36252=CARTESIAN_POINT('Ctrl Pts',(1.67250335383248,-1.,-1.00692206696387));
#36253=CARTESIAN_POINT('Ctrl Pts',(1.67250335383248,1.,-1.00692206696387));
#36254=CARTESIAN_POINT('Ctrl Pts',(1.67648246776457,-1.,-1.01123236493507));
#36255=CARTESIAN_POINT('Ctrl Pts',(1.67648246776457,1.,-1.01123236493507));
#36256=CARTESIAN_POINT('Ctrl Pts',(1.6804428989482,-1.,-1.01561026162787));
#36257=CARTESIAN_POINT('Ctrl Pts',(1.6804428989482,1.,-1.01561026162787));
#36258=CARTESIAN_POINT('Ctrl Pts',(1.68440578021739,-1.,-1.02006795074222));
#36259=CARTESIAN_POINT('Ctrl Pts',(1.68440578021739,1.,-1.02006795074222));
#36260=CARTESIAN_POINT('Ctrl Pts',(1.68836910178475,-1.,-1.02460180535272));
#36261=CARTESIAN_POINT('Ctrl Pts',(1.68836910178475,1.,-1.02460180535272));
#36262=CARTESIAN_POINT('Ctrl Pts',(1.69231840863471,-1.,-1.02919977579155));
#36263=CARTESIAN_POINT('Ctrl Pts',(1.69231840863471,1.,-1.02919977579155));
#36264=CARTESIAN_POINT('Ctrl Pts',(1.69623414782769,-1.,-1.03384646003587));
#36265=CARTESIAN_POINT('Ctrl Pts',(1.69623414782769,1.,-1.03384646003587));
#36266=CARTESIAN_POINT('Ctrl Pts',(1.70010052930951,-1.,-1.03852922490782));
#36267=CARTESIAN_POINT('Ctrl Pts',(1.70010052930951,1.,-1.03852922490782));
#36268=CARTESIAN_POINT('Ctrl Pts',(1.70391338707969,-1.,-1.04324363334546));
#36269=CARTESIAN_POINT('Ctrl Pts',(1.70391338707969,1.,-1.04324363334546));
#36270=CARTESIAN_POINT('Ctrl Pts',(1.70767646263641,-1.,-1.0479908540499));
#36271=CARTESIAN_POINT('Ctrl Pts',(1.70767646263641,1.,-1.0479908540499));
#36272=CARTESIAN_POINT('Ctrl Pts',(1.71139783543986,-1.,-1.05277517202854));
#36273=CARTESIAN_POINT('Ctrl Pts',(1.71139783543986,1.,-1.05277517202854));
#36274=CARTESIAN_POINT('Ctrl Pts',(1.71508654427022,-1.,-1.05760163192481));
#36275=CARTESIAN_POINT('Ctrl Pts',(1.71508654427022,1.,-1.05760163192481));
#36276=CARTESIAN_POINT('Ctrl Pts',(1.71874858456908,-1.,-1.0624732468065));
#36277=CARTESIAN_POINT('Ctrl Pts',(1.71874858456908,1.,-1.0624732468065));
#36278=CARTESIAN_POINT('Ctrl Pts',(1.72238500928456,-1.,-1.06738966975463));
#36279=CARTESIAN_POINT('Ctrl Pts',(1.72238500928456,1.,-1.06738966975463));
#36280=CARTESIAN_POINT('Ctrl Pts',(1.72599406198489,-1.,-1.07234866990252));
#36281=CARTESIAN_POINT('Ctrl Pts',(1.72599406198489,1.,-1.07234866990252));
#36282=CARTESIAN_POINT('Ctrl Pts',(1.72957248977424,-1.,-1.0773470373727));
#36283=CARTESIAN_POINT('Ctrl Pts',(1.72957248977424,1.,-1.0773470373727));
#36284=CARTESIAN_POINT('Ctrl Pts',(1.73311705663407,-1.,-1.08238162784749));
#36285=CARTESIAN_POINT('Ctrl Pts',(1.73311705663407,1.,-1.08238162784749));
#36286=CARTESIAN_POINT('Ctrl Pts',(1.73662628326093,-1.,-1.08745056285429));
#36287=CARTESIAN_POINT('Ctrl Pts',(1.73662628326093,1.,-1.08745056285429));
#36288=CARTESIAN_POINT('Ctrl Pts',(1.74010053962252,-1.,-1.09255329056496));
#36289=CARTESIAN_POINT('Ctrl Pts',(1.74010053962252,1.,-1.09255329056496));
#36290=CARTESIAN_POINT('Ctrl Pts',(1.74354119236212,-1.,-1.09768999241229));
#36291=CARTESIAN_POINT('Ctrl Pts',(1.74354119236212,1.,-1.09768999241229));
#36292=CARTESIAN_POINT('Ctrl Pts',(1.74695004214924,-1.,-1.10286118991144));
#36293=CARTESIAN_POINT('Ctrl Pts',(1.74695004214924,1.,-1.10286118991144));
#36294=CARTESIAN_POINT('Ctrl Pts',(1.75032866075914,-1.,-1.10806728183003));
#36295=CARTESIAN_POINT('Ctrl Pts',(1.75032866075914,1.,-1.10806728183003));
#36296=CARTESIAN_POINT('Ctrl Pts',(1.75367772094617,-1.,-1.11330807582542));
#36297=CARTESIAN_POINT('Ctrl Pts',(1.75367772094617,1.,-1.11330807582542));
#36298=CARTESIAN_POINT('Ctrl Pts',(1.75699720772089,-1.,-1.11858293216752));
#36299=CARTESIAN_POINT('Ctrl Pts',(1.75699720772089,1.,-1.11858293216752));
#36300=CARTESIAN_POINT('Ctrl Pts',(1.76028671825084,-1.,-1.12389096855078));
#36301=CARTESIAN_POINT('Ctrl Pts',(1.76028671825084,1.,-1.12389096855078));
#36302=CARTESIAN_POINT('Ctrl Pts',(1.76354571966171,-1.,-1.12923123555076));
#36303=CARTESIAN_POINT('Ctrl Pts',(1.76354571966171,1.,-1.12923123555076));
#36304=CARTESIAN_POINT('Ctrl Pts',(1.76677384551883,-1.,-1.13460291804635));
#36305=CARTESIAN_POINT('Ctrl Pts',(1.76677384551883,1.,-1.13460291804635));
#36306=CARTESIAN_POINT('Ctrl Pts',(1.76997111386806,-1.,-1.14000548337));
#36307=CARTESIAN_POINT('Ctrl Pts',(1.76997111386806,1.,-1.14000548337));
#36308=CARTESIAN_POINT('Ctrl Pts',(1.77313777896234,-1.,-1.14543858226948));
#36309=CARTESIAN_POINT('Ctrl Pts',(1.77313777896234,1.,-1.14543858226948));
#36310=CARTESIAN_POINT('Ctrl Pts',(1.77627422557034,-1.,-1.15090197841531));
#36311=CARTESIAN_POINT('Ctrl Pts',(1.77627422557034,1.,-1.15090197841531));
#36312=CARTESIAN_POINT('Ctrl Pts',(1.77938085564261,-1.,-1.15639547194689));
#36313=CARTESIAN_POINT('Ctrl Pts',(1.77938085564261,1.,-1.15639547194689));
#36314=CARTESIAN_POINT('Ctrl Pts',(1.78245795880949,-1.,-1.16191881298458));
#36315=CARTESIAN_POINT('Ctrl Pts',(1.78245795880949,1.,-1.16191881298458));
#36316=CARTESIAN_POINT('Ctrl Pts',(1.78550566040349,-1.,-1.16747166312239));
#36317=CARTESIAN_POINT('Ctrl Pts',(1.78550566040349,1.,-1.16747166312239));
#36318=CARTESIAN_POINT('Ctrl Pts',(1.78852398877523,-1.,-1.17305363177265));
#36319=CARTESIAN_POINT('Ctrl Pts',(1.78852398877523,1.,-1.17305363177265));
#36320=CARTESIAN_POINT('Ctrl Pts',(1.79151291552646,-1.,-1.17866429440781));
#36321=CARTESIAN_POINT('Ctrl Pts',(1.79151291552646,1.,-1.17866429440781));
#36322=CARTESIAN_POINT('Ctrl Pts',(1.79447240321572,-1.,-1.18430321697471));
#36323=CARTESIAN_POINT('Ctrl Pts',(1.79447240321572,1.,-1.18430321697471));
#36324=CARTESIAN_POINT('Ctrl Pts',(1.79740245923649,-1.,-1.1899699793456));
#36325=CARTESIAN_POINT('Ctrl Pts',(1.79740245923649,1.,-1.1899699793456));
#36326=CARTESIAN_POINT('Ctrl Pts',(1.80030314370121,-1.,-1.19566418930405));
#36327=CARTESIAN_POINT('Ctrl Pts',(1.80030314370121,1.,-1.19566418930405));
#36328=CARTESIAN_POINT('Ctrl Pts',(1.8031745483882,-1.,-1.2013854893912));
#36329=CARTESIAN_POINT('Ctrl Pts',(1.8031745483882,1.,-1.2013854893912));
#36330=CARTESIAN_POINT('Ctrl Pts',(1.80601678480772,-1.,-1.20713356605519));
#36331=CARTESIAN_POINT('Ctrl Pts',(1.80601678480772,1.,-1.20713356605519));
#36332=CARTESIAN_POINT('Ctrl Pts',(1.80882996916931,-1.,-1.2129081570818));
#36333=CARTESIAN_POINT('Ctrl Pts',(1.80882996916931,1.,-1.2129081570818));
#36334=CARTESIAN_POINT('Ctrl Pts',(1.81161420806172,-1.,-1.2187090610323));
#36335=CARTESIAN_POINT('Ctrl Pts',(1.81161420806172,1.,-1.2187090610323));
#36336=CARTESIAN_POINT('Ctrl Pts',(1.81436959209778,-1.,-1.22453613304507));
#36337=CARTESIAN_POINT('Ctrl Pts',(1.81436959209778,1.,-1.22453613304507));
#36338=CARTESIAN_POINT('Ctrl Pts',(1.81655087183054,-1.,-1.22921864890975));
#36339=CARTESIAN_POINT('Ctrl Pts',(1.81655087183054,1.,-1.22921864890975));
#36340=CARTESIAN_POINT('Ctrl Pts',(1.81817389920914,-1.,-1.23274224526804));
#36341=CARTESIAN_POINT('Ctrl Pts',(1.81817389920914,1.,-1.23274224526804));
#36342=CARTESIAN_POINT('Ctrl Pts',(1.81925017193531,-1.,-1.23509651170384));
#36343=CARTESIAN_POINT('Ctrl Pts',(1.81925017193531,1.,-1.23509651170384));
#36344=CARTESIAN_POINT('Ctrl Pts',(1.81978687191668,-1.,-1.23627494547115));
#36345=CARTESIAN_POINT('Ctrl Pts',(1.81978687191668,1.,-1.23627494547115));
#36346=CARTESIAN_POINT('',(1.5055822144029,1.,-0.892032620296855));
#36347=CARTESIAN_POINT('Ctrl Pts',(1.5055822144029,1.,-0.892032620296855));
#36348=CARTESIAN_POINT('Ctrl Pts',(1.50980486807181,1.,-0.894452006967538));
#36349=CARTESIAN_POINT('Ctrl Pts',(1.51805569591479,1.,-0.89918504749193));
#36350=CARTESIAN_POINT('Ctrl Pts',(1.52984849890434,1.,-0.905967409640499));
#36351=CARTESIAN_POINT('Ctrl Pts',(1.54440491152807,1.,-0.91437591904658));
#36352=CARTESIAN_POINT('Ctrl Pts',(1.56065988582509,1.,-0.923832188966322));
#36353=CARTESIAN_POINT('Ctrl Pts',(1.57499388385561,1.,-0.932246680128849));
#36354=CARTESIAN_POINT('Ctrl Pts',(1.58744937489796,1.,-0.939646377909319));
#36355=CARTESIAN_POINT('Ctrl Pts',(1.59810042045408,1.,-0.946078063325796));
#36356=CARTESIAN_POINT('Ctrl Pts',(1.60706069897794,1.,-0.951613284361248));
#36357=CARTESIAN_POINT('Ctrl Pts',(1.61449324337233,1.,-0.956354422921573));
#36358=CARTESIAN_POINT('Ctrl Pts',(1.62061638139929,1.,-0.960438326099958));
#36359=CARTESIAN_POINT('Ctrl Pts',(1.6257193066974,1.,-0.964046107037821));
#36360=CARTESIAN_POINT('Ctrl Pts',(1.63013849959083,1.,-0.967387853228041));
#36361=CARTESIAN_POINT('Ctrl Pts',(1.63420665729609,1.,-0.970669715996356));
#36362=CARTESIAN_POINT('Ctrl Pts',(1.63820952658157,1.,-0.974066058287501));
#36363=CARTESIAN_POINT('Ctrl Pts',(1.64233990826831,1.,-0.977689794120297));
#36364=CARTESIAN_POINT('Ctrl Pts',(1.64665139190834,1.,-0.981562530940574));
#36365=CARTESIAN_POINT('Ctrl Pts',(1.6511001661277,1.,-0.985642622921626));
#36366=CARTESIAN_POINT('Ctrl Pts',(1.65559044289746,1.,-0.98985562785445));
#36367=CARTESIAN_POINT('Ctrl Pts',(1.66001553809916,1.,-0.994121836661116));
#36368=CARTESIAN_POINT('Ctrl Pts',(1.66430758030304,1.,-0.998389654952317));
#36369=CARTESIAN_POINT('Ctrl Pts',(1.66846059277231,1.,-1.00265091003682));
#36370=CARTESIAN_POINT('Ctrl Pts',(1.67250335383248,1.,-1.00692206696387));
#36371=CARTESIAN_POINT('Ctrl Pts',(1.67648246776457,1.,-1.01123236493507));
#36372=CARTESIAN_POINT('Ctrl Pts',(1.6804428989482,1.,-1.01561026162787));
#36373=CARTESIAN_POINT('Ctrl Pts',(1.68440578021739,1.,-1.02006795074222));
#36374=CARTESIAN_POINT('Ctrl Pts',(1.68836910178475,1.,-1.02460180535272));
#36375=CARTESIAN_POINT('Ctrl Pts',(1.69231840863471,1.,-1.02919977579155));
#36376=CARTESIAN_POINT('Ctrl Pts',(1.69623414782769,1.,-1.03384646003587));
#36377=CARTESIAN_POINT('Ctrl Pts',(1.70010052930951,1.,-1.03852922490782));
#36378=CARTESIAN_POINT('Ctrl Pts',(1.70391338707969,1.,-1.04324363334546));
#36379=CARTESIAN_POINT('Ctrl Pts',(1.70767646263641,1.,-1.0479908540499));
#36380=CARTESIAN_POINT('Ctrl Pts',(1.71139783543986,1.,-1.05277517202854));
#36381=CARTESIAN_POINT('Ctrl Pts',(1.71508654427022,1.,-1.05760163192481));
#36382=CARTESIAN_POINT('Ctrl Pts',(1.71874858456908,1.,-1.0624732468065));
#36383=CARTESIAN_POINT('Ctrl Pts',(1.72238500928456,1.,-1.06738966975463));
#36384=CARTESIAN_POINT('Ctrl Pts',(1.72599406198489,1.,-1.07234866990252));
#36385=CARTESIAN_POINT('Ctrl Pts',(1.72957248977424,1.,-1.0773470373727));
#36386=CARTESIAN_POINT('Ctrl Pts',(1.73311705663407,1.,-1.08238162784749));
#36387=CARTESIAN_POINT('Ctrl Pts',(1.73662628326093,1.,-1.08745056285429));
#36388=CARTESIAN_POINT('Ctrl Pts',(1.74010053962252,1.,-1.09255329056496));
#36389=CARTESIAN_POINT('Ctrl Pts',(1.74354119236212,1.,-1.09768999241229));
#36390=CARTESIAN_POINT('Ctrl Pts',(1.74695004214924,1.,-1.10286118991144));
#36391=CARTESIAN_POINT('Ctrl Pts',(1.75032866075914,1.,-1.10806728183003));
#36392=CARTESIAN_POINT('Ctrl Pts',(1.75367772094617,1.,-1.11330807582542));
#36393=CARTESIAN_POINT('Ctrl Pts',(1.75699720772089,1.,-1.11858293216752));
#36394=CARTESIAN_POINT('Ctrl Pts',(1.76028671825084,1.,-1.12389096855078));
#36395=CARTESIAN_POINT('Ctrl Pts',(1.76354571966171,1.,-1.12923123555076));
#36396=CARTESIAN_POINT('Ctrl Pts',(1.76677384551883,1.,-1.13460291804635));
#36397=CARTESIAN_POINT('Ctrl Pts',(1.76997111386806,1.,-1.14000548337));
#36398=CARTESIAN_POINT('Ctrl Pts',(1.77313777896234,1.,-1.14543858226948));
#36399=CARTESIAN_POINT('Ctrl Pts',(1.77627422557034,1.,-1.15090197841531));
#36400=CARTESIAN_POINT('Ctrl Pts',(1.77938085564261,1.,-1.15639547194689));
#36401=CARTESIAN_POINT('Ctrl Pts',(1.78245795880949,1.,-1.16191881298458));
#36402=CARTESIAN_POINT('Ctrl Pts',(1.78550566040349,1.,-1.16747166312239));
#36403=CARTESIAN_POINT('Ctrl Pts',(1.78852398877523,1.,-1.17305363177265));
#36404=CARTESIAN_POINT('Ctrl Pts',(1.79151291552646,1.,-1.17866429440781));
#36405=CARTESIAN_POINT('Ctrl Pts',(1.79447240321572,1.,-1.18430321697471));
#36406=CARTESIAN_POINT('Ctrl Pts',(1.79740245923649,1.,-1.1899699793456));
#36407=CARTESIAN_POINT('Ctrl Pts',(1.80030314370121,1.,-1.19566418930405));
#36408=CARTESIAN_POINT('Ctrl Pts',(1.8031745483882,1.,-1.2013854893912));
#36409=CARTESIAN_POINT('Ctrl Pts',(1.80601678480772,1.,-1.20713356605519));
#36410=CARTESIAN_POINT('Ctrl Pts',(1.80882996916931,1.,-1.2129081570818));
#36411=CARTESIAN_POINT('Ctrl Pts',(1.81161420806172,1.,-1.2187090610323));
#36412=CARTESIAN_POINT('Ctrl Pts',(1.81436959209778,1.,-1.22453613304507));
#36413=CARTESIAN_POINT('Ctrl Pts',(1.81655087183054,1.,-1.22921864890975));
#36414=CARTESIAN_POINT('Ctrl Pts',(1.81817389920914,1.,-1.23274224526804));
#36415=CARTESIAN_POINT('Ctrl Pts',(1.81925017193531,1.,-1.23509651170384));
#36416=CARTESIAN_POINT('Ctrl Pts',(1.81978687191668,1.,-1.23627494547115));
#36417=CARTESIAN_POINT('',(1.5055822144029,0.,-0.892032620296855));
#36418=CARTESIAN_POINT('Origin',(0.,0.,0.));
#36419=CARTESIAN_POINT('',(1.60662857109684,1.,-0.693717979106306));
#36420=CARTESIAN_POINT('Origin',(0.,1.,0.));
#36421=CARTESIAN_POINT('',(1.60662857109684,0.,-0.693717979106308));
#36422=CARTESIAN_POINT('Ctrl Pts',(2.0698113262342,-1.,-0.745574324794401));
#36423=CARTESIAN_POINT('Ctrl Pts',(2.0698113262342,1.,-0.745574324794401));
#36424=CARTESIAN_POINT('Ctrl Pts',(2.06854248895728,-1.,-0.745832791378367));
#36425=CARTESIAN_POINT('Ctrl Pts',(2.06854248895728,1.,-0.745832791378367));
#36426=CARTESIAN_POINT('Ctrl Pts',(2.06600523016815,-1.,-0.746345871544201));
#36427=CARTESIAN_POINT('Ctrl Pts',(2.06600523016815,1.,-0.746345871544201));
#36428=CARTESIAN_POINT('Ctrl Pts',(2.06220058927826,-1.,-0.74710393278792));
#36429=CARTESIAN_POINT('Ctrl Pts',(2.06220058927826,1.,-0.74710393278792));
#36430=CARTESIAN_POINT('Ctrl Pts',(2.05713023031006,-1.,-0.748091554183803));
#36431=CARTESIAN_POINT('Ctrl Pts',(2.05713023031006,1.,-0.748091554183803));
#36432=CARTESIAN_POINT('Ctrl Pts',(2.05079645592154,-1.,-0.749287468665046));
#36433=CARTESIAN_POINT('Ctrl Pts',(2.05079645592154,1.,-0.749287468665046));
#36434=CARTESIAN_POINT('Ctrl Pts',(2.04446689147979,-1.,-0.750444657875576));
#36435=CARTESIAN_POINT('Ctrl Pts',(2.04446689147979,1.,-0.750444657875576));
#36436=CARTESIAN_POINT('Ctrl Pts',(2.03814160092099,-1.,-0.751562963361115));
#36437=CARTESIAN_POINT('Ctrl Pts',(2.03814160092099,1.,-0.751562963361115));
#36438=CARTESIAN_POINT('Ctrl Pts',(2.03182068456221,-1.,-0.752642180487211));
#36439=CARTESIAN_POINT('Ctrl Pts',(2.03182068456221,1.,-0.752642180487211));
#36440=CARTESIAN_POINT('Ctrl Pts',(2.02550428623313,-1.,-0.753682061112768));
#36441=CARTESIAN_POINT('Ctrl Pts',(2.02550428623313,1.,-0.753682061112768));
#36442=CARTESIAN_POINT('Ctrl Pts',(2.01919259405809,-1.,-0.754682330722816));
#36443=CARTESIAN_POINT('Ctrl Pts',(2.01919259405809,1.,-0.754682330722816));
#36444=CARTESIAN_POINT('Ctrl Pts',(2.01288584328084,-1.,-0.755642704957865));
#36445=CARTESIAN_POINT('Ctrl Pts',(2.01288584328084,1.,-0.755642704957865));
#36446=CARTESIAN_POINT('Ctrl Pts',(2.0065843158773,-1.,-0.756562904646671));
#36447=CARTESIAN_POINT('Ctrl Pts',(2.0065843158773,1.,-0.756562904646671));
#36448=CARTESIAN_POINT('Ctrl Pts',(2.00028834739178,-1.,-0.757442676862724));
#36449=CARTESIAN_POINT('Ctrl Pts',(2.00028834739178,1.,-0.757442676862724));
#36450=CARTESIAN_POINT('Ctrl Pts',(1.99399831098817,-1.,-0.758281796766761));
#36451=CARTESIAN_POINT('Ctrl Pts',(1.99399831098817,1.,-0.758281796766761));
#36452=CARTESIAN_POINT('Ctrl Pts',(1.98771456680874,-1.,-0.759080037802488));
#36453=CARTESIAN_POINT('Ctrl Pts',(1.98771456680874,1.,-0.759080037802488));
#36454=CARTESIAN_POINT('Ctrl Pts',(1.98143741418172,-1.,-0.75983714745219));
#36455=CARTESIAN_POINT('Ctrl Pts',(1.98143741418172,1.,-0.75983714745219));
#36456=CARTESIAN_POINT('Ctrl Pts',(1.97516705321494,-1.,-0.760552825409757));
#36457=CARTESIAN_POINT('Ctrl Pts',(1.97516705321494,1.,-0.760552825409757));
#36458=CARTESIAN_POINT('Ctrl Pts',(1.96890351582499,-1.,-0.761226690483821));
#36459=CARTESIAN_POINT('Ctrl Pts',(1.96890351582499,1.,-0.761226690483821));
#36460=CARTESIAN_POINT('Ctrl Pts',(1.96264672744186,-1.,-0.761858300014424));
#36461=CARTESIAN_POINT('Ctrl Pts',(1.96264672744186,1.,-0.761858300014424));
#36462=CARTESIAN_POINT('Ctrl Pts',(1.95639665309869,-1.,-0.762447203806179));
#36463=CARTESIAN_POINT('Ctrl Pts',(1.95639665309869,1.,-0.762447203806179));
#36464=CARTESIAN_POINT('Ctrl Pts',(1.95015342590024,-1.,-0.762992990878769));
#36465=CARTESIAN_POINT('Ctrl Pts',(1.95015342590024,1.,-0.762992990878769));
#36466=CARTESIAN_POINT('Ctrl Pts',(1.9439174661764,-1.,-0.763495333538629));
#36467=CARTESIAN_POINT('Ctrl Pts',(1.9439174661764,1.,-0.763495333538629));
#36468=CARTESIAN_POINT('Ctrl Pts',(1.93768964875886,-1.,-0.763954049121459));
#36469=CARTESIAN_POINT('Ctrl Pts',(1.93768964875886,1.,-0.763954049121459));
#36470=CARTESIAN_POINT('Ctrl Pts',(1.93147105496382,-1.,-0.764369010673941));
#36471=CARTESIAN_POINT('Ctrl Pts',(1.93147105496382,1.,-0.764369010673941));
#36472=CARTESIAN_POINT('Ctrl Pts',(1.92526263537048,-1.,-0.764740025488212));
#36473=CARTESIAN_POINT('Ctrl Pts',(1.92526263537048,1.,-0.764740025488212));
#36474=CARTESIAN_POINT('Ctrl Pts',(1.91906491634196,-1.,-0.765066729667089));
#36475=CARTESIAN_POINT('Ctrl Pts',(1.91906491634196,1.,-0.765066729667089));
#36476=CARTESIAN_POINT('Ctrl Pts',(1.91287765805169,-1.,-0.765348465884722));
#36477=CARTESIAN_POINT('Ctrl Pts',(1.91287765805169,1.,-0.765348465884722));
#36478=CARTESIAN_POINT('Ctrl Pts',(1.90669961402356,-1.,-0.765584196937919));
#36479=CARTESIAN_POINT('Ctrl Pts',(1.90669961402356,1.,-0.765584196937919));
#36480=CARTESIAN_POINT('Ctrl Pts',(1.90052930393596,-1.,-0.765772772593386));
#36481=CARTESIAN_POINT('Ctrl Pts',(1.90052930393596,1.,-0.765772772593386));
#36482=CARTESIAN_POINT('Ctrl Pts',(1.89436577771388,-1.,-0.765913193856978));
#36483=CARTESIAN_POINT('Ctrl Pts',(1.89436577771388,1.,-0.765913193856978));
#36484=CARTESIAN_POINT('Ctrl Pts',(1.88820926433409,-1.,-0.766004837062091));
#36485=CARTESIAN_POINT('Ctrl Pts',(1.88820926433409,1.,-0.766004837062091));
#36486=CARTESIAN_POINT('Ctrl Pts',(1.88206215302561,-1.,-0.766047794851865));
#36487=CARTESIAN_POINT('Ctrl Pts',(1.88206215302561,1.,-0.766047794851865));
#36488=CARTESIAN_POINT('Ctrl Pts',(1.87592888967883,-1.,-0.766042837036744));
#36489=CARTESIAN_POINT('Ctrl Pts',(1.87592888967883,1.,-0.766042837036744));
#36490=CARTESIAN_POINT('Ctrl Pts',(1.86981398314341,-1.,-0.765990708546091));
#36491=CARTESIAN_POINT('Ctrl Pts',(1.86981398314341,1.,-0.765990708546091));
#36492=CARTESIAN_POINT('Ctrl Pts',(1.86372027063312,-1.,-0.765891519092547));
#36493=CARTESIAN_POINT('Ctrl Pts',(1.86372027063312,1.,-0.765891519092547));
#36494=CARTESIAN_POINT('Ctrl Pts',(1.85764741390394,-1.,-0.765744212909319));
#36495=CARTESIAN_POINT('Ctrl Pts',(1.85764741390394,1.,-0.765744212909319));
#36496=CARTESIAN_POINT('Ctrl Pts',(1.85158945130063,-1.,-0.765545710619063));
#36497=CARTESIAN_POINT('Ctrl Pts',(1.85158945130063,1.,-0.765545710619063));
#36498=CARTESIAN_POINT('Ctrl Pts',(1.84553698875924,-1.,-0.765291664862029));
#36499=CARTESIAN_POINT('Ctrl Pts',(1.84553698875924,1.,-0.765291664862029));
#36500=CARTESIAN_POINT('Ctrl Pts',(1.83948181064835,-1.,-0.764978057881738));
#36501=CARTESIAN_POINT('Ctrl Pts',(1.83948181064835,1.,-0.764978057881738));
#36502=CARTESIAN_POINT('Ctrl Pts',(1.83342077227142,-1.,-0.764602549687853));
#36503=CARTESIAN_POINT('Ctrl Pts',(1.83342077227142,1.,-0.764602549687853));
#36504=CARTESIAN_POINT('Ctrl Pts',(1.82735991200065,-1.,-0.764165902605995));
#36505=CARTESIAN_POINT('Ctrl Pts',(1.82735991200065,1.,-0.764165902605995));
#36506=CARTESIAN_POINT('Ctrl Pts',(1.82131873145266,-1.,-0.763673465462727));
#36507=CARTESIAN_POINT('Ctrl Pts',(1.82131873145266,1.,-0.763673465462727));
#36508=CARTESIAN_POINT('Ctrl Pts',(1.8153211840553,-1.,-0.763132003836634));
#36509=CARTESIAN_POINT('Ctrl Pts',(1.8153211840553,1.,-0.763132003836634));
#36510=CARTESIAN_POINT('Ctrl Pts',(1.80938551463965,-1.,-0.762546129463938));
#36511=CARTESIAN_POINT('Ctrl Pts',(1.80938551463965,1.,-0.762546129463938));
#36512=CARTESIAN_POINT('Ctrl Pts',(1.80351583877342,-1.,-0.761915336443547));
#36513=CARTESIAN_POINT('Ctrl Pts',(1.80351583877342,1.,-0.761915336443547));
#36514=CARTESIAN_POINT('Ctrl Pts',(1.79768986997783,-1.,-0.761229695230558));
#36515=CARTESIAN_POINT('Ctrl Pts',(1.79768986997783,1.,-0.761229695230558));
#36516=CARTESIAN_POINT('Ctrl Pts',(1.7918581561088,-1.,-0.760469555880749));
#36517=CARTESIAN_POINT('Ctrl Pts',(1.7918581561088,1.,-0.760469555880749));
#36518=CARTESIAN_POINT('Ctrl Pts',(1.78596964884604,-1.,-0.75961440111019));
#36519=CARTESIAN_POINT('Ctrl Pts',(1.78596964884604,1.,-0.75961440111019));
#36520=CARTESIAN_POINT('Ctrl Pts',(1.77999411220945,-1.,-0.758650626677519));
#36521=CARTESIAN_POINT('Ctrl Pts',(1.77999411220945,1.,-0.758650626677519));
#36522=CARTESIAN_POINT('Ctrl Pts',(1.77394167108292,-1.,-0.757578264077029));
#36523=CARTESIAN_POINT('Ctrl Pts',(1.77394167108292,1.,-0.757578264077029));
#36524=CARTESIAN_POINT('Ctrl Pts',(1.76789396002998,-1.,-0.75642189602781));
#36525=CARTESIAN_POINT('Ctrl Pts',(1.76789396002998,1.,-0.75642189602781));
#36526=CARTESIAN_POINT('Ctrl Pts',(1.76197817240128,-1.,-0.755220979974462));
#36527=CARTESIAN_POINT('Ctrl Pts',(1.76197817240128,1.,-0.755220979974462));
#36528=CARTESIAN_POINT('Ctrl Pts',(1.75631083600019,-1.,-0.754009254027829));
#36529=CARTESIAN_POINT('Ctrl Pts',(1.75631083600019,1.,-0.754009254027829));
#36530=CARTESIAN_POINT('Ctrl Pts',(1.75095139468794,-1.,-0.752797683531314));
#36531=CARTESIAN_POINT('Ctrl Pts',(1.75095139468794,1.,-0.752797683531314));
#36532=CARTESIAN_POINT('Ctrl Pts',(1.74585086852502,-1.,-0.751555614164483));
#36533=CARTESIAN_POINT('Ctrl Pts',(1.74585086852502,1.,-0.751555614164483));
#36534=CARTESIAN_POINT('Ctrl Pts',(1.74080458267114,-1.,-0.75019343598125));
#36535=CARTESIAN_POINT('Ctrl Pts',(1.74080458267114,1.,-0.75019343598125));
#36536=CARTESIAN_POINT('Ctrl Pts',(1.7355035168033,-1.,-0.74858246295687));
#36537=CARTESIAN_POINT('Ctrl Pts',(1.7355035168033,1.,-0.74858246295687));
#36538=CARTESIAN_POINT('Ctrl Pts',(1.72958533647714,-1.,-0.746574710097752));
#36539=CARTESIAN_POINT('Ctrl Pts',(1.72958533647714,1.,-0.746574710097752));
#36540=CARTESIAN_POINT('Ctrl Pts',(1.72268229916769,-1.,-0.744021445433094));
#36541=CARTESIAN_POINT('Ctrl Pts',(1.72268229916769,1.,-0.744021445433094));
#36542=CARTESIAN_POINT('Ctrl Pts',(1.71447789751001,-1.,-0.74079516202821));
#36543=CARTESIAN_POINT('Ctrl Pts',(1.71447789751001,1.,-0.74079516202821));
#36544=CARTESIAN_POINT('Ctrl Pts',(1.70473309004249,-1.,-0.736799665716932));
#36545=CARTESIAN_POINT('Ctrl Pts',(1.70473309004249,1.,-0.736799665716932));
#36546=CARTESIAN_POINT('Ctrl Pts',(1.69326921972915,-1.,-0.731963238685357));
#36547=CARTESIAN_POINT('Ctrl Pts',(1.69326921972915,1.,-0.731963238685357));
#36548=CARTESIAN_POINT('Ctrl Pts',(1.67996158451922,-1.,-0.726235967982445));
#36549=CARTESIAN_POINT('Ctrl Pts',(1.67996158451922,1.,-0.726235967982445));
#36550=CARTESIAN_POINT('Ctrl Pts',(1.66472880551777,-1.,-0.71958543378795));
#36551=CARTESIAN_POINT('Ctrl Pts',(1.66472880551777,1.,-0.71958543378795));
#36552=CARTESIAN_POINT('Ctrl Pts',(1.64752408828442,-1.,-0.711993139340448));
#36553=CARTESIAN_POINT('Ctrl Pts',(1.64752408828442,1.,-0.711993139340448));
#36554=CARTESIAN_POINT('Ctrl Pts',(1.6321654166204,-1.,-0.705159151977294));
#36555=CARTESIAN_POINT('Ctrl Pts',(1.6321654166204,1.,-0.705159151977294));
#36556=CARTESIAN_POINT('Ctrl Pts',(1.61974673471117,-1.,-0.699605146398837));
#36557=CARTESIAN_POINT('Ctrl Pts',(1.61974673471117,1.,-0.699605146398837));
#36558=CARTESIAN_POINT('Ctrl Pts',(1.61106790957619,-1.,-0.69571209787897));
#36559=CARTESIAN_POINT('Ctrl Pts',(1.61106790957619,1.,-0.69571209787897));
#36560=CARTESIAN_POINT('Ctrl Pts',(1.60662857109684,-1.,-0.693717979106306));
#36561=CARTESIAN_POINT('Ctrl Pts',(1.60662857109684,1.,-0.693717979106306));
#36562=CARTESIAN_POINT('',(2.0698113262342,1.,-0.745574324794401));
#36563=CARTESIAN_POINT('Ctrl Pts',(2.0698113262342,1.,-0.745574324794401));
#36564=CARTESIAN_POINT('Ctrl Pts',(2.06854248895728,1.,-0.745832791378367));
#36565=CARTESIAN_POINT('Ctrl Pts',(2.06600523016815,1.,-0.746345871544201));
#36566=CARTESIAN_POINT('Ctrl Pts',(2.06220058927826,1.,-0.74710393278792));
#36567=CARTESIAN_POINT('Ctrl Pts',(2.05713023031006,1.,-0.748091554183803));
#36568=CARTESIAN_POINT('Ctrl Pts',(2.05079645592154,1.,-0.749287468665046));
#36569=CARTESIAN_POINT('Ctrl Pts',(2.04446689147979,1.,-0.750444657875576));
#36570=CARTESIAN_POINT('Ctrl Pts',(2.03814160092099,1.,-0.751562963361115));
#36571=CARTESIAN_POINT('Ctrl Pts',(2.03182068456221,1.,-0.752642180487211));
#36572=CARTESIAN_POINT('Ctrl Pts',(2.02550428623313,1.,-0.753682061112768));
#36573=CARTESIAN_POINT('Ctrl Pts',(2.01919259405809,1.,-0.754682330722816));
#36574=CARTESIAN_POINT('Ctrl Pts',(2.01288584328084,1.,-0.755642704957865));
#36575=CARTESIAN_POINT('Ctrl Pts',(2.0065843158773,1.,-0.756562904646671));
#36576=CARTESIAN_POINT('Ctrl Pts',(2.00028834739178,1.,-0.757442676862724));
#36577=CARTESIAN_POINT('Ctrl Pts',(1.99399831098817,1.,-0.758281796766761));
#36578=CARTESIAN_POINT('Ctrl Pts',(1.98771456680874,1.,-0.759080037802488));
#36579=CARTESIAN_POINT('Ctrl Pts',(1.98143741418172,1.,-0.75983714745219));
#36580=CARTESIAN_POINT('Ctrl Pts',(1.97516705321494,1.,-0.760552825409757));
#36581=CARTESIAN_POINT('Ctrl Pts',(1.96890351582499,1.,-0.761226690483821));
#36582=CARTESIAN_POINT('Ctrl Pts',(1.96264672744186,1.,-0.761858300014424));
#36583=CARTESIAN_POINT('Ctrl Pts',(1.95639665309869,1.,-0.762447203806179));
#36584=CARTESIAN_POINT('Ctrl Pts',(1.95015342590024,1.,-0.762992990878769));
#36585=CARTESIAN_POINT('Ctrl Pts',(1.9439174661764,1.,-0.763495333538629));
#36586=CARTESIAN_POINT('Ctrl Pts',(1.93768964875886,1.,-0.763954049121459));
#36587=CARTESIAN_POINT('Ctrl Pts',(1.93147105496382,1.,-0.764369010673941));
#36588=CARTESIAN_POINT('Ctrl Pts',(1.92526263537048,1.,-0.764740025488212));
#36589=CARTESIAN_POINT('Ctrl Pts',(1.91906491634196,1.,-0.765066729667089));
#36590=CARTESIAN_POINT('Ctrl Pts',(1.91287765805169,1.,-0.765348465884722));
#36591=CARTESIAN_POINT('Ctrl Pts',(1.90669961402356,1.,-0.765584196937919));
#36592=CARTESIAN_POINT('Ctrl Pts',(1.90052930393596,1.,-0.765772772593386));
#36593=CARTESIAN_POINT('Ctrl Pts',(1.89436577771388,1.,-0.765913193856978));
#36594=CARTESIAN_POINT('Ctrl Pts',(1.88820926433409,1.,-0.766004837062091));
#36595=CARTESIAN_POINT('Ctrl Pts',(1.88206215302561,1.,-0.766047794851865));
#36596=CARTESIAN_POINT('Ctrl Pts',(1.87592888967883,1.,-0.766042837036744));
#36597=CARTESIAN_POINT('Ctrl Pts',(1.86981398314341,1.,-0.765990708546091));
#36598=CARTESIAN_POINT('Ctrl Pts',(1.86372027063312,1.,-0.765891519092547));
#36599=CARTESIAN_POINT('Ctrl Pts',(1.85764741390394,1.,-0.765744212909319));
#36600=CARTESIAN_POINT('Ctrl Pts',(1.85158945130063,1.,-0.765545710619063));
#36601=CARTESIAN_POINT('Ctrl Pts',(1.84553698875924,1.,-0.765291664862029));
#36602=CARTESIAN_POINT('Ctrl Pts',(1.83948181064835,1.,-0.764978057881738));
#36603=CARTESIAN_POINT('Ctrl Pts',(1.83342077227142,1.,-0.764602549687853));
#36604=CARTESIAN_POINT('Ctrl Pts',(1.82735991200065,1.,-0.764165902605995));
#36605=CARTESIAN_POINT('Ctrl Pts',(1.82131873145266,1.,-0.763673465462727));
#36606=CARTESIAN_POINT('Ctrl Pts',(1.8153211840553,1.,-0.763132003836634));
#36607=CARTESIAN_POINT('Ctrl Pts',(1.80938551463965,1.,-0.762546129463938));
#36608=CARTESIAN_POINT('Ctrl Pts',(1.80351583877342,1.,-0.761915336443547));
#36609=CARTESIAN_POINT('Ctrl Pts',(1.79768986997783,1.,-0.761229695230558));
#36610=CARTESIAN_POINT('Ctrl Pts',(1.7918581561088,1.,-0.760469555880749));
#36611=CARTESIAN_POINT('Ctrl Pts',(1.78596964884604,1.,-0.75961440111019));
#36612=CARTESIAN_POINT('Ctrl Pts',(1.77999411220945,1.,-0.758650626677519));
#36613=CARTESIAN_POINT('Ctrl Pts',(1.77394167108292,1.,-0.757578264077029));
#36614=CARTESIAN_POINT('Ctrl Pts',(1.76789396002998,1.,-0.75642189602781));
#36615=CARTESIAN_POINT('Ctrl Pts',(1.76197817240128,1.,-0.755220979974462));
#36616=CARTESIAN_POINT('Ctrl Pts',(1.75631083600019,1.,-0.754009254027829));
#36617=CARTESIAN_POINT('Ctrl Pts',(1.75095139468794,1.,-0.752797683531314));
#36618=CARTESIAN_POINT('Ctrl Pts',(1.74585086852502,1.,-0.751555614164483));
#36619=CARTESIAN_POINT('Ctrl Pts',(1.74080458267114,1.,-0.75019343598125));
#36620=CARTESIAN_POINT('Ctrl Pts',(1.7355035168033,1.,-0.74858246295687));
#36621=CARTESIAN_POINT('Ctrl Pts',(1.72958533647714,1.,-0.746574710097752));
#36622=CARTESIAN_POINT('Ctrl Pts',(1.72268229916769,1.,-0.744021445433094));
#36623=CARTESIAN_POINT('Ctrl Pts',(1.71447789751001,1.,-0.74079516202821));
#36624=CARTESIAN_POINT('Ctrl Pts',(1.70473309004249,1.,-0.736799665716932));
#36625=CARTESIAN_POINT('Ctrl Pts',(1.69326921972915,1.,-0.731963238685357));
#36626=CARTESIAN_POINT('Ctrl Pts',(1.67996158451922,1.,-0.726235967982445));
#36627=CARTESIAN_POINT('Ctrl Pts',(1.66472880551777,1.,-0.71958543378795));
#36628=CARTESIAN_POINT('Ctrl Pts',(1.64752408828442,1.,-0.711993139340448));
#36629=CARTESIAN_POINT('Ctrl Pts',(1.6321654166204,1.,-0.705159151977294));
#36630=CARTESIAN_POINT('Ctrl Pts',(1.61974673471117,1.,-0.699605146398837));
#36631=CARTESIAN_POINT('Ctrl Pts',(1.61106790957619,1.,-0.69571209787897));
#36632=CARTESIAN_POINT('Ctrl Pts',(1.60662857109684,1.,-0.693717979106306));
#36633=CARTESIAN_POINT('',(2.0698113262342,0.,-0.745574324794401));
#36634=CARTESIAN_POINT('Origin',(2.11275013067528,0.,-0.61342227326009));
#36635=CARTESIAN_POINT('',(2.11275013067528,1.,-0.61342227326009));
#36636=CARTESIAN_POINT('',(2.0698113262342,1.,-0.745574324794401));
#36637=CARTESIAN_POINT('',(2.11275013067528,0.,-0.61342227326009));
#36638=CARTESIAN_POINT('Ctrl Pts',(1.7075470150345,-1.,-0.383122945602004));
#36639=CARTESIAN_POINT('Ctrl Pts',(1.7075470150345,1.,-0.383122945602004));
#36640=CARTESIAN_POINT('Ctrl Pts',(1.71231062891958,-1.,-0.384119047315542));
#36641=CARTESIAN_POINT('Ctrl Pts',(1.71231062891958,1.,-0.384119047315542));
#36642=CARTESIAN_POINT('Ctrl Pts',(1.72162022246158,-1.,-0.38607079032701));
#36643=CARTESIAN_POINT('Ctrl Pts',(1.72162022246158,1.,-0.38607079032701));
#36644=CARTESIAN_POINT('Ctrl Pts',(1.7349317097561,-1.,-0.388877023509192));
#36645=CARTESIAN_POINT('Ctrl Pts',(1.7349317097561,1.,-0.388877023509192));
#36646=CARTESIAN_POINT('Ctrl Pts',(1.75137405313962,-1.,-0.392375812294307));
#36647=CARTESIAN_POINT('Ctrl Pts',(1.75137405313962,1.,-0.392375812294307));
#36648=CARTESIAN_POINT('Ctrl Pts',(1.7697556004756,-1.,-0.39634619612042));
#36649=CARTESIAN_POINT('Ctrl Pts',(1.7697556004756,1.,-0.39634619612042));
#36650=CARTESIAN_POINT('Ctrl Pts',(1.78598826347533,-1.,-0.399919403783081));
#36651=CARTESIAN_POINT('Ctrl Pts',(1.78598826347533,1.,-0.399919403783081));
#36652=CARTESIAN_POINT('Ctrl Pts',(1.80012077176221,-1.,-0.403107976170441));
#36653=CARTESIAN_POINT('Ctrl Pts',(1.80012077176221,1.,-0.403107976170441));
#36654=CARTESIAN_POINT('Ctrl Pts',(1.81223801813988,-1.,-0.405933518411838));
#36655=CARTESIAN_POINT('Ctrl Pts',(1.81223801813988,1.,-0.405933518411838));
#36656=CARTESIAN_POINT('Ctrl Pts',(1.8224702267854,-1.,-0.408428948108534));
#36657=CARTESIAN_POINT('Ctrl Pts',(1.8224702267854,1.,-0.408428948108534));
#36658=CARTESIAN_POINT('Ctrl Pts',(1.83100408895216,-1.,-0.410641256301675));
#36659=CARTESIAN_POINT('Ctrl Pts',(1.83100408895216,1.,-0.410641256301675));
#36660=CARTESIAN_POINT('Ctrl Pts',(1.83808953475839,-1.,-0.412633125322162));
#36661=CARTESIAN_POINT('Ctrl Pts',(1.83808953475839,1.,-0.412633125322162));
#36662=CARTESIAN_POINT('Ctrl Pts',(1.8440575707371,-1.,-0.41448743825434));
#36663=CARTESIAN_POINT('Ctrl Pts',(1.8440575707371,1.,-0.41448743825434));
#36664=CARTESIAN_POINT('Ctrl Pts',(1.84929312929882,-1.,-0.416300022038864));
#36665=CARTESIAN_POINT('Ctrl Pts',(1.84929312929882,1.,-0.416300022038864));
#36666=CARTESIAN_POINT('Ctrl Pts',(1.85417632856234,-1.,-0.418164129143534));
#36667=CARTESIAN_POINT('Ctrl Pts',(1.85417632856234,1.,-0.418164129143534));
#36668=CARTESIAN_POINT('Ctrl Pts',(1.85903281096686,-1.,-0.42015728797562));
#36669=CARTESIAN_POINT('Ctrl Pts',(1.85903281096686,1.,-0.42015728797562));
#36670=CARTESIAN_POINT('Ctrl Pts',(1.86408083334028,-1.,-0.422327307418275));
#36671=CARTESIAN_POINT('Ctrl Pts',(1.86408083334028,1.,-0.422327307418275));
#36672=CARTESIAN_POINT('Ctrl Pts',(1.86937803944323,-1.,-0.424678177291359));
#36673=CARTESIAN_POINT('Ctrl Pts',(1.86937803944323,1.,-0.424678177291359));
#36674=CARTESIAN_POINT('Ctrl Pts',(1.87486989291484,-1.,-0.427183828519102));
#36675=CARTESIAN_POINT('Ctrl Pts',(1.87486989291484,1.,-0.427183828519102));
#36676=CARTESIAN_POINT('Ctrl Pts',(1.88044229001832,-1.,-0.429803062482345));
#36677=CARTESIAN_POINT('Ctrl Pts',(1.88044229001832,1.,-0.429803062482345));
#36678=CARTESIAN_POINT('Ctrl Pts',(1.88596913666793,-1.,-0.432493038548748));
#36679=CARTESIAN_POINT('Ctrl Pts',(1.88596913666793,1.,-0.432493038548748));
#36680=CARTESIAN_POINT('Ctrl Pts',(1.89136993975504,-1.,-0.435225660963383));
#36681=CARTESIAN_POINT('Ctrl Pts',(1.89136993975504,1.,-0.435225660963383));
#36682=CARTESIAN_POINT('Ctrl Pts',(1.89663648956466,-1.,-0.437995003948244));
#36683=CARTESIAN_POINT('Ctrl Pts',(1.89663648956466,1.,-0.437995003948244));
#36684=CARTESIAN_POINT('Ctrl Pts',(1.90180124389086,-1.,-0.440807833704038));
#36685=CARTESIAN_POINT('Ctrl Pts',(1.90180124389086,1.,-0.440807833704038));
#36686=CARTESIAN_POINT('Ctrl Pts',(1.90691756144898,-1.,-0.443677556849151));
#36687=CARTESIAN_POINT('Ctrl Pts',(1.90691756144898,1.,-0.443677556849151));
#36688=CARTESIAN_POINT('Ctrl Pts',(1.9120369998112,-1.,-0.446617343485711));
#36689=CARTESIAN_POINT('Ctrl Pts',(1.9120369998112,1.,-0.446617343485711));
#36690=CARTESIAN_POINT('Ctrl Pts',(1.91718342555755,-1.,-0.449632260106662));
#36691=CARTESIAN_POINT('Ctrl Pts',(1.91718342555755,1.,-0.449632260106662));
#36692=CARTESIAN_POINT('Ctrl Pts',(1.92235380648502,-1.,-0.452719478359433));
#36693=CARTESIAN_POINT('Ctrl Pts',(1.92235380648502,1.,-0.452719478359433));
#36694=CARTESIAN_POINT('Ctrl Pts',(1.92753067150476,-1.,-0.455872005174371));
#36695=CARTESIAN_POINT('Ctrl Pts',(1.92753067150476,1.,-0.455872005174371));
#36696=CARTESIAN_POINT('Ctrl Pts',(1.93269066517934,-1.,-0.459081234547926));
#36697=CARTESIAN_POINT('Ctrl Pts',(1.93269066517934,1.,-0.459081234547926));
#36698=CARTESIAN_POINT('Ctrl Pts',(1.93781486640821,-1.,-0.462340031009057));
#36699=CARTESIAN_POINT('Ctrl Pts',(1.93781486640821,1.,-0.462340031009057));
#36700=CARTESIAN_POINT('Ctrl Pts',(1.9428979419619,-1.,-0.46564546202603));
#36701=CARTESIAN_POINT('Ctrl Pts',(1.9428979419619,1.,-0.46564546202603));
#36702=CARTESIAN_POINT('Ctrl Pts',(1.94794381136514,-1.,-0.468997482913135));
#36703=CARTESIAN_POINT('Ctrl Pts',(1.94794381136514,1.,-0.468997482913135));
#36704=CARTESIAN_POINT('Ctrl Pts',(1.95296148278133,-1.,-0.472397672264072));
#36705=CARTESIAN_POINT('Ctrl Pts',(1.95296148278133,1.,-0.472397672264072));
#36706=CARTESIAN_POINT('Ctrl Pts',(1.95796111148177,-1.,-0.475848034683176));
#36707=CARTESIAN_POINT('Ctrl Pts',(1.95796111148177,1.,-0.475848034683176));
#36708=CARTESIAN_POINT('Ctrl Pts',(1.96294933055943,-1.,-0.479349583074855));
#36709=CARTESIAN_POINT('Ctrl Pts',(1.96294933055943,1.,-0.479349583074855));
#36710=CARTESIAN_POINT('Ctrl Pts',(1.96792703422362,-1.,-0.482901662120691));
#36711=CARTESIAN_POINT('Ctrl Pts',(1.96792703422362,1.,-0.482901662120691));
#36712=CARTESIAN_POINT('Ctrl Pts',(1.97289186263272,-1.,-0.486502692907659));
#36713=CARTESIAN_POINT('Ctrl Pts',(1.97289186263272,1.,-0.486502692907659));
#36714=CARTESIAN_POINT('Ctrl Pts',(1.97783973019229,-1.,-0.490150627860953));
#36715=CARTESIAN_POINT('Ctrl Pts',(1.97783973019229,1.,-0.490150627860953));
#36716=CARTESIAN_POINT('Ctrl Pts',(1.98276658761821,-1.,-0.493843476541495));
#36717=CARTESIAN_POINT('Ctrl Pts',(1.98276658761821,1.,-0.493843476541495));
#36718=CARTESIAN_POINT('Ctrl Pts',(1.98767044752932,-1.,-0.497579909545574));
#36719=CARTESIAN_POINT('Ctrl Pts',(1.98767044752932,1.,-0.497579909545574));
#36720=CARTESIAN_POINT('Ctrl Pts',(1.99255149126155,-1.,-0.501359287727146));
#36721=CARTESIAN_POINT('Ctrl Pts',(1.99255149126155,1.,-0.501359287727146));
#36722=CARTESIAN_POINT('Ctrl Pts',(1.99741107463572,-1.,-0.505181361323026));
#36723=CARTESIAN_POINT('Ctrl Pts',(1.99741107463572,1.,-0.505181361323026));
#36724=CARTESIAN_POINT('Ctrl Pts',(2.00225107134734,-1.,-0.509046069886157));
#36725=CARTESIAN_POINT('Ctrl Pts',(2.00225107134734,1.,-0.509046069886157));
#36726=CARTESIAN_POINT('Ctrl Pts',(2.00707309946949,-1.,-0.512953306961793));
#36727=CARTESIAN_POINT('Ctrl Pts',(2.00707309946949,1.,-0.512953306961793));
#36728=CARTESIAN_POINT('Ctrl Pts',(2.01187773939242,-1.,-0.516902681728687));
#36729=CARTESIAN_POINT('Ctrl Pts',(2.01187773939242,1.,-0.516902681728687));
#36730=CARTESIAN_POINT('Ctrl Pts',(2.01666477917286,-1.,-0.520893590399371));
#36731=CARTESIAN_POINT('Ctrl Pts',(2.01666477917286,1.,-0.520893590399371));
#36732=CARTESIAN_POINT('Ctrl Pts',(2.02143356304698,-1.,-0.524925318333476));
#36733=CARTESIAN_POINT('Ctrl Pts',(2.02143356304698,1.,-0.524925318333476));
#36734=CARTESIAN_POINT('Ctrl Pts',(2.0261832908329,-1.,-0.528997127241914));
#36735=CARTESIAN_POINT('Ctrl Pts',(2.0261832908329,1.,-0.528997127241914));
#36736=CARTESIAN_POINT('Ctrl Pts',(2.03091336214426,-1.,-0.533108355132977));
#36737=CARTESIAN_POINT('Ctrl Pts',(2.03091336214426,1.,-0.533108355132977));
#36738=CARTESIAN_POINT('Ctrl Pts',(2.03562362954037,-1.,-0.537258489833262));
#36739=CARTESIAN_POINT('Ctrl Pts',(2.03562362954037,1.,-0.537258489833262));
#36740=CARTESIAN_POINT('Ctrl Pts',(2.04031422690527,-1.,-0.541447120615659));
#36741=CARTESIAN_POINT('Ctrl Pts',(2.04031422690527,1.,-0.541447120615659));
#36742=CARTESIAN_POINT('Ctrl Pts',(2.04498544714588,-1.,-0.54567390381743));
#36743=CARTESIAN_POINT('Ctrl Pts',(2.04498544714588,1.,-0.54567390381743));
#36744=CARTESIAN_POINT('Ctrl Pts',(2.04963761077958,-1.,-0.549938525150295));
#36745=CARTESIAN_POINT('Ctrl Pts',(2.04963761077958,1.,-0.549938525150295));
#36746=CARTESIAN_POINT('Ctrl Pts',(2.05427091604413,-1.,-0.554240657463906));
#36747=CARTESIAN_POINT('Ctrl Pts',(2.05427091604413,1.,-0.554240657463906));
#36748=CARTESIAN_POINT('Ctrl Pts',(2.05888537756462,-1.,-0.558579940185152));
#36749=CARTESIAN_POINT('Ctrl Pts',(2.05888537756462,1.,-0.558579940185152));
#36750=CARTESIAN_POINT('Ctrl Pts',(2.06348090160589,-1.,-0.562955993082262));
#36751=CARTESIAN_POINT('Ctrl Pts',(2.06348090160589,1.,-0.562955993082262));
#36752=CARTESIAN_POINT('Ctrl Pts',(2.06805732997334,-1.,-0.567368421181087));
#36753=CARTESIAN_POINT('Ctrl Pts',(2.06805732997334,1.,-0.567368421181087));
#36754=CARTESIAN_POINT('Ctrl Pts',(2.07261449292824,-1.,-0.571816823242603));
#36755=CARTESIAN_POINT('Ctrl Pts',(2.07261449292824,1.,-0.571816823242603));
#36756=CARTESIAN_POINT('Ctrl Pts',(2.07715226767559,-1.,-0.576300797416845));
#36757=CARTESIAN_POINT('Ctrl Pts',(2.07715226767559,1.,-0.576300797416845));
#36758=CARTESIAN_POINT('Ctrl Pts',(2.08167059018418,-1.,-0.580819952108064));
#36759=CARTESIAN_POINT('Ctrl Pts',(2.08167059018418,1.,-0.580819952108064));
#36760=CARTESIAN_POINT('Ctrl Pts',(2.08616943727951,-1.,-0.585373918991617));
#36761=CARTESIAN_POINT('Ctrl Pts',(2.08616943727951,1.,-0.585373918991617));
#36762=CARTESIAN_POINT('Ctrl Pts',(2.09064881812129,-1.,-0.589962365403406));
#36763=CARTESIAN_POINT('Ctrl Pts',(2.09064881812129,1.,-0.589962365403406));
#36764=CARTESIAN_POINT('Ctrl Pts',(2.0951087622027,-1.,-0.594585006052162));
#36765=CARTESIAN_POINT('Ctrl Pts',(2.0951087622027,1.,-0.594585006052162));
#36766=CARTESIAN_POINT('Ctrl Pts',(2.0995493086477,-1.,-0.599241616420534));
#36767=CARTESIAN_POINT('Ctrl Pts',(2.0995493086477,1.,-0.599241616420534));
#36768=CARTESIAN_POINT('Ctrl Pts',(2.10397049886949,-1.,-0.60393203073603));
#36769=CARTESIAN_POINT('Ctrl Pts',(2.10397049886949,1.,-0.60393203073603));
#36770=CARTESIAN_POINT('Ctrl Pts',(2.1074919961518,-1.,-0.607711315454876));
#36771=CARTESIAN_POINT('Ctrl Pts',(2.1074919961518,1.,-0.607711315454876));
#36772=CARTESIAN_POINT('Ctrl Pts',(2.11012443807238,-1.,-0.610560911689899));
#36773=CARTESIAN_POINT('Ctrl Pts',(2.11012443807238,1.,-0.610560911689899));
#36774=CARTESIAN_POINT('Ctrl Pts',(2.11187554259986,-1.,-0.6124673655618));
#36775=CARTESIAN_POINT('Ctrl Pts',(2.11187554259986,1.,-0.6124673655618));
#36776=CARTESIAN_POINT('Ctrl Pts',(2.11275013067528,-1.,-0.61342227326009));
#36777=CARTESIAN_POINT('Ctrl Pts',(2.11275013067528,1.,-0.61342227326009));
#36778=CARTESIAN_POINT('',(1.7075470150345,1.,-0.383122945602004));
#36779=CARTESIAN_POINT('Ctrl Pts',(1.7075470150345,1.,-0.383122945602004));
#36780=CARTESIAN_POINT('Ctrl Pts',(1.71231062891958,1.,-0.384119047315542));
#36781=CARTESIAN_POINT('Ctrl Pts',(1.72162022246158,1.,-0.38607079032701));
#36782=CARTESIAN_POINT('Ctrl Pts',(1.7349317097561,1.,-0.388877023509192));
#36783=CARTESIAN_POINT('Ctrl Pts',(1.75137405313962,1.,-0.392375812294307));
#36784=CARTESIAN_POINT('Ctrl Pts',(1.7697556004756,1.,-0.39634619612042));
#36785=CARTESIAN_POINT('Ctrl Pts',(1.78598826347533,1.,-0.399919403783081));
#36786=CARTESIAN_POINT('Ctrl Pts',(1.80012077176221,1.,-0.403107976170441));
#36787=CARTESIAN_POINT('Ctrl Pts',(1.81223801813988,1.,-0.405933518411838));
#36788=CARTESIAN_POINT('Ctrl Pts',(1.8224702267854,1.,-0.408428948108534));
#36789=CARTESIAN_POINT('Ctrl Pts',(1.83100408895216,1.,-0.410641256301675));
#36790=CARTESIAN_POINT('Ctrl Pts',(1.83808953475839,1.,-0.412633125322162));
#36791=CARTESIAN_POINT('Ctrl Pts',(1.8440575707371,1.,-0.41448743825434));
#36792=CARTESIAN_POINT('Ctrl Pts',(1.84929312929882,1.,-0.416300022038864));
#36793=CARTESIAN_POINT('Ctrl Pts',(1.85417632856234,1.,-0.418164129143534));
#36794=CARTESIAN_POINT('Ctrl Pts',(1.85903281096686,1.,-0.42015728797562));
#36795=CARTESIAN_POINT('Ctrl Pts',(1.86408083334028,1.,-0.422327307418275));
#36796=CARTESIAN_POINT('Ctrl Pts',(1.86937803944323,1.,-0.424678177291359));
#36797=CARTESIAN_POINT('Ctrl Pts',(1.87486989291484,1.,-0.427183828519102));
#36798=CARTESIAN_POINT('Ctrl Pts',(1.88044229001832,1.,-0.429803062482345));
#36799=CARTESIAN_POINT('Ctrl Pts',(1.88596913666793,1.,-0.432493038548748));
#36800=CARTESIAN_POINT('Ctrl Pts',(1.89136993975504,1.,-0.435225660963383));
#36801=CARTESIAN_POINT('Ctrl Pts',(1.89663648956466,1.,-0.437995003948244));
#36802=CARTESIAN_POINT('Ctrl Pts',(1.90180124389086,1.,-0.440807833704038));
#36803=CARTESIAN_POINT('Ctrl Pts',(1.90691756144898,1.,-0.443677556849151));
#36804=CARTESIAN_POINT('Ctrl Pts',(1.9120369998112,1.,-0.446617343485711));
#36805=CARTESIAN_POINT('Ctrl Pts',(1.91718342555755,1.,-0.449632260106662));
#36806=CARTESIAN_POINT('Ctrl Pts',(1.92235380648502,1.,-0.452719478359433));
#36807=CARTESIAN_POINT('Ctrl Pts',(1.92753067150476,1.,-0.455872005174371));
#36808=CARTESIAN_POINT('Ctrl Pts',(1.93269066517934,1.,-0.459081234547926));
#36809=CARTESIAN_POINT('Ctrl Pts',(1.93781486640821,1.,-0.462340031009057));
#36810=CARTESIAN_POINT('Ctrl Pts',(1.9428979419619,1.,-0.46564546202603));
#36811=CARTESIAN_POINT('Ctrl Pts',(1.94794381136514,1.,-0.468997482913135));
#36812=CARTESIAN_POINT('Ctrl Pts',(1.95296148278133,1.,-0.472397672264072));
#36813=CARTESIAN_POINT('Ctrl Pts',(1.95796111148177,1.,-0.475848034683176));
#36814=CARTESIAN_POINT('Ctrl Pts',(1.96294933055943,1.,-0.479349583074855));
#36815=CARTESIAN_POINT('Ctrl Pts',(1.96792703422362,1.,-0.482901662120691));
#36816=CARTESIAN_POINT('Ctrl Pts',(1.97289186263272,1.,-0.486502692907659));
#36817=CARTESIAN_POINT('Ctrl Pts',(1.97783973019229,1.,-0.490150627860953));
#36818=CARTESIAN_POINT('Ctrl Pts',(1.98276658761821,1.,-0.493843476541495));
#36819=CARTESIAN_POINT('Ctrl Pts',(1.98767044752932,1.,-0.497579909545574));
#36820=CARTESIAN_POINT('Ctrl Pts',(1.99255149126155,1.,-0.501359287727146));
#36821=CARTESIAN_POINT('Ctrl Pts',(1.99741107463572,1.,-0.505181361323026));
#36822=CARTESIAN_POINT('Ctrl Pts',(2.00225107134734,1.,-0.509046069886157));
#36823=CARTESIAN_POINT('Ctrl Pts',(2.00707309946949,1.,-0.512953306961793));
#36824=CARTESIAN_POINT('Ctrl Pts',(2.01187773939242,1.,-0.516902681728687));
#36825=CARTESIAN_POINT('Ctrl Pts',(2.01666477917286,1.,-0.520893590399371));
#36826=CARTESIAN_POINT('Ctrl Pts',(2.02143356304698,1.,-0.524925318333476));
#36827=CARTESIAN_POINT('Ctrl Pts',(2.0261832908329,1.,-0.528997127241914));
#36828=CARTESIAN_POINT('Ctrl Pts',(2.03091336214426,1.,-0.533108355132977));
#36829=CARTESIAN_POINT('Ctrl Pts',(2.03562362954037,1.,-0.537258489833262));
#36830=CARTESIAN_POINT('Ctrl Pts',(2.04031422690527,1.,-0.541447120615659));
#36831=CARTESIAN_POINT('Ctrl Pts',(2.04498544714588,1.,-0.54567390381743));
#36832=CARTESIAN_POINT('Ctrl Pts',(2.04963761077958,1.,-0.549938525150295));
#36833=CARTESIAN_POINT('Ctrl Pts',(2.05427091604413,1.,-0.554240657463906));
#36834=CARTESIAN_POINT('Ctrl Pts',(2.05888537756462,1.,-0.558579940185152));
#36835=CARTESIAN_POINT('Ctrl Pts',(2.06348090160589,1.,-0.562955993082262));
#36836=CARTESIAN_POINT('Ctrl Pts',(2.06805732997334,1.,-0.567368421181087));
#36837=CARTESIAN_POINT('Ctrl Pts',(2.07261449292824,1.,-0.571816823242603));
#36838=CARTESIAN_POINT('Ctrl Pts',(2.07715226767559,1.,-0.576300797416845));
#36839=CARTESIAN_POINT('Ctrl Pts',(2.08167059018418,1.,-0.580819952108064));
#36840=CARTESIAN_POINT('Ctrl Pts',(2.08616943727951,1.,-0.585373918991617));
#36841=CARTESIAN_POINT('Ctrl Pts',(2.09064881812129,1.,-0.589962365403406));
#36842=CARTESIAN_POINT('Ctrl Pts',(2.0951087622027,1.,-0.594585006052162));
#36843=CARTESIAN_POINT('Ctrl Pts',(2.0995493086477,1.,-0.599241616420534));
#36844=CARTESIAN_POINT('Ctrl Pts',(2.10397049886949,1.,-0.60393203073603));
#36845=CARTESIAN_POINT('Ctrl Pts',(2.1074919961518,1.,-0.607711315454876));
#36846=CARTESIAN_POINT('Ctrl Pts',(2.11012443807238,1.,-0.610560911689899));
#36847=CARTESIAN_POINT('Ctrl Pts',(2.11187554259986,1.,-0.6124673655618));
#36848=CARTESIAN_POINT('Ctrl Pts',(2.11275013067528,1.,-0.61342227326009));
#36849=CARTESIAN_POINT('',(1.7075470150345,0.,-0.383122945602001));
#36850=CARTESIAN_POINT('Origin',(0.,0.,0.));
#36851=CARTESIAN_POINT('',(1.74236521665491,1.,-0.163289472382896));
#36852=CARTESIAN_POINT('Origin',(0.,1.,0.));
#36853=CARTESIAN_POINT('',(1.74236521665491,0.,-0.163289472382896));
#36854=CARTESIAN_POINT('Ctrl Pts',(2.19890268624765,-1.,-0.0694764450219582));
#36855=CARTESIAN_POINT('Ctrl Pts',(2.19890268624765,1.,-0.0694764450219582));
#36856=CARTESIAN_POINT('Ctrl Pts',(2.19777582085423,-1.,-0.0701143536325491));
#36857=CARTESIAN_POINT('Ctrl Pts',(2.19777582085423,1.,-0.0701143536325491));
#36858=CARTESIAN_POINT('Ctrl Pts',(2.19552129484002,-1.,-0.0713863779526155));
#36859=CARTESIAN_POINT('Ctrl Pts',(2.19552129484002,1.,-0.0713863779526155));
#36860=CARTESIAN_POINT('Ctrl Pts',(2.19213712013662,-1.,-0.0732830357306726));
#36861=CARTESIAN_POINT('Ctrl Pts',(2.19213712013662,1.,-0.0732830357306726));
#36862=CARTESIAN_POINT('Ctrl Pts',(2.1876201139953,-1.,-0.0757891465836149));
#36863=CARTESIAN_POINT('Ctrl Pts',(2.1876201139953,1.,-0.0757891465836149));
#36864=CARTESIAN_POINT('Ctrl Pts',(2.18196589448887,-1.,-0.0788837727685244));
#36865=CARTESIAN_POINT('Ctrl Pts',(2.18196589448887,1.,-0.0788837727685244));
#36866=CARTESIAN_POINT('Ctrl Pts',(2.176303712113,-1.,-0.0819402680872767));
#36867=CARTESIAN_POINT('Ctrl Pts',(2.176303712113,1.,-0.0819402680872767));
#36868=CARTESIAN_POINT('Ctrl Pts',(2.17063357870952,-1.,-0.0849584620835374));
#36869=CARTESIAN_POINT('Ctrl Pts',(2.17063357870952,1.,-0.0849584620835374));
#36870=CARTESIAN_POINT('Ctrl Pts',(2.16495552645014,-1.,-0.0879381291386924));
#36871=CARTESIAN_POINT('Ctrl Pts',(2.16495552645014,1.,-0.0879381291386924));
#36872=CARTESIAN_POINT('Ctrl Pts',(2.15926961544516,-1.,-0.0908789888107267));
#36873=CARTESIAN_POINT('Ctrl Pts',(2.15926961544516,1.,-0.0908789888107267));
#36874=CARTESIAN_POINT('Ctrl Pts',(2.1535759397817,-1.,-0.0937807218867645));
#36875=CARTESIAN_POINT('Ctrl Pts',(2.1535759397817,1.,-0.0937807218867645));
#36876=CARTESIAN_POINT('Ctrl Pts',(2.14787463531795,-1.,-0.096642985230546));
#36877=CARTESIAN_POINT('Ctrl Pts',(2.14787463531795,1.,-0.096642985230546));
#36878=CARTESIAN_POINT('Ctrl Pts',(2.14216588396025,-1.,-0.0994654261990917));
#36879=CARTESIAN_POINT('Ctrl Pts',(2.14216588396025,1.,-0.0994654261990917));
#36880=CARTESIAN_POINT('Ctrl Pts',(2.13644992667165,-1.,-0.102247700556101));
#36881=CARTESIAN_POINT('Ctrl Pts',(2.13644992667165,1.,-0.102247700556101));
#36882=CARTESIAN_POINT('Ctrl Pts',(2.13072704887293,-1.,-0.10498947915274));
#36883=CARTESIAN_POINT('Ctrl Pts',(2.13072704887293,1.,-0.10498947915274));
#36884=CARTESIAN_POINT('Ctrl Pts',(2.12499752307,-1.,-0.10769043523109));
#36885=CARTESIAN_POINT('Ctrl Pts',(2.12499752307,1.,-0.10769043523109));
#36886=CARTESIAN_POINT('Ctrl Pts',(2.11926155590865,-1.,-0.110350236135025));
#36887=CARTESIAN_POINT('Ctrl Pts',(2.11926155590865,1.,-0.110350236135025));
#36888=CARTESIAN_POINT('Ctrl Pts',(2.11351924490306,-1.,-0.112968534419737));
#36889=CARTESIAN_POINT('Ctrl Pts',(2.11351924490306,1.,-0.112968534419737));
#36890=CARTESIAN_POINT('Ctrl Pts',(2.10777050261309,-1.,-0.115544957687927));
#36891=CARTESIAN_POINT('Ctrl Pts',(2.10777050261309,1.,-0.115544957687927));
#36892=CARTESIAN_POINT('Ctrl Pts',(2.102015121329,-1.,-0.118079107988356));
#36893=CARTESIAN_POINT('Ctrl Pts',(2.102015121329,1.,-0.118079107988356));
#36894=CARTESIAN_POINT('Ctrl Pts',(2.0962529286773,-1.,-0.120570567965122));
#36895=CARTESIAN_POINT('Ctrl Pts',(2.0962529286773,1.,-0.120570567965122));
#36896=CARTESIAN_POINT('Ctrl Pts',(2.09048392424825,-1.,-0.123018905621083));
#36897=CARTESIAN_POINT('Ctrl Pts',(2.09048392424825,1.,-0.123018905621083));
#36898=CARTESIAN_POINT('Ctrl Pts',(2.08470840653643,-1.,-0.125423679412062));
#36899=CARTESIAN_POINT('Ctrl Pts',(2.08470840653643,1.,-0.125423679412062));
#36900=CARTESIAN_POINT('Ctrl Pts',(2.07892715110987,-1.,-0.12778444527612));
#36901=CARTESIAN_POINT('Ctrl Pts',(2.07892715110987,1.,-0.12778444527612));
#36902=CARTESIAN_POINT('Ctrl Pts',(2.07314114713063,-1.,-0.130100748328404));
#36903=CARTESIAN_POINT('Ctrl Pts',(2.07314114713063,1.,-0.130100748328404));
#36904=CARTESIAN_POINT('Ctrl Pts',(2.06735123910326,-1.,-0.132372111547711));
#36905=CARTESIAN_POINT('Ctrl Pts',(2.06735123910326,1.,-0.132372111547711));
#36906=CARTESIAN_POINT('Ctrl Pts',(2.06155781517842,-1.,-0.134598026192106));
#36907=CARTESIAN_POINT('Ctrl Pts',(2.06155781517842,1.,-0.134598026192106));
#36908=CARTESIAN_POINT('Ctrl Pts',(2.05576044414264,-1.,-0.136777941218044));
#36909=CARTESIAN_POINT('Ctrl Pts',(2.05576044414264,1.,-0.136777941218044));
#36910=CARTESIAN_POINT('Ctrl Pts',(2.04995762001328,-1.,-0.138911255368966));
#36911=CARTESIAN_POINT('Ctrl Pts',(2.04995762001328,1.,-0.138911255368966));
#36912=CARTESIAN_POINT('Ctrl Pts',(2.04414757947916,-1.,-0.140997332152546));
#36913=CARTESIAN_POINT('Ctrl Pts',(2.04414757947916,1.,-0.140997332152546));
#36914=CARTESIAN_POINT('Ctrl Pts',(2.03832911025912,-1.,-0.143035515058209));
#36915=CARTESIAN_POINT('Ctrl Pts',(2.03832911025912,1.,-0.143035515058209));
#36916=CARTESIAN_POINT('Ctrl Pts',(2.03250223739942,-1.,-0.145025140186058));
#36917=CARTESIAN_POINT('Ctrl Pts',(2.03250223739942,1.,-0.145025140186058));
#36918=CARTESIAN_POINT('Ctrl Pts',(2.02666926182017,-1.,-0.146965557332583));
#36919=CARTESIAN_POINT('Ctrl Pts',(2.02666926182017,1.,-0.146965557332583));
#36920=CARTESIAN_POINT('Ctrl Pts',(2.02083464969894,-1.,-0.148856124775337));
#36921=CARTESIAN_POINT('Ctrl Pts',(2.02083464969894,1.,-0.148856124775337));
#36922=CARTESIAN_POINT('Ctrl Pts',(2.01500291940238,-1.,-0.150696157673078));
#36923=CARTESIAN_POINT('Ctrl Pts',(2.01500291940238,1.,-0.150696157673078));
#36924=CARTESIAN_POINT('Ctrl Pts',(2.00917680318424,-1.,-0.15248488362145));
#36925=CARTESIAN_POINT('Ctrl Pts',(2.00917680318424,1.,-0.15248488362145));
#36926=CARTESIAN_POINT('Ctrl Pts',(2.00335565310543,-1.,-0.154221403049722));
#36927=CARTESIAN_POINT('Ctrl Pts',(2.00335565310543,1.,-0.154221403049722));
#36928=CARTESIAN_POINT('Ctrl Pts',(1.99753284771497,-1.,-0.155904629548784));
#36929=CARTESIAN_POINT('Ctrl Pts',(1.99753284771497,1.,-0.155904629548784));
#36930=CARTESIAN_POINT('Ctrl Pts',(1.99169810931908,-1.,-0.157533331459227));
#36931=CARTESIAN_POINT('Ctrl Pts',(1.99169810931908,1.,-0.157533331459227));
#36932=CARTESIAN_POINT('Ctrl Pts',(1.98584238283292,-1.,-0.159106226437299));
#36933=CARTESIAN_POINT('Ctrl Pts',(1.98584238283292,1.,-0.159106226437299));
#36934=CARTESIAN_POINT('Ctrl Pts',(1.97996195437559,-1.,-0.160622060784611));
#36935=CARTESIAN_POINT('Ctrl Pts',(1.97996195437559,1.,-0.160622060784611));
#36936=CARTESIAN_POINT('Ctrl Pts',(1.97406280235188,-1.,-0.162079693556289));
#36937=CARTESIAN_POINT('Ctrl Pts',(1.97406280235188,1.,-0.162079693556289));
#36938=CARTESIAN_POINT('Ctrl Pts',(1.96816512677967,-1.,-0.163478185457734));
#36939=CARTESIAN_POINT('Ctrl Pts',(1.96816512677967,1.,-0.163478185457734));
#36940=CARTESIAN_POINT('Ctrl Pts',(1.96229379940136,-1.,-0.164816568920269));
#36941=CARTESIAN_POINT('Ctrl Pts',(1.96229379940136,1.,-0.164816568920269));
#36942=CARTESIAN_POINT('Ctrl Pts',(1.9564675971873,-1.,-0.166093592002813));
#36943=CARTESIAN_POINT('Ctrl Pts',(1.9564675971873,1.,-0.166093592002813));
#36944=CARTESIAN_POINT('Ctrl Pts',(1.95069027794294,-1.,-0.167307501784476));
#36945=CARTESIAN_POINT('Ctrl Pts',(1.95069027794294,1.,-0.167307501784476));
#36946=CARTESIAN_POINT('Ctrl Pts',(1.94493757756931,-1.,-0.168455741607556));
#36947=CARTESIAN_POINT('Ctrl Pts',(1.94493757756931,1.,-0.168455741607556));
#36948=CARTESIAN_POINT('Ctrl Pts',(1.93915639211581,-1.,-0.169534904817491));
#36949=CARTESIAN_POINT('Ctrl Pts',(1.93915639211581,1.,-0.169534904817491));
#36950=CARTESIAN_POINT('Ctrl Pts',(1.93329183155539,-1.,-0.170541253116202));
#36951=CARTESIAN_POINT('Ctrl Pts',(1.93329183155539,1.,-0.170541253116202));
#36952=CARTESIAN_POINT('Ctrl Pts',(1.92731093582036,-1.,-0.171471191532988));
#36953=CARTESIAN_POINT('Ctrl Pts',(1.92731093582036,1.,-0.171471191532988));
#36954=CARTESIAN_POINT('Ctrl Pts',(1.9212233439798,-1.,-0.172321621259514));
#36955=CARTESIAN_POINT('Ctrl Pts',(1.9212233439798,1.,-0.172321621259514));
#36956=CARTESIAN_POINT('Ctrl Pts',(1.91511429159527,-1.,-0.173090695383496));
#36957=CARTESIAN_POINT('Ctrl Pts',(1.91511429159527,1.,-0.173090695383496));
#36958=CARTESIAN_POINT('Ctrl Pts',(1.90911693975267,-1.,-0.173776635257817));
#36959=CARTESIAN_POINT('Ctrl Pts',(1.90911693975267,1.,-0.173776635257817));
#36960=CARTESIAN_POINT('Ctrl Pts',(1.90335253862834,-1.,-0.174375518661085));
#36961=CARTESIAN_POINT('Ctrl Pts',(1.90335253862834,1.,-0.174375518661085));
#36962=CARTESIAN_POINT('Ctrl Pts',(1.89788101117132,-1.,-0.174879405091263));
#36963=CARTESIAN_POINT('Ctrl Pts',(1.89788101117132,1.,-0.174879405091263));
#36964=CARTESIAN_POINT('Ctrl Pts',(1.892646301985,-1.,-0.175274276190844));
#36965=CARTESIAN_POINT('Ctrl Pts',(1.892646301985,1.,-0.175274276190844));
#36966=CARTESIAN_POINT('Ctrl Pts',(1.88742606273259,-1.,-0.175538155840648));
#36967=CARTESIAN_POINT('Ctrl Pts',(1.88742606273259,1.,-0.175538155840648));
#36968=CARTESIAN_POINT('Ctrl Pts',(1.88188663145367,-1.,-0.175644148889699));
#36969=CARTESIAN_POINT('Ctrl Pts',(1.88188663145367,1.,-0.175644148889699));
#36970=CARTESIAN_POINT('Ctrl Pts',(1.87563767773588,-1.,-0.175563480746485));
#36971=CARTESIAN_POINT('Ctrl Pts',(1.87563767773588,1.,-0.175563480746485));
#36972=CARTESIAN_POINT('Ctrl Pts',(1.86828349694799,-1.,-0.175268337590758));
#36973=CARTESIAN_POINT('Ctrl Pts',(1.86828349694799,1.,-0.175268337590758));
#36974=CARTESIAN_POINT('Ctrl Pts',(1.85948367088837,-1.,-0.17473525927603));
#36975=CARTESIAN_POINT('Ctrl Pts',(1.85948367088837,1.,-0.17473525927603));
#36976=CARTESIAN_POINT('Ctrl Pts',(1.8489811319852,-1.,-0.173946627587732));
#36977=CARTESIAN_POINT('Ctrl Pts',(1.8489811319852,1.,-0.173946627587732));
#36978=CARTESIAN_POINT('Ctrl Pts',(1.83658380527692,-1.,-0.1728894428919));
#36979=CARTESIAN_POINT('Ctrl Pts',(1.83658380527692,1.,-0.1728894428919));
#36980=CARTESIAN_POINT('Ctrl Pts',(1.82215766811545,-1.,-0.171554770204119));
#36981=CARTESIAN_POINT('Ctrl Pts',(1.82215766811545,1.,-0.171554770204119));
#36982=CARTESIAN_POINT('Ctrl Pts',(1.80561530629706,-1.,-0.169936923904608));
#36983=CARTESIAN_POINT('Ctrl Pts',(1.80561530629706,1.,-0.169936923904608));
#36984=CARTESIAN_POINT('Ctrl Pts',(1.7869064998507,-1.,-0.168032772805197));
#36985=CARTESIAN_POINT('Ctrl Pts',(1.7869064998507,1.,-0.168032772805197));
#36986=CARTESIAN_POINT('Ctrl Pts',(1.77018771684844,-1.,-0.1662793551464));
#36987=CARTESIAN_POINT('Ctrl Pts',(1.77018771684844,1.,-0.1662793551464));
#36988=CARTESIAN_POINT('Ctrl Pts',(1.75666056638427,-1.,-0.164834765707159));
#36989=CARTESIAN_POINT('Ctrl Pts',(1.75666056638427,1.,-0.164834765707159));
#36990=CARTESIAN_POINT('Ctrl Pts',(1.7472034950333,-1.,-0.163814161002002));
#36991=CARTESIAN_POINT('Ctrl Pts',(1.7472034950333,1.,-0.163814161002002));
#36992=CARTESIAN_POINT('Ctrl Pts',(1.74236521665491,-1.,-0.163289472382896));
#36993=CARTESIAN_POINT('Ctrl Pts',(1.74236521665491,1.,-0.163289472382896));
#36994=CARTESIAN_POINT('',(2.19890268624765,1.,-0.0694764450219582));
#36995=CARTESIAN_POINT('Ctrl Pts',(2.19890268624765,1.,-0.0694764450219582));
#36996=CARTESIAN_POINT('Ctrl Pts',(2.19777582085423,1.,-0.0701143536325491));
#36997=CARTESIAN_POINT('Ctrl Pts',(2.19552129484002,1.,-0.0713863779526155));
#36998=CARTESIAN_POINT('Ctrl Pts',(2.19213712013662,1.,-0.0732830357306726));
#36999=CARTESIAN_POINT('Ctrl Pts',(2.1876201139953,1.,-0.0757891465836149));
#37000=CARTESIAN_POINT('Ctrl Pts',(2.18196589448887,1.,-0.0788837727685244));
#37001=CARTESIAN_POINT('Ctrl Pts',(2.176303712113,1.,-0.0819402680872767));
#37002=CARTESIAN_POINT('Ctrl Pts',(2.17063357870952,1.,-0.0849584620835374));
#37003=CARTESIAN_POINT('Ctrl Pts',(2.16495552645014,1.,-0.0879381291386924));
#37004=CARTESIAN_POINT('Ctrl Pts',(2.15926961544516,1.,-0.0908789888107267));
#37005=CARTESIAN_POINT('Ctrl Pts',(2.1535759397817,1.,-0.0937807218867645));
#37006=CARTESIAN_POINT('Ctrl Pts',(2.14787463531795,1.,-0.096642985230546));
#37007=CARTESIAN_POINT('Ctrl Pts',(2.14216588396025,1.,-0.0994654261990917));
#37008=CARTESIAN_POINT('Ctrl Pts',(2.13644992667165,1.,-0.102247700556101));
#37009=CARTESIAN_POINT('Ctrl Pts',(2.13072704887293,1.,-0.10498947915274));
#37010=CARTESIAN_POINT('Ctrl Pts',(2.12499752307,1.,-0.10769043523109));
#37011=CARTESIAN_POINT('Ctrl Pts',(2.11926155590865,1.,-0.110350236135025));
#37012=CARTESIAN_POINT('Ctrl Pts',(2.11351924490306,1.,-0.112968534419737));
#37013=CARTESIAN_POINT('Ctrl Pts',(2.10777050261309,1.,-0.115544957687927));
#37014=CARTESIAN_POINT('Ctrl Pts',(2.102015121329,1.,-0.118079107988356));
#37015=CARTESIAN_POINT('Ctrl Pts',(2.0962529286773,1.,-0.120570567965122));
#37016=CARTESIAN_POINT('Ctrl Pts',(2.09048392424825,1.,-0.123018905621083));
#37017=CARTESIAN_POINT('Ctrl Pts',(2.08470840653643,1.,-0.125423679412062));
#37018=CARTESIAN_POINT('Ctrl Pts',(2.07892715110987,1.,-0.12778444527612));
#37019=CARTESIAN_POINT('Ctrl Pts',(2.07314114713063,1.,-0.130100748328404));
#37020=CARTESIAN_POINT('Ctrl Pts',(2.06735123910326,1.,-0.132372111547711));
#37021=CARTESIAN_POINT('Ctrl Pts',(2.06155781517842,1.,-0.134598026192106));
#37022=CARTESIAN_POINT('Ctrl Pts',(2.05576044414264,1.,-0.136777941218044));
#37023=CARTESIAN_POINT('Ctrl Pts',(2.04995762001328,1.,-0.138911255368966));
#37024=CARTESIAN_POINT('Ctrl Pts',(2.04414757947916,1.,-0.140997332152546));
#37025=CARTESIAN_POINT('Ctrl Pts',(2.03832911025912,1.,-0.143035515058209));
#37026=CARTESIAN_POINT('Ctrl Pts',(2.03250223739942,1.,-0.145025140186058));
#37027=CARTESIAN_POINT('Ctrl Pts',(2.02666926182017,1.,-0.146965557332583));
#37028=CARTESIAN_POINT('Ctrl Pts',(2.02083464969894,1.,-0.148856124775337));
#37029=CARTESIAN_POINT('Ctrl Pts',(2.01500291940238,1.,-0.150696157673078));
#37030=CARTESIAN_POINT('Ctrl Pts',(2.00917680318424,1.,-0.15248488362145));
#37031=CARTESIAN_POINT('Ctrl Pts',(2.00335565310543,1.,-0.154221403049722));
#37032=CARTESIAN_POINT('Ctrl Pts',(1.99753284771497,1.,-0.155904629548784));
#37033=CARTESIAN_POINT('Ctrl Pts',(1.99169810931908,1.,-0.157533331459227));
#37034=CARTESIAN_POINT('Ctrl Pts',(1.98584238283292,1.,-0.159106226437299));
#37035=CARTESIAN_POINT('Ctrl Pts',(1.97996195437559,1.,-0.160622060784611));
#37036=CARTESIAN_POINT('Ctrl Pts',(1.97406280235188,1.,-0.162079693556289));
#37037=CARTESIAN_POINT('Ctrl Pts',(1.96816512677967,1.,-0.163478185457734));
#37038=CARTESIAN_POINT('Ctrl Pts',(1.96229379940136,1.,-0.164816568920269));
#37039=CARTESIAN_POINT('Ctrl Pts',(1.9564675971873,1.,-0.166093592002813));
#37040=CARTESIAN_POINT('Ctrl Pts',(1.95069027794294,1.,-0.167307501784476));
#37041=CARTESIAN_POINT('Ctrl Pts',(1.94493757756931,1.,-0.168455741607556));
#37042=CARTESIAN_POINT('Ctrl Pts',(1.93915639211581,1.,-0.169534904817491));
#37043=CARTESIAN_POINT('Ctrl Pts',(1.93329183155539,1.,-0.170541253116202));
#37044=CARTESIAN_POINT('Ctrl Pts',(1.92731093582036,1.,-0.171471191532988));
#37045=CARTESIAN_POINT('Ctrl Pts',(1.9212233439798,1.,-0.172321621259514));
#37046=CARTESIAN_POINT('Ctrl Pts',(1.91511429159527,1.,-0.173090695383496));
#37047=CARTESIAN_POINT('Ctrl Pts',(1.90911693975267,1.,-0.173776635257817));
#37048=CARTESIAN_POINT('Ctrl Pts',(1.90335253862834,1.,-0.174375518661085));
#37049=CARTESIAN_POINT('Ctrl Pts',(1.89788101117132,1.,-0.174879405091263));
#37050=CARTESIAN_POINT('Ctrl Pts',(1.892646301985,1.,-0.175274276190844));
#37051=CARTESIAN_POINT('Ctrl Pts',(1.88742606273259,1.,-0.175538155840648));
#37052=CARTESIAN_POINT('Ctrl Pts',(1.88188663145367,1.,-0.175644148889699));
#37053=CARTESIAN_POINT('Ctrl Pts',(1.87563767773588,1.,-0.175563480746485));
#37054=CARTESIAN_POINT('Ctrl Pts',(1.86828349694799,1.,-0.175268337590758));
#37055=CARTESIAN_POINT('Ctrl Pts',(1.85948367088837,1.,-0.17473525927603));
#37056=CARTESIAN_POINT('Ctrl Pts',(1.8489811319852,1.,-0.173946627587732));
#37057=CARTESIAN_POINT('Ctrl Pts',(1.83658380527692,1.,-0.1728894428919));
#37058=CARTESIAN_POINT('Ctrl Pts',(1.82215766811545,1.,-0.171554770204119));
#37059=CARTESIAN_POINT('Ctrl Pts',(1.80561530629706,1.,-0.169936923904608));
#37060=CARTESIAN_POINT('Ctrl Pts',(1.7869064998507,1.,-0.168032772805197));
#37061=CARTESIAN_POINT('Ctrl Pts',(1.77018771684844,1.,-0.1662793551464));
#37062=CARTESIAN_POINT('Ctrl Pts',(1.75666056638427,1.,-0.164834765707159));
#37063=CARTESIAN_POINT('Ctrl Pts',(1.7472034950333,1.,-0.163814161002002));
#37064=CARTESIAN_POINT('Ctrl Pts',(1.74236521665491,1.,-0.163289472382896));
#37065=CARTESIAN_POINT('',(2.19890268624765,0.,-0.0694764450219582));
#37066=CARTESIAN_POINT('Origin',(2.19890268624765,0.,0.0694764450219582));
#37067=CARTESIAN_POINT('',(2.19890268624765,1.,0.0694764450219582));
#37068=CARTESIAN_POINT('',(2.19890268624765,1.,-0.0694764450219582));
#37069=CARTESIAN_POINT('',(2.19890268624765,0.,0.0694764450219582));
#37070=CARTESIAN_POINT('Ctrl Pts',(1.74236521665491,-1.,0.163289472382896));
#37071=CARTESIAN_POINT('Ctrl Pts',(1.74236521665491,1.,0.163289472382896));
#37072=CARTESIAN_POINT('Ctrl Pts',(1.74720349503904,-1.,0.163814161002474));
#37073=CARTESIAN_POINT('Ctrl Pts',(1.74720349503904,1.,0.163814161002474));
#37074=CARTESIAN_POINT('Ctrl Pts',(1.75666056640041,-1.,0.164834765708484));
#37075=CARTESIAN_POINT('Ctrl Pts',(1.75666056640041,1.,0.164834765708484));
#37076=CARTESIAN_POINT('Ctrl Pts',(1.77018771687692,-1.,0.166279355148738));
#37077=CARTESIAN_POINT('Ctrl Pts',(1.77018771687692,1.,0.166279355148738));
#37078=CARTESIAN_POINT('Ctrl Pts',(1.78690649988931,-1.,0.16803277280837));
#37079=CARTESIAN_POINT('Ctrl Pts',(1.78690649988931,1.,0.16803277280837));
#37080=CARTESIAN_POINT('Ctrl Pts',(1.80561530633924,-1.,0.169936923908078));
#37081=CARTESIAN_POINT('Ctrl Pts',(1.80561530633924,1.,0.169936923908078));
#37082=CARTESIAN_POINT('Ctrl Pts',(1.82215766815414,-1.,0.171554770207306));
#37083=CARTESIAN_POINT('Ctrl Pts',(1.82215766815414,1.,0.171554770207306));
#37084=CARTESIAN_POINT('Ctrl Pts',(1.83658380530747,-1.,0.17288944289442));
#37085=CARTESIAN_POINT('Ctrl Pts',(1.83658380530747,1.,0.17288944289442));
#37086=CARTESIAN_POINT('Ctrl Pts',(1.84898113200543,-1.,0.173946627589401));
#37087=CARTESIAN_POINT('Ctrl Pts',(1.84898113200543,1.,0.173946627589401));
#37088=CARTESIAN_POINT('Ctrl Pts',(1.85948367089838,-1.,0.174735259276856));
#37089=CARTESIAN_POINT('Ctrl Pts',(1.85948367089838,1.,0.174735259276856));
#37090=CARTESIAN_POINT('Ctrl Pts',(1.86828349694972,-1.,0.1752683375909));
#37091=CARTESIAN_POINT('Ctrl Pts',(1.86828349694972,1.,0.1752683375909));
#37092=CARTESIAN_POINT('Ctrl Pts',(1.87563767773249,-1.,0.175563480746205));
#37093=CARTESIAN_POINT('Ctrl Pts',(1.87563767773249,1.,0.175563480746205));
#37094=CARTESIAN_POINT('Ctrl Pts',(1.88188663144846,-1.,0.175644148889271));
#37095=CARTESIAN_POINT('Ctrl Pts',(1.88188663144846,1.,0.175644148889271));
#37096=CARTESIAN_POINT('Ctrl Pts',(1.88742606272818,-1.,0.175538155840286));
#37097=CARTESIAN_POINT('Ctrl Pts',(1.88742606272818,1.,0.175538155840286));
#37098=CARTESIAN_POINT('Ctrl Pts',(1.89264630198279,-1.,0.175274276190664));
#37099=CARTESIAN_POINT('Ctrl Pts',(1.89264630198279,1.,0.175274276190664));
#37100=CARTESIAN_POINT('Ctrl Pts',(1.89788101117148,-1.,0.174879405091277));
#37101=CARTESIAN_POINT('Ctrl Pts',(1.89788101117148,1.,0.174879405091277));
#37102=CARTESIAN_POINT('Ctrl Pts',(1.90335253863003,-1.,0.174375518661222));
#37103=CARTESIAN_POINT('Ctrl Pts',(1.90335253863003,1.,0.174375518661222));
#37104=CARTESIAN_POINT('Ctrl Pts',(1.90911693975475,-1.,0.173776635257983));
#37105=CARTESIAN_POINT('Ctrl Pts',(1.90911693975475,1.,0.173776635257983));
#37106=CARTESIAN_POINT('Ctrl Pts',(1.91511429159681,-1.,0.173090695383619));
#37107=CARTESIAN_POINT('Ctrl Pts',(1.91511429159681,1.,0.173090695383619));
#37108=CARTESIAN_POINT('Ctrl Pts',(1.92122334398034,-1.,0.172321621259556));
#37109=CARTESIAN_POINT('Ctrl Pts',(1.92122334398034,1.,0.172321621259556));
#37110=CARTESIAN_POINT('Ctrl Pts',(1.92731093582,-1.,0.17147119153296));
#37111=CARTESIAN_POINT('Ctrl Pts',(1.92731093582,1.,0.17147119153296));
#37112=CARTESIAN_POINT('Ctrl Pts',(1.93329183155455,-1.,0.170541253116136));
#37113=CARTESIAN_POINT('Ctrl Pts',(1.93329183155455,1.,0.170541253116136));
#37114=CARTESIAN_POINT('Ctrl Pts',(1.93915639211497,-1.,0.169534904817425));
#37115=CARTESIAN_POINT('Ctrl Pts',(1.93915639211497,1.,0.169534904817425));
#37116=CARTESIAN_POINT('Ctrl Pts',(1.94493757756879,-1.,0.168455741607515));
#37117=CARTESIAN_POINT('Ctrl Pts',(1.94493757756879,1.,0.168455741607515));
#37118=CARTESIAN_POINT('Ctrl Pts',(1.95069027794286,-1.,0.167307501784469));
#37119=CARTESIAN_POINT('Ctrl Pts',(1.95069027794286,1.,0.167307501784469));
#37120=CARTESIAN_POINT('Ctrl Pts',(1.95646759718755,-1.,0.166093592002832));
#37121=CARTESIAN_POINT('Ctrl Pts',(1.95646759718755,1.,0.166093592002832));
#37122=CARTESIAN_POINT('Ctrl Pts',(1.96229379940174,-1.,0.1648165689203));
#37123=CARTESIAN_POINT('Ctrl Pts',(1.96229379940174,1.,0.1648165689203));
#37124=CARTESIAN_POINT('Ctrl Pts',(1.96816512678,-1.,0.16347818545776));
#37125=CARTESIAN_POINT('Ctrl Pts',(1.96816512678,1.,0.16347818545776));
#37126=CARTESIAN_POINT('Ctrl Pts',(1.97406280235204,-1.,0.162079693556302));
#37127=CARTESIAN_POINT('Ctrl Pts',(1.97406280235204,1.,0.162079693556302));
#37128=CARTESIAN_POINT('Ctrl Pts',(1.97996195437557,-1.,0.16062206078461));
#37129=CARTESIAN_POINT('Ctrl Pts',(1.97996195437557,1.,0.16062206078461));
#37130=CARTESIAN_POINT('Ctrl Pts',(1.98584238283279,-1.,0.159106226437288));
#37131=CARTESIAN_POINT('Ctrl Pts',(1.98584238283279,1.,0.159106226437288));
#37132=CARTESIAN_POINT('Ctrl Pts',(1.99169810931893,-1.,0.157533331459215));
#37133=CARTESIAN_POINT('Ctrl Pts',(1.99169810931893,1.,0.157533331459215));
#37134=CARTESIAN_POINT('Ctrl Pts',(1.99753284771487,-1.,0.155904629548774));
#37135=CARTESIAN_POINT('Ctrl Pts',(1.99753284771487,1.,0.155904629548774));
#37136=CARTESIAN_POINT('Ctrl Pts',(2.00335565310539,-1.,0.154221403049719));
#37137=CARTESIAN_POINT('Ctrl Pts',(2.00335565310539,1.,0.154221403049719));
#37138=CARTESIAN_POINT('Ctrl Pts',(2.00917680318426,-1.,0.152484883621452));
#37139=CARTESIAN_POINT('Ctrl Pts',(2.00917680318426,1.,0.152484883621452));
#37140=CARTESIAN_POINT('Ctrl Pts',(2.01500291940243,-1.,0.150696157673084));
#37141=CARTESIAN_POINT('Ctrl Pts',(2.01500291940243,1.,0.150696157673084));
#37142=CARTESIAN_POINT('Ctrl Pts',(2.02083464969897,-1.,0.148856124775342));
#37143=CARTESIAN_POINT('Ctrl Pts',(2.02083464969897,1.,0.148856124775342));
#37144=CARTESIAN_POINT('Ctrl Pts',(2.02666926182017,-1.,0.146965557332586));
#37145=CARTESIAN_POINT('Ctrl Pts',(2.02666926182017,1.,0.146965557332586));
#37146=CARTESIAN_POINT('Ctrl Pts',(2.03250223739941,-1.,0.145025140186058));
#37147=CARTESIAN_POINT('Ctrl Pts',(2.03250223739941,1.,0.145025140186058));
#37148=CARTESIAN_POINT('Ctrl Pts',(2.03832911025913,-1.,0.143035515058208));
#37149=CARTESIAN_POINT('Ctrl Pts',(2.03832911025913,1.,0.143035515058208));
#37150=CARTESIAN_POINT('Ctrl Pts',(2.04414757947919,-1.,0.140997332152545));
#37151=CARTESIAN_POINT('Ctrl Pts',(2.04414757947919,1.,0.140997332152545));
#37152=CARTESIAN_POINT('Ctrl Pts',(2.04995762001333,-1.,0.138911255368966));
#37153=CARTESIAN_POINT('Ctrl Pts',(2.04995762001333,1.,0.138911255368966));
#37154=CARTESIAN_POINT('Ctrl Pts',(2.0557604441427,-1.,0.136777941218044));
#37155=CARTESIAN_POINT('Ctrl Pts',(2.0557604441427,1.,0.136777941218044));
#37156=CARTESIAN_POINT('Ctrl Pts',(2.06155781517844,-1.,0.134598026192107));
#37157=CARTESIAN_POINT('Ctrl Pts',(2.06155781517844,1.,0.134598026192107));
#37158=CARTESIAN_POINT('Ctrl Pts',(2.06735123910319,-1.,0.132372111547709));
#37159=CARTESIAN_POINT('Ctrl Pts',(2.06735123910319,1.,0.132372111547709));
#37160=CARTESIAN_POINT('Ctrl Pts',(2.07314114713047,-1.,0.1301007483284));
#37161=CARTESIAN_POINT('Ctrl Pts',(2.07314114713047,1.,0.1301007483284));
#37162=CARTESIAN_POINT('Ctrl Pts',(2.07892715110967,-1.,0.127784445276116));
#37163=CARTESIAN_POINT('Ctrl Pts',(2.07892715110967,1.,0.127784445276116));
#37164=CARTESIAN_POINT('Ctrl Pts',(2.08470840653628,-1.,0.125423679412058));
#37165=CARTESIAN_POINT('Ctrl Pts',(2.08470840653628,1.,0.125423679412058));
#37166=CARTESIAN_POINT('Ctrl Pts',(2.09048392424826,-1.,0.123018905621083));
#37167=CARTESIAN_POINT('Ctrl Pts',(2.09048392424826,1.,0.123018905621083));
#37168=CARTESIAN_POINT('Ctrl Pts',(2.09625292867756,-1.,0.120570567965129));
#37169=CARTESIAN_POINT('Ctrl Pts',(2.09625292867756,1.,0.120570567965129));
#37170=CARTESIAN_POINT('Ctrl Pts',(2.10201512132945,-1.,0.118079107988368));
#37171=CARTESIAN_POINT('Ctrl Pts',(2.10201512132945,1.,0.118079107988368));
#37172=CARTESIAN_POINT('Ctrl Pts',(2.10777050261359,-1.,0.11554495768794));
#37173=CARTESIAN_POINT('Ctrl Pts',(2.10777050261359,1.,0.11554495768794));
#37174=CARTESIAN_POINT('Ctrl Pts',(2.11351924490335,-1.,0.112968534419746));
#37175=CARTESIAN_POINT('Ctrl Pts',(2.11351924490335,1.,0.112968534419746));
#37176=CARTESIAN_POINT('Ctrl Pts',(2.11926155590849,-1.,0.11035023613502));
#37177=CARTESIAN_POINT('Ctrl Pts',(2.11926155590849,1.,0.11035023613502));
#37178=CARTESIAN_POINT('Ctrl Pts',(2.12499752306927,-1.,0.107690435231068));
#37179=CARTESIAN_POINT('Ctrl Pts',(2.12499752306927,1.,0.107690435231068));
#37180=CARTESIAN_POINT('Ctrl Pts',(2.1307270488718,-1.,0.104989479152703));
#37181=CARTESIAN_POINT('Ctrl Pts',(2.1307270488718,1.,0.104989479152703));
#37182=CARTESIAN_POINT('Ctrl Pts',(2.13644992667052,-1.,0.102247700556063));
#37183=CARTESIAN_POINT('Ctrl Pts',(2.13644992667052,1.,0.102247700556063));
#37184=CARTESIAN_POINT('Ctrl Pts',(2.14216588395974,-1.,0.0994654261990741));
#37185=CARTESIAN_POINT('Ctrl Pts',(2.14216588395974,1.,0.0994654261990741));
#37186=CARTESIAN_POINT('Ctrl Pts',(2.14787463531864,-1.,0.0966429852305688));
#37187=CARTESIAN_POINT('Ctrl Pts',(2.14787463531864,1.,0.0966429852305688));
#37188=CARTESIAN_POINT('Ctrl Pts',(2.15357593978377,-1.,0.0937807218868344));
#37189=CARTESIAN_POINT('Ctrl Pts',(2.15357593978377,1.,0.0937807218868344));
#37190=CARTESIAN_POINT('Ctrl Pts',(2.15926961544808,-1.,0.0908789888108265));
#37191=CARTESIAN_POINT('Ctrl Pts',(2.15926961544808,1.,0.0908789888108265));
#37192=CARTESIAN_POINT('Ctrl Pts',(2.16495552645275,-1.,0.0879381291387821));
#37193=CARTESIAN_POINT('Ctrl Pts',(2.16495552645275,1.,0.0879381291387821));
#37194=CARTESIAN_POINT('Ctrl Pts',(2.17063357871031,-1.,0.0849584620835642));
#37195=CARTESIAN_POINT('Ctrl Pts',(2.17063357871031,1.,0.0849584620835642));
#37196=CARTESIAN_POINT('Ctrl Pts',(2.1763037121106,-1.,0.0819402680871938));
#37197=CARTESIAN_POINT('Ctrl Pts',(2.1763037121106,1.,0.0819402680871938));
#37198=CARTESIAN_POINT('Ctrl Pts',(2.18196589448304,-1.,0.0788837727683226));
#37199=CARTESIAN_POINT('Ctrl Pts',(2.18196589448304,1.,0.0788837727683226));
#37200=CARTESIAN_POINT('Ctrl Pts',(2.1876201139874,-1.,0.075789146583341));
#37201=CARTESIAN_POINT('Ctrl Pts',(2.1876201139874,1.,0.075789146583341));
#37202=CARTESIAN_POINT('Ctrl Pts',(2.19213712012956,-1.,0.0732830357304275));
#37203=CARTESIAN_POINT('Ctrl Pts',(2.19213712012956,1.,0.0732830357304275));
#37204=CARTESIAN_POINT('Ctrl Pts',(2.19552129483562,-1.,0.0713863779524626));
#37205=CARTESIAN_POINT('Ctrl Pts',(2.19552129483562,1.,0.0713863779524626));
#37206=CARTESIAN_POINT('Ctrl Pts',(2.19777582085261,-1.,0.0701143536324925));
#37207=CARTESIAN_POINT('Ctrl Pts',(2.19777582085261,1.,0.0701143536324925));
#37208=CARTESIAN_POINT('Ctrl Pts',(2.19890268624765,-1.,0.0694764450219582));
#37209=CARTESIAN_POINT('Ctrl Pts',(2.19890268624765,1.,0.0694764450219582));
#37210=CARTESIAN_POINT('',(1.74236521665491,1.,0.163289472382896));
#37211=CARTESIAN_POINT('Ctrl Pts',(1.74236521665491,1.,0.163289472382896));
#37212=CARTESIAN_POINT('Ctrl Pts',(1.74720349503904,1.,0.163814161002474));
#37213=CARTESIAN_POINT('Ctrl Pts',(1.75666056640041,1.,0.164834765708484));
#37214=CARTESIAN_POINT('Ctrl Pts',(1.77018771687692,1.,0.166279355148738));
#37215=CARTESIAN_POINT('Ctrl Pts',(1.78690649988931,1.,0.16803277280837));
#37216=CARTESIAN_POINT('Ctrl Pts',(1.80561530633924,1.,0.169936923908078));
#37217=CARTESIAN_POINT('Ctrl Pts',(1.82215766815414,1.,0.171554770207306));
#37218=CARTESIAN_POINT('Ctrl Pts',(1.83658380530747,1.,0.17288944289442));
#37219=CARTESIAN_POINT('Ctrl Pts',(1.84898113200543,1.,0.173946627589401));
#37220=CARTESIAN_POINT('Ctrl Pts',(1.85948367089838,1.,0.174735259276856));
#37221=CARTESIAN_POINT('Ctrl Pts',(1.86828349694972,1.,0.1752683375909));
#37222=CARTESIAN_POINT('Ctrl Pts',(1.87563767773249,1.,0.175563480746205));
#37223=CARTESIAN_POINT('Ctrl Pts',(1.88188663144846,1.,0.175644148889271));
#37224=CARTESIAN_POINT('Ctrl Pts',(1.88742606272818,1.,0.175538155840286));
#37225=CARTESIAN_POINT('Ctrl Pts',(1.89264630198279,1.,0.175274276190664));
#37226=CARTESIAN_POINT('Ctrl Pts',(1.89788101117148,1.,0.174879405091277));
#37227=CARTESIAN_POINT('Ctrl Pts',(1.90335253863003,1.,0.174375518661222));
#37228=CARTESIAN_POINT('Ctrl Pts',(1.90911693975475,1.,0.173776635257983));
#37229=CARTESIAN_POINT('Ctrl Pts',(1.91511429159681,1.,0.173090695383619));
#37230=CARTESIAN_POINT('Ctrl Pts',(1.92122334398034,1.,0.172321621259556));
#37231=CARTESIAN_POINT('Ctrl Pts',(1.92731093582,1.,0.17147119153296));
#37232=CARTESIAN_POINT('Ctrl Pts',(1.93329183155455,1.,0.170541253116136));
#37233=CARTESIAN_POINT('Ctrl Pts',(1.93915639211497,1.,0.169534904817425));
#37234=CARTESIAN_POINT('Ctrl Pts',(1.94493757756879,1.,0.168455741607515));
#37235=CARTESIAN_POINT('Ctrl Pts',(1.95069027794286,1.,0.167307501784469));
#37236=CARTESIAN_POINT('Ctrl Pts',(1.95646759718755,1.,0.166093592002832));
#37237=CARTESIAN_POINT('Ctrl Pts',(1.96229379940174,1.,0.1648165689203));
#37238=CARTESIAN_POINT('Ctrl Pts',(1.96816512678,1.,0.16347818545776));
#37239=CARTESIAN_POINT('Ctrl Pts',(1.97406280235204,1.,0.162079693556302));
#37240=CARTESIAN_POINT('Ctrl Pts',(1.97996195437557,1.,0.16062206078461));
#37241=CARTESIAN_POINT('Ctrl Pts',(1.98584238283279,1.,0.159106226437288));
#37242=CARTESIAN_POINT('Ctrl Pts',(1.99169810931893,1.,0.157533331459215));
#37243=CARTESIAN_POINT('Ctrl Pts',(1.99753284771487,1.,0.155904629548774));
#37244=CARTESIAN_POINT('Ctrl Pts',(2.00335565310539,1.,0.154221403049719));
#37245=CARTESIAN_POINT('Ctrl Pts',(2.00917680318426,1.,0.152484883621452));
#37246=CARTESIAN_POINT('Ctrl Pts',(2.01500291940243,1.,0.150696157673084));
#37247=CARTESIAN_POINT('Ctrl Pts',(2.02083464969897,1.,0.148856124775342));
#37248=CARTESIAN_POINT('Ctrl Pts',(2.02666926182017,1.,0.146965557332586));
#37249=CARTESIAN_POINT('Ctrl Pts',(2.03250223739941,1.,0.145025140186058));
#37250=CARTESIAN_POINT('Ctrl Pts',(2.03832911025913,1.,0.143035515058208));
#37251=CARTESIAN_POINT('Ctrl Pts',(2.04414757947919,1.,0.140997332152545));
#37252=CARTESIAN_POINT('Ctrl Pts',(2.04995762001333,1.,0.138911255368966));
#37253=CARTESIAN_POINT('Ctrl Pts',(2.0557604441427,1.,0.136777941218044));
#37254=CARTESIAN_POINT('Ctrl Pts',(2.06155781517844,1.,0.134598026192107));
#37255=CARTESIAN_POINT('Ctrl Pts',(2.06735123910319,1.,0.132372111547709));
#37256=CARTESIAN_POINT('Ctrl Pts',(2.07314114713047,1.,0.1301007483284));
#37257=CARTESIAN_POINT('Ctrl Pts',(2.07892715110967,1.,0.127784445276116));
#37258=CARTESIAN_POINT('Ctrl Pts',(2.08470840653628,1.,0.125423679412058));
#37259=CARTESIAN_POINT('Ctrl Pts',(2.09048392424826,1.,0.123018905621083));
#37260=CARTESIAN_POINT('Ctrl Pts',(2.09625292867756,1.,0.120570567965129));
#37261=CARTESIAN_POINT('Ctrl Pts',(2.10201512132945,1.,0.118079107988368));
#37262=CARTESIAN_POINT('Ctrl Pts',(2.10777050261359,1.,0.11554495768794));
#37263=CARTESIAN_POINT('Ctrl Pts',(2.11351924490335,1.,0.112968534419746));
#37264=CARTESIAN_POINT('Ctrl Pts',(2.11926155590849,1.,0.11035023613502));
#37265=CARTESIAN_POINT('Ctrl Pts',(2.12499752306927,1.,0.107690435231068));
#37266=CARTESIAN_POINT('Ctrl Pts',(2.1307270488718,1.,0.104989479152703));
#37267=CARTESIAN_POINT('Ctrl Pts',(2.13644992667052,1.,0.102247700556063));
#37268=CARTESIAN_POINT('Ctrl Pts',(2.14216588395974,1.,0.0994654261990741));
#37269=CARTESIAN_POINT('Ctrl Pts',(2.14787463531864,1.,0.0966429852305688));
#37270=CARTESIAN_POINT('Ctrl Pts',(2.15357593978377,1.,0.0937807218868344));
#37271=CARTESIAN_POINT('Ctrl Pts',(2.15926961544808,1.,0.0908789888108265));
#37272=CARTESIAN_POINT('Ctrl Pts',(2.16495552645275,1.,0.0879381291387821));
#37273=CARTESIAN_POINT('Ctrl Pts',(2.17063357871031,1.,0.0849584620835642));
#37274=CARTESIAN_POINT('Ctrl Pts',(2.1763037121106,1.,0.0819402680871938));
#37275=CARTESIAN_POINT('Ctrl Pts',(2.18196589448304,1.,0.0788837727683226));
#37276=CARTESIAN_POINT('Ctrl Pts',(2.1876201139874,1.,0.075789146583341));
#37277=CARTESIAN_POINT('Ctrl Pts',(2.19213712012956,1.,0.0732830357304275));
#37278=CARTESIAN_POINT('Ctrl Pts',(2.19552129483562,1.,0.0713863779524626));
#37279=CARTESIAN_POINT('Ctrl Pts',(2.19777582085261,1.,0.0701143536324925));
#37280=CARTESIAN_POINT('Ctrl Pts',(2.19890268624765,1.,0.0694764450219582));
#37281=CARTESIAN_POINT('',(1.74236521665491,0.,0.163289472382896));
#37282=CARTESIAN_POINT('Origin',(0.,1.,0.));
#37283=CARTESIAN_POINT('Origin',(0.,1.,0.));
#37284=CARTESIAN_POINT('Origin',(0.,0.,0.));
#37285=CARTESIAN_POINT('',(0.,0.,0.));
#37286=CARTESIAN_POINT('Origin',(0.7,0.,0.25));
#37287=CARTESIAN_POINT('',(0.7,0.16,0.4));
#37288=CARTESIAN_POINT('',(0.7,0.2,0.36));
#37289=CARTESIAN_POINT('',(0.7,0.1675,0.3925));
#37290=CARTESIAN_POINT('',(0.7,-0.16,0.4));
#37291=CARTESIAN_POINT('',(0.7,0.,0.4));
#37292=CARTESIAN_POINT('',(0.7,-0.2,0.36));
#37293=CARTESIAN_POINT('',(0.7,-0.1675,0.3925));
#37294=CARTESIAN_POINT('',(0.7,-0.2,0.04));
#37295=CARTESIAN_POINT('',(0.7,-0.2,0.125));
#37296=CARTESIAN_POINT('',(0.7,-0.16,0.));
#37297=CARTESIAN_POINT('',(0.7,-0.1925,0.0325));
#37298=CARTESIAN_POINT('',(0.7,0.16,0.));
#37299=CARTESIAN_POINT('',(0.7,0.,0.));
#37300=CARTESIAN_POINT('',(0.7,0.2,0.04));
#37301=CARTESIAN_POINT('',(0.7,0.1925,0.0325));
#37302=CARTESIAN_POINT('',(0.7,0.2,0.125));
#37303=CARTESIAN_POINT('Origin',(-0.4,-0.18,0.02));
#37304=CARTESIAN_POINT('',(-0.7,-0.2,0.04));
#37305=CARTESIAN_POINT('',(-0.4,-0.2,0.04));
#37306=CARTESIAN_POINT('',(-0.7,-0.16,0.));
#37307=CARTESIAN_POINT('',(-0.7,-0.1925,0.0325));
#37308=CARTESIAN_POINT('',(-0.4,-0.16,0.));
#37309=CARTESIAN_POINT('Origin',(-0.8,-0.2,0.));
#37310=CARTESIAN_POINT('',(-0.7,-0.2,0.36));
#37311=CARTESIAN_POINT('',(-0.4,-0.2,0.36));
#37312=CARTESIAN_POINT('',(-0.7,-0.2,0.125));
#37313=CARTESIAN_POINT('Origin',(-0.4,-0.18,0.38));
#37314=CARTESIAN_POINT('',(-0.7,-0.16,0.4));
#37315=CARTESIAN_POINT('',(-0.4,-0.16,0.4));
#37316=CARTESIAN_POINT('',(-0.7,-0.1675,0.3925));
#37317=CARTESIAN_POINT('Origin',(0.,0.,0.4));
#37318=CARTESIAN_POINT('',(-0.7,0.16,0.4));
#37319=CARTESIAN_POINT('',(0.4,0.16,0.4));
#37320=CARTESIAN_POINT('',(-0.7,0.,0.4));
#37321=CARTESIAN_POINT('Origin',(-0.7,0.,0.25));
#37322=CARTESIAN_POINT('',(-0.7,0.2,0.36));
#37323=CARTESIAN_POINT('',(-0.7,0.1675,0.3925));
#37324=CARTESIAN_POINT('',(-0.7,0.2,0.04));
#37325=CARTESIAN_POINT('',(-0.7,0.2,0.125));
#37326=CARTESIAN_POINT('',(-0.7,0.16,0.));
#37327=CARTESIAN_POINT('',(-0.7,0.1925,0.0325));
#37328=CARTESIAN_POINT('',(-0.7,0.,0.));
#37329=CARTESIAN_POINT('Origin',(0.4,0.18,0.38));
#37330=CARTESIAN_POINT('',(0.4,0.2,0.36));
#37331=CARTESIAN_POINT('Origin',(0.8,0.2,0.));
#37332=CARTESIAN_POINT('',(0.4,0.2,0.04));
#37333=CARTESIAN_POINT('Origin',(0.4,0.18,0.02));
#37334=CARTESIAN_POINT('',(0.4,0.16,0.));
#37335=CARTESIAN_POINT('Origin',(0.,0.,0.));
#37336=CARTESIAN_POINT('',(0.,0.,0.));
#37337=CARTESIAN_POINT('',(0.,0.,0.));
#37338=CARTESIAN_POINT('Origin',(5.7,1.6,8.));
#37339=CARTESIAN_POINT('',(5.7,3.6,9.04606079858305));
#37340=CARTESIAN_POINT('',(5.7,1.6,9.04606079858305));
#37341=CARTESIAN_POINT('',(5.7,-9.4,9.04606079858305));
#37342=CARTESIAN_POINT('',(5.7,3.6,9.35));
#37343=CARTESIAN_POINT('',(5.7,3.6,9.35));
#37344=CARTESIAN_POINT('',(5.7,1.6,9.35));
#37345=CARTESIAN_POINT('',(5.7,1.6,9.35));
#37346=CARTESIAN_POINT('',(5.7,1.6,9.35));
#37347=CARTESIAN_POINT('Origin',(6.,1.6,8.675));
#37348=CARTESIAN_POINT('',(6.3,1.6,9.04606079858305));
#37349=CARTESIAN_POINT('Origin',(6.,1.6,10.));
#37350=CARTESIAN_POINT('',(6.3,1.6,9.35));
#37351=CARTESIAN_POINT('',(6.3,1.6,9.35));
#37352=CARTESIAN_POINT('',(6.3,1.6,8.));
#37353=CARTESIAN_POINT('Origin',(6.3,1.6,9.35));
#37354=CARTESIAN_POINT('',(6.3,3.6,9.04606079858305));
#37355=CARTESIAN_POINT('',(6.3,-9.4,9.04606079858305));
#37356=CARTESIAN_POINT('',(6.3,3.6,9.35));
#37357=CARTESIAN_POINT('',(6.3,1.6,9.35));
#37358=CARTESIAN_POINT('',(6.3,3.6,8.));
#37359=CARTESIAN_POINT('Origin',(5.7,1.6,9.35));
#37360=CARTESIAN_POINT('',(6.3,3.6,9.35));
#37361=CARTESIAN_POINT('Origin',(6.,3.6,8.675));
#37362=CARTESIAN_POINT('Origin',(6.,3.6,10.));
#37363=CARTESIAN_POINT('Origin',(5.54400660842437,-2.4,8.0297030612521));
#37364=CARTESIAN_POINT('',(5.62607959275755,-0.4,9.07253920349826));
#37365=CARTESIAN_POINT('',(5.62607959275755,-2.4,9.07253920349826));
#37366=CARTESIAN_POINT('',(5.62607959275755,-9.4,9.07253920349826));
#37367=CARTESIAN_POINT('',(5.64992638765696,-0.4,9.37554146179182));
#37368=CARTESIAN_POINT('',(5.64992638765696,-0.4,9.37554146179182));
#37369=CARTESIAN_POINT('',(5.64992638765696,-2.4,9.37554146179182));
#37370=CARTESIAN_POINT('',(5.64992638765696,-2.4,9.37554146179182));
#37371=CARTESIAN_POINT('',(5.64992638765696,-2.4,9.37554146179182));
#37372=CARTESIAN_POINT('Origin',(5.89604169816061,-2.4,8.67908453280361));
#37373=CARTESIAN_POINT('',(6.22422999299742,-2.4,9.02546374606156));
#37374=CARTESIAN_POINT('Origin',(6.,-2.4,10.));
#37375=CARTESIAN_POINT('',(6.24807678789684,-2.4,9.32846600435511));
#37376=CARTESIAN_POINT('',(6.24807678789684,-2.4,9.32846600435511));
#37377=CARTESIAN_POINT('',(6.14215700866425,-2.4,7.98262760381539));
#37378=CARTESIAN_POINT('Origin',(6.24807678789684,-2.4,9.32846600435511));
#37379=CARTESIAN_POINT('',(6.22422999299742,-0.4,9.02546374606156));
#37380=CARTESIAN_POINT('',(6.22422999299742,-9.4,9.02546374606156));
#37381=CARTESIAN_POINT('',(6.24807678789684,-0.4,9.32846600435511));
#37382=CARTESIAN_POINT('',(6.24807678789684,-2.4,9.32846600435511));
#37383=CARTESIAN_POINT('',(6.14215700866425,-0.4,7.98262760381539));
#37384=CARTESIAN_POINT('Origin',(5.64992638765696,-2.4,9.37554146179182));
#37385=CARTESIAN_POINT('',(6.24807678789684,-0.4,9.32846600435511));
#37386=CARTESIAN_POINT('Origin',(5.89604169816061,-0.4,8.67908453280361));
#37387=CARTESIAN_POINT('Origin',(6.,-0.4,10.));
#37388=CARTESIAN_POINT('Origin',(6.,-9.4,10.));
#37389=CARTESIAN_POINT('',(5.,9.4,10.));
#37390=CARTESIAN_POINT('Origin',(6.,9.4,10.));
#37391=CARTESIAN_POINT('',(5.,-9.4,10.));
#37392=CARTESIAN_POINT('',(5.,-9.4,10.));
#37393=CARTESIAN_POINT('Origin',(6.,-9.4,10.));
#37394=CARTESIAN_POINT('Origin',(6.,9.4,10.));
#37395=CARTESIAN_POINT('Origin',(6.,-9.4,10.));
#37396=CARTESIAN_POINT('',(0.,0.,0.));
#37397=CARTESIAN_POINT('Origin',(6.,-8.2,10.99));
#37398=CARTESIAN_POINT('',(6.17298843892005,-8.31905880899792,10.99));
#37399=CARTESIAN_POINT('',(6.17298843892005,-8.08094119100208,10.99));
#37400=CARTESIAN_POINT('',(6.17298843892005,-8.6,10.99));
#37401=CARTESIAN_POINT('Origin',(6.,-8.2,10.99));
#37402=CARTESIAN_POINT('Origin',(6.,-8.2,10.99));
#37403=CARTESIAN_POINT('',(5.82701156107995,-8.31905880899792,10.99));
#37404=CARTESIAN_POINT('Ctrl Pts',(5.82701156107995,-8.31905880899792,10.99));
#37405=CARTESIAN_POINT('Ctrl Pts',(5.83440513468869,-8.3298014223953,10.9912919219764));
#37406=CARTESIAN_POINT('Ctrl Pts',(5.8427028612744,-8.33968770937275,10.992653949439));
#37407=CARTESIAN_POINT('Ctrl Pts',(5.87010792615492,-8.36709277425327,10.9967480843909));
#37408=CARTESIAN_POINT('Ctrl Pts',(5.89366983224072,-8.38324205633295,10.9996958932764));
#37409=CARTESIAN_POINT('Ctrl Pts',(5.94538709536759,-8.40469779396491,11.0038502947236));
#37410=CARTESIAN_POINT('Ctrl Pts',(5.97354876917015,-8.41,11.005));
#37411=CARTESIAN_POINT('Ctrl Pts',(6.02645123082985,-8.41,11.005));
#37412=CARTESIAN_POINT('Ctrl Pts',(6.05461290463241,-8.40469779396491,11.0038502947236));
#37413=CARTESIAN_POINT('Ctrl Pts',(6.10633016775928,-8.38324205633295,10.9996958932764));
#37414=CARTESIAN_POINT('Ctrl Pts',(6.12989207384508,-8.36709277425327,10.9967480843909));
#37415=CARTESIAN_POINT('Ctrl Pts',(6.1572971387256,-8.33968770937275,10.992653949439));
#37416=CARTESIAN_POINT('Ctrl Pts',(6.16559486531131,-8.3298014223953,10.9912919219764));
#37417=CARTESIAN_POINT('Ctrl Pts',(6.17298843892005,-8.31905880899792,10.99));
#37418=CARTESIAN_POINT('',(5.79,-8.2,10.99));
#37419=CARTESIAN_POINT('Origin',(6.,-8.2,10.99));
#37420=CARTESIAN_POINT('',(5.79,-8.2,11.38416039533));
#37421=CARTESIAN_POINT('',(5.79,-8.2,10.99));
#37422=CARTESIAN_POINT('',(6.21,-8.2,11.38416039533));
#37423=CARTESIAN_POINT('Ctrl Pts',(6.21,-8.2,11.38416039533));
#37424=CARTESIAN_POINT('Ctrl Pts',(6.21,-8.22641116018714,11.38416039533));
#37425=CARTESIAN_POINT('Ctrl Pts',(6.20471354911189,-8.2545550596171,11.3849944296993));
#37426=CARTESIAN_POINT('Ctrl Pts',(6.18326999585849,-8.30628264999174,11.3879947099895));
#37427=CARTESIAN_POINT('Ctrl Pts',(6.16711503760643,-8.32986981049192,11.3901162943626));
#37428=CARTESIAN_POINT('Ctrl Pts',(6.12987013519678,-8.36711471290156,11.394089123191));
#37429=CARTESIAN_POINT('Ctrl Pts',(6.10628283459019,-8.38326992585508,11.3962002442067));
#37430=CARTESIAN_POINT('Ctrl Pts',(6.05455476560391,-8.40471366447292,11.3991765222353));
#37431=CARTESIAN_POINT('Ctrl Pts',(6.02641069968078,-8.41,11.4));
#37432=CARTESIAN_POINT('Ctrl Pts',(5.97358930031922,-8.41,11.4));
#37433=CARTESIAN_POINT('Ctrl Pts',(5.94544523439609,-8.40471366447292,11.3991765222353));
#37434=CARTESIAN_POINT('Ctrl Pts',(5.89371716540981,-8.38326992585508,11.3962002442067));
#37435=CARTESIAN_POINT('Ctrl Pts',(5.87012986480322,-8.36711471290156,11.394089123191));
#37436=CARTESIAN_POINT('Ctrl Pts',(5.83288496239357,-8.32986981049192,11.3901162943626));
#37437=CARTESIAN_POINT('Ctrl Pts',(5.81673000414151,-8.30628264999174,11.3879947099895));
#37438=CARTESIAN_POINT('Ctrl Pts',(5.79528645088811,-8.2545550596171,11.3849944296993));
#37439=CARTESIAN_POINT('Ctrl Pts',(5.79,-8.22641116018714,11.38416039533));
#37440=CARTESIAN_POINT('Ctrl Pts',(5.79,-8.2,11.38416039533));
#37441=CARTESIAN_POINT('Ctrl Pts',(5.79,-8.2,11.38416039533));
#37442=CARTESIAN_POINT('Ctrl Pts',(5.79,-8.17358883981285,11.38416039533));
#37443=CARTESIAN_POINT('Ctrl Pts',(5.79528645088811,-8.1454449403829,11.3849944296993));
#37444=CARTESIAN_POINT('Ctrl Pts',(5.81673000414151,-8.09371735000826,11.3879947099895));
#37445=CARTESIAN_POINT('Ctrl Pts',(5.83288496239357,-8.07013018950807,11.3901162943626));
#37446=CARTESIAN_POINT('Ctrl Pts',(5.87012986480322,-8.03288528709843,11.394089123191));
#37447=CARTESIAN_POINT('Ctrl Pts',(5.89371716540981,-8.01673007414492,11.3962002442067));
#37448=CARTESIAN_POINT('Ctrl Pts',(5.94544523439609,-7.99528633552708,11.3991765222353));
#37449=CARTESIAN_POINT('Ctrl Pts',(5.97358930031922,-7.99,11.4));
#37450=CARTESIAN_POINT('Ctrl Pts',(6.02641069968078,-7.99,11.4));
#37451=CARTESIAN_POINT('Ctrl Pts',(6.05455476560391,-7.99528633552708,11.3991765222353));
#37452=CARTESIAN_POINT('Ctrl Pts',(6.10628283459019,-8.01673007414492,11.3962002442067));
#37453=CARTESIAN_POINT('Ctrl Pts',(6.12987013519678,-8.03288528709843,11.394089123191));
#37454=CARTESIAN_POINT('Ctrl Pts',(6.16711503760642,-8.07013018950807,11.3901162943626));
#37455=CARTESIAN_POINT('Ctrl Pts',(6.18326999585848,-8.09371735000826,11.3879947099895));
#37456=CARTESIAN_POINT('Ctrl Pts',(6.20471354911189,-8.1454449403829,11.3849944296993));
#37457=CARTESIAN_POINT('Ctrl Pts',(6.21,-8.17358883981285,11.38416039533));
#37458=CARTESIAN_POINT('Ctrl Pts',(6.21,-8.2,11.38416039533));
#37459=CARTESIAN_POINT('',(5.82701156107995,-8.08094119100208,10.99));
#37460=CARTESIAN_POINT('Origin',(6.,-8.2,10.99));
#37461=CARTESIAN_POINT('Ctrl Pts',(6.17298843892005,-8.08094119100207,10.99));
#37462=CARTESIAN_POINT('Ctrl Pts',(6.16559486531131,-8.0701985776047,10.9912919219764));
#37463=CARTESIAN_POINT('Ctrl Pts',(6.1572971387256,-8.06031229062725,10.992653949439));
#37464=CARTESIAN_POINT('Ctrl Pts',(6.12989207384508,-8.03290722574673,10.9967480843909));
#37465=CARTESIAN_POINT('Ctrl Pts',(6.10633016775929,-8.01675794366705,10.9996958932764));
#37466=CARTESIAN_POINT('Ctrl Pts',(6.05461290463241,-7.99530220603509,11.0038502947236));
#37467=CARTESIAN_POINT('Ctrl Pts',(6.02645123082985,-7.99,11.005));
#37468=CARTESIAN_POINT('Ctrl Pts',(5.97354876917015,-7.99,11.005));
#37469=CARTESIAN_POINT('Ctrl Pts',(5.94538709536759,-7.99530220603509,11.0038502947236));
#37470=CARTESIAN_POINT('Ctrl Pts',(5.89366983224071,-8.01675794366705,10.9996958932764));
#37471=CARTESIAN_POINT('Ctrl Pts',(5.87010792615492,-8.03290722574673,10.9967480843909));
#37472=CARTESIAN_POINT('Ctrl Pts',(5.8427028612744,-8.06031229062725,10.992653949439));
#37473=CARTESIAN_POINT('Ctrl Pts',(5.83440513468869,-8.0701985776047,10.9912919219764));
#37474=CARTESIAN_POINT('Ctrl Pts',(5.82701156107995,-8.08094119100208,10.99));
#37475=CARTESIAN_POINT('Origin',(6.,-8.2,10.99));
#37476=CARTESIAN_POINT('',(5.82701156107995,-8.6,10.99));
#37477=CARTESIAN_POINT('Origin',(6.,-8.6,10.));
#37478=CARTESIAN_POINT('',(4.995,-7.8,10.));
#37479=CARTESIAN_POINT('Origin',(6.,-7.8,10.));
#37480=CARTESIAN_POINT('',(4.995,-8.6,10.));
#37481=CARTESIAN_POINT('',(4.995,-8.6,10.));
#37482=CARTESIAN_POINT('Origin',(6.,-8.6,10.));
#37483=CARTESIAN_POINT('Origin',(6.,-8.6,10.));
#37484=CARTESIAN_POINT('',(4.6,-7.8,10.));
#37485=CARTESIAN_POINT('Origin',(6.,-7.8,10.));
#37486=CARTESIAN_POINT('',(4.6,-8.6,10.));
#37487=CARTESIAN_POINT('',(4.6,-8.6,10.));
#37488=CARTESIAN_POINT('Origin',(6.,-8.6,10.));
#37489=CARTESIAN_POINT('Origin',(6.,-7.8,10.));
#37490=CARTESIAN_POINT('Origin',(6.,-8.6,10.));
#37491=CARTESIAN_POINT('',(0.,0.,0.));
#37492=CARTESIAN_POINT('Origin',(6.,8.2,10.99));
#37493=CARTESIAN_POINT('',(6.17298843892005,8.08094119100208,10.99));
#37494=CARTESIAN_POINT('',(6.17298843892005,8.31905880899792,10.99));
#37495=CARTESIAN_POINT('',(6.17298843892005,7.8,10.99));
#37496=CARTESIAN_POINT('Origin',(6.,8.2,10.99));
#37497=CARTESIAN_POINT('Origin',(6.,8.2,10.99));
#37498=CARTESIAN_POINT('',(5.82701156107995,8.08094119100208,10.99));
#37499=CARTESIAN_POINT('Ctrl Pts',(5.82701156107995,8.08094119100207,10.99));
#37500=CARTESIAN_POINT('Ctrl Pts',(5.83440513468869,8.0701985776047,10.9912919219764));
#37501=CARTESIAN_POINT('Ctrl Pts',(5.8427028612744,8.06031229062725,10.992653949439));
#37502=CARTESIAN_POINT('Ctrl Pts',(5.87010792615492,8.03290722574673,10.9967480843909));
#37503=CARTESIAN_POINT('Ctrl Pts',(5.89366983224071,8.01675794366705,10.9996958932764));
#37504=CARTESIAN_POINT('Ctrl Pts',(5.94538709536759,7.99530220603509,11.0038502947236));
#37505=CARTESIAN_POINT('Ctrl Pts',(5.97354876917015,7.99,11.005));
#37506=CARTESIAN_POINT('Ctrl Pts',(6.02645123082985,7.99,11.005));
#37507=CARTESIAN_POINT('Ctrl Pts',(6.05461290463241,7.99530220603509,11.0038502947236));
#37508=CARTESIAN_POINT('Ctrl Pts',(6.10633016775928,8.01675794366705,10.9996958932764));
#37509=CARTESIAN_POINT('Ctrl Pts',(6.12989207384508,8.03290722574673,10.9967480843909));
#37510=CARTESIAN_POINT('Ctrl Pts',(6.1572971387256,8.06031229062725,10.992653949439));
#37511=CARTESIAN_POINT('Ctrl Pts',(6.16559486531131,8.0701985776047,10.9912919219764));
#37512=CARTESIAN_POINT('Ctrl Pts',(6.17298843892005,8.08094119100208,10.99));
#37513=CARTESIAN_POINT('',(5.79,8.2,10.99));
#37514=CARTESIAN_POINT('Origin',(6.,8.2,10.99));
#37515=CARTESIAN_POINT('',(5.79,8.2,11.38416039533));
#37516=CARTESIAN_POINT('',(5.79,8.2,10.99));
#37517=CARTESIAN_POINT('',(6.21,8.2,11.38416039533));
#37518=CARTESIAN_POINT('Ctrl Pts',(6.21,8.2,11.38416039533));
#37519=CARTESIAN_POINT('Ctrl Pts',(6.21,8.17358883981285,11.38416039533));
#37520=CARTESIAN_POINT('Ctrl Pts',(6.20471354911189,8.1454449403829,11.3849944296993));
#37521=CARTESIAN_POINT('Ctrl Pts',(6.18326999585849,8.09371735000826,11.3879947099895));
#37522=CARTESIAN_POINT('Ctrl Pts',(6.16711503760643,8.07013018950807,11.3901162943626));
#37523=CARTESIAN_POINT('Ctrl Pts',(6.12987013519678,8.03288528709843,11.394089123191));
#37524=CARTESIAN_POINT('Ctrl Pts',(6.10628283459019,8.01673007414492,11.3962002442067));
#37525=CARTESIAN_POINT('Ctrl Pts',(6.05455476560391,7.99528633552708,11.3991765222353));
#37526=CARTESIAN_POINT('Ctrl Pts',(6.02641069968078,7.99,11.4));
#37527=CARTESIAN_POINT('Ctrl Pts',(5.97358930031922,7.99,11.4));
#37528=CARTESIAN_POINT('Ctrl Pts',(5.94544523439609,7.99528633552708,11.3991765222353));
#37529=CARTESIAN_POINT('Ctrl Pts',(5.89371716540981,8.01673007414492,11.3962002442067));
#37530=CARTESIAN_POINT('Ctrl Pts',(5.87012986480322,8.03288528709843,11.394089123191));
#37531=CARTESIAN_POINT('Ctrl Pts',(5.83288496239357,8.07013018950807,11.3901162943626));
#37532=CARTESIAN_POINT('Ctrl Pts',(5.81673000414151,8.09371735000826,11.3879947099895));
#37533=CARTESIAN_POINT('Ctrl Pts',(5.79528645088811,8.1454449403829,11.3849944296993));
#37534=CARTESIAN_POINT('Ctrl Pts',(5.79,8.17358883981285,11.38416039533));
#37535=CARTESIAN_POINT('Ctrl Pts',(5.79,8.2,11.38416039533));
#37536=CARTESIAN_POINT('Ctrl Pts',(5.79,8.2,11.38416039533));
#37537=CARTESIAN_POINT('Ctrl Pts',(5.79,8.22641116018715,11.38416039533));
#37538=CARTESIAN_POINT('Ctrl Pts',(5.79528645088811,8.2545550596171,11.3849944296993));
#37539=CARTESIAN_POINT('Ctrl Pts',(5.81673000414151,8.30628264999174,11.3879947099895));
#37540=CARTESIAN_POINT('Ctrl Pts',(5.83288496239357,8.32986981049192,11.3901162943626));
#37541=CARTESIAN_POINT('Ctrl Pts',(5.87012986480322,8.36711471290156,11.394089123191));
#37542=CARTESIAN_POINT('Ctrl Pts',(5.89371716540981,8.38326992585508,11.3962002442067));
#37543=CARTESIAN_POINT('Ctrl Pts',(5.94544523439609,8.40471366447292,11.3991765222353));
#37544=CARTESIAN_POINT('Ctrl Pts',(5.97358930031922,8.41,11.4));
#37545=CARTESIAN_POINT('Ctrl Pts',(6.02641069968078,8.41,11.4));
#37546=CARTESIAN_POINT('Ctrl Pts',(6.05455476560391,8.40471366447292,11.3991765222353));
#37547=CARTESIAN_POINT('Ctrl Pts',(6.10628283459019,8.38326992585508,11.3962002442067));
#37548=CARTESIAN_POINT('Ctrl Pts',(6.12987013519678,8.36711471290156,11.394089123191));
#37549=CARTESIAN_POINT('Ctrl Pts',(6.16711503760642,8.32986981049192,11.3901162943626));
#37550=CARTESIAN_POINT('Ctrl Pts',(6.18326999585849,8.30628264999174,11.3879947099895));
#37551=CARTESIAN_POINT('Ctrl Pts',(6.2047135491119,8.2545550596171,11.3849944296993));
#37552=CARTESIAN_POINT('Ctrl Pts',(6.21,8.22641116018714,11.38416039533));
#37553=CARTESIAN_POINT('Ctrl Pts',(6.21,8.2,11.38416039533));
#37554=CARTESIAN_POINT('',(5.82701156107995,8.31905880899792,10.99));
#37555=CARTESIAN_POINT('Origin',(6.,8.2,10.99));
#37556=CARTESIAN_POINT('Ctrl Pts',(6.17298843892005,8.31905880899792,10.99));
#37557=CARTESIAN_POINT('Ctrl Pts',(6.16559486531131,8.3298014223953,10.9912919219764));
#37558=CARTESIAN_POINT('Ctrl Pts',(6.1572971387256,8.33968770937275,10.992653949439));
#37559=CARTESIAN_POINT('Ctrl Pts',(6.12989207384508,8.36709277425327,10.9967480843909));
#37560=CARTESIAN_POINT('Ctrl Pts',(6.10633016775928,8.38324205633295,10.9996958932764));
#37561=CARTESIAN_POINT('Ctrl Pts',(6.05461290463241,8.40469779396491,11.0038502947236));
#37562=CARTESIAN_POINT('Ctrl Pts',(6.02645123082985,8.41,11.005));
#37563=CARTESIAN_POINT('Ctrl Pts',(5.97354876917015,8.41,11.005));
#37564=CARTESIAN_POINT('Ctrl Pts',(5.94538709536759,8.40469779396491,11.0038502947236));
#37565=CARTESIAN_POINT('Ctrl Pts',(5.89366983224072,8.38324205633295,10.9996958932764));
#37566=CARTESIAN_POINT('Ctrl Pts',(5.87010792615492,8.36709277425327,10.9967480843909));
#37567=CARTESIAN_POINT('Ctrl Pts',(5.8427028612744,8.33968770937275,10.992653949439));
#37568=CARTESIAN_POINT('Ctrl Pts',(5.83440513468869,8.3298014223953,10.9912919219764));
#37569=CARTESIAN_POINT('Ctrl Pts',(5.82701156107995,8.31905880899792,10.99));
#37570=CARTESIAN_POINT('Origin',(6.,8.2,10.99));
#37571=CARTESIAN_POINT('',(5.82701156107995,7.8,10.99));
#37572=CARTESIAN_POINT('Origin',(6.,7.8,10.));
#37573=CARTESIAN_POINT('',(4.995,8.6,10.));
#37574=CARTESIAN_POINT('Origin',(6.,8.6,10.));
#37575=CARTESIAN_POINT('',(4.995,7.8,10.));
#37576=CARTESIAN_POINT('',(4.995,7.8,10.));
#37577=CARTESIAN_POINT('Origin',(6.,7.8,10.));
#37578=CARTESIAN_POINT('Origin',(6.,7.8,10.));
#37579=CARTESIAN_POINT('',(4.6,8.6,10.));
#37580=CARTESIAN_POINT('Origin',(6.,8.6,10.));
#37581=CARTESIAN_POINT('',(4.6,7.8,10.));
#37582=CARTESIAN_POINT('',(4.6,7.8,10.));
#37583=CARTESIAN_POINT('Origin',(6.,7.8,10.));
#37584=CARTESIAN_POINT('Origin',(6.,8.6,10.));
#37585=CARTESIAN_POINT('Origin',(6.,7.8,10.));
#37586=CARTESIAN_POINT('',(0.,0.,0.));
#37587=CARTESIAN_POINT('Origin',(6.,-7.8,10.));
#37588=CARTESIAN_POINT('',(4.995,-6.7,10.));
#37589=CARTESIAN_POINT('Origin',(6.,-6.7,10.));
#37590=CARTESIAN_POINT('',(4.995,-7.8,10.));
#37591=CARTESIAN_POINT('',(4.995,-7.8,10.));
#37592=CARTESIAN_POINT('Origin',(6.,-7.8,10.));
#37593=CARTESIAN_POINT('Origin',(6.,-7.8,10.));
#37594=CARTESIAN_POINT('',(4.7,-6.7,10.));
#37595=CARTESIAN_POINT('Origin',(6.,-6.7,10.));
#37596=CARTESIAN_POINT('',(4.7,-7.8,10.));
#37597=CARTESIAN_POINT('',(4.7,-7.8,10.));
#37598=CARTESIAN_POINT('Origin',(6.,-7.8,10.));
#37599=CARTESIAN_POINT('Origin',(6.,-6.7,10.));
#37600=CARTESIAN_POINT('Origin',(6.,-7.8,10.));
#37601=CARTESIAN_POINT('',(0.,0.,0.));
#37602=CARTESIAN_POINT('Origin',(6.,6.7,10.));
#37603=CARTESIAN_POINT('',(4.995,7.8,10.));
#37604=CARTESIAN_POINT('Origin',(6.,7.8,10.));
#37605=CARTESIAN_POINT('',(4.995,6.7,10.));
#37606=CARTESIAN_POINT('',(4.995,6.7,10.));
#37607=CARTESIAN_POINT('Origin',(6.,6.7,10.));
#37608=CARTESIAN_POINT('Origin',(6.,6.7,10.));
#37609=CARTESIAN_POINT('',(4.7,7.8,10.));
#37610=CARTESIAN_POINT('Origin',(6.,7.8,10.));
#37611=CARTESIAN_POINT('',(4.7,6.7,10.));
#37612=CARTESIAN_POINT('',(4.7,6.7,10.));
#37613=CARTESIAN_POINT('Origin',(6.,6.7,10.));
#37614=CARTESIAN_POINT('Origin',(6.,7.8,10.));
#37615=CARTESIAN_POINT('Origin',(6.,6.7,10.));
#37616=CARTESIAN_POINT('',(0.,0.,0.));
#37617=CARTESIAN_POINT('Origin',(6.,-5.3,10.));
#37618=CARTESIAN_POINT('',(4.995,-3.,10.));
#37619=CARTESIAN_POINT('Origin',(6.,-3.,10.));
#37620=CARTESIAN_POINT('',(4.995,-5.3,10.));
#37621=CARTESIAN_POINT('',(4.995,-5.3,10.));
#37622=CARTESIAN_POINT('Origin',(6.,-5.3,10.));
#37623=CARTESIAN_POINT('Origin',(6.,-5.3,10.));
#37624=CARTESIAN_POINT('',(4.7,-3.,10.));
#37625=CARTESIAN_POINT('Origin',(6.,-3.,10.));
#37626=CARTESIAN_POINT('',(4.7,-5.3,10.));
#37627=CARTESIAN_POINT('',(4.7,-5.3,10.));
#37628=CARTESIAN_POINT('Origin',(6.,-5.3,10.));
#37629=CARTESIAN_POINT('Origin',(6.,-3.,10.));
#37630=CARTESIAN_POINT('Origin',(6.,-5.3,10.));
#37631=CARTESIAN_POINT('',(0.,0.,0.));
#37632=CARTESIAN_POINT('Origin',(6.,0.2,10.));
#37633=CARTESIAN_POINT('',(4.995,1.,10.));
#37634=CARTESIAN_POINT('Origin',(6.,1.,10.));
#37635=CARTESIAN_POINT('',(4.995,0.2,10.));
#37636=CARTESIAN_POINT('',(4.995,0.2,10.));
#37637=CARTESIAN_POINT('Origin',(6.,0.2,10.));
#37638=CARTESIAN_POINT('Origin',(6.,0.2,10.));
#37639=CARTESIAN_POINT('',(4.7,1.,10.));
#37640=CARTESIAN_POINT('Origin',(6.,1.,10.));
#37641=CARTESIAN_POINT('',(4.7,0.2,10.));
#37642=CARTESIAN_POINT('',(4.7,0.2,10.));
#37643=CARTESIAN_POINT('Origin',(6.,0.2,10.));
#37644=CARTESIAN_POINT('Origin',(6.,1.,10.));
#37645=CARTESIAN_POINT('Origin',(6.,0.2,10.));
#37646=CARTESIAN_POINT('',(0.,0.,0.));
#37647=CARTESIAN_POINT('Origin',(6.,4.2,10.));
#37648=CARTESIAN_POINT('',(4.995,5.3,10.));
#37649=CARTESIAN_POINT('Origin',(6.,5.3,10.));
#37650=CARTESIAN_POINT('',(4.995,4.2,10.));
#37651=CARTESIAN_POINT('',(4.995,4.2,10.));
#37652=CARTESIAN_POINT('Origin',(6.,4.2,10.));
#37653=CARTESIAN_POINT('Origin',(6.,4.2,10.));
#37654=CARTESIAN_POINT('',(4.7,5.3,10.));
#37655=CARTESIAN_POINT('Origin',(6.,5.3,10.));
#37656=CARTESIAN_POINT('',(4.7,4.2,10.));
#37657=CARTESIAN_POINT('',(4.7,4.2,10.));
#37658=CARTESIAN_POINT('Origin',(6.,4.2,10.));
#37659=CARTESIAN_POINT('Origin',(6.,5.3,10.));
#37660=CARTESIAN_POINT('Origin',(6.,4.2,10.));
#37661=CARTESIAN_POINT('',(0.,0.,0.));
#37662=CARTESIAN_POINT('Origin',(-0.3,-1.1,-1.28));
#37663=CARTESIAN_POINT('',(-0.3,-1.,-1.28));
#37664=CARTESIAN_POINT('',(-0.3,-1.,-0.953939201416946));
#37665=CARTESIAN_POINT('',(-0.3,-1.,-0.64));
#37666=CARTESIAN_POINT('',(-0.3,2.2,-1.28));
#37667=CARTESIAN_POINT('',(-0.3,-1.1,-1.28));
#37668=CARTESIAN_POINT('',(-0.3,2.2,-0.953939201416946));
#37669=CARTESIAN_POINT('',(-0.3,2.2,-0.64));
#37670=CARTESIAN_POINT('',(-0.3,-1.1,-0.953939201416946));
#37671=CARTESIAN_POINT('Origin',(0.3,-1.1,-1.28));
#37672=CARTESIAN_POINT('',(0.3,-1.,-1.28));
#37673=CARTESIAN_POINT('',(0.15,-1.,-1.28));
#37674=CARTESIAN_POINT('',(0.3,2.2,-1.28));
#37675=CARTESIAN_POINT('',(0.3,-1.1,-1.28));
#37676=CARTESIAN_POINT('',(0.15,2.2,-1.28));
#37677=CARTESIAN_POINT('Origin',(0.3,-1.1,0.));
#37678=CARTESIAN_POINT('',(0.3,-1.,-0.953939201416946));
#37679=CARTESIAN_POINT('',(0.3,-1.,0.));
#37680=CARTESIAN_POINT('',(0.3,2.2,-0.953939201416946));
#37681=CARTESIAN_POINT('',(0.3,-1.1,-0.953939201416946));
#37682=CARTESIAN_POINT('',(0.3,2.2,0.));
#37683=CARTESIAN_POINT('Origin',(0.,2.2,0.));
#37684=CARTESIAN_POINT('',(-1.4,2.2,1.71450551880629E-16));
#37685=CARTESIAN_POINT('Origin',(0.,2.2,0.));
#37686=CARTESIAN_POINT('Origin',(0.,2.2,0.));
#37687=CARTESIAN_POINT('Origin',(0.,-1.1,0.));
#37688=CARTESIAN_POINT('Origin',(0.,-1.,0.));
#37689=CARTESIAN_POINT('Origin',(0.,-1.,0.));
#37690=CARTESIAN_POINT('',(1.60662857109684,-1.,0.693717979106306));
#37691=CARTESIAN_POINT('',(1.5055822144029,-1.,0.892032620296856));
#37692=CARTESIAN_POINT('Origin',(0.,-1.,0.));
#37693=CARTESIAN_POINT('',(1.81978687191668,-1.,1.23627494547115));
#37694=CARTESIAN_POINT('Ctrl Pts',(1.5055822144029,-1.,0.892032620296856));
#37695=CARTESIAN_POINT('Ctrl Pts',(1.50980486806688,-1.,0.894452006964544));
#37696=CARTESIAN_POINT('Ctrl Pts',(1.51805569590094,-1.,0.899185047483511));
#37697=CARTESIAN_POINT('Ctrl Pts',(1.52984849887993,-1.,0.905967409625651));
#37698=CARTESIAN_POINT('Ctrl Pts',(1.54440491149498,-1.,0.914375919026456));
#37699=CARTESIAN_POINT('Ctrl Pts',(1.56065988578893,-1.,0.923832188944341));
#37700=CARTESIAN_POINT('Ctrl Pts',(1.57499388382243,-1.,0.932246680108685));
#37701=CARTESIAN_POINT('Ctrl Pts',(1.58744937487176,-1.,0.939646377893399));
#37702=CARTESIAN_POINT('Ctrl Pts',(1.59810042043673,-1.,0.946078063315257));
#37703=CARTESIAN_POINT('Ctrl Pts',(1.60706069896936,-1.,0.951613284356035));
#37704=CARTESIAN_POINT('Ctrl Pts',(1.61449324337085,-1.,0.956354422920671));
#37705=CARTESIAN_POINT('Ctrl Pts',(1.62061638140221,-1.,0.960438326101729));
#37706=CARTESIAN_POINT('Ctrl Pts',(1.62571930670187,-1.,0.964046107040536));
#37707=CARTESIAN_POINT('Ctrl Pts',(1.63013849959461,-1.,0.967387853230345));
#37708=CARTESIAN_POINT('Ctrl Pts',(1.63420665729798,-1.,0.970669715997509));
#37709=CARTESIAN_POINT('Ctrl Pts',(1.63820952658144,-1.,0.974066058287419));
#37710=CARTESIAN_POINT('Ctrl Pts',(1.64233990826687,-1.,0.977689794119417));
#37711=CARTESIAN_POINT('Ctrl Pts',(1.64665139190656,-1.,0.981562530939489));
#37712=CARTESIAN_POINT('Ctrl Pts',(1.65110016612638,-1.,0.985642622920821));
#37713=CARTESIAN_POINT('Ctrl Pts',(1.65559044289699,-1.,0.989855627854165));
#37714=CARTESIAN_POINT('Ctrl Pts',(1.66001553809947,-1.,0.994121836661306));
#37715=CARTESIAN_POINT('Ctrl Pts',(1.66430758030376,-1.,0.998389654952758));
#37716=CARTESIAN_POINT('Ctrl Pts',(1.66846059277303,-1.,1.00265091003727));
#37717=CARTESIAN_POINT('Ctrl Pts',(1.67250335383293,-1.,1.00692206696414));
#37718=CARTESIAN_POINT('Ctrl Pts',(1.67648246776464,-1.,1.01123236493511));
#37719=CARTESIAN_POINT('Ctrl Pts',(1.68044289894798,-1.,1.01561026162773));
#37720=CARTESIAN_POINT('Ctrl Pts',(1.68440578021706,-1.,1.02006795074201));
#37721=CARTESIAN_POINT('Ctrl Pts',(1.68836910178447,-1.,1.02460180535255));
#37722=CARTESIAN_POINT('Ctrl Pts',(1.69231840863458,-1.,1.02919977579147));
#37723=CARTESIAN_POINT('Ctrl Pts',(1.69623414782771,-1.,1.03384646003588));
#37724=CARTESIAN_POINT('Ctrl Pts',(1.70010052930962,-1.,1.03852922490789));
#37725=CARTESIAN_POINT('Ctrl Pts',(1.70391338707982,-1.,1.04324363334554));
#37726=CARTESIAN_POINT('Ctrl Pts',(1.70767646263649,-1.,1.04799085404995));
#37727=CARTESIAN_POINT('Ctrl Pts',(1.71139783543989,-1.,1.05277517202855));
#37728=CARTESIAN_POINT('Ctrl Pts',(1.7150865442702,-1.,1.05760163192479));
#37729=CARTESIAN_POINT('Ctrl Pts',(1.71874858456904,-1.,1.06247324680647));
#37730=CARTESIAN_POINT('Ctrl Pts',(1.72238500928453,-1.,1.06738966975462));
#37731=CARTESIAN_POINT('Ctrl Pts',(1.72599406198488,-1.,1.07234866990252));
#37732=CARTESIAN_POINT('Ctrl Pts',(1.72957248977424,-1.,1.0773470373727));
#37733=CARTESIAN_POINT('Ctrl Pts',(1.73311705663407,-1.,1.08238162784749));
#37734=CARTESIAN_POINT('Ctrl Pts',(1.73662628326091,-1.,1.08745056285427));
#37735=CARTESIAN_POINT('Ctrl Pts',(1.74010053962247,-1.,1.09255329056493));
#37736=CARTESIAN_POINT('Ctrl Pts',(1.74354119236208,-1.,1.09768999241226));
#37737=CARTESIAN_POINT('Ctrl Pts',(1.74695004214923,-1.,1.10286118991143));
#37738=CARTESIAN_POINT('Ctrl Pts',(1.7503286607592,-1.,1.10806728183007));
#37739=CARTESIAN_POINT('Ctrl Pts',(1.7536777209463,-1.,1.11330807582551));
#37740=CARTESIAN_POINT('Ctrl Pts',(1.75699720772105,-1.,1.11858293216763));
#37741=CARTESIAN_POINT('Ctrl Pts',(1.76028671825096,-1.,1.12389096855086));
#37742=CARTESIAN_POINT('Ctrl Pts',(1.7635457196617,-1.,1.12923123555075));
#37743=CARTESIAN_POINT('Ctrl Pts',(1.76677384551862,-1.,1.1346029180462));
#37744=CARTESIAN_POINT('Ctrl Pts',(1.76997111386769,-1.,1.14000548336975));
#37745=CARTESIAN_POINT('Ctrl Pts',(1.77313777896194,-1.,1.1454385822692));
#37746=CARTESIAN_POINT('Ctrl Pts',(1.7762742255701,-1.,1.15090197841515));
#37747=CARTESIAN_POINT('Ctrl Pts',(1.77938085564275,-1.,1.15639547194698));
#37748=CARTESIAN_POINT('Ctrl Pts',(1.78245795881009,-1.,1.16191881298499));
#37749=CARTESIAN_POINT('Ctrl Pts',(1.78550566040443,-1.,1.16747166312303));
#37750=CARTESIAN_POINT('Ctrl Pts',(1.78852398877616,-1.,1.17305363177328));
#37751=CARTESIAN_POINT('Ctrl Pts',(1.79151291552689,-1.,1.17866429440809));
#37752=CARTESIAN_POINT('Ctrl Pts',(1.79447240321515,-1.,1.18430321697432));
#37753=CARTESIAN_POINT('Ctrl Pts',(1.79740245923478,-1.,1.18996997934445));
#37754=CARTESIAN_POINT('Ctrl Pts',(1.80030314369879,-1.,1.19566418930242));
#37755=CARTESIAN_POINT('Ctrl Pts',(1.80317454838603,-1.,1.20138548938974));
#37756=CARTESIAN_POINT('Ctrl Pts',(1.80601678480707,-1.,1.20713356605475));
#37757=CARTESIAN_POINT('Ctrl Pts',(1.80882996917129,-1.,1.21290815708314));
#37758=CARTESIAN_POINT('Ctrl Pts',(1.81161420806656,-1.,1.21870906103557));
#37759=CARTESIAN_POINT('Ctrl Pts',(1.81436959210434,-1.,1.2245361330495));
#37760=CARTESIAN_POINT('Ctrl Pts',(1.8165508718364,-1.,1.2292186489137));
#37761=CARTESIAN_POINT('Ctrl Pts',(1.81817389921279,-1.,1.2327422452705));
#37762=CARTESIAN_POINT('Ctrl Pts',(1.81925017193666,-1.,1.23509651170476));
#37763=CARTESIAN_POINT('Ctrl Pts',(1.81978687191668,-1.,1.23627494547115));
#37764=CARTESIAN_POINT('',(1.73811241238545,-1.,1.34869019493419));
#37765=CARTESIAN_POINT('',(1.81978687191668,-1.,1.23627494547115));
#37766=CARTESIAN_POINT('',(1.31362392696032,-1.,1.15624053661742));
#37767=CARTESIAN_POINT('Ctrl Pts',(1.73811241238545,-1.,1.34869019493419));
#37768=CARTESIAN_POINT('Ctrl Pts',(1.73682580585691,-1.,1.34854391898045));
#37769=CARTESIAN_POINT('Ctrl Pts',(1.73425417885907,-1.,1.34824783112887));
#37770=CARTESIAN_POINT('Ctrl Pts',(1.7304014965394,-1.,1.34779309152035));
#37771=CARTESIAN_POINT('Ctrl Pts',(1.72527410680674,-1.,1.34716554819527));
#37772=CARTESIAN_POINT('Ctrl Pts',(1.7188807715049,-1.,1.34634568653227));
#37773=CARTESIAN_POINT('Ctrl Pts',(1.71250340686822,-1.,1.34549029589416));
#37774=CARTESIAN_POINT('Ctrl Pts',(1.70614212266738,-1.,1.34459924533831));
#37775=CARTESIAN_POINT('Ctrl Pts',(1.69979707754427,-1.,1.34367237124483));
#37776=CARTESIAN_POINT('Ctrl Pts',(1.6934684849687,-1.,1.34270948206319));
#37777=CARTESIAN_POINT('Ctrl Pts',(1.68715660868764,-1.,1.341710374848));
#37778=CARTESIAN_POINT('Ctrl Pts',(1.68086176030362,-1.,1.34067485185203));
#37779=CARTESIAN_POINT('Ctrl Pts',(1.67458429426086,-1.,1.3396027347034));
#37780=CARTESIAN_POINT('Ctrl Pts',(1.66832460783989,-1.,1.33849388654388));
#37781=CARTESIAN_POINT('Ctrl Pts',(1.66208312541983,-1.,1.33734820885262));
#37782=CARTESIAN_POINT('Ctrl Pts',(1.65586025952593,-1.,1.33616559745172));
#37783=CARTESIAN_POINT('Ctrl Pts',(1.6496563728683,-1.,1.33494590467993));
#37784=CARTESIAN_POINT('Ctrl Pts',(1.6434717485603,-1.,1.33368890676572));
#37785=CARTESIAN_POINT('Ctrl Pts',(1.63730653475089,-1.,1.33239425103724));
#37786=CARTESIAN_POINT('Ctrl Pts',(1.63116079730923,-1.,1.33106149345645));
#37787=CARTESIAN_POINT('Ctrl Pts',(1.62503464209797,-1.,1.3296901950568));
#37788=CARTESIAN_POINT('Ctrl Pts',(1.61892832270724,-1.,1.32828000610449));
#37789=CARTESIAN_POINT('Ctrl Pts',(1.6128423401575,-1.,1.32683074483356));
#37790=CARTESIAN_POINT('Ctrl Pts',(1.60677758290954,-1.,1.32534250785782));
#37791=CARTESIAN_POINT('Ctrl Pts',(1.60073511858687,-1.,1.32381550858256));
#37792=CARTESIAN_POINT('Ctrl Pts',(1.59471591079403,-1.,1.32224985747682));
#37793=CARTESIAN_POINT('Ctrl Pts',(1.58872057258245,-1.,1.32064537110892));
#37794=CARTESIAN_POINT('Ctrl Pts',(1.58274907898834,-1.,1.31900135021432));
#37795=CARTESIAN_POINT('Ctrl Pts',(1.5768005650559,-1.,1.31731642317187));
#37796=CARTESIAN_POINT('Ctrl Pts',(1.57087397835723,-1.,1.31558903860016));
#37797=CARTESIAN_POINT('Ctrl Pts',(1.56496872402353,-1.,1.31381795281002));
#37798=CARTESIAN_POINT('Ctrl Pts',(1.55908521254821,-1.,1.31200264341696));
#37799=CARTESIAN_POINT('Ctrl Pts',(1.55322568759481,-1.,1.31014393684222));
#37800=CARTESIAN_POINT('Ctrl Pts',(1.54739413957185,-1.,1.30824393907473));
#37801=CARTESIAN_POINT('Ctrl Pts',(1.54159462645432,-1.,1.30630475189556));
#37802=CARTESIAN_POINT('Ctrl Pts',(1.53582981268977,-1.,1.30432735639489));
#37803=CARTESIAN_POINT('Ctrl Pts',(1.53009970283891,-1.,1.30231064395568));
#37804=CARTESIAN_POINT('Ctrl Pts',(1.52439957861062,-1.,1.30024984366328));
#37805=CARTESIAN_POINT('Ctrl Pts',(1.51872184912724,-1.,1.29813791800747));
#37806=CARTESIAN_POINT('Ctrl Pts',(1.51305994241402,-1.,1.29596850710509));
#37807=CARTESIAN_POINT('Ctrl Pts',(1.50741159078365,-1.,1.29373841372842));
#37808=CARTESIAN_POINT('Ctrl Pts',(1.50178230149776,-1.,1.29145022885181));
#37809=CARTESIAN_POINT('Ctrl Pts',(1.49618896881754,-1.,1.28911506584254));
#37810=CARTESIAN_POINT('Ctrl Pts',(1.4906522831278,-1.,1.2867467611644));
#37811=CARTESIAN_POINT('Ctrl Pts',(1.4851881711891,-1.,1.28435533880201));
#37812=CARTESIAN_POINT('Ctrl Pts',(1.47980070347095,-1.,1.28194158939517));
#37813=CARTESIAN_POINT('Ctrl Pts',(1.4744717526707,-1.,1.2794891824849));
#37814=CARTESIAN_POINT('Ctrl Pts',(1.46916035917133,-1.,1.2769641483109));
#37815=CARTESIAN_POINT('Ctrl Pts',(1.46382431332476,-1.,1.27433119897822));
#37816=CARTESIAN_POINT('Ctrl Pts',(1.45843906294697,-1.,1.27156805265289));
#37817=CARTESIAN_POINT('Ctrl Pts',(1.45301422764247,-1.,1.2686778680489));
#37818=CARTESIAN_POINT('Ctrl Pts',(1.44761985001662,-1.,1.26570925118868));
#37819=CARTESIAN_POINT('Ctrl Pts',(1.44236470511303,-1.,1.26273903323859));
#37820=CARTESIAN_POINT('Ctrl Pts',(1.43734919180847,-1.,1.25983531012005));
#37821=CARTESIAN_POINT('Ctrl Pts',(1.43262645609691,-1.,1.25702687965755));
#37822=CARTESIAN_POINT('Ctrl Pts',(1.42815938799387,-1.,1.25426945222639));
#37823=CARTESIAN_POINT('Ctrl Pts',(1.42378102115575,-1.,1.2514145557001));
#37824=CARTESIAN_POINT('Ctrl Pts',(1.41923722596025,-1.,1.24824430986571));
#37825=CARTESIAN_POINT('Ctrl Pts',(1.41422913175179,-1.,1.24450600513056));
#37826=CARTESIAN_POINT('Ctrl Pts',(1.40845295531283,-1.,1.23994455029534));
#37827=CARTESIAN_POINT('Ctrl Pts',(1.40164708206106,-1.,1.23434087290423));
#37828=CARTESIAN_POINT('Ctrl Pts',(1.39361389568796,-1.,1.22752961899387));
#37829=CARTESIAN_POINT('Ctrl Pts',(1.38420564527715,-1.,1.21938737280852));
#37830=CARTESIAN_POINT('Ctrl Pts',(1.37331915607905,-1.,1.20982812925645));
#37831=CARTESIAN_POINT('Ctrl Pts',(1.36088705043885,-1.,1.1987959077932));
#37832=CARTESIAN_POINT('Ctrl Pts',(1.34687054001093,-1.,1.18625865667441));
#37833=CARTESIAN_POINT('Ctrl Pts',(1.33437539347008,-1.,1.17501305789857));
#37834=CARTESIAN_POINT('Ctrl Pts',(1.32428080721772,-1.,1.16589330093588));
#37835=CARTESIAN_POINT('Ctrl Pts',(1.31722977216397,-1.,1.15950888730809));
#37836=CARTESIAN_POINT('Ctrl Pts',(1.31362392696032,-1.,1.15624053661742));
#37837=CARTESIAN_POINT('',(1.15624053661742,-1.,1.31362392696033));
#37838=CARTESIAN_POINT('Origin',(0.,-1.,0.));
#37839=CARTESIAN_POINT('',(1.34869019493419,-1.,1.73811241238545));
#37840=CARTESIAN_POINT('Ctrl Pts',(1.15624053661742,-1.,1.31362392696033));
#37841=CARTESIAN_POINT('Ctrl Pts',(1.15950888730433,-1.,1.3172297721596));
#37842=CARTESIAN_POINT('Ctrl Pts',(1.16589330092532,-1.,1.32428080720544));
#37843=CARTESIAN_POINT('Ctrl Pts',(1.17501305787994,-1.,1.33437539344842));
#37844=CARTESIAN_POINT('Ctrl Pts',(1.18625865664915,-1.,1.34687053998157));
#37845=CARTESIAN_POINT('Ctrl Pts',(1.1987959077656,-1.,1.36088705040677));
#37846=CARTESIAN_POINT('Ctrl Pts',(1.20982812923113,-1.,1.37331915604962));
#37847=CARTESIAN_POINT('Ctrl Pts',(1.21938737278853,-1.,1.38420564525391));
#37848=CARTESIAN_POINT('Ctrl Pts',(1.22752961898063,-1.,1.39361389567257));
#37849=CARTESIAN_POINT('Ctrl Pts',(1.23434087289768,-1.,1.40164708205345));
#37850=CARTESIAN_POINT('Ctrl Pts',(1.23994455029421,-1.,1.40845295531151));
#37851=CARTESIAN_POINT('Ctrl Pts',(1.24450600513278,-1.,1.41422913175437));
#37852=CARTESIAN_POINT('Ctrl Pts',(1.24824430986911,-1.,1.41923722596421));
#37853=CARTESIAN_POINT('Ctrl Pts',(1.25141455570299,-1.,1.42378102115911));
#37854=CARTESIAN_POINT('Ctrl Pts',(1.25426945222783,-1.,1.42815938799555));
#37855=CARTESIAN_POINT('Ctrl Pts',(1.25702687965744,-1.,1.43262645609679));
#37856=CARTESIAN_POINT('Ctrl Pts',(1.25983531011894,-1.,1.43734919180719));
#37857=CARTESIAN_POINT('Ctrl Pts',(1.26273903323723,-1.,1.44236470511145));
#37858=CARTESIAN_POINT('Ctrl Pts',(1.26570925118767,-1.,1.44761985001544));
#37859=CARTESIAN_POINT('Ctrl Pts',(1.26867786804854,-1.,1.45301422764205));
#37860=CARTESIAN_POINT('Ctrl Pts',(1.27156805265312,-1.,1.45843906294725));
#37861=CARTESIAN_POINT('Ctrl Pts',(1.27433119897877,-1.,1.4638243133254));
#37862=CARTESIAN_POINT('Ctrl Pts',(1.27696414831144,-1.,1.46916035917197));
#37863=CARTESIAN_POINT('Ctrl Pts',(1.27948918248524,-1.,1.4744717526711));
#37864=CARTESIAN_POINT('Ctrl Pts',(1.28194158939522,-1.,1.47980070347102));
#37865=CARTESIAN_POINT('Ctrl Pts',(1.28435533880184,-1.,1.48518817118891));
#37866=CARTESIAN_POINT('Ctrl Pts',(1.28674676116415,-1.,1.4906522831275));
#37867=CARTESIAN_POINT('Ctrl Pts',(1.28911506584232,-1.,1.49618896881729));
#37868=CARTESIAN_POINT('Ctrl Pts',(1.29145022885171,-1.,1.50178230149764));
#37869=CARTESIAN_POINT('Ctrl Pts',(1.29373841372843,-1.,1.50741159078367));
#37870=CARTESIAN_POINT('Ctrl Pts',(1.29596850710518,-1.,1.51305994241412));
#37871=CARTESIAN_POINT('Ctrl Pts',(1.29813791800757,-1.,1.51872184912735));
#37872=CARTESIAN_POINT('Ctrl Pts',(1.30024984366334,-1.,1.5243995786107));
#37873=CARTESIAN_POINT('Ctrl Pts',(1.3023106439557,-1.,1.53009970283893));
#37874=CARTESIAN_POINT('Ctrl Pts',(1.30432735639487,-1.,1.53582981268976));
#37875=CARTESIAN_POINT('Ctrl Pts',(1.30630475189553,-1.,1.54159462645428));
#37876=CARTESIAN_POINT('Ctrl Pts',(1.30824393907471,-1.,1.54739413957183));
#37877=CARTESIAN_POINT('Ctrl Pts',(1.31014393684221,-1.,1.55322568759481));
#37878=CARTESIAN_POINT('Ctrl Pts',(1.31200264341696,-1.,1.55908521254822));
#37879=CARTESIAN_POINT('Ctrl Pts',(1.31381795281002,-1.,1.56496872402352));
#37880=CARTESIAN_POINT('Ctrl Pts',(1.31558903860015,-1.,1.57087397835721));
#37881=CARTESIAN_POINT('Ctrl Pts',(1.31731642317183,-1.,1.57680056505585));
#37882=CARTESIAN_POINT('Ctrl Pts',(1.31900135021428,-1.,1.58274907898829));
#37883=CARTESIAN_POINT('Ctrl Pts',(1.32064537110891,-1.,1.58872057258244));
#37884=CARTESIAN_POINT('Ctrl Pts',(1.32224985747686,-1.,1.59471591079408));
#37885=CARTESIAN_POINT('Ctrl Pts',(1.32381550858266,-1.,1.600735118587));
#37886=CARTESIAN_POINT('Ctrl Pts',(1.32534250785794,-1.,1.6067775829097));
#37887=CARTESIAN_POINT('Ctrl Pts',(1.32683074483365,-1.,1.61284234015762));
#37888=CARTESIAN_POINT('Ctrl Pts',(1.32828000610448,-1.,1.61892832270723));
#37889=CARTESIAN_POINT('Ctrl Pts',(1.32969019505665,-1.,1.62503464209777));
#37890=CARTESIAN_POINT('Ctrl Pts',(1.33106149345618,-1.,1.63116079730887));
#37891=CARTESIAN_POINT('Ctrl Pts',(1.33239425103694,-1.,1.6373065347505));
#37892=CARTESIAN_POINT('Ctrl Pts',(1.33368890676554,-1.,1.64347174856007));
#37893=CARTESIAN_POINT('Ctrl Pts',(1.33494590468003,-1.,1.64965637286843));
#37894=CARTESIAN_POINT('Ctrl Pts',(1.33616559745217,-1.,1.65586025952651));
#37895=CARTESIAN_POINT('Ctrl Pts',(1.33734820885331,-1.,1.66208312542073));
#37896=CARTESIAN_POINT('Ctrl Pts',(1.33849388654458,-1.,1.66832460784078));
#37897=CARTESIAN_POINT('Ctrl Pts',(1.33960273470372,-1.,1.67458429426126));
#37898=CARTESIAN_POINT('Ctrl Pts',(1.3406748518516,-1.,1.68086176030308));
#37899=CARTESIAN_POINT('Ctrl Pts',(1.34171037484673,-1.,1.68715660868602));
#37900=CARTESIAN_POINT('Ctrl Pts',(1.34270948206139,-1.,1.6934684849664));
#37901=CARTESIAN_POINT('Ctrl Pts',(1.34367237124322,-1.,1.69979707754221));
#37902=CARTESIAN_POINT('Ctrl Pts',(1.34459924533783,-1.,1.70614212266676));
#37903=CARTESIAN_POINT('Ctrl Pts',(1.34549029589563,-1.,1.71250340687011));
#37904=CARTESIAN_POINT('Ctrl Pts',(1.34634568653586,-1.,1.7188807715095));
#37905=CARTESIAN_POINT('Ctrl Pts',(1.34716554820013,-1.,1.72527410681298));
#37906=CARTESIAN_POINT('Ctrl Pts',(1.3477930915247,-1.,1.73040149654497));
#37907=CARTESIAN_POINT('Ctrl Pts',(1.34824783113158,-1.,1.73425417886255));
#37908=CARTESIAN_POINT('Ctrl Pts',(1.34854391898145,-1.,1.73682580585819));
#37909=CARTESIAN_POINT('Ctrl Pts',(1.34869019493419,-1.,1.73811241238545));
#37910=CARTESIAN_POINT('',(1.23627494547115,-1.,1.81978687191668));
#37911=CARTESIAN_POINT('',(1.34869019493419,-1.,1.73811241238545));
#37912=CARTESIAN_POINT('',(0.892032620296855,-1.,1.5055822144029));
#37913=CARTESIAN_POINT('Ctrl Pts',(1.23627494547115,-1.,1.81978687191668));
#37914=CARTESIAN_POINT('Ctrl Pts',(1.23509651170384,-1.,1.81925017193531));
#37915=CARTESIAN_POINT('Ctrl Pts',(1.23274224526804,-1.,1.81817389920914));
#37916=CARTESIAN_POINT('Ctrl Pts',(1.22921864890975,-1.,1.81655087183054));
#37917=CARTESIAN_POINT('Ctrl Pts',(1.22453613304507,-1.,1.81436959209778));
#37918=CARTESIAN_POINT('Ctrl Pts',(1.2187090610323,-1.,1.81161420806172));
#37919=CARTESIAN_POINT('Ctrl Pts',(1.2129081570818,-1.,1.80882996916931));
#37920=CARTESIAN_POINT('Ctrl Pts',(1.20713356605519,-1.,1.80601678480772));
#37921=CARTESIAN_POINT('Ctrl Pts',(1.2013854893912,-1.,1.8031745483882));
#37922=CARTESIAN_POINT('Ctrl Pts',(1.19566418930405,-1.,1.80030314370121));
#37923=CARTESIAN_POINT('Ctrl Pts',(1.1899699793456,-1.,1.79740245923649));
#37924=CARTESIAN_POINT('Ctrl Pts',(1.18430321697471,-1.,1.79447240321572));
#37925=CARTESIAN_POINT('Ctrl Pts',(1.17866429440781,-1.,1.79151291552646));
#37926=CARTESIAN_POINT('Ctrl Pts',(1.17305363177265,-1.,1.78852398877523));
#37927=CARTESIAN_POINT('Ctrl Pts',(1.16747166312239,-1.,1.78550566040349));
#37928=CARTESIAN_POINT('Ctrl Pts',(1.16191881298458,-1.,1.78245795880949));
#37929=CARTESIAN_POINT('Ctrl Pts',(1.15639547194689,-1.,1.77938085564261));
#37930=CARTESIAN_POINT('Ctrl Pts',(1.15090197841531,-1.,1.77627422557034));
#37931=CARTESIAN_POINT('Ctrl Pts',(1.14543858226948,-1.,1.77313777896234));
#37932=CARTESIAN_POINT('Ctrl Pts',(1.14000548337,-1.,1.76997111386806));
#37933=CARTESIAN_POINT('Ctrl Pts',(1.13460291804634,-1.,1.76677384551883));
#37934=CARTESIAN_POINT('Ctrl Pts',(1.12923123555076,-1.,1.76354571966171));
#37935=CARTESIAN_POINT('Ctrl Pts',(1.12389096855078,-1.,1.76028671825084));
#37936=CARTESIAN_POINT('Ctrl Pts',(1.11858293216752,-1.,1.75699720772089));
#37937=CARTESIAN_POINT('Ctrl Pts',(1.11330807582542,-1.,1.75367772094617));
#37938=CARTESIAN_POINT('Ctrl Pts',(1.10806728183003,-1.,1.75032866075914));
#37939=CARTESIAN_POINT('Ctrl Pts',(1.10286118991144,-1.,1.74695004214924));
#37940=CARTESIAN_POINT('Ctrl Pts',(1.09768999241229,-1.,1.74354119236212));
#37941=CARTESIAN_POINT('Ctrl Pts',(1.09255329056496,-1.,1.74010053962252));
#37942=CARTESIAN_POINT('Ctrl Pts',(1.08745056285429,-1.,1.73662628326093));
#37943=CARTESIAN_POINT('Ctrl Pts',(1.08238162784749,-1.,1.73311705663407));
#37944=CARTESIAN_POINT('Ctrl Pts',(1.0773470373727,-1.,1.72957248977424));
#37945=CARTESIAN_POINT('Ctrl Pts',(1.07234866990252,-1.,1.72599406198489));
#37946=CARTESIAN_POINT('Ctrl Pts',(1.06738966975463,-1.,1.72238500928456));
#37947=CARTESIAN_POINT('Ctrl Pts',(1.06247324680649,-1.,1.71874858456908));
#37948=CARTESIAN_POINT('Ctrl Pts',(1.05760163192481,-1.,1.71508654427022));
#37949=CARTESIAN_POINT('Ctrl Pts',(1.05277517202853,-1.,1.71139783543986));
#37950=CARTESIAN_POINT('Ctrl Pts',(1.0479908540499,-1.,1.70767646263641));
#37951=CARTESIAN_POINT('Ctrl Pts',(1.04324363334546,-1.,1.70391338707969));
#37952=CARTESIAN_POINT('Ctrl Pts',(1.03852922490782,-1.,1.70010052930951));
#37953=CARTESIAN_POINT('Ctrl Pts',(1.03384646003587,-1.,1.69623414782769));
#37954=CARTESIAN_POINT('Ctrl Pts',(1.02919977579155,-1.,1.69231840863471));
#37955=CARTESIAN_POINT('Ctrl Pts',(1.02460180535272,-1.,1.68836910178475));
#37956=CARTESIAN_POINT('Ctrl Pts',(1.02006795074222,-1.,1.68440578021739));
#37957=CARTESIAN_POINT('Ctrl Pts',(1.01561026162786,-1.,1.6804428989482));
#37958=CARTESIAN_POINT('Ctrl Pts',(1.01123236493507,-1.,1.67648246776457));
#37959=CARTESIAN_POINT('Ctrl Pts',(1.00692206696387,-1.,1.67250335383248));
#37960=CARTESIAN_POINT('Ctrl Pts',(1.00265091003682,-1.,1.66846059277231));
#37961=CARTESIAN_POINT('Ctrl Pts',(0.998389654952317,-1.,1.66430758030304));
#37962=CARTESIAN_POINT('Ctrl Pts',(0.994121836661115,-1.,1.66001553809916));
#37963=CARTESIAN_POINT('Ctrl Pts',(0.98985562785445,-1.,1.65559044289746));
#37964=CARTESIAN_POINT('Ctrl Pts',(0.985642622921626,-1.,1.6511001661277));
#37965=CARTESIAN_POINT('Ctrl Pts',(0.981562530940574,-1.,1.64665139190834));
#37966=CARTESIAN_POINT('Ctrl Pts',(0.977689794120296,-1.,1.64233990826831));
#37967=CARTESIAN_POINT('Ctrl Pts',(0.974066058287501,-1.,1.63820952658157));
#37968=CARTESIAN_POINT('Ctrl Pts',(0.970669715996356,-1.,1.63420665729609));
#37969=CARTESIAN_POINT('Ctrl Pts',(0.967387853228041,-1.,1.63013849959083));
#37970=CARTESIAN_POINT('Ctrl Pts',(0.964046107037821,-1.,1.6257193066974));
#37971=CARTESIAN_POINT('Ctrl Pts',(0.960438326099958,-1.,1.62061638139929));
#37972=CARTESIAN_POINT('Ctrl Pts',(0.956354422921572,-1.,1.61449324337233));
#37973=CARTESIAN_POINT('Ctrl Pts',(0.951613284361247,-1.,1.60706069897794));
#37974=CARTESIAN_POINT('Ctrl Pts',(0.946078063325795,-1.,1.59810042045408));
#37975=CARTESIAN_POINT('Ctrl Pts',(0.939646377909319,-1.,1.58744937489796));
#37976=CARTESIAN_POINT('Ctrl Pts',(0.932246680128848,-1.,1.57499388385561));
#37977=CARTESIAN_POINT('Ctrl Pts',(0.923832188966322,-1.,1.56065988582509));
#37978=CARTESIAN_POINT('Ctrl Pts',(0.914375919046579,-1.,1.54440491152808));
#37979=CARTESIAN_POINT('Ctrl Pts',(0.905967409640498,-1.,1.52984849890434));
#37980=CARTESIAN_POINT('Ctrl Pts',(0.89918504749193,-1.,1.51805569591479));
#37981=CARTESIAN_POINT('Ctrl Pts',(0.894452006967538,-1.,1.50980486807181));
#37982=CARTESIAN_POINT('Ctrl Pts',(0.892032620296855,-1.,1.5055822144029));
#37983=CARTESIAN_POINT('',(0.693717979106305,-1.,1.60662857109684));
#37984=CARTESIAN_POINT('Origin',(0.,-1.,0.));
#37985=CARTESIAN_POINT('',(0.7455743247944,-1.,2.0698113262342));
#37986=CARTESIAN_POINT('Ctrl Pts',(0.693717979106305,-1.,1.60662857109684));
#37987=CARTESIAN_POINT('Ctrl Pts',(0.69571209787897,-1.,1.61106790957619));
#37988=CARTESIAN_POINT('Ctrl Pts',(0.699605146398836,-1.,1.61974673471117));
#37989=CARTESIAN_POINT('Ctrl Pts',(0.705159151977294,-1.,1.6321654166204));
#37990=CARTESIAN_POINT('Ctrl Pts',(0.711993139340447,-1.,1.64752408828442));
#37991=CARTESIAN_POINT('Ctrl Pts',(0.719585433787949,-1.,1.66472880551777));
#37992=CARTESIAN_POINT('Ctrl Pts',(0.726235967982445,-1.,1.67996158451922));
#37993=CARTESIAN_POINT('Ctrl Pts',(0.731963238685357,-1.,1.69326921972915));
#37994=CARTESIAN_POINT('Ctrl Pts',(0.736799665716932,-1.,1.70473309004249));
#37995=CARTESIAN_POINT('Ctrl Pts',(0.74079516202821,-1.,1.71447789751001));
#37996=CARTESIAN_POINT('Ctrl Pts',(0.744021445433093,-1.,1.72268229916769));
#37997=CARTESIAN_POINT('Ctrl Pts',(0.746574710097752,-1.,1.72958533647714));
#37998=CARTESIAN_POINT('Ctrl Pts',(0.74858246295687,-1.,1.7355035168033));
#37999=CARTESIAN_POINT('Ctrl Pts',(0.750193435981249,-1.,1.74080458267114));
#38000=CARTESIAN_POINT('Ctrl Pts',(0.751555614164482,-1.,1.74585086852502));
#38001=CARTESIAN_POINT('Ctrl Pts',(0.752797683531314,-1.,1.75095139468794));
#38002=CARTESIAN_POINT('Ctrl Pts',(0.754009254027828,-1.,1.75631083600019));
#38003=CARTESIAN_POINT('Ctrl Pts',(0.755220979974461,-1.,1.76197817240128));
#38004=CARTESIAN_POINT('Ctrl Pts',(0.75642189602781,-1.,1.76789396002998));
#38005=CARTESIAN_POINT('Ctrl Pts',(0.757578264077028,-1.,1.77394167108292));
#38006=CARTESIAN_POINT('Ctrl Pts',(0.758650626677518,-1.,1.77999411220945));
#38007=CARTESIAN_POINT('Ctrl Pts',(0.759614401110189,-1.,1.78596964884604));
#38008=CARTESIAN_POINT('Ctrl Pts',(0.760469555880749,-1.,1.7918581561088));
#38009=CARTESIAN_POINT('Ctrl Pts',(0.761229695230558,-1.,1.79768986997783));
#38010=CARTESIAN_POINT('Ctrl Pts',(0.761915336443547,-1.,1.80351583877342));
#38011=CARTESIAN_POINT('Ctrl Pts',(0.762546129463938,-1.,1.80938551463965));
#38012=CARTESIAN_POINT('Ctrl Pts',(0.763132003836634,-1.,1.8153211840553));
#38013=CARTESIAN_POINT('Ctrl Pts',(0.763673465462726,-1.,1.82131873145266));
#38014=CARTESIAN_POINT('Ctrl Pts',(0.764165902605995,-1.,1.82735991200065));
#38015=CARTESIAN_POINT('Ctrl Pts',(0.764602549687853,-1.,1.83342077227142));
#38016=CARTESIAN_POINT('Ctrl Pts',(0.764978057881737,-1.,1.83948181064835));
#38017=CARTESIAN_POINT('Ctrl Pts',(0.765291664862029,-1.,1.84553698875924));
#38018=CARTESIAN_POINT('Ctrl Pts',(0.765545710619062,-1.,1.85158945130063));
#38019=CARTESIAN_POINT('Ctrl Pts',(0.765744212909318,-1.,1.85764741390394));
#38020=CARTESIAN_POINT('Ctrl Pts',(0.765891519092547,-1.,1.86372027063312));
#38021=CARTESIAN_POINT('Ctrl Pts',(0.765990708546091,-1.,1.86981398314341));
#38022=CARTESIAN_POINT('Ctrl Pts',(0.766042837036744,-1.,1.87592888967883));
#38023=CARTESIAN_POINT('Ctrl Pts',(0.766047794851864,-1.,1.88206215302561));
#38024=CARTESIAN_POINT('Ctrl Pts',(0.766004837062091,-1.,1.88820926433409));
#38025=CARTESIAN_POINT('Ctrl Pts',(0.765913193856978,-1.,1.89436577771388));
#38026=CARTESIAN_POINT('Ctrl Pts',(0.765772772593386,-1.,1.90052930393596));
#38027=CARTESIAN_POINT('Ctrl Pts',(0.765584196937919,-1.,1.90669961402356));
#38028=CARTESIAN_POINT('Ctrl Pts',(0.765348465884722,-1.,1.91287765805169));
#38029=CARTESIAN_POINT('Ctrl Pts',(0.765066729667088,-1.,1.91906491634196));
#38030=CARTESIAN_POINT('Ctrl Pts',(0.764740025488211,-1.,1.92526263537048));
#38031=CARTESIAN_POINT('Ctrl Pts',(0.76436901067394,-1.,1.93147105496382));
#38032=CARTESIAN_POINT('Ctrl Pts',(0.763954049121458,-1.,1.93768964875886));
#38033=CARTESIAN_POINT('Ctrl Pts',(0.763495333538629,-1.,1.9439174661764));
#38034=CARTESIAN_POINT('Ctrl Pts',(0.762992990878769,-1.,1.95015342590024));
#38035=CARTESIAN_POINT('Ctrl Pts',(0.762447203806178,-1.,1.95639665309869));
#38036=CARTESIAN_POINT('Ctrl Pts',(0.761858300014423,-1.,1.96264672744186));
#38037=CARTESIAN_POINT('Ctrl Pts',(0.76122669048382,-1.,1.96890351582499));
#38038=CARTESIAN_POINT('Ctrl Pts',(0.760552825409757,-1.,1.97516705321494));
#38039=CARTESIAN_POINT('Ctrl Pts',(0.75983714745219,-1.,1.98143741418172));
#38040=CARTESIAN_POINT('Ctrl Pts',(0.759080037802488,-1.,1.98771456680874));
#38041=CARTESIAN_POINT('Ctrl Pts',(0.758281796766761,-1.,1.99399831098817));
#38042=CARTESIAN_POINT('Ctrl Pts',(0.757442676862724,-1.,2.00028834739178));
#38043=CARTESIAN_POINT('Ctrl Pts',(0.75656290464667,-1.,2.0065843158773));
#38044=CARTESIAN_POINT('Ctrl Pts',(0.755642704957865,-1.,2.01288584328084));
#38045=CARTESIAN_POINT('Ctrl Pts',(0.754682330722816,-1.,2.01919259405809));
#38046=CARTESIAN_POINT('Ctrl Pts',(0.753682061112768,-1.,2.02550428623313));
#38047=CARTESIAN_POINT('Ctrl Pts',(0.75264218048721,-1.,2.03182068456221));
#38048=CARTESIAN_POINT('Ctrl Pts',(0.751562963361115,-1.,2.03814160092099));
#38049=CARTESIAN_POINT('Ctrl Pts',(0.750444657875575,-1.,2.04446689147979));
#38050=CARTESIAN_POINT('Ctrl Pts',(0.749287468665046,-1.,2.05079645592154));
#38051=CARTESIAN_POINT('Ctrl Pts',(0.748091554183802,-1.,2.05713023031007));
#38052=CARTESIAN_POINT('Ctrl Pts',(0.747103932787919,-1.,2.06220058927826));
#38053=CARTESIAN_POINT('Ctrl Pts',(0.7463458715442,-1.,2.06600523016815));
#38054=CARTESIAN_POINT('Ctrl Pts',(0.745832791378367,-1.,2.06854248895728));
#38055=CARTESIAN_POINT('Ctrl Pts',(0.7455743247944,-1.,2.0698113262342));
#38056=CARTESIAN_POINT('',(0.61342227326009,-1.,2.11275013067528));
#38057=CARTESIAN_POINT('',(0.7455743247944,-1.,2.0698113262342));
#38058=CARTESIAN_POINT('',(0.383122945602004,-1.,1.7075470150345));
#38059=CARTESIAN_POINT('Ctrl Pts',(0.61342227326009,-1.,2.11275013067528));
#38060=CARTESIAN_POINT('Ctrl Pts',(0.6124673655618,-1.,2.11187554259986));
#38061=CARTESIAN_POINT('Ctrl Pts',(0.610560911689898,-1.,2.11012443807238));
#38062=CARTESIAN_POINT('Ctrl Pts',(0.607711315454876,-1.,2.1074919961518));
#38063=CARTESIAN_POINT('Ctrl Pts',(0.60393203073603,-1.,2.10397049886949));
#38064=CARTESIAN_POINT('Ctrl Pts',(0.599241616420533,-1.,2.0995493086477));
#38065=CARTESIAN_POINT('Ctrl Pts',(0.594585006052162,-1.,2.0951087622027));
#38066=CARTESIAN_POINT('Ctrl Pts',(0.589962365403406,-1.,2.09064881812129));
#38067=CARTESIAN_POINT('Ctrl Pts',(0.585373918991617,-1.,2.08616943727951));
#38068=CARTESIAN_POINT('Ctrl Pts',(0.580819952108063,-1.,2.08167059018418));
#38069=CARTESIAN_POINT('Ctrl Pts',(0.576300797416844,-1.,2.07715226767559));
#38070=CARTESIAN_POINT('Ctrl Pts',(0.571816823242602,-1.,2.07261449292824));
#38071=CARTESIAN_POINT('Ctrl Pts',(0.567368421181087,-1.,2.06805732997334));
#38072=CARTESIAN_POINT('Ctrl Pts',(0.562955993082261,-1.,2.06348090160589));
#38073=CARTESIAN_POINT('Ctrl Pts',(0.558579940185151,-1.,2.05888537756462));
#38074=CARTESIAN_POINT('Ctrl Pts',(0.554240657463906,-1.,2.05427091604413));
#38075=CARTESIAN_POINT('Ctrl Pts',(0.549938525150295,-1.,2.04963761077958));
#38076=CARTESIAN_POINT('Ctrl Pts',(0.54567390381743,-1.,2.04498544714588));
#38077=CARTESIAN_POINT('Ctrl Pts',(0.541447120615659,-1.,2.04031422690527));
#38078=CARTESIAN_POINT('Ctrl Pts',(0.537258489833262,-1.,2.03562362954037));
#38079=CARTESIAN_POINT('Ctrl Pts',(0.533108355132976,-1.,2.03091336214426));
#38080=CARTESIAN_POINT('Ctrl Pts',(0.528997127241914,-1.,2.0261832908329));
#38081=CARTESIAN_POINT('Ctrl Pts',(0.524925318333476,-1.,2.02143356304698));
#38082=CARTESIAN_POINT('Ctrl Pts',(0.52089359039937,-1.,2.01666477917286));
#38083=CARTESIAN_POINT('Ctrl Pts',(0.516902681728687,-1.,2.01187773939242));
#38084=CARTESIAN_POINT('Ctrl Pts',(0.512953306961792,-1.,2.00707309946949));
#38085=CARTESIAN_POINT('Ctrl Pts',(0.509046069886157,-1.,2.00225107134734));
#38086=CARTESIAN_POINT('Ctrl Pts',(0.505181361323026,-1.,1.99741107463572));
#38087=CARTESIAN_POINT('Ctrl Pts',(0.501359287727146,-1.,1.99255149126155));
#38088=CARTESIAN_POINT('Ctrl Pts',(0.497579909545574,-1.,1.98767044752932));
#38089=CARTESIAN_POINT('Ctrl Pts',(0.493843476541494,-1.,1.98276658761821));
#38090=CARTESIAN_POINT('Ctrl Pts',(0.490150627860952,-1.,1.97783973019229));
#38091=CARTESIAN_POINT('Ctrl Pts',(0.486502692907658,-1.,1.97289186263272));
#38092=CARTESIAN_POINT('Ctrl Pts',(0.48290166212069,-1.,1.96792703422362));
#38093=CARTESIAN_POINT('Ctrl Pts',(0.479349583074855,-1.,1.96294933055943));
#38094=CARTESIAN_POINT('Ctrl Pts',(0.475848034683176,-1.,1.95796111148177));
#38095=CARTESIAN_POINT('Ctrl Pts',(0.472397672264072,-1.,1.95296148278133));
#38096=CARTESIAN_POINT('Ctrl Pts',(0.468997482913135,-1.,1.94794381136514));
#38097=CARTESIAN_POINT('Ctrl Pts',(0.46564546202603,-1.,1.9428979419619));
#38098=CARTESIAN_POINT('Ctrl Pts',(0.462340031009056,-1.,1.93781486640821));
#38099=CARTESIAN_POINT('Ctrl Pts',(0.459081234547926,-1.,1.93269066517934));
#38100=CARTESIAN_POINT('Ctrl Pts',(0.45587200517437,-1.,1.92753067150476));
#38101=CARTESIAN_POINT('Ctrl Pts',(0.452719478359432,-1.,1.92235380648502));
#38102=CARTESIAN_POINT('Ctrl Pts',(0.449632260106662,-1.,1.91718342555755));
#38103=CARTESIAN_POINT('Ctrl Pts',(0.446617343485711,-1.,1.9120369998112));
#38104=CARTESIAN_POINT('Ctrl Pts',(0.44367755684915,-1.,1.90691756144898));
#38105=CARTESIAN_POINT('Ctrl Pts',(0.440807833704038,-1.,1.90180124389086));
#38106=CARTESIAN_POINT('Ctrl Pts',(0.437995003948244,-1.,1.89663648956466));
#38107=CARTESIAN_POINT('Ctrl Pts',(0.435225660963383,-1.,1.89136993975504));
#38108=CARTESIAN_POINT('Ctrl Pts',(0.432493038548748,-1.,1.88596913666793));
#38109=CARTESIAN_POINT('Ctrl Pts',(0.429803062482344,-1.,1.88044229001832));
#38110=CARTESIAN_POINT('Ctrl Pts',(0.427183828519102,-1.,1.87486989291484));
#38111=CARTESIAN_POINT('Ctrl Pts',(0.424678177291358,-1.,1.86937803944323));
#38112=CARTESIAN_POINT('Ctrl Pts',(0.422327307418275,-1.,1.86408083334028));
#38113=CARTESIAN_POINT('Ctrl Pts',(0.420157287975619,-1.,1.85903281096686));
#38114=CARTESIAN_POINT('Ctrl Pts',(0.418164129143534,-1.,1.85417632856234));
#38115=CARTESIAN_POINT('Ctrl Pts',(0.416300022038864,-1.,1.84929312929882));
#38116=CARTESIAN_POINT('Ctrl Pts',(0.41448743825434,-1.,1.8440575707371));
#38117=CARTESIAN_POINT('Ctrl Pts',(0.412633125322161,-1.,1.83808953475839));
#38118=CARTESIAN_POINT('Ctrl Pts',(0.410641256301674,-1.,1.83100408895216));
#38119=CARTESIAN_POINT('Ctrl Pts',(0.408428948108533,-1.,1.8224702267854));
#38120=CARTESIAN_POINT('Ctrl Pts',(0.405933518411838,-1.,1.81223801813988));
#38121=CARTESIAN_POINT('Ctrl Pts',(0.403107976170441,-1.,1.80012077176221));
#38122=CARTESIAN_POINT('Ctrl Pts',(0.39991940378308,-1.,1.78598826347533));
#38123=CARTESIAN_POINT('Ctrl Pts',(0.39634619612042,-1.,1.7697556004756));
#38124=CARTESIAN_POINT('Ctrl Pts',(0.392375812294307,-1.,1.75137405313962));
#38125=CARTESIAN_POINT('Ctrl Pts',(0.388877023509191,-1.,1.7349317097561));
#38126=CARTESIAN_POINT('Ctrl Pts',(0.38607079032701,-1.,1.72162022246158));
#38127=CARTESIAN_POINT('Ctrl Pts',(0.384119047315541,-1.,1.71231062891958));
#38128=CARTESIAN_POINT('Ctrl Pts',(0.383122945602004,-1.,1.7075470150345));
#38129=CARTESIAN_POINT('',(0.163289472382896,-1.,1.74236521665491));
#38130=CARTESIAN_POINT('Origin',(0.,-1.,0.));
#38131=CARTESIAN_POINT('',(0.0694764450219578,-1.,2.19890268624765));
#38132=CARTESIAN_POINT('Ctrl Pts',(0.163289472382896,-1.,1.74236521665491));
#38133=CARTESIAN_POINT('Ctrl Pts',(0.163814161002002,-1.,1.7472034950333));
#38134=CARTESIAN_POINT('Ctrl Pts',(0.164834765707158,-1.,1.75666056638427));
#38135=CARTESIAN_POINT('Ctrl Pts',(0.1662793551464,-1.,1.77018771684844));
#38136=CARTESIAN_POINT('Ctrl Pts',(0.168032772805197,-1.,1.7869064998507));
#38137=CARTESIAN_POINT('Ctrl Pts',(0.169936923904608,-1.,1.80561530629706));
#38138=CARTESIAN_POINT('Ctrl Pts',(0.171554770204119,-1.,1.82215766811545));
#38139=CARTESIAN_POINT('Ctrl Pts',(0.1728894428919,-1.,1.83658380527692));
#38140=CARTESIAN_POINT('Ctrl Pts',(0.173946627587731,-1.,1.8489811319852));
#38141=CARTESIAN_POINT('Ctrl Pts',(0.17473525927603,-1.,1.85948367088837));
#38142=CARTESIAN_POINT('Ctrl Pts',(0.175268337590757,-1.,1.86828349694799));
#38143=CARTESIAN_POINT('Ctrl Pts',(0.175563480746485,-1.,1.87563767773588));
#38144=CARTESIAN_POINT('Ctrl Pts',(0.175644148889698,-1.,1.88188663145367));
#38145=CARTESIAN_POINT('Ctrl Pts',(0.175538155840648,-1.,1.88742606273259));
#38146=CARTESIAN_POINT('Ctrl Pts',(0.175274276190844,-1.,1.892646301985));
#38147=CARTESIAN_POINT('Ctrl Pts',(0.174879405091263,-1.,1.89788101117132));
#38148=CARTESIAN_POINT('Ctrl Pts',(0.174375518661085,-1.,1.90335253862834));
#38149=CARTESIAN_POINT('Ctrl Pts',(0.173776635257816,-1.,1.90911693975267));
#38150=CARTESIAN_POINT('Ctrl Pts',(0.173090695383496,-1.,1.91511429159527));
#38151=CARTESIAN_POINT('Ctrl Pts',(0.172321621259513,-1.,1.9212233439798));
#38152=CARTESIAN_POINT('Ctrl Pts',(0.171471191532988,-1.,1.92731093582036));
#38153=CARTESIAN_POINT('Ctrl Pts',(0.170541253116201,-1.,1.93329183155539));
#38154=CARTESIAN_POINT('Ctrl Pts',(0.16953490481749,-1.,1.93915639211581));
#38155=CARTESIAN_POINT('Ctrl Pts',(0.168455741607556,-1.,1.94493757756931));
#38156=CARTESIAN_POINT('Ctrl Pts',(0.167307501784475,-1.,1.95069027794294));
#38157=CARTESIAN_POINT('Ctrl Pts',(0.166093592002812,-1.,1.9564675971873));
#38158=CARTESIAN_POINT('Ctrl Pts',(0.164816568920269,-1.,1.96229379940136));
#38159=CARTESIAN_POINT('Ctrl Pts',(0.163478185457734,-1.,1.96816512677967));
#38160=CARTESIAN_POINT('Ctrl Pts',(0.162079693556288,-1.,1.97406280235188));
#38161=CARTESIAN_POINT('Ctrl Pts',(0.160622060784611,-1.,1.97996195437559));
#38162=CARTESIAN_POINT('Ctrl Pts',(0.159106226437299,-1.,1.98584238283292));
#38163=CARTESIAN_POINT('Ctrl Pts',(0.157533331459227,-1.,1.99169810931908));
#38164=CARTESIAN_POINT('Ctrl Pts',(0.155904629548783,-1.,1.99753284771497));
#38165=CARTESIAN_POINT('Ctrl Pts',(0.154221403049722,-1.,2.00335565310543));
#38166=CARTESIAN_POINT('Ctrl Pts',(0.152484883621449,-1.,2.00917680318424));
#38167=CARTESIAN_POINT('Ctrl Pts',(0.150696157673078,-1.,2.01500291940238));
#38168=CARTESIAN_POINT('Ctrl Pts',(0.148856124775337,-1.,2.02083464969894));
#38169=CARTESIAN_POINT('Ctrl Pts',(0.146965557332583,-1.,2.02666926182017));
#38170=CARTESIAN_POINT('Ctrl Pts',(0.145025140186057,-1.,2.03250223739942));
#38171=CARTESIAN_POINT('Ctrl Pts',(0.143035515058208,-1.,2.03832911025912));
#38172=CARTESIAN_POINT('Ctrl Pts',(0.140997332152546,-1.,2.04414757947916));
#38173=CARTESIAN_POINT('Ctrl Pts',(0.138911255368966,-1.,2.04995762001328));
#38174=CARTESIAN_POINT('Ctrl Pts',(0.136777941218043,-1.,2.05576044414264));
#38175=CARTESIAN_POINT('Ctrl Pts',(0.134598026192106,-1.,2.06155781517842));
#38176=CARTESIAN_POINT('Ctrl Pts',(0.13237211154771,-1.,2.06735123910326));
#38177=CARTESIAN_POINT('Ctrl Pts',(0.130100748328403,-1.,2.07314114713063));
#38178=CARTESIAN_POINT('Ctrl Pts',(0.12778444527612,-1.,2.07892715110987));
#38179=CARTESIAN_POINT('Ctrl Pts',(0.125423679412061,-1.,2.08470840653643));
#38180=CARTESIAN_POINT('Ctrl Pts',(0.123018905621083,-1.,2.09048392424825));
#38181=CARTESIAN_POINT('Ctrl Pts',(0.120570567965122,-1.,2.0962529286773));
#38182=CARTESIAN_POINT('Ctrl Pts',(0.118079107988355,-1.,2.102015121329));
#38183=CARTESIAN_POINT('Ctrl Pts',(0.115544957687926,-1.,2.10777050261309));
#38184=CARTESIAN_POINT('Ctrl Pts',(0.112968534419737,-1.,2.11351924490306));
#38185=CARTESIAN_POINT('Ctrl Pts',(0.110350236135025,-1.,2.11926155590865));
#38186=CARTESIAN_POINT('Ctrl Pts',(0.10769043523109,-1.,2.12499752307));
#38187=CARTESIAN_POINT('Ctrl Pts',(0.104989479152739,-1.,2.13072704887293));
#38188=CARTESIAN_POINT('Ctrl Pts',(0.1022477005561,-1.,2.13644992667165));
#38189=CARTESIAN_POINT('Ctrl Pts',(0.0994654261990913,-1.,2.14216588396025));
#38190=CARTESIAN_POINT('Ctrl Pts',(0.0966429852305456,-1.,2.14787463531795));
#38191=CARTESIAN_POINT('Ctrl Pts',(0.0937807218867641,-1.,2.1535759397817));
#38192=CARTESIAN_POINT('Ctrl Pts',(0.0908789888107263,-1.,2.15926961544516));
#38193=CARTESIAN_POINT('Ctrl Pts',(0.087938129138692,-1.,2.16495552645014));
#38194=CARTESIAN_POINT('Ctrl Pts',(0.084958462083537,-1.,2.17063357870952));
#38195=CARTESIAN_POINT('Ctrl Pts',(0.0819402680872763,-1.,2.176303712113));
#38196=CARTESIAN_POINT('Ctrl Pts',(0.078883772768524,-1.,2.18196589448887));
#38197=CARTESIAN_POINT('Ctrl Pts',(0.0757891465836145,-1.,2.1876201139953));
#38198=CARTESIAN_POINT('Ctrl Pts',(0.0732830357306722,-1.,2.19213712013662));
#38199=CARTESIAN_POINT('Ctrl Pts',(0.0713863779526151,-1.,2.19552129484002));
#38200=CARTESIAN_POINT('Ctrl Pts',(0.0701143536325487,-1.,2.19777582085423));
#38201=CARTESIAN_POINT('Ctrl Pts',(0.0694764450219578,-1.,2.19890268624765));
#38202=CARTESIAN_POINT('',(-0.0694764450219586,-1.,2.19890268624765));
#38203=CARTESIAN_POINT('',(0.0694764450219578,-1.,2.19890268624765));
#38204=CARTESIAN_POINT('',(-0.163289472382896,-1.,1.74236521665491));
#38205=CARTESIAN_POINT('Ctrl Pts',(-0.0694764450219586,-1.,2.19890268624765));
#38206=CARTESIAN_POINT('Ctrl Pts',(-0.0701143536324929,-1.,2.19777582085261));
#38207=CARTESIAN_POINT('Ctrl Pts',(-0.071386377952463,-1.,2.19552129483562));
#38208=CARTESIAN_POINT('Ctrl Pts',(-0.0732830357304279,-1.,2.19213712012956));
#38209=CARTESIAN_POINT('Ctrl Pts',(-0.0757891465833414,-1.,2.1876201139874));
#38210=CARTESIAN_POINT('Ctrl Pts',(-0.078883772768323,-1.,2.18196589448304));
#38211=CARTESIAN_POINT('Ctrl Pts',(-0.0819402680871942,-1.,2.1763037121106));
#38212=CARTESIAN_POINT('Ctrl Pts',(-0.0849584620835646,-1.,2.17063357871031));
#38213=CARTESIAN_POINT('Ctrl Pts',(-0.0879381291387825,-1.,2.16495552645275));
#38214=CARTESIAN_POINT('Ctrl Pts',(-0.0908789888108269,-1.,2.15926961544808));
#38215=CARTESIAN_POINT('Ctrl Pts',(-0.0937807218868348,-1.,2.15357593978377));
#38216=CARTESIAN_POINT('Ctrl Pts',(-0.0966429852305691,-1.,2.14787463531864));
#38217=CARTESIAN_POINT('Ctrl Pts',(-0.0994654261990745,-1.,2.14216588395974));
#38218=CARTESIAN_POINT('Ctrl Pts',(-0.102247700556064,-1.,2.13644992667052));
#38219=CARTESIAN_POINT('Ctrl Pts',(-0.104989479152703,-1.,2.1307270488718));
#38220=CARTESIAN_POINT('Ctrl Pts',(-0.107690435231068,-1.,2.12499752306927));
#38221=CARTESIAN_POINT('Ctrl Pts',(-0.11035023613502,-1.,2.11926155590849));
#38222=CARTESIAN_POINT('Ctrl Pts',(-0.112968534419746,-1.,2.11351924490335));
#38223=CARTESIAN_POINT('Ctrl Pts',(-0.115544957687941,-1.,2.10777050261359));
#38224=CARTESIAN_POINT('Ctrl Pts',(-0.118079107988368,-1.,2.10201512132945));
#38225=CARTESIAN_POINT('Ctrl Pts',(-0.120570567965129,-1.,2.09625292867756));
#38226=CARTESIAN_POINT('Ctrl Pts',(-0.123018905621083,-1.,2.09048392424826));
#38227=CARTESIAN_POINT('Ctrl Pts',(-0.125423679412058,-1.,2.08470840653628));
#38228=CARTESIAN_POINT('Ctrl Pts',(-0.127784445276116,-1.,2.07892715110967));
#38229=CARTESIAN_POINT('Ctrl Pts',(-0.130100748328401,-1.,2.07314114713047));
#38230=CARTESIAN_POINT('Ctrl Pts',(-0.13237211154771,-1.,2.06735123910319));
#38231=CARTESIAN_POINT('Ctrl Pts',(-0.134598026192107,-1.,2.06155781517844));
#38232=CARTESIAN_POINT('Ctrl Pts',(-0.136777941218044,-1.,2.0557604441427));
#38233=CARTESIAN_POINT('Ctrl Pts',(-0.138911255368966,-1.,2.04995762001333));
#38234=CARTESIAN_POINT('Ctrl Pts',(-0.140997332152546,-1.,2.04414757947919));
#38235=CARTESIAN_POINT('Ctrl Pts',(-0.143035515058208,-1.,2.03832911025913));
#38236=CARTESIAN_POINT('Ctrl Pts',(-0.145025140186058,-1.,2.03250223739941));
#38237=CARTESIAN_POINT('Ctrl Pts',(-0.146965557332586,-1.,2.02666926182017));
#38238=CARTESIAN_POINT('Ctrl Pts',(-0.148856124775343,-1.,2.02083464969897));
#38239=CARTESIAN_POINT('Ctrl Pts',(-0.150696157673084,-1.,2.01500291940243));
#38240=CARTESIAN_POINT('Ctrl Pts',(-0.152484883621452,-1.,2.00917680318426));
#38241=CARTESIAN_POINT('Ctrl Pts',(-0.154221403049719,-1.,2.00335565310539));
#38242=CARTESIAN_POINT('Ctrl Pts',(-0.155904629548775,-1.,1.99753284771487));
#38243=CARTESIAN_POINT('Ctrl Pts',(-0.157533331459215,-1.,1.99169810931893));
#38244=CARTESIAN_POINT('Ctrl Pts',(-0.159106226437289,-1.,1.98584238283279));
#38245=CARTESIAN_POINT('Ctrl Pts',(-0.16062206078461,-1.,1.97996195437557));
#38246=CARTESIAN_POINT('Ctrl Pts',(-0.162079693556302,-1.,1.97406280235204));
#38247=CARTESIAN_POINT('Ctrl Pts',(-0.16347818545776,-1.,1.96816512678));
#38248=CARTESIAN_POINT('Ctrl Pts',(-0.1648165689203,-1.,1.96229379940174));
#38249=CARTESIAN_POINT('Ctrl Pts',(-0.166093592002833,-1.,1.95646759718755));
#38250=CARTESIAN_POINT('Ctrl Pts',(-0.167307501784469,-1.,1.95069027794286));
#38251=CARTESIAN_POINT('Ctrl Pts',(-0.168455741607516,-1.,1.94493757756879));
#38252=CARTESIAN_POINT('Ctrl Pts',(-0.169534904817425,-1.,1.93915639211497));
#38253=CARTESIAN_POINT('Ctrl Pts',(-0.170541253116136,-1.,1.93329183155455));
#38254=CARTESIAN_POINT('Ctrl Pts',(-0.17147119153296,-1.,1.92731093582));
#38255=CARTESIAN_POINT('Ctrl Pts',(-0.172321621259557,-1.,1.92122334398034));
#38256=CARTESIAN_POINT('Ctrl Pts',(-0.173090695383619,-1.,1.91511429159681));
#38257=CARTESIAN_POINT('Ctrl Pts',(-0.173776635257984,-1.,1.90911693975475));
#38258=CARTESIAN_POINT('Ctrl Pts',(-0.174375518661222,-1.,1.90335253863003));
#38259=CARTESIAN_POINT('Ctrl Pts',(-0.174879405091277,-1.,1.89788101117148));
#38260=CARTESIAN_POINT('Ctrl Pts',(-0.175274276190664,-1.,1.89264630198279));
#38261=CARTESIAN_POINT('Ctrl Pts',(-0.175538155840286,-1.,1.88742606272818));
#38262=CARTESIAN_POINT('Ctrl Pts',(-0.175644148889271,-1.,1.88188663144846));
#38263=CARTESIAN_POINT('Ctrl Pts',(-0.175563480746206,-1.,1.87563767773249));
#38264=CARTESIAN_POINT('Ctrl Pts',(-0.175268337590901,-1.,1.86828349694972));
#38265=CARTESIAN_POINT('Ctrl Pts',(-0.174735259276856,-1.,1.85948367089838));
#38266=CARTESIAN_POINT('Ctrl Pts',(-0.173946627589401,-1.,1.84898113200543));
#38267=CARTESIAN_POINT('Ctrl Pts',(-0.17288944289442,-1.,1.83658380530747));
#38268=CARTESIAN_POINT('Ctrl Pts',(-0.171554770207306,-1.,1.82215766815414));
#38269=CARTESIAN_POINT('Ctrl Pts',(-0.169936923908078,-1.,1.80561530633924));
#38270=CARTESIAN_POINT('Ctrl Pts',(-0.16803277280837,-1.,1.78690649988931));
#38271=CARTESIAN_POINT('Ctrl Pts',(-0.166279355148738,-1.,1.77018771687692));
#38272=CARTESIAN_POINT('Ctrl Pts',(-0.164834765708484,-1.,1.75666056640041));
#38273=CARTESIAN_POINT('Ctrl Pts',(-0.163814161002474,-1.,1.74720349503904));
#38274=CARTESIAN_POINT('Ctrl Pts',(-0.163289472382896,-1.,1.74236521665491));
#38275=CARTESIAN_POINT('',(-0.383122945602004,-1.,1.7075470150345));
#38276=CARTESIAN_POINT('Origin',(0.,-1.,0.));
#38277=CARTESIAN_POINT('',(-0.61342227326009,-1.,2.11275013067528));
#38278=CARTESIAN_POINT('Ctrl Pts',(-0.383122945602004,-1.,1.7075470150345));
#38279=CARTESIAN_POINT('Ctrl Pts',(-0.384119047314215,-1.,1.71231062891398));
#38280=CARTESIAN_POINT('Ctrl Pts',(-0.386070790323281,-1.,1.72162022244582));
#38281=CARTESIAN_POINT('Ctrl Pts',(-0.388877023502615,-1.,1.73493170972829));
#38282=CARTESIAN_POINT('Ctrl Pts',(-0.392375812285395,-1.,1.75137405310193));
#38283=CARTESIAN_POINT('Ctrl Pts',(-0.396346196110688,-1.,1.76975560043442));
#38284=CARTESIAN_POINT('Ctrl Pts',(-0.399919403774155,-1.,1.78598826343754));
#38285=CARTESIAN_POINT('Ctrl Pts',(-0.403107976163396,-1.,1.80012077173238));
#38286=CARTESIAN_POINT('Ctrl Pts',(-0.405933518407175,-1.,1.81223801812013));
#38287=CARTESIAN_POINT('Ctrl Pts',(-0.408428948106227,-1.,1.82247022677562));
#38288=CARTESIAN_POINT('Ctrl Pts',(-0.410641256301276,-1.,1.83100408895047));
#38289=CARTESIAN_POINT('Ctrl Pts',(-0.412633125322945,-1.,1.8380895347617));
#38290=CARTESIAN_POINT('Ctrl Pts',(-0.414487438255542,-1.,1.84405757074218));
#38291=CARTESIAN_POINT('Ctrl Pts',(-0.416300022039885,-1.,1.84929312930314));
#38292=CARTESIAN_POINT('Ctrl Pts',(-0.418164129144045,-1.,1.8541763285645));
#38293=CARTESIAN_POINT('Ctrl Pts',(-0.420157287975583,-1.,1.8590328109667));
#38294=CARTESIAN_POINT('Ctrl Pts',(-0.422327307417885,-1.,1.86408083333863));
#38295=CARTESIAN_POINT('Ctrl Pts',(-0.424678177290876,-1.,1.8693780394412));
#38296=CARTESIAN_POINT('Ctrl Pts',(-0.427183828518743,-1.,1.87486989291333));
#38297=CARTESIAN_POINT('Ctrl Pts',(-0.429803062482217,-1.,1.88044229001778));
#38298=CARTESIAN_POINT('Ctrl Pts',(-0.432493038548833,-1.,1.88596913666828));
#38299=CARTESIAN_POINT('Ctrl Pts',(-0.43522566096358,-1.,1.89136993975585));
#38300=CARTESIAN_POINT('Ctrl Pts',(-0.437995003948443,-1.,1.89663648956549));
#38301=CARTESIAN_POINT('Ctrl Pts',(-0.440807833704161,-1.,1.90180124389137));
#38302=CARTESIAN_POINT('Ctrl Pts',(-0.44367755684917,-1.,1.90691756144906));
#38303=CARTESIAN_POINT('Ctrl Pts',(-0.446617343485651,-1.,1.91203699981095));
#38304=CARTESIAN_POINT('Ctrl Pts',(-0.449632260106572,-1.,1.91718342555717));
#38305=CARTESIAN_POINT('Ctrl Pts',(-0.452719478359356,-1.,1.9223538064847));
#38306=CARTESIAN_POINT('Ctrl Pts',(-0.455872005174335,-1.,1.92753067150461));
#38307=CARTESIAN_POINT('Ctrl Pts',(-0.459081234547931,-1.,1.93269066517936));
#38308=CARTESIAN_POINT('Ctrl Pts',(-0.462340031009087,-1.,1.93781486640834));
#38309=CARTESIAN_POINT('Ctrl Pts',(-0.465645462026065,-1.,1.94289794196205));
#38310=CARTESIAN_POINT('Ctrl Pts',(-0.468997482913158,-1.,1.94794381136524));
#38311=CARTESIAN_POINT('Ctrl Pts',(-0.47239767226408,-1.,1.95296148278136));
#38312=CARTESIAN_POINT('Ctrl Pts',(-0.475848034683172,-1.,1.95796111148175));
#38313=CARTESIAN_POINT('Ctrl Pts',(-0.479349583074846,-1.,1.96294933055938));
#38314=CARTESIAN_POINT('Ctrl Pts',(-0.482901662120687,-1.,1.96792703422358));
#38315=CARTESIAN_POINT('Ctrl Pts',(-0.486502692907661,-1.,1.97289186263272));
#38316=CARTESIAN_POINT('Ctrl Pts',(-0.490150627860955,-1.,1.97783973019229));
#38317=CARTESIAN_POINT('Ctrl Pts',(-0.493843476541492,-1.,1.9827665876182));
#38318=CARTESIAN_POINT('Ctrl Pts',(-0.497579909545564,-1.,1.98767044752929));
#38319=CARTESIAN_POINT('Ctrl Pts',(-0.501359287727129,-1.,1.9925514912615));
#38320=CARTESIAN_POINT('Ctrl Pts',(-0.505181361323011,-1.,1.99741107463567));
#38321=CARTESIAN_POINT('Ctrl Pts',(-0.509046069886152,-1.,2.00225107134733));
#38322=CARTESIAN_POINT('Ctrl Pts',(-0.512953306961814,-1.,2.00707309946955));
#38323=CARTESIAN_POINT('Ctrl Pts',(-0.516902681728733,-1.,2.01187773939257));
#38324=CARTESIAN_POINT('Ctrl Pts',(-0.520893590399428,-1.,2.01666477917305));
#38325=CARTESIAN_POINT('Ctrl Pts',(-0.524925318333518,-1.,2.02143356304712));
#38326=CARTESIAN_POINT('Ctrl Pts',(-0.528997127241911,-1.,2.02618329083289));
#38327=CARTESIAN_POINT('Ctrl Pts',(-0.533108355132905,-1.,2.03091336214401));
#38328=CARTESIAN_POINT('Ctrl Pts',(-0.537258489833134,-1.,2.03562362953993));
#38329=CARTESIAN_POINT('Ctrl Pts',(-0.54144712061552,-1.,2.0403142269048));
#38330=CARTESIAN_POINT('Ctrl Pts',(-0.545673903817348,-1.,2.0449854471456));
#38331=CARTESIAN_POINT('Ctrl Pts',(-0.549938525150342,-1.,2.04963761077974));
#38332=CARTESIAN_POINT('Ctrl Pts',(-0.55424065746411,-1.,2.05427091604482));
#38333=CARTESIAN_POINT('Ctrl Pts',(-0.558579940185467,-1.,2.05888537756571));
#38334=CARTESIAN_POINT('Ctrl Pts',(-0.562955993082574,-1.,2.06348090160697));
#38335=CARTESIAN_POINT('Ctrl Pts',(-0.567368421181229,-1.,2.06805732997383));
#38336=CARTESIAN_POINT('Ctrl Pts',(-0.571816823242411,-1.,2.07261449292757));
#38337=CARTESIAN_POINT('Ctrl Pts',(-0.576300797416275,-1.,2.07715226767361));
#38338=CARTESIAN_POINT('Ctrl Pts',(-0.580819952107257,-1.,2.08167059018138));
#38339=CARTESIAN_POINT('Ctrl Pts',(-0.585373918990895,-1.,2.086169437277));
#38340=CARTESIAN_POINT('Ctrl Pts',(-0.589962365403189,-1.,2.09064881812053));
#38341=CARTESIAN_POINT('Ctrl Pts',(-0.594585006052824,-1.,2.09510876220501));
#38342=CARTESIAN_POINT('Ctrl Pts',(-0.599241616422144,-1.,2.09954930865331));
#38343=CARTESIAN_POINT('Ctrl Pts',(-0.603932030738212,-1.,2.10397049887709));
#38344=CARTESIAN_POINT('Ctrl Pts',(-0.607711315456826,-1.,2.10749199615859));
#38345=CARTESIAN_POINT('Ctrl Pts',(-0.610560911691113,-1.,2.11012443807661));
#38346=CARTESIAN_POINT('Ctrl Pts',(-0.61246736556225,-1.,2.11187554260142));
#38347=CARTESIAN_POINT('Ctrl Pts',(-0.61342227326009,-1.,2.11275013067528));
#38348=CARTESIAN_POINT('',(-0.745574324794401,-1.,2.0698113262342));
#38349=CARTESIAN_POINT('',(-0.61342227326009,-1.,2.11275013067528));
#38350=CARTESIAN_POINT('',(-0.693717979106306,-1.,1.60662857109684));
#38351=CARTESIAN_POINT('Ctrl Pts',(-0.745574324794401,-1.,2.0698113262342));
#38352=CARTESIAN_POINT('Ctrl Pts',(-0.74583279137781,-1.,2.06854248895575));
#38353=CARTESIAN_POINT('Ctrl Pts',(-0.746345871542696,-1.,2.06600523016401));
#38354=CARTESIAN_POINT('Ctrl Pts',(-0.747103932785504,-1.,2.06220058927162));
#38355=CARTESIAN_POINT('Ctrl Pts',(-0.748091554181101,-1.,2.05713023030263));
#38356=CARTESIAN_POINT('Ctrl Pts',(-0.749287468663053,-1.,2.05079645591606));
#38357=CARTESIAN_POINT('Ctrl Pts',(-0.750444657874758,-1.,2.04446689147754));
#38358=CARTESIAN_POINT('Ctrl Pts',(-0.751562963361384,-1.,2.03814160092173));
#38359=CARTESIAN_POINT('Ctrl Pts',(-0.752642180488104,-1.,2.03182068456467));
#38360=CARTESIAN_POINT('Ctrl Pts',(-0.753682061113766,-1.,2.02550428623587));
#38361=CARTESIAN_POINT('Ctrl Pts',(-0.75468233072352,-1.,2.01919259406003));
#38362=CARTESIAN_POINT('Ctrl Pts',(-0.7556427049581,-1.,2.01288584328149));
#38363=CARTESIAN_POINT('Ctrl Pts',(-0.756562904646496,-1.,2.00658431587682));
#38364=CARTESIAN_POINT('Ctrl Pts',(-0.757442676862341,-1.,2.00028834739072));
#38365=CARTESIAN_POINT('Ctrl Pts',(-0.758281796766377,-1.,1.9939983109871));
#38366=CARTESIAN_POINT('Ctrl Pts',(-0.759080037802243,-1.,1.98771456680806));
#38367=CARTESIAN_POINT('Ctrl Pts',(-0.759837147452135,-1.,1.98143741418156));
#38368=CARTESIAN_POINT('Ctrl Pts',(-0.760552825409855,-1.,1.97516705321521));
#38369=CARTESIAN_POINT('Ctrl Pts',(-0.761226690483986,-1.,1.96890351582545));
#38370=CARTESIAN_POINT('Ctrl Pts',(-0.761858300014575,-1.,1.96264672744229));
#38371=CARTESIAN_POINT('Ctrl Pts',(-0.762447203806263,-1.,1.95639665309893));
#38372=CARTESIAN_POINT('Ctrl Pts',(-0.762992990878774,-1.,1.95015342590025));
#38373=CARTESIAN_POINT('Ctrl Pts',(-0.76349533353858,-1.,1.94391746617626));
#38374=CARTESIAN_POINT('Ctrl Pts',(-0.763954049121393,-1.,1.93768964875867));
#38375=CARTESIAN_POINT('Ctrl Pts',(-0.764369010673889,-1.,1.93147105496367));
#38376=CARTESIAN_POINT('Ctrl Pts',(-0.764740025488189,-1.,1.92526263537041));
#38377=CARTESIAN_POINT('Ctrl Pts',(-0.765066729667095,-1.,1.91906491634197));
#38378=CARTESIAN_POINT('Ctrl Pts',(-0.765348465884739,-1.,1.91287765805174));
#38379=CARTESIAN_POINT('Ctrl Pts',(-0.765584196937936,-1.,1.90669961402362));
#38380=CARTESIAN_POINT('Ctrl Pts',(-0.765772772593395,-1.,1.90052930393599));
#38381=CARTESIAN_POINT('Ctrl Pts',(-0.765913193856979,-1.,1.89436577771389));
#38382=CARTESIAN_POINT('Ctrl Pts',(-0.76600483706209,-1.,1.88820926433409));
#38383=CARTESIAN_POINT('Ctrl Pts',(-0.766047794851869,-1.,1.88206215302561));
#38384=CARTESIAN_POINT('Ctrl Pts',(-0.766042837036759,-1.,1.87592888967886));
#38385=CARTESIAN_POINT('Ctrl Pts',(-0.765990708546111,-1.,1.86981398314345));
#38386=CARTESIAN_POINT('Ctrl Pts',(-0.765891519092557,-1.,1.86372027063314));
#38387=CARTESIAN_POINT('Ctrl Pts',(-0.765744212909305,-1.,1.85764741390391));
#38388=CARTESIAN_POINT('Ctrl Pts',(-0.765545710619023,-1.,1.85158945130054));
#38389=CARTESIAN_POINT('Ctrl Pts',(-0.765291664861971,-1.,1.8455369887591));
#38390=CARTESIAN_POINT('Ctrl Pts',(-0.764978057881687,-1.,1.83948181064823));
#38391=CARTESIAN_POINT('Ctrl Pts',(-0.764602549687845,-1.,1.8334207722714));
#38392=CARTESIAN_POINT('Ctrl Pts',(-0.764165902606055,-1.,1.8273599120008));
#38393=CARTESIAN_POINT('Ctrl Pts',(-0.763673465462854,-1.,1.82131873145297));
#38394=CARTESIAN_POINT('Ctrl Pts',(-0.763132003836783,-1.,1.81532118405566));
#38395=CARTESIAN_POINT('Ctrl Pts',(-0.762546129464036,-1.,1.80938551463989));
#38396=CARTESIAN_POINT('Ctrl Pts',(-0.761915336443516,-1.,1.80351583877334));
#38397=CARTESIAN_POINT('Ctrl Pts',(-0.761229695230359,-1.,1.79768986997735));
#38398=CARTESIAN_POINT('Ctrl Pts',(-0.760469555880425,-1.,1.79185815610802));
#38399=CARTESIAN_POINT('Ctrl Pts',(-0.759614401109868,-1.,1.78596964884526));
#38400=CARTESIAN_POINT('Ctrl Pts',(-0.75865062667738,-1.,1.77999411220912));
#38401=CARTESIAN_POINT('Ctrl Pts',(-0.757578264077238,-1.,1.77394167108342));
#38402=CARTESIAN_POINT('Ctrl Pts',(-0.756421896028403,-1.,1.76789396003141));
#38403=CARTESIAN_POINT('Ctrl Pts',(-0.755220979975262,-1.,1.7619781724032));
#38404=CARTESIAN_POINT('Ctrl Pts',(-0.75400925402848,-1.,1.75631083600175));
#38405=CARTESIAN_POINT('Ctrl Pts',(-0.752797683531377,-1.,1.75095139468809));
#38406=CARTESIAN_POINT('Ctrl Pts',(-0.751555614163629,-1.,1.74585086852298));
#38407=CARTESIAN_POINT('Ctrl Pts',(-0.75019343597954,-1.,1.74080458266705));
#38408=CARTESIAN_POINT('Ctrl Pts',(-0.748582462954855,-1.,1.73550351679848));
#38409=CARTESIAN_POINT('Ctrl Pts',(-0.746574710096436,-1.,1.72958533647399));
#38410=CARTESIAN_POINT('Ctrl Pts',(-0.744021445433764,-1.,1.7226822991693));
#38411=CARTESIAN_POINT('Ctrl Pts',(-0.740795162032088,-1.,1.71447789751927));
#38412=CARTESIAN_POINT('Ctrl Pts',(-0.736799665724771,-1.,1.70473309006121));
#38413=CARTESIAN_POINT('Ctrl Pts',(-0.731963238697195,-1.,1.69326921975743));
#38414=CARTESIAN_POINT('Ctrl Pts',(-0.726235967997433,-1.,1.67996158455503));
#38415=CARTESIAN_POINT('Ctrl Pts',(-0.719585433804282,-1.,1.6647288055568));
#38416=CARTESIAN_POINT('Ctrl Pts',(-0.711993139355394,-1.,1.64752408832016));
#38417=CARTESIAN_POINT('Ctrl Pts',(-0.705159151988319,-1.,1.63216541664676));
#38418=CARTESIAN_POINT('Ctrl Pts',(-0.699605146405088,-1.,1.61974673472612));
#38419=CARTESIAN_POINT('Ctrl Pts',(-0.695712097881194,-1.,1.61106790958151));
#38420=CARTESIAN_POINT('Ctrl Pts',(-0.693717979106306,-1.,1.60662857109684));
#38421=CARTESIAN_POINT('',(-0.892032620296855,-1.,1.5055822144029));
#38422=CARTESIAN_POINT('Origin',(0.,-1.,0.));
#38423=CARTESIAN_POINT('',(-1.23627494547115,-1.,1.81978687191668));
#38424=CARTESIAN_POINT('Ctrl Pts',(-0.892032620296855,-1.,1.5055822144029));
#38425=CARTESIAN_POINT('Ctrl Pts',(-0.894452006964543,-1.,1.50980486806688));
#38426=CARTESIAN_POINT('Ctrl Pts',(-0.899185047483511,-1.,1.51805569590094));
#38427=CARTESIAN_POINT('Ctrl Pts',(-0.905967409625651,-1.,1.52984849887993));
#38428=CARTESIAN_POINT('Ctrl Pts',(-0.914375919026456,-1.,1.54440491149498));
#38429=CARTESIAN_POINT('Ctrl Pts',(-0.923832188944341,-1.,1.56065988578893));
#38430=CARTESIAN_POINT('Ctrl Pts',(-0.932246680108685,-1.,1.57499388382243));
#38431=CARTESIAN_POINT('Ctrl Pts',(-0.939646377893399,-1.,1.58744937487176));
#38432=CARTESIAN_POINT('Ctrl Pts',(-0.946078063315257,-1.,1.59810042043673));
#38433=CARTESIAN_POINT('Ctrl Pts',(-0.951613284356035,-1.,1.60706069896936));
#38434=CARTESIAN_POINT('Ctrl Pts',(-0.956354422920671,-1.,1.61449324337085));
#38435=CARTESIAN_POINT('Ctrl Pts',(-0.960438326101729,-1.,1.62061638140221));
#38436=CARTESIAN_POINT('Ctrl Pts',(-0.964046107040536,-1.,1.62571930670187));
#38437=CARTESIAN_POINT('Ctrl Pts',(-0.967387853230345,-1.,1.63013849959461));
#38438=CARTESIAN_POINT('Ctrl Pts',(-0.970669715997509,-1.,1.63420665729798));
#38439=CARTESIAN_POINT('Ctrl Pts',(-0.974066058287418,-1.,1.63820952658144));
#38440=CARTESIAN_POINT('Ctrl Pts',(-0.977689794119416,-1.,1.64233990826687));
#38441=CARTESIAN_POINT('Ctrl Pts',(-0.981562530939489,-1.,1.64665139190656));
#38442=CARTESIAN_POINT('Ctrl Pts',(-0.985642622920821,-1.,1.65110016612638));
#38443=CARTESIAN_POINT('Ctrl Pts',(-0.989855627854165,-1.,1.65559044289699));
#38444=CARTESIAN_POINT('Ctrl Pts',(-0.994121836661306,-1.,1.66001553809947));
#38445=CARTESIAN_POINT('Ctrl Pts',(-0.998389654952758,-1.,1.66430758030376));
#38446=CARTESIAN_POINT('Ctrl Pts',(-1.00265091003727,-1.,1.66846059277303));
#38447=CARTESIAN_POINT('Ctrl Pts',(-1.00692206696414,-1.,1.67250335383293));
#38448=CARTESIAN_POINT('Ctrl Pts',(-1.01123236493511,-1.,1.67648246776464));
#38449=CARTESIAN_POINT('Ctrl Pts',(-1.01561026162773,-1.,1.68044289894798));
#38450=CARTESIAN_POINT('Ctrl Pts',(-1.02006795074201,-1.,1.68440578021706));
#38451=CARTESIAN_POINT('Ctrl Pts',(-1.02460180535255,-1.,1.68836910178447));
#38452=CARTESIAN_POINT('Ctrl Pts',(-1.02919977579147,-1.,1.69231840863458));
#38453=CARTESIAN_POINT('Ctrl Pts',(-1.03384646003588,-1.,1.69623414782771));
#38454=CARTESIAN_POINT('Ctrl Pts',(-1.03852922490789,-1.,1.70010052930962));
#38455=CARTESIAN_POINT('Ctrl Pts',(-1.04324363334554,-1.,1.70391338707982));
#38456=CARTESIAN_POINT('Ctrl Pts',(-1.04799085404995,-1.,1.70767646263649));
#38457=CARTESIAN_POINT('Ctrl Pts',(-1.05277517202855,-1.,1.71139783543989));
#38458=CARTESIAN_POINT('Ctrl Pts',(-1.05760163192479,-1.,1.7150865442702));
#38459=CARTESIAN_POINT('Ctrl Pts',(-1.06247324680647,-1.,1.71874858456904));
#38460=CARTESIAN_POINT('Ctrl Pts',(-1.06738966975462,-1.,1.72238500928453));
#38461=CARTESIAN_POINT('Ctrl Pts',(-1.07234866990252,-1.,1.72599406198488));
#38462=CARTESIAN_POINT('Ctrl Pts',(-1.0773470373727,-1.,1.72957248977424));
#38463=CARTESIAN_POINT('Ctrl Pts',(-1.08238162784749,-1.,1.73311705663407));
#38464=CARTESIAN_POINT('Ctrl Pts',(-1.08745056285427,-1.,1.73662628326091));
#38465=CARTESIAN_POINT('Ctrl Pts',(-1.09255329056493,-1.,1.74010053962247));
#38466=CARTESIAN_POINT('Ctrl Pts',(-1.09768999241225,-1.,1.74354119236208));
#38467=CARTESIAN_POINT('Ctrl Pts',(-1.10286118991143,-1.,1.74695004214923));
#38468=CARTESIAN_POINT('Ctrl Pts',(-1.10806728183007,-1.,1.7503286607592));
#38469=CARTESIAN_POINT('Ctrl Pts',(-1.11330807582551,-1.,1.7536777209463));
#38470=CARTESIAN_POINT('Ctrl Pts',(-1.11858293216763,-1.,1.75699720772105));
#38471=CARTESIAN_POINT('Ctrl Pts',(-1.12389096855086,-1.,1.76028671825096));
#38472=CARTESIAN_POINT('Ctrl Pts',(-1.12923123555075,-1.,1.7635457196617));
#38473=CARTESIAN_POINT('Ctrl Pts',(-1.1346029180462,-1.,1.76677384551862));
#38474=CARTESIAN_POINT('Ctrl Pts',(-1.14000548336975,-1.,1.76997111386769));
#38475=CARTESIAN_POINT('Ctrl Pts',(-1.1454385822692,-1.,1.77313777896194));
#38476=CARTESIAN_POINT('Ctrl Pts',(-1.15090197841515,-1.,1.7762742255701));
#38477=CARTESIAN_POINT('Ctrl Pts',(-1.15639547194698,-1.,1.77938085564275));
#38478=CARTESIAN_POINT('Ctrl Pts',(-1.16191881298499,-1.,1.78245795881009));
#38479=CARTESIAN_POINT('Ctrl Pts',(-1.16747166312303,-1.,1.78550566040443));
#38480=CARTESIAN_POINT('Ctrl Pts',(-1.17305363177328,-1.,1.78852398877616));
#38481=CARTESIAN_POINT('Ctrl Pts',(-1.17866429440809,-1.,1.79151291552689));
#38482=CARTESIAN_POINT('Ctrl Pts',(-1.18430321697432,-1.,1.79447240321515));
#38483=CARTESIAN_POINT('Ctrl Pts',(-1.18996997934445,-1.,1.79740245923478));
#38484=CARTESIAN_POINT('Ctrl Pts',(-1.19566418930242,-1.,1.80030314369879));
#38485=CARTESIAN_POINT('Ctrl Pts',(-1.20138548938974,-1.,1.80317454838603));
#38486=CARTESIAN_POINT('Ctrl Pts',(-1.20713356605475,-1.,1.80601678480707));
#38487=CARTESIAN_POINT('Ctrl Pts',(-1.21290815708314,-1.,1.80882996917129));
#38488=CARTESIAN_POINT('Ctrl Pts',(-1.21870906103557,-1.,1.81161420806656));
#38489=CARTESIAN_POINT('Ctrl Pts',(-1.2245361330495,-1.,1.81436959210434));
#38490=CARTESIAN_POINT('Ctrl Pts',(-1.2292186489137,-1.,1.8165508718364));
#38491=CARTESIAN_POINT('Ctrl Pts',(-1.2327422452705,-1.,1.81817389921279));
#38492=CARTESIAN_POINT('Ctrl Pts',(-1.23509651170476,-1.,1.81925017193666));
#38493=CARTESIAN_POINT('Ctrl Pts',(-1.23627494547115,-1.,1.81978687191668));
#38494=CARTESIAN_POINT('',(-1.34869019493419,-1.,1.73811241238545));
#38495=CARTESIAN_POINT('',(-1.23627494547115,-1.,1.81978687191668));
#38496=CARTESIAN_POINT('',(-1.15624053661742,-1.,1.31362392696032));
#38497=CARTESIAN_POINT('Ctrl Pts',(-1.34869019493419,-1.,1.73811241238545));
#38498=CARTESIAN_POINT('Ctrl Pts',(-1.34854391898045,-1.,1.73682580585691));
#38499=CARTESIAN_POINT('Ctrl Pts',(-1.34824783112887,-1.,1.73425417885907));
#38500=CARTESIAN_POINT('Ctrl Pts',(-1.34779309152035,-1.,1.7304014965394));
#38501=CARTESIAN_POINT('Ctrl Pts',(-1.34716554819527,-1.,1.72527410680674));
#38502=CARTESIAN_POINT('Ctrl Pts',(-1.34634568653227,-1.,1.7188807715049));
#38503=CARTESIAN_POINT('Ctrl Pts',(-1.34549029589416,-1.,1.71250340686822));
#38504=CARTESIAN_POINT('Ctrl Pts',(-1.34459924533831,-1.,1.70614212266738));
#38505=CARTESIAN_POINT('Ctrl Pts',(-1.34367237124483,-1.,1.69979707754427));
#38506=CARTESIAN_POINT('Ctrl Pts',(-1.34270948206319,-1.,1.6934684849687));
#38507=CARTESIAN_POINT('Ctrl Pts',(-1.341710374848,-1.,1.68715660868764));
#38508=CARTESIAN_POINT('Ctrl Pts',(-1.34067485185203,-1.,1.68086176030362));
#38509=CARTESIAN_POINT('Ctrl Pts',(-1.3396027347034,-1.,1.67458429426086));
#38510=CARTESIAN_POINT('Ctrl Pts',(-1.33849388654388,-1.,1.66832460783989));
#38511=CARTESIAN_POINT('Ctrl Pts',(-1.33734820885262,-1.,1.66208312541983));
#38512=CARTESIAN_POINT('Ctrl Pts',(-1.33616559745172,-1.,1.65586025952593));
#38513=CARTESIAN_POINT('Ctrl Pts',(-1.33494590467993,-1.,1.6496563728683));
#38514=CARTESIAN_POINT('Ctrl Pts',(-1.33368890676572,-1.,1.6434717485603));
#38515=CARTESIAN_POINT('Ctrl Pts',(-1.33239425103724,-1.,1.63730653475089));
#38516=CARTESIAN_POINT('Ctrl Pts',(-1.33106149345645,-1.,1.63116079730923));
#38517=CARTESIAN_POINT('Ctrl Pts',(-1.3296901950568,-1.,1.62503464209797));
#38518=CARTESIAN_POINT('Ctrl Pts',(-1.32828000610449,-1.,1.61892832270724));
#38519=CARTESIAN_POINT('Ctrl Pts',(-1.32683074483356,-1.,1.6128423401575));
#38520=CARTESIAN_POINT('Ctrl Pts',(-1.32534250785782,-1.,1.60677758290954));
#38521=CARTESIAN_POINT('Ctrl Pts',(-1.32381550858256,-1.,1.60073511858687));
#38522=CARTESIAN_POINT('Ctrl Pts',(-1.32224985747682,-1.,1.59471591079403));
#38523=CARTESIAN_POINT('Ctrl Pts',(-1.32064537110892,-1.,1.58872057258245));
#38524=CARTESIAN_POINT('Ctrl Pts',(-1.31900135021432,-1.,1.58274907898834));
#38525=CARTESIAN_POINT('Ctrl Pts',(-1.31731642317187,-1.,1.5768005650559));
#38526=CARTESIAN_POINT('Ctrl Pts',(-1.31558903860016,-1.,1.57087397835723));
#38527=CARTESIAN_POINT('Ctrl Pts',(-1.31381795281002,-1.,1.56496872402353));
#38528=CARTESIAN_POINT('Ctrl Pts',(-1.31200264341696,-1.,1.55908521254821));
#38529=CARTESIAN_POINT('Ctrl Pts',(-1.31014393684222,-1.,1.55322568759481));
#38530=CARTESIAN_POINT('Ctrl Pts',(-1.30824393907473,-1.,1.54739413957185));
#38531=CARTESIAN_POINT('Ctrl Pts',(-1.30630475189556,-1.,1.54159462645432));
#38532=CARTESIAN_POINT('Ctrl Pts',(-1.30432735639489,-1.,1.53582981268977));
#38533=CARTESIAN_POINT('Ctrl Pts',(-1.30231064395568,-1.,1.53009970283891));
#38534=CARTESIAN_POINT('Ctrl Pts',(-1.30024984366328,-1.,1.52439957861062));
#38535=CARTESIAN_POINT('Ctrl Pts',(-1.29813791800747,-1.,1.51872184912724));
#38536=CARTESIAN_POINT('Ctrl Pts',(-1.29596850710509,-1.,1.51305994241402));
#38537=CARTESIAN_POINT('Ctrl Pts',(-1.29373841372842,-1.,1.50741159078365));
#38538=CARTESIAN_POINT('Ctrl Pts',(-1.29145022885181,-1.,1.50178230149776));
#38539=CARTESIAN_POINT('Ctrl Pts',(-1.28911506584254,-1.,1.49618896881754));
#38540=CARTESIAN_POINT('Ctrl Pts',(-1.2867467611644,-1.,1.4906522831278));
#38541=CARTESIAN_POINT('Ctrl Pts',(-1.28435533880201,-1.,1.4851881711891));
#38542=CARTESIAN_POINT('Ctrl Pts',(-1.28194158939517,-1.,1.47980070347095));
#38543=CARTESIAN_POINT('Ctrl Pts',(-1.2794891824849,-1.,1.4744717526707));
#38544=CARTESIAN_POINT('Ctrl Pts',(-1.27696414831089,-1.,1.46916035917133));
#38545=CARTESIAN_POINT('Ctrl Pts',(-1.27433119897822,-1.,1.46382431332476));
#38546=CARTESIAN_POINT('Ctrl Pts',(-1.27156805265289,-1.,1.45843906294697));
#38547=CARTESIAN_POINT('Ctrl Pts',(-1.2686778680489,-1.,1.45301422764247));
#38548=CARTESIAN_POINT('Ctrl Pts',(-1.26570925118868,-1.,1.44761985001662));
#38549=CARTESIAN_POINT('Ctrl Pts',(-1.26273903323859,-1.,1.44236470511303));
#38550=CARTESIAN_POINT('Ctrl Pts',(-1.25983531012005,-1.,1.43734919180848));
#38551=CARTESIAN_POINT('Ctrl Pts',(-1.25702687965755,-1.,1.43262645609691));
#38552=CARTESIAN_POINT('Ctrl Pts',(-1.25426945222639,-1.,1.42815938799387));
#38553=CARTESIAN_POINT('Ctrl Pts',(-1.2514145557001,-1.,1.42378102115575));
#38554=CARTESIAN_POINT('Ctrl Pts',(-1.24824430986571,-1.,1.41923722596025));
#38555=CARTESIAN_POINT('Ctrl Pts',(-1.24450600513056,-1.,1.41422913175179));
#38556=CARTESIAN_POINT('Ctrl Pts',(-1.23994455029534,-1.,1.40845295531283));
#38557=CARTESIAN_POINT('Ctrl Pts',(-1.23434087290423,-1.,1.40164708206106));
#38558=CARTESIAN_POINT('Ctrl Pts',(-1.22752961899387,-1.,1.39361389568796));
#38559=CARTESIAN_POINT('Ctrl Pts',(-1.21938737280852,-1.,1.38420564527715));
#38560=CARTESIAN_POINT('Ctrl Pts',(-1.20982812925645,-1.,1.37331915607905));
#38561=CARTESIAN_POINT('Ctrl Pts',(-1.1987959077932,-1.,1.36088705043885));
#38562=CARTESIAN_POINT('Ctrl Pts',(-1.18625865667441,-1.,1.34687054001093));
#38563=CARTESIAN_POINT('Ctrl Pts',(-1.17501305789857,-1.,1.33437539347008));
#38564=CARTESIAN_POINT('Ctrl Pts',(-1.16589330093588,-1.,1.32428080721772));
#38565=CARTESIAN_POINT('Ctrl Pts',(-1.15950888730809,-1.,1.31722977216397));
#38566=CARTESIAN_POINT('Ctrl Pts',(-1.15624053661742,-1.,1.31362392696032));
#38567=CARTESIAN_POINT('',(-1.31362392696033,-1.,1.15624053661742));
#38568=CARTESIAN_POINT('Origin',(0.,-1.,0.));
#38569=CARTESIAN_POINT('',(-1.73811241238545,-1.,1.34869019493419));
#38570=CARTESIAN_POINT('Ctrl Pts',(-1.31362392696033,-1.,1.15624053661742));
#38571=CARTESIAN_POINT('Ctrl Pts',(-1.3172297721596,-1.,1.15950888730433));
#38572=CARTESIAN_POINT('Ctrl Pts',(-1.32428080720544,-1.,1.16589330092532));
#38573=CARTESIAN_POINT('Ctrl Pts',(-1.33437539344842,-1.,1.17501305787994));
#38574=CARTESIAN_POINT('Ctrl Pts',(-1.34687053998157,-1.,1.18625865664915));
#38575=CARTESIAN_POINT('Ctrl Pts',(-1.36088705040677,-1.,1.1987959077656));
#38576=CARTESIAN_POINT('Ctrl Pts',(-1.37331915604962,-1.,1.20982812923113));
#38577=CARTESIAN_POINT('Ctrl Pts',(-1.38420564525391,-1.,1.21938737278853));
#38578=CARTESIAN_POINT('Ctrl Pts',(-1.39361389567257,-1.,1.22752961898063));
#38579=CARTESIAN_POINT('Ctrl Pts',(-1.40164708205345,-1.,1.23434087289768));
#38580=CARTESIAN_POINT('Ctrl Pts',(-1.40845295531151,-1.,1.23994455029421));
#38581=CARTESIAN_POINT('Ctrl Pts',(-1.41422913175437,-1.,1.24450600513278));
#38582=CARTESIAN_POINT('Ctrl Pts',(-1.41923722596421,-1.,1.24824430986911));
#38583=CARTESIAN_POINT('Ctrl Pts',(-1.42378102115911,-1.,1.25141455570299));
#38584=CARTESIAN_POINT('Ctrl Pts',(-1.42815938799555,-1.,1.25426945222783));
#38585=CARTESIAN_POINT('Ctrl Pts',(-1.43262645609679,-1.,1.25702687965744));
#38586=CARTESIAN_POINT('Ctrl Pts',(-1.43734919180719,-1.,1.25983531011894));
#38587=CARTESIAN_POINT('Ctrl Pts',(-1.44236470511145,-1.,1.26273903323723));
#38588=CARTESIAN_POINT('Ctrl Pts',(-1.44761985001544,-1.,1.26570925118767));
#38589=CARTESIAN_POINT('Ctrl Pts',(-1.45301422764205,-1.,1.26867786804854));
#38590=CARTESIAN_POINT('Ctrl Pts',(-1.45843906294725,-1.,1.27156805265312));
#38591=CARTESIAN_POINT('Ctrl Pts',(-1.4638243133254,-1.,1.27433119897877));
#38592=CARTESIAN_POINT('Ctrl Pts',(-1.46916035917197,-1.,1.27696414831144));
#38593=CARTESIAN_POINT('Ctrl Pts',(-1.4744717526711,-1.,1.27948918248524));
#38594=CARTESIAN_POINT('Ctrl Pts',(-1.47980070347102,-1.,1.28194158939522));
#38595=CARTESIAN_POINT('Ctrl Pts',(-1.48518817118891,-1.,1.28435533880184));
#38596=CARTESIAN_POINT('Ctrl Pts',(-1.4906522831275,-1.,1.28674676116415));
#38597=CARTESIAN_POINT('Ctrl Pts',(-1.49618896881729,-1.,1.28911506584232));
#38598=CARTESIAN_POINT('Ctrl Pts',(-1.50178230149764,-1.,1.29145022885171));
#38599=CARTESIAN_POINT('Ctrl Pts',(-1.50741159078367,-1.,1.29373841372843));
#38600=CARTESIAN_POINT('Ctrl Pts',(-1.51305994241412,-1.,1.29596850710518));
#38601=CARTESIAN_POINT('Ctrl Pts',(-1.51872184912735,-1.,1.29813791800757));
#38602=CARTESIAN_POINT('Ctrl Pts',(-1.5243995786107,-1.,1.30024984366334));
#38603=CARTESIAN_POINT('Ctrl Pts',(-1.53009970283893,-1.,1.3023106439557));
#38604=CARTESIAN_POINT('Ctrl Pts',(-1.53582981268976,-1.,1.30432735639487));
#38605=CARTESIAN_POINT('Ctrl Pts',(-1.54159462645428,-1.,1.30630475189553));
#38606=CARTESIAN_POINT('Ctrl Pts',(-1.54739413957183,-1.,1.30824393907471));
#38607=CARTESIAN_POINT('Ctrl Pts',(-1.55322568759481,-1.,1.31014393684221));
#38608=CARTESIAN_POINT('Ctrl Pts',(-1.55908521254822,-1.,1.31200264341696));
#38609=CARTESIAN_POINT('Ctrl Pts',(-1.56496872402352,-1.,1.31381795281002));
#38610=CARTESIAN_POINT('Ctrl Pts',(-1.57087397835721,-1.,1.31558903860015));
#38611=CARTESIAN_POINT('Ctrl Pts',(-1.57680056505585,-1.,1.31731642317183));
#38612=CARTESIAN_POINT('Ctrl Pts',(-1.58274907898829,-1.,1.31900135021428));
#38613=CARTESIAN_POINT('Ctrl Pts',(-1.58872057258244,-1.,1.32064537110891));
#38614=CARTESIAN_POINT('Ctrl Pts',(-1.59471591079408,-1.,1.32224985747686));
#38615=CARTESIAN_POINT('Ctrl Pts',(-1.600735118587,-1.,1.32381550858266));
#38616=CARTESIAN_POINT('Ctrl Pts',(-1.6067775829097,-1.,1.32534250785794));
#38617=CARTESIAN_POINT('Ctrl Pts',(-1.61284234015762,-1.,1.32683074483365));
#38618=CARTESIAN_POINT('Ctrl Pts',(-1.61892832270723,-1.,1.32828000610448));
#38619=CARTESIAN_POINT('Ctrl Pts',(-1.62503464209777,-1.,1.32969019505665));
#38620=CARTESIAN_POINT('Ctrl Pts',(-1.63116079730887,-1.,1.33106149345618));
#38621=CARTESIAN_POINT('Ctrl Pts',(-1.6373065347505,-1.,1.33239425103694));
#38622=CARTESIAN_POINT('Ctrl Pts',(-1.64347174856007,-1.,1.33368890676554));
#38623=CARTESIAN_POINT('Ctrl Pts',(-1.64965637286843,-1.,1.33494590468003));
#38624=CARTESIAN_POINT('Ctrl Pts',(-1.65586025952651,-1.,1.33616559745217));
#38625=CARTESIAN_POINT('Ctrl Pts',(-1.66208312542073,-1.,1.33734820885331));
#38626=CARTESIAN_POINT('Ctrl Pts',(-1.66832460784078,-1.,1.33849388654458));
#38627=CARTESIAN_POINT('Ctrl Pts',(-1.67458429426126,-1.,1.33960273470372));
#38628=CARTESIAN_POINT('Ctrl Pts',(-1.68086176030308,-1.,1.3406748518516));
#38629=CARTESIAN_POINT('Ctrl Pts',(-1.68715660868602,-1.,1.34171037484673));
#38630=CARTESIAN_POINT('Ctrl Pts',(-1.6934684849664,-1.,1.34270948206139));
#38631=CARTESIAN_POINT('Ctrl Pts',(-1.69979707754221,-1.,1.34367237124322));
#38632=CARTESIAN_POINT('Ctrl Pts',(-1.70614212266676,-1.,1.34459924533783));
#38633=CARTESIAN_POINT('Ctrl Pts',(-1.71250340687011,-1.,1.34549029589563));
#38634=CARTESIAN_POINT('Ctrl Pts',(-1.7188807715095,-1.,1.34634568653586));
#38635=CARTESIAN_POINT('Ctrl Pts',(-1.72527410681298,-1.,1.34716554820013));
#38636=CARTESIAN_POINT('Ctrl Pts',(-1.73040149654497,-1.,1.3477930915247));
#38637=CARTESIAN_POINT('Ctrl Pts',(-1.73425417886255,-1.,1.34824783113158));
#38638=CARTESIAN_POINT('Ctrl Pts',(-1.73682580585819,-1.,1.34854391898145));
#38639=CARTESIAN_POINT('Ctrl Pts',(-1.73811241238545,-1.,1.34869019493419));
#38640=CARTESIAN_POINT('',(-1.81978687191668,-1.,1.23627494547115));
#38641=CARTESIAN_POINT('',(-1.73811241238545,-1.,1.34869019493419));
#38642=CARTESIAN_POINT('',(-1.5055822144029,-1.,0.892032620296855));
#38643=CARTESIAN_POINT('Ctrl Pts',(-1.81978687191668,-1.,1.23627494547115));
#38644=CARTESIAN_POINT('Ctrl Pts',(-1.81925017193531,-1.,1.23509651170384));
#38645=CARTESIAN_POINT('Ctrl Pts',(-1.81817389920914,-1.,1.23274224526804));
#38646=CARTESIAN_POINT('Ctrl Pts',(-1.81655087183054,-1.,1.22921864890975));
#38647=CARTESIAN_POINT('Ctrl Pts',(-1.81436959209778,-1.,1.22453613304507));
#38648=CARTESIAN_POINT('Ctrl Pts',(-1.81161420806172,-1.,1.2187090610323));
#38649=CARTESIAN_POINT('Ctrl Pts',(-1.80882996916931,-1.,1.2129081570818));
#38650=CARTESIAN_POINT('Ctrl Pts',(-1.80601678480772,-1.,1.20713356605519));
#38651=CARTESIAN_POINT('Ctrl Pts',(-1.8031745483882,-1.,1.2013854893912));
#38652=CARTESIAN_POINT('Ctrl Pts',(-1.80030314370121,-1.,1.19566418930405));
#38653=CARTESIAN_POINT('Ctrl Pts',(-1.79740245923649,-1.,1.1899699793456));
#38654=CARTESIAN_POINT('Ctrl Pts',(-1.79447240321572,-1.,1.18430321697471));
#38655=CARTESIAN_POINT('Ctrl Pts',(-1.79151291552646,-1.,1.17866429440781));
#38656=CARTESIAN_POINT('Ctrl Pts',(-1.78852398877523,-1.,1.17305363177265));
#38657=CARTESIAN_POINT('Ctrl Pts',(-1.78550566040349,-1.,1.16747166312239));
#38658=CARTESIAN_POINT('Ctrl Pts',(-1.78245795880949,-1.,1.16191881298458));
#38659=CARTESIAN_POINT('Ctrl Pts',(-1.77938085564261,-1.,1.15639547194689));
#38660=CARTESIAN_POINT('Ctrl Pts',(-1.77627422557034,-1.,1.15090197841531));
#38661=CARTESIAN_POINT('Ctrl Pts',(-1.77313777896234,-1.,1.14543858226948));
#38662=CARTESIAN_POINT('Ctrl Pts',(-1.76997111386806,-1.,1.14000548337));
#38663=CARTESIAN_POINT('Ctrl Pts',(-1.76677384551883,-1.,1.13460291804635));
#38664=CARTESIAN_POINT('Ctrl Pts',(-1.76354571966171,-1.,1.12923123555076));
#38665=CARTESIAN_POINT('Ctrl Pts',(-1.76028671825084,-1.,1.12389096855078));
#38666=CARTESIAN_POINT('Ctrl Pts',(-1.75699720772089,-1.,1.11858293216752));
#38667=CARTESIAN_POINT('Ctrl Pts',(-1.75367772094617,-1.,1.11330807582542));
#38668=CARTESIAN_POINT('Ctrl Pts',(-1.75032866075914,-1.,1.10806728183003));
#38669=CARTESIAN_POINT('Ctrl Pts',(-1.74695004214924,-1.,1.10286118991144));
#38670=CARTESIAN_POINT('Ctrl Pts',(-1.74354119236212,-1.,1.09768999241229));
#38671=CARTESIAN_POINT('Ctrl Pts',(-1.74010053962252,-1.,1.09255329056496));
#38672=CARTESIAN_POINT('Ctrl Pts',(-1.73662628326093,-1.,1.08745056285429));
#38673=CARTESIAN_POINT('Ctrl Pts',(-1.73311705663407,-1.,1.08238162784749));
#38674=CARTESIAN_POINT('Ctrl Pts',(-1.72957248977424,-1.,1.0773470373727));
#38675=CARTESIAN_POINT('Ctrl Pts',(-1.72599406198489,-1.,1.07234866990252));
#38676=CARTESIAN_POINT('Ctrl Pts',(-1.72238500928456,-1.,1.06738966975463));
#38677=CARTESIAN_POINT('Ctrl Pts',(-1.71874858456908,-1.,1.0624732468065));
#38678=CARTESIAN_POINT('Ctrl Pts',(-1.71508654427022,-1.,1.05760163192481));
#38679=CARTESIAN_POINT('Ctrl Pts',(-1.71139783543986,-1.,1.05277517202854));
#38680=CARTESIAN_POINT('Ctrl Pts',(-1.70767646263641,-1.,1.0479908540499));
#38681=CARTESIAN_POINT('Ctrl Pts',(-1.70391338707969,-1.,1.04324363334546));
#38682=CARTESIAN_POINT('Ctrl Pts',(-1.70010052930951,-1.,1.03852922490782));
#38683=CARTESIAN_POINT('Ctrl Pts',(-1.69623414782769,-1.,1.03384646003587));
#38684=CARTESIAN_POINT('Ctrl Pts',(-1.69231840863471,-1.,1.02919977579155));
#38685=CARTESIAN_POINT('Ctrl Pts',(-1.68836910178475,-1.,1.02460180535272));
#38686=CARTESIAN_POINT('Ctrl Pts',(-1.68440578021739,-1.,1.02006795074222));
#38687=CARTESIAN_POINT('Ctrl Pts',(-1.6804428989482,-1.,1.01561026162787));
#38688=CARTESIAN_POINT('Ctrl Pts',(-1.67648246776457,-1.,1.01123236493507));
#38689=CARTESIAN_POINT('Ctrl Pts',(-1.67250335383248,-1.,1.00692206696387));
#38690=CARTESIAN_POINT('Ctrl Pts',(-1.66846059277231,-1.,1.00265091003682));
#38691=CARTESIAN_POINT('Ctrl Pts',(-1.66430758030304,-1.,0.998389654952317));
#38692=CARTESIAN_POINT('Ctrl Pts',(-1.66001553809916,-1.,0.994121836661116));
#38693=CARTESIAN_POINT('Ctrl Pts',(-1.65559044289746,-1.,0.98985562785445));
#38694=CARTESIAN_POINT('Ctrl Pts',(-1.6511001661277,-1.,0.985642622921626));
#38695=CARTESIAN_POINT('Ctrl Pts',(-1.64665139190834,-1.,0.981562530940574));
#38696=CARTESIAN_POINT('Ctrl Pts',(-1.64233990826831,-1.,0.977689794120297));
#38697=CARTESIAN_POINT('Ctrl Pts',(-1.63820952658157,-1.,0.974066058287501));
#38698=CARTESIAN_POINT('Ctrl Pts',(-1.63420665729609,-1.,0.970669715996356));
#38699=CARTESIAN_POINT('Ctrl Pts',(-1.63013849959083,-1.,0.967387853228041));
#38700=CARTESIAN_POINT('Ctrl Pts',(-1.6257193066974,-1.,0.964046107037821));
#38701=CARTESIAN_POINT('Ctrl Pts',(-1.62061638139929,-1.,0.960438326099958));
#38702=CARTESIAN_POINT('Ctrl Pts',(-1.61449324337233,-1.,0.956354422921573));
#38703=CARTESIAN_POINT('Ctrl Pts',(-1.60706069897794,-1.,0.951613284361248));
#38704=CARTESIAN_POINT('Ctrl Pts',(-1.59810042045408,-1.,0.946078063325796));
#38705=CARTESIAN_POINT('Ctrl Pts',(-1.58744937489796,-1.,0.939646377909319));
#38706=CARTESIAN_POINT('Ctrl Pts',(-1.57499388385561,-1.,0.932246680128849));
#38707=CARTESIAN_POINT('Ctrl Pts',(-1.56065988582509,-1.,0.923832188966322));
#38708=CARTESIAN_POINT('Ctrl Pts',(-1.54440491152808,-1.,0.91437591904658));
#38709=CARTESIAN_POINT('Ctrl Pts',(-1.52984849890434,-1.,0.905967409640499));
#38710=CARTESIAN_POINT('Ctrl Pts',(-1.51805569591479,-1.,0.89918504749193));
#38711=CARTESIAN_POINT('Ctrl Pts',(-1.50980486807181,-1.,0.894452006967538));
#38712=CARTESIAN_POINT('Ctrl Pts',(-1.5055822144029,-1.,0.892032620296855));
#38713=CARTESIAN_POINT('',(-1.60662857109684,-1.,0.693717979106305));
#38714=CARTESIAN_POINT('Origin',(0.,-1.,0.));
#38715=CARTESIAN_POINT('',(-2.0698113262342,-1.,0.7455743247944));
#38716=CARTESIAN_POINT('Ctrl Pts',(-1.60662857109684,-1.,0.693717979106305));
#38717=CARTESIAN_POINT('Ctrl Pts',(-1.61106790957619,-1.,0.69571209787897));
#38718=CARTESIAN_POINT('Ctrl Pts',(-1.61974673471117,-1.,0.699605146398837));
#38719=CARTESIAN_POINT('Ctrl Pts',(-1.6321654166204,-1.,0.705159151977294));
#38720=CARTESIAN_POINT('Ctrl Pts',(-1.64752408828442,-1.,0.711993139340447));
#38721=CARTESIAN_POINT('Ctrl Pts',(-1.66472880551777,-1.,0.71958543378795));
#38722=CARTESIAN_POINT('Ctrl Pts',(-1.67996158451922,-1.,0.726235967982445));
#38723=CARTESIAN_POINT('Ctrl Pts',(-1.69326921972915,-1.,0.731963238685357));
#38724=CARTESIAN_POINT('Ctrl Pts',(-1.70473309004249,-1.,0.736799665716932));
#38725=CARTESIAN_POINT('Ctrl Pts',(-1.71447789751001,-1.,0.74079516202821));
#38726=CARTESIAN_POINT('Ctrl Pts',(-1.72268229916769,-1.,0.744021445433093));
#38727=CARTESIAN_POINT('Ctrl Pts',(-1.72958533647714,-1.,0.746574710097752));
#38728=CARTESIAN_POINT('Ctrl Pts',(-1.7355035168033,-1.,0.74858246295687));
#38729=CARTESIAN_POINT('Ctrl Pts',(-1.74080458267114,-1.,0.750193435981249));
#38730=CARTESIAN_POINT('Ctrl Pts',(-1.74585086852502,-1.,0.751555614164482));
#38731=CARTESIAN_POINT('Ctrl Pts',(-1.75095139468794,-1.,0.752797683531314));
#38732=CARTESIAN_POINT('Ctrl Pts',(-1.75631083600019,-1.,0.754009254027829));
#38733=CARTESIAN_POINT('Ctrl Pts',(-1.76197817240128,-1.,0.755220979974461));
#38734=CARTESIAN_POINT('Ctrl Pts',(-1.76789396002998,-1.,0.75642189602781));
#38735=CARTESIAN_POINT('Ctrl Pts',(-1.77394167108292,-1.,0.757578264077029));
#38736=CARTESIAN_POINT('Ctrl Pts',(-1.77999411220945,-1.,0.758650626677518));
#38737=CARTESIAN_POINT('Ctrl Pts',(-1.78596964884604,-1.,0.759614401110189));
#38738=CARTESIAN_POINT('Ctrl Pts',(-1.7918581561088,-1.,0.760469555880749));
#38739=CARTESIAN_POINT('Ctrl Pts',(-1.79768986997783,-1.,0.761229695230558));
#38740=CARTESIAN_POINT('Ctrl Pts',(-1.80351583877342,-1.,0.761915336443547));
#38741=CARTESIAN_POINT('Ctrl Pts',(-1.80938551463965,-1.,0.762546129463938));
#38742=CARTESIAN_POINT('Ctrl Pts',(-1.8153211840553,-1.,0.763132003836634));
#38743=CARTESIAN_POINT('Ctrl Pts',(-1.82131873145266,-1.,0.763673465462726));
#38744=CARTESIAN_POINT('Ctrl Pts',(-1.82735991200065,-1.,0.764165902605995));
#38745=CARTESIAN_POINT('Ctrl Pts',(-1.83342077227142,-1.,0.764602549687853));
#38746=CARTESIAN_POINT('Ctrl Pts',(-1.83948181064835,-1.,0.764978057881737));
#38747=CARTESIAN_POINT('Ctrl Pts',(-1.84553698875924,-1.,0.765291664862029));
#38748=CARTESIAN_POINT('Ctrl Pts',(-1.85158945130063,-1.,0.765545710619062));
#38749=CARTESIAN_POINT('Ctrl Pts',(-1.85764741390394,-1.,0.765744212909318));
#38750=CARTESIAN_POINT('Ctrl Pts',(-1.86372027063312,-1.,0.765891519092547));
#38751=CARTESIAN_POINT('Ctrl Pts',(-1.86981398314341,-1.,0.765990708546091));
#38752=CARTESIAN_POINT('Ctrl Pts',(-1.87592888967883,-1.,0.766042837036744));
#38753=CARTESIAN_POINT('Ctrl Pts',(-1.88206215302561,-1.,0.766047794851864));
#38754=CARTESIAN_POINT('Ctrl Pts',(-1.88820926433409,-1.,0.766004837062091));
#38755=CARTESIAN_POINT('Ctrl Pts',(-1.89436577771388,-1.,0.765913193856978));
#38756=CARTESIAN_POINT('Ctrl Pts',(-1.90052930393596,-1.,0.765772772593386));
#38757=CARTESIAN_POINT('Ctrl Pts',(-1.90669961402356,-1.,0.765584196937919));
#38758=CARTESIAN_POINT('Ctrl Pts',(-1.91287765805169,-1.,0.765348465884722));
#38759=CARTESIAN_POINT('Ctrl Pts',(-1.91906491634196,-1.,0.765066729667088));
#38760=CARTESIAN_POINT('Ctrl Pts',(-1.92526263537048,-1.,0.764740025488211));
#38761=CARTESIAN_POINT('Ctrl Pts',(-1.93147105496382,-1.,0.76436901067394));
#38762=CARTESIAN_POINT('Ctrl Pts',(-1.93768964875886,-1.,0.763954049121458));
#38763=CARTESIAN_POINT('Ctrl Pts',(-1.9439174661764,-1.,0.763495333538629));
#38764=CARTESIAN_POINT('Ctrl Pts',(-1.95015342590024,-1.,0.762992990878769));
#38765=CARTESIAN_POINT('Ctrl Pts',(-1.95639665309869,-1.,0.762447203806179));
#38766=CARTESIAN_POINT('Ctrl Pts',(-1.96264672744186,-1.,0.761858300014423));
#38767=CARTESIAN_POINT('Ctrl Pts',(-1.96890351582499,-1.,0.76122669048382));
#38768=CARTESIAN_POINT('Ctrl Pts',(-1.97516705321494,-1.,0.760552825409757));
#38769=CARTESIAN_POINT('Ctrl Pts',(-1.98143741418172,-1.,0.75983714745219));
#38770=CARTESIAN_POINT('Ctrl Pts',(-1.98771456680874,-1.,0.759080037802488));
#38771=CARTESIAN_POINT('Ctrl Pts',(-1.99399831098817,-1.,0.758281796766761));
#38772=CARTESIAN_POINT('Ctrl Pts',(-2.00028834739178,-1.,0.757442676862724));
#38773=CARTESIAN_POINT('Ctrl Pts',(-2.0065843158773,-1.,0.75656290464667));
#38774=CARTESIAN_POINT('Ctrl Pts',(-2.01288584328084,-1.,0.755642704957865));
#38775=CARTESIAN_POINT('Ctrl Pts',(-2.01919259405809,-1.,0.754682330722816));
#38776=CARTESIAN_POINT('Ctrl Pts',(-2.02550428623313,-1.,0.753682061112768));
#38777=CARTESIAN_POINT('Ctrl Pts',(-2.03182068456221,-1.,0.752642180487211));
#38778=CARTESIAN_POINT('Ctrl Pts',(-2.03814160092099,-1.,0.751562963361115));
#38779=CARTESIAN_POINT('Ctrl Pts',(-2.04446689147979,-1.,0.750444657875576));
#38780=CARTESIAN_POINT('Ctrl Pts',(-2.05079645592154,-1.,0.749287468665046));
#38781=CARTESIAN_POINT('Ctrl Pts',(-2.05713023031006,-1.,0.748091554183802));
#38782=CARTESIAN_POINT('Ctrl Pts',(-2.06220058927826,-1.,0.747103932787919));
#38783=CARTESIAN_POINT('Ctrl Pts',(-2.06600523016815,-1.,0.7463458715442));
#38784=CARTESIAN_POINT('Ctrl Pts',(-2.06854248895728,-1.,0.745832791378367));
#38785=CARTESIAN_POINT('Ctrl Pts',(-2.0698113262342,-1.,0.7455743247944));
#38786=CARTESIAN_POINT('',(-2.11275013067528,-1.,0.61342227326009));
#38787=CARTESIAN_POINT('',(-2.0698113262342,-1.,0.7455743247944));
#38788=CARTESIAN_POINT('',(-1.7075470150345,-1.,0.383122945602004));
#38789=CARTESIAN_POINT('Ctrl Pts',(-2.11275013067528,-1.,0.61342227326009));
#38790=CARTESIAN_POINT('Ctrl Pts',(-2.11187554259986,-1.,0.6124673655618));
#38791=CARTESIAN_POINT('Ctrl Pts',(-2.11012443807238,-1.,0.610560911689899));
#38792=CARTESIAN_POINT('Ctrl Pts',(-2.1074919961518,-1.,0.607711315454876));
#38793=CARTESIAN_POINT('Ctrl Pts',(-2.10397049886949,-1.,0.60393203073603));
#38794=CARTESIAN_POINT('Ctrl Pts',(-2.0995493086477,-1.,0.599241616420533));
#38795=CARTESIAN_POINT('Ctrl Pts',(-2.0951087622027,-1.,0.594585006052162));
#38796=CARTESIAN_POINT('Ctrl Pts',(-2.09064881812129,-1.,0.589962365403406));
#38797=CARTESIAN_POINT('Ctrl Pts',(-2.08616943727951,-1.,0.585373918991617));
#38798=CARTESIAN_POINT('Ctrl Pts',(-2.08167059018418,-1.,0.580819952108063));
#38799=CARTESIAN_POINT('Ctrl Pts',(-2.07715226767559,-1.,0.576300797416844));
#38800=CARTESIAN_POINT('Ctrl Pts',(-2.07261449292824,-1.,0.571816823242603));
#38801=CARTESIAN_POINT('Ctrl Pts',(-2.06805732997334,-1.,0.567368421181087));
#38802=CARTESIAN_POINT('Ctrl Pts',(-2.06348090160589,-1.,0.562955993082261));
#38803=CARTESIAN_POINT('Ctrl Pts',(-2.05888537756462,-1.,0.558579940185151));
#38804=CARTESIAN_POINT('Ctrl Pts',(-2.05427091604413,-1.,0.554240657463906));
#38805=CARTESIAN_POINT('Ctrl Pts',(-2.04963761077958,-1.,0.549938525150295));
#38806=CARTESIAN_POINT('Ctrl Pts',(-2.04498544714588,-1.,0.54567390381743));
#38807=CARTESIAN_POINT('Ctrl Pts',(-2.04031422690527,-1.,0.541447120615659));
#38808=CARTESIAN_POINT('Ctrl Pts',(-2.03562362954037,-1.,0.537258489833262));
#38809=CARTESIAN_POINT('Ctrl Pts',(-2.03091336214426,-1.,0.533108355132976));
#38810=CARTESIAN_POINT('Ctrl Pts',(-2.0261832908329,-1.,0.528997127241914));
#38811=CARTESIAN_POINT('Ctrl Pts',(-2.02143356304698,-1.,0.524925318333476));
#38812=CARTESIAN_POINT('Ctrl Pts',(-2.01666477917286,-1.,0.52089359039937));
#38813=CARTESIAN_POINT('Ctrl Pts',(-2.01187773939242,-1.,0.516902681728687));
#38814=CARTESIAN_POINT('Ctrl Pts',(-2.00707309946949,-1.,0.512953306961792));
#38815=CARTESIAN_POINT('Ctrl Pts',(-2.00225107134734,-1.,0.509046069886157));
#38816=CARTESIAN_POINT('Ctrl Pts',(-1.99741107463572,-1.,0.505181361323026));
#38817=CARTESIAN_POINT('Ctrl Pts',(-1.99255149126155,-1.,0.501359287727146));
#38818=CARTESIAN_POINT('Ctrl Pts',(-1.98767044752932,-1.,0.497579909545574));
#38819=CARTESIAN_POINT('Ctrl Pts',(-1.98276658761821,-1.,0.493843476541494));
#38820=CARTESIAN_POINT('Ctrl Pts',(-1.97783973019229,-1.,0.490150627860952));
#38821=CARTESIAN_POINT('Ctrl Pts',(-1.97289186263272,-1.,0.486502692907659));
#38822=CARTESIAN_POINT('Ctrl Pts',(-1.96792703422362,-1.,0.48290166212069));
#38823=CARTESIAN_POINT('Ctrl Pts',(-1.96294933055943,-1.,0.479349583074855));
#38824=CARTESIAN_POINT('Ctrl Pts',(-1.95796111148177,-1.,0.475848034683176));
#38825=CARTESIAN_POINT('Ctrl Pts',(-1.95296148278133,-1.,0.472397672264072));
#38826=CARTESIAN_POINT('Ctrl Pts',(-1.94794381136514,-1.,0.468997482913135));
#38827=CARTESIAN_POINT('Ctrl Pts',(-1.9428979419619,-1.,0.46564546202603));
#38828=CARTESIAN_POINT('Ctrl Pts',(-1.93781486640821,-1.,0.462340031009056));
#38829=CARTESIAN_POINT('Ctrl Pts',(-1.93269066517934,-1.,0.459081234547926));
#38830=CARTESIAN_POINT('Ctrl Pts',(-1.92753067150476,-1.,0.455872005174371));
#38831=CARTESIAN_POINT('Ctrl Pts',(-1.92235380648502,-1.,0.452719478359432));
#38832=CARTESIAN_POINT('Ctrl Pts',(-1.91718342555755,-1.,0.449632260106662));
#38833=CARTESIAN_POINT('Ctrl Pts',(-1.9120369998112,-1.,0.446617343485711));
#38834=CARTESIAN_POINT('Ctrl Pts',(-1.90691756144898,-1.,0.44367755684915));
#38835=CARTESIAN_POINT('Ctrl Pts',(-1.90180124389086,-1.,0.440807833704038));
#38836=CARTESIAN_POINT('Ctrl Pts',(-1.89663648956466,-1.,0.437995003948244));
#38837=CARTESIAN_POINT('Ctrl Pts',(-1.89136993975504,-1.,0.435225660963383));
#38838=CARTESIAN_POINT('Ctrl Pts',(-1.88596913666793,-1.,0.432493038548748));
#38839=CARTESIAN_POINT('Ctrl Pts',(-1.88044229001832,-1.,0.429803062482344));
#38840=CARTESIAN_POINT('Ctrl Pts',(-1.87486989291484,-1.,0.427183828519102));
#38841=CARTESIAN_POINT('Ctrl Pts',(-1.86937803944323,-1.,0.424678177291359));
#38842=CARTESIAN_POINT('Ctrl Pts',(-1.86408083334028,-1.,0.422327307418275));
#38843=CARTESIAN_POINT('Ctrl Pts',(-1.85903281096686,-1.,0.420157287975619));
#38844=CARTESIAN_POINT('Ctrl Pts',(-1.85417632856234,-1.,0.418164129143534));
#38845=CARTESIAN_POINT('Ctrl Pts',(-1.84929312929882,-1.,0.416300022038864));
#38846=CARTESIAN_POINT('Ctrl Pts',(-1.8440575707371,-1.,0.41448743825434));
#38847=CARTESIAN_POINT('Ctrl Pts',(-1.83808953475839,-1.,0.412633125322161));
#38848=CARTESIAN_POINT('Ctrl Pts',(-1.83100408895216,-1.,0.410641256301675));
#38849=CARTESIAN_POINT('Ctrl Pts',(-1.8224702267854,-1.,0.408428948108533));
#38850=CARTESIAN_POINT('Ctrl Pts',(-1.81223801813988,-1.,0.405933518411838));
#38851=CARTESIAN_POINT('Ctrl Pts',(-1.80012077176221,-1.,0.403107976170441));
#38852=CARTESIAN_POINT('Ctrl Pts',(-1.78598826347533,-1.,0.39991940378308));
#38853=CARTESIAN_POINT('Ctrl Pts',(-1.7697556004756,-1.,0.39634619612042));
#38854=CARTESIAN_POINT('Ctrl Pts',(-1.75137405313962,-1.,0.392375812294307));
#38855=CARTESIAN_POINT('Ctrl Pts',(-1.7349317097561,-1.,0.388877023509191));
#38856=CARTESIAN_POINT('Ctrl Pts',(-1.72162022246158,-1.,0.38607079032701));
#38857=CARTESIAN_POINT('Ctrl Pts',(-1.71231062891958,-1.,0.384119047315542));
#38858=CARTESIAN_POINT('Ctrl Pts',(-1.7075470150345,-1.,0.383122945602004));
#38859=CARTESIAN_POINT('',(-1.74236521665491,-1.,0.163289472382896));
#38860=CARTESIAN_POINT('Origin',(0.,-1.,0.));
#38861=CARTESIAN_POINT('',(-2.19890268624765,-1.,0.069476445021958));
#38862=CARTESIAN_POINT('Ctrl Pts',(-1.74236521665491,-1.,0.163289472382896));
#38863=CARTESIAN_POINT('Ctrl Pts',(-1.7472034950333,-1.,0.163814161002002));
#38864=CARTESIAN_POINT('Ctrl Pts',(-1.75666056638427,-1.,0.164834765707158));
#38865=CARTESIAN_POINT('Ctrl Pts',(-1.77018771684844,-1.,0.1662793551464));
#38866=CARTESIAN_POINT('Ctrl Pts',(-1.7869064998507,-1.,0.168032772805197));
#38867=CARTESIAN_POINT('Ctrl Pts',(-1.80561530629706,-1.,0.169936923904608));
#38868=CARTESIAN_POINT('Ctrl Pts',(-1.82215766811545,-1.,0.171554770204119));
#38869=CARTESIAN_POINT('Ctrl Pts',(-1.83658380527692,-1.,0.1728894428919));
#38870=CARTESIAN_POINT('Ctrl Pts',(-1.8489811319852,-1.,0.173946627587731));
#38871=CARTESIAN_POINT('Ctrl Pts',(-1.85948367088837,-1.,0.17473525927603));
#38872=CARTESIAN_POINT('Ctrl Pts',(-1.86828349694799,-1.,0.175268337590758));
#38873=CARTESIAN_POINT('Ctrl Pts',(-1.87563767773588,-1.,0.175563480746485));
#38874=CARTESIAN_POINT('Ctrl Pts',(-1.88188663145367,-1.,0.175644148889698));
#38875=CARTESIAN_POINT('Ctrl Pts',(-1.88742606273259,-1.,0.175538155840648));
#38876=CARTESIAN_POINT('Ctrl Pts',(-1.892646301985,-1.,0.175274276190844));
#38877=CARTESIAN_POINT('Ctrl Pts',(-1.89788101117132,-1.,0.174879405091263));
#38878=CARTESIAN_POINT('Ctrl Pts',(-1.90335253862834,-1.,0.174375518661085));
#38879=CARTESIAN_POINT('Ctrl Pts',(-1.90911693975267,-1.,0.173776635257817));
#38880=CARTESIAN_POINT('Ctrl Pts',(-1.91511429159527,-1.,0.173090695383496));
#38881=CARTESIAN_POINT('Ctrl Pts',(-1.9212233439798,-1.,0.172321621259514));
#38882=CARTESIAN_POINT('Ctrl Pts',(-1.92731093582036,-1.,0.171471191532988));
#38883=CARTESIAN_POINT('Ctrl Pts',(-1.93329183155539,-1.,0.170541253116201));
#38884=CARTESIAN_POINT('Ctrl Pts',(-1.93915639211581,-1.,0.169534904817491));
#38885=CARTESIAN_POINT('Ctrl Pts',(-1.94493757756931,-1.,0.168455741607556));
#38886=CARTESIAN_POINT('Ctrl Pts',(-1.95069027794294,-1.,0.167307501784475));
#38887=CARTESIAN_POINT('Ctrl Pts',(-1.9564675971873,-1.,0.166093592002812));
#38888=CARTESIAN_POINT('Ctrl Pts',(-1.96229379940136,-1.,0.164816568920269));
#38889=CARTESIAN_POINT('Ctrl Pts',(-1.96816512677967,-1.,0.163478185457734));
#38890=CARTESIAN_POINT('Ctrl Pts',(-1.97406280235188,-1.,0.162079693556288));
#38891=CARTESIAN_POINT('Ctrl Pts',(-1.97996195437559,-1.,0.160622060784611));
#38892=CARTESIAN_POINT('Ctrl Pts',(-1.98584238283292,-1.,0.159106226437299));
#38893=CARTESIAN_POINT('Ctrl Pts',(-1.99169810931908,-1.,0.157533331459227));
#38894=CARTESIAN_POINT('Ctrl Pts',(-1.99753284771497,-1.,0.155904629548783));
#38895=CARTESIAN_POINT('Ctrl Pts',(-2.00335565310543,-1.,0.154221403049722));
#38896=CARTESIAN_POINT('Ctrl Pts',(-2.00917680318424,-1.,0.15248488362145));
#38897=CARTESIAN_POINT('Ctrl Pts',(-2.01500291940238,-1.,0.150696157673078));
#38898=CARTESIAN_POINT('Ctrl Pts',(-2.02083464969894,-1.,0.148856124775337));
#38899=CARTESIAN_POINT('Ctrl Pts',(-2.02666926182017,-1.,0.146965557332583));
#38900=CARTESIAN_POINT('Ctrl Pts',(-2.03250223739942,-1.,0.145025140186057));
#38901=CARTESIAN_POINT('Ctrl Pts',(-2.03832911025912,-1.,0.143035515058209));
#38902=CARTESIAN_POINT('Ctrl Pts',(-2.04414757947916,-1.,0.140997332152546));
#38903=CARTESIAN_POINT('Ctrl Pts',(-2.04995762001328,-1.,0.138911255368966));
#38904=CARTESIAN_POINT('Ctrl Pts',(-2.05576044414264,-1.,0.136777941218043));
#38905=CARTESIAN_POINT('Ctrl Pts',(-2.06155781517842,-1.,0.134598026192106));
#38906=CARTESIAN_POINT('Ctrl Pts',(-2.06735123910326,-1.,0.13237211154771));
#38907=CARTESIAN_POINT('Ctrl Pts',(-2.07314114713063,-1.,0.130100748328403));
#38908=CARTESIAN_POINT('Ctrl Pts',(-2.07892715110987,-1.,0.12778444527612));
#38909=CARTESIAN_POINT('Ctrl Pts',(-2.08470840653643,-1.,0.125423679412061));
#38910=CARTESIAN_POINT('Ctrl Pts',(-2.09048392424825,-1.,0.123018905621083));
#38911=CARTESIAN_POINT('Ctrl Pts',(-2.0962529286773,-1.,0.120570567965122));
#38912=CARTESIAN_POINT('Ctrl Pts',(-2.102015121329,-1.,0.118079107988355));
#38913=CARTESIAN_POINT('Ctrl Pts',(-2.10777050261309,-1.,0.115544957687926));
#38914=CARTESIAN_POINT('Ctrl Pts',(-2.11351924490306,-1.,0.112968534419737));
#38915=CARTESIAN_POINT('Ctrl Pts',(-2.11926155590865,-1.,0.110350236135025));
#38916=CARTESIAN_POINT('Ctrl Pts',(-2.12499752307,-1.,0.10769043523109));
#38917=CARTESIAN_POINT('Ctrl Pts',(-2.13072704887293,-1.,0.104989479152739));
#38918=CARTESIAN_POINT('Ctrl Pts',(-2.13644992667165,-1.,0.1022477005561));
#38919=CARTESIAN_POINT('Ctrl Pts',(-2.14216588396025,-1.,0.0994654261990914));
#38920=CARTESIAN_POINT('Ctrl Pts',(-2.14787463531795,-1.,0.0966429852305457));
#38921=CARTESIAN_POINT('Ctrl Pts',(-2.1535759397817,-1.,0.0937807218867642));
#38922=CARTESIAN_POINT('Ctrl Pts',(-2.15926961544516,-1.,0.0908789888107264));
#38923=CARTESIAN_POINT('Ctrl Pts',(-2.16495552645014,-1.,0.0879381291386921));
#38924=CARTESIAN_POINT('Ctrl Pts',(-2.17063357870952,-1.,0.0849584620835371));
#38925=CARTESIAN_POINT('Ctrl Pts',(-2.176303712113,-1.,0.0819402680872764));
#38926=CARTESIAN_POINT('Ctrl Pts',(-2.18196589448887,-1.,0.0788837727685241));
#38927=CARTESIAN_POINT('Ctrl Pts',(-2.1876201139953,-1.,0.0757891465836146));
#38928=CARTESIAN_POINT('Ctrl Pts',(-2.19213712013662,-1.,0.0732830357306724));
#38929=CARTESIAN_POINT('Ctrl Pts',(-2.19552129484002,-1.,0.0713863779526153));
#38930=CARTESIAN_POINT('Ctrl Pts',(-2.19777582085423,-1.,0.0701143536325489));
#38931=CARTESIAN_POINT('Ctrl Pts',(-2.19890268624765,-1.,0.069476445021958));
#38932=CARTESIAN_POINT('',(-2.19890268624765,-1.,-0.0694764450219585));
#38933=CARTESIAN_POINT('',(-2.19890268624765,-1.,0.069476445021958));
#38934=CARTESIAN_POINT('',(-1.74236521665491,-1.,-0.163289472382896));
#38935=CARTESIAN_POINT('Ctrl Pts',(-2.19890268624765,-1.,-0.0694764450219585));
#38936=CARTESIAN_POINT('Ctrl Pts',(-2.19777582085261,-1.,-0.0701143536324927));
#38937=CARTESIAN_POINT('Ctrl Pts',(-2.19552129483562,-1.,-0.0713863779524629));
#38938=CARTESIAN_POINT('Ctrl Pts',(-2.19213712012956,-1.,-0.0732830357304277));
#38939=CARTESIAN_POINT('Ctrl Pts',(-2.1876201139874,-1.,-0.0757891465833413));
#38940=CARTESIAN_POINT('Ctrl Pts',(-2.18196589448304,-1.,-0.0788837727683229));
#38941=CARTESIAN_POINT('Ctrl Pts',(-2.1763037121106,-1.,-0.0819402680871941));
#38942=CARTESIAN_POINT('Ctrl Pts',(-2.17063357871031,-1.,-0.0849584620835644));
#38943=CARTESIAN_POINT('Ctrl Pts',(-2.16495552645275,-1.,-0.0879381291387824));
#38944=CARTESIAN_POINT('Ctrl Pts',(-2.15926961544808,-1.,-0.0908789888108267));
#38945=CARTESIAN_POINT('Ctrl Pts',(-2.15357593978377,-1.,-0.0937807218868346));
#38946=CARTESIAN_POINT('Ctrl Pts',(-2.14787463531864,-1.,-0.096642985230569));
#38947=CARTESIAN_POINT('Ctrl Pts',(-2.14216588395974,-1.,-0.0994654261990744));
#38948=CARTESIAN_POINT('Ctrl Pts',(-2.13644992667052,-1.,-0.102247700556064));
#38949=CARTESIAN_POINT('Ctrl Pts',(-2.1307270488718,-1.,-0.104989479152703));
#38950=CARTESIAN_POINT('Ctrl Pts',(-2.12499752306927,-1.,-0.107690435231068));
#38951=CARTESIAN_POINT('Ctrl Pts',(-2.11926155590849,-1.,-0.11035023613502));
#38952=CARTESIAN_POINT('Ctrl Pts',(-2.11351924490335,-1.,-0.112968534419746));
#38953=CARTESIAN_POINT('Ctrl Pts',(-2.10777050261359,-1.,-0.11554495768794));
#38954=CARTESIAN_POINT('Ctrl Pts',(-2.10201512132945,-1.,-0.118079107988368));
#38955=CARTESIAN_POINT('Ctrl Pts',(-2.09625292867756,-1.,-0.120570567965129));
#38956=CARTESIAN_POINT('Ctrl Pts',(-2.09048392424826,-1.,-0.123018905621083));
#38957=CARTESIAN_POINT('Ctrl Pts',(-2.08470840653628,-1.,-0.125423679412058));
#38958=CARTESIAN_POINT('Ctrl Pts',(-2.07892715110967,-1.,-0.127784445276116));
#38959=CARTESIAN_POINT('Ctrl Pts',(-2.07314114713047,-1.,-0.130100748328401));
#38960=CARTESIAN_POINT('Ctrl Pts',(-2.06735123910319,-1.,-0.13237211154771));
#38961=CARTESIAN_POINT('Ctrl Pts',(-2.06155781517844,-1.,-0.134598026192107));
#38962=CARTESIAN_POINT('Ctrl Pts',(-2.0557604441427,-1.,-0.136777941218044));
#38963=CARTESIAN_POINT('Ctrl Pts',(-2.04995762001333,-1.,-0.138911255368966));
#38964=CARTESIAN_POINT('Ctrl Pts',(-2.04414757947919,-1.,-0.140997332152545));
#38965=CARTESIAN_POINT('Ctrl Pts',(-2.03832911025913,-1.,-0.143035515058208));
#38966=CARTESIAN_POINT('Ctrl Pts',(-2.03250223739941,-1.,-0.145025140186058));
#38967=CARTESIAN_POINT('Ctrl Pts',(-2.02666926182017,-1.,-0.146965557332586));
#38968=CARTESIAN_POINT('Ctrl Pts',(-2.02083464969897,-1.,-0.148856124775343));
#38969=CARTESIAN_POINT('Ctrl Pts',(-2.01500291940243,-1.,-0.150696157673084));
#38970=CARTESIAN_POINT('Ctrl Pts',(-2.00917680318426,-1.,-0.152484883621452));
#38971=CARTESIAN_POINT('Ctrl Pts',(-2.00335565310539,-1.,-0.154221403049719));
#38972=CARTESIAN_POINT('Ctrl Pts',(-1.99753284771487,-1.,-0.155904629548775));
#38973=CARTESIAN_POINT('Ctrl Pts',(-1.99169810931893,-1.,-0.157533331459215));
#38974=CARTESIAN_POINT('Ctrl Pts',(-1.98584238283279,-1.,-0.159106226437289));
#38975=CARTESIAN_POINT('Ctrl Pts',(-1.97996195437557,-1.,-0.16062206078461));
#38976=CARTESIAN_POINT('Ctrl Pts',(-1.97406280235204,-1.,-0.162079693556302));
#38977=CARTESIAN_POINT('Ctrl Pts',(-1.96816512678,-1.,-0.16347818545776));
#38978=CARTESIAN_POINT('Ctrl Pts',(-1.96229379940174,-1.,-0.1648165689203));
#38979=CARTESIAN_POINT('Ctrl Pts',(-1.95646759718755,-1.,-0.166093592002833));
#38980=CARTESIAN_POINT('Ctrl Pts',(-1.95069027794286,-1.,-0.167307501784469));
#38981=CARTESIAN_POINT('Ctrl Pts',(-1.94493757756879,-1.,-0.168455741607516));
#38982=CARTESIAN_POINT('Ctrl Pts',(-1.93915639211497,-1.,-0.169534904817425));
#38983=CARTESIAN_POINT('Ctrl Pts',(-1.93329183155455,-1.,-0.170541253116136));
#38984=CARTESIAN_POINT('Ctrl Pts',(-1.92731093582,-1.,-0.17147119153296));
#38985=CARTESIAN_POINT('Ctrl Pts',(-1.92122334398034,-1.,-0.172321621259557));
#38986=CARTESIAN_POINT('Ctrl Pts',(-1.91511429159681,-1.,-0.173090695383619));
#38987=CARTESIAN_POINT('Ctrl Pts',(-1.90911693975475,-1.,-0.173776635257984));
#38988=CARTESIAN_POINT('Ctrl Pts',(-1.90335253863003,-1.,-0.174375518661222));
#38989=CARTESIAN_POINT('Ctrl Pts',(-1.89788101117148,-1.,-0.174879405091277));
#38990=CARTESIAN_POINT('Ctrl Pts',(-1.89264630198279,-1.,-0.175274276190664));
#38991=CARTESIAN_POINT('Ctrl Pts',(-1.88742606272818,-1.,-0.175538155840286));
#38992=CARTESIAN_POINT('Ctrl Pts',(-1.88188663144846,-1.,-0.175644148889271));
#38993=CARTESIAN_POINT('Ctrl Pts',(-1.87563767773249,-1.,-0.175563480746205));
#38994=CARTESIAN_POINT('Ctrl Pts',(-1.86828349694972,-1.,-0.175268337590901));
#38995=CARTESIAN_POINT('Ctrl Pts',(-1.85948367089838,-1.,-0.174735259276856));
#38996=CARTESIAN_POINT('Ctrl Pts',(-1.84898113200543,-1.,-0.173946627589401));
#38997=CARTESIAN_POINT('Ctrl Pts',(-1.83658380530747,-1.,-0.17288944289442));
#38998=CARTESIAN_POINT('Ctrl Pts',(-1.82215766815414,-1.,-0.171554770207306));
#38999=CARTESIAN_POINT('Ctrl Pts',(-1.80561530633924,-1.,-0.169936923908078));
#39000=CARTESIAN_POINT('Ctrl Pts',(-1.78690649988931,-1.,-0.16803277280837));
#39001=CARTESIAN_POINT('Ctrl Pts',(-1.77018771687692,-1.,-0.166279355148738));
#39002=CARTESIAN_POINT('Ctrl Pts',(-1.75666056640041,-1.,-0.164834765708484));
#39003=CARTESIAN_POINT('Ctrl Pts',(-1.74720349503904,-1.,-0.163814161002474));
#39004=CARTESIAN_POINT('Ctrl Pts',(-1.74236521665491,-1.,-0.163289472382896));
#39005=CARTESIAN_POINT('',(-1.7075470150345,-1.,-0.383122945602004));
#39006=CARTESIAN_POINT('Origin',(0.,-1.,0.));
#39007=CARTESIAN_POINT('',(-2.11275013067528,-1.,-0.61342227326009));
#39008=CARTESIAN_POINT('Ctrl Pts',(-1.7075470150345,-1.,-0.383122945602004));
#39009=CARTESIAN_POINT('Ctrl Pts',(-1.71231062891398,-1.,-0.384119047314215));
#39010=CARTESIAN_POINT('Ctrl Pts',(-1.72162022244582,-1.,-0.386070790323281));
#39011=CARTESIAN_POINT('Ctrl Pts',(-1.73493170972829,-1.,-0.388877023502615));
#39012=CARTESIAN_POINT('Ctrl Pts',(-1.75137405310193,-1.,-0.392375812285395));
#39013=CARTESIAN_POINT('Ctrl Pts',(-1.76975560043442,-1.,-0.396346196110688));
#39014=CARTESIAN_POINT('Ctrl Pts',(-1.78598826343754,-1.,-0.399919403774155));
#39015=CARTESIAN_POINT('Ctrl Pts',(-1.80012077173238,-1.,-0.403107976163396));
#39016=CARTESIAN_POINT('Ctrl Pts',(-1.81223801812013,-1.,-0.405933518407175));
#39017=CARTESIAN_POINT('Ctrl Pts',(-1.82247022677562,-1.,-0.408428948106227));
#39018=CARTESIAN_POINT('Ctrl Pts',(-1.83100408895047,-1.,-0.410641256301276));
#39019=CARTESIAN_POINT('Ctrl Pts',(-1.8380895347617,-1.,-0.412633125322945));
#39020=CARTESIAN_POINT('Ctrl Pts',(-1.84405757074218,-1.,-0.414487438255542));
#39021=CARTESIAN_POINT('Ctrl Pts',(-1.84929312930314,-1.,-0.416300022039885));
#39022=CARTESIAN_POINT('Ctrl Pts',(-1.8541763285645,-1.,-0.418164129144045));
#39023=CARTESIAN_POINT('Ctrl Pts',(-1.8590328109667,-1.,-0.420157287975583));
#39024=CARTESIAN_POINT('Ctrl Pts',(-1.86408083333863,-1.,-0.422327307417884));
#39025=CARTESIAN_POINT('Ctrl Pts',(-1.8693780394412,-1.,-0.424678177290876));
#39026=CARTESIAN_POINT('Ctrl Pts',(-1.87486989291333,-1.,-0.427183828518743));
#39027=CARTESIAN_POINT('Ctrl Pts',(-1.88044229001778,-1.,-0.429803062482217));
#39028=CARTESIAN_POINT('Ctrl Pts',(-1.88596913666828,-1.,-0.432493038548833));
#39029=CARTESIAN_POINT('Ctrl Pts',(-1.89136993975585,-1.,-0.43522566096358));
#39030=CARTESIAN_POINT('Ctrl Pts',(-1.89663648956549,-1.,-0.437995003948443));
#39031=CARTESIAN_POINT('Ctrl Pts',(-1.90180124389137,-1.,-0.44080783370416));
#39032=CARTESIAN_POINT('Ctrl Pts',(-1.90691756144906,-1.,-0.44367755684917));
#39033=CARTESIAN_POINT('Ctrl Pts',(-1.91203699981095,-1.,-0.446617343485651));
#39034=CARTESIAN_POINT('Ctrl Pts',(-1.91718342555717,-1.,-0.449632260106572));
#39035=CARTESIAN_POINT('Ctrl Pts',(-1.9223538064847,-1.,-0.452719478359356));
#39036=CARTESIAN_POINT('Ctrl Pts',(-1.92753067150461,-1.,-0.455872005174335));
#39037=CARTESIAN_POINT('Ctrl Pts',(-1.93269066517936,-1.,-0.459081234547931));
#39038=CARTESIAN_POINT('Ctrl Pts',(-1.93781486640834,-1.,-0.462340031009087));
#39039=CARTESIAN_POINT('Ctrl Pts',(-1.94289794196205,-1.,-0.465645462026064));
#39040=CARTESIAN_POINT('Ctrl Pts',(-1.94794381136524,-1.,-0.468997482913158));
#39041=CARTESIAN_POINT('Ctrl Pts',(-1.95296148278136,-1.,-0.472397672264079));
#39042=CARTESIAN_POINT('Ctrl Pts',(-1.95796111148175,-1.,-0.475848034683171));
#39043=CARTESIAN_POINT('Ctrl Pts',(-1.96294933055938,-1.,-0.479349583074846));
#39044=CARTESIAN_POINT('Ctrl Pts',(-1.96792703422358,-1.,-0.482901662120686));
#39045=CARTESIAN_POINT('Ctrl Pts',(-1.97289186263272,-1.,-0.486502692907661));
#39046=CARTESIAN_POINT('Ctrl Pts',(-1.97783973019229,-1.,-0.490150627860955));
#39047=CARTESIAN_POINT('Ctrl Pts',(-1.9827665876182,-1.,-0.493843476541492));
#39048=CARTESIAN_POINT('Ctrl Pts',(-1.98767044752929,-1.,-0.497579909545564));
#39049=CARTESIAN_POINT('Ctrl Pts',(-1.9925514912615,-1.,-0.501359287727129));
#39050=CARTESIAN_POINT('Ctrl Pts',(-1.99741107463567,-1.,-0.505181361323011));
#39051=CARTESIAN_POINT('Ctrl Pts',(-2.00225107134733,-1.,-0.509046069886152));
#39052=CARTESIAN_POINT('Ctrl Pts',(-2.00707309946955,-1.,-0.512953306961813));
#39053=CARTESIAN_POINT('Ctrl Pts',(-2.01187773939257,-1.,-0.516902681728733));
#39054=CARTESIAN_POINT('Ctrl Pts',(-2.01666477917305,-1.,-0.520893590399428));
#39055=CARTESIAN_POINT('Ctrl Pts',(-2.02143356304712,-1.,-0.524925318333518));
#39056=CARTESIAN_POINT('Ctrl Pts',(-2.02618329083289,-1.,-0.52899712724191));
#39057=CARTESIAN_POINT('Ctrl Pts',(-2.03091336214401,-1.,-0.533108355132905));
#39058=CARTESIAN_POINT('Ctrl Pts',(-2.03562362953993,-1.,-0.537258489833134));
#39059=CARTESIAN_POINT('Ctrl Pts',(-2.0403142269048,-1.,-0.54144712061552));
#39060=CARTESIAN_POINT('Ctrl Pts',(-2.0449854471456,-1.,-0.545673903817348));
#39061=CARTESIAN_POINT('Ctrl Pts',(-2.04963761077974,-1.,-0.549938525150342));
#39062=CARTESIAN_POINT('Ctrl Pts',(-2.05427091604482,-1.,-0.554240657464109));
#39063=CARTESIAN_POINT('Ctrl Pts',(-2.05888537756571,-1.,-0.558579940185467));
#39064=CARTESIAN_POINT('Ctrl Pts',(-2.06348090160697,-1.,-0.562955993082574));
#39065=CARTESIAN_POINT('Ctrl Pts',(-2.06805732997383,-1.,-0.567368421181229));
#39066=CARTESIAN_POINT('Ctrl Pts',(-2.07261449292757,-1.,-0.571816823242411));
#39067=CARTESIAN_POINT('Ctrl Pts',(-2.07715226767361,-1.,-0.576300797416274));
#39068=CARTESIAN_POINT('Ctrl Pts',(-2.08167059018138,-1.,-0.580819952107257));
#39069=CARTESIAN_POINT('Ctrl Pts',(-2.086169437277,-1.,-0.585373918990895));
#39070=CARTESIAN_POINT('Ctrl Pts',(-2.09064881812053,-1.,-0.589962365403189));
#39071=CARTESIAN_POINT('Ctrl Pts',(-2.09510876220501,-1.,-0.594585006052823));
#39072=CARTESIAN_POINT('Ctrl Pts',(-2.09954930865331,-1.,-0.599241616422144));
#39073=CARTESIAN_POINT('Ctrl Pts',(-2.10397049887709,-1.,-0.603932030738212));
#39074=CARTESIAN_POINT('Ctrl Pts',(-2.10749199615859,-1.,-0.607711315456826));
#39075=CARTESIAN_POINT('Ctrl Pts',(-2.11012443807661,-1.,-0.610560911691113));
#39076=CARTESIAN_POINT('Ctrl Pts',(-2.11187554260142,-1.,-0.61246736556225));
#39077=CARTESIAN_POINT('Ctrl Pts',(-2.11275013067528,-1.,-0.61342227326009));
#39078=CARTESIAN_POINT('',(-2.0698113262342,-1.,-0.745574324794401));
#39079=CARTESIAN_POINT('',(-2.11275013067528,-1.,-0.61342227326009));
#39080=CARTESIAN_POINT('',(-1.60662857109684,-1.,-0.693717979106306));
#39081=CARTESIAN_POINT('Ctrl Pts',(-2.0698113262342,-1.,-0.745574324794401));
#39082=CARTESIAN_POINT('Ctrl Pts',(-2.06854248895575,-1.,-0.74583279137781));
#39083=CARTESIAN_POINT('Ctrl Pts',(-2.06600523016401,-1.,-0.746345871542695));
#39084=CARTESIAN_POINT('Ctrl Pts',(-2.06220058927162,-1.,-0.747103932785504));
#39085=CARTESIAN_POINT('Ctrl Pts',(-2.05713023030263,-1.,-0.748091554181101));
#39086=CARTESIAN_POINT('Ctrl Pts',(-2.05079645591606,-1.,-0.749287468663053));
#39087=CARTESIAN_POINT('Ctrl Pts',(-2.04446689147754,-1.,-0.750444657874758));
#39088=CARTESIAN_POINT('Ctrl Pts',(-2.03814160092173,-1.,-0.751562963361383));
#39089=CARTESIAN_POINT('Ctrl Pts',(-2.03182068456467,-1.,-0.752642180488104));
#39090=CARTESIAN_POINT('Ctrl Pts',(-2.02550428623587,-1.,-0.753682061113765));
#39091=CARTESIAN_POINT('Ctrl Pts',(-2.01919259406003,-1.,-0.75468233072352));
#39092=CARTESIAN_POINT('Ctrl Pts',(-2.01288584328149,-1.,-0.7556427049581));
#39093=CARTESIAN_POINT('Ctrl Pts',(-2.00658431587682,-1.,-0.756562904646496));
#39094=CARTESIAN_POINT('Ctrl Pts',(-2.00028834739072,-1.,-0.757442676862341));
#39095=CARTESIAN_POINT('Ctrl Pts',(-1.9939983109871,-1.,-0.758281796766377));
#39096=CARTESIAN_POINT('Ctrl Pts',(-1.98771456680806,-1.,-0.759080037802242));
#39097=CARTESIAN_POINT('Ctrl Pts',(-1.98143741418156,-1.,-0.759837147452135));
#39098=CARTESIAN_POINT('Ctrl Pts',(-1.97516705321521,-1.,-0.760552825409855));
#39099=CARTESIAN_POINT('Ctrl Pts',(-1.96890351582545,-1.,-0.761226690483986));
#39100=CARTESIAN_POINT('Ctrl Pts',(-1.96264672744229,-1.,-0.761858300014575));
#39101=CARTESIAN_POINT('Ctrl Pts',(-1.95639665309893,-1.,-0.762447203806263));
#39102=CARTESIAN_POINT('Ctrl Pts',(-1.95015342590025,-1.,-0.762992990878774));
#39103=CARTESIAN_POINT('Ctrl Pts',(-1.94391746617626,-1.,-0.76349533353858));
#39104=CARTESIAN_POINT('Ctrl Pts',(-1.93768964875867,-1.,-0.763954049121393));
#39105=CARTESIAN_POINT('Ctrl Pts',(-1.93147105496367,-1.,-0.764369010673889));
#39106=CARTESIAN_POINT('Ctrl Pts',(-1.92526263537041,-1.,-0.764740025488189));
#39107=CARTESIAN_POINT('Ctrl Pts',(-1.91906491634197,-1.,-0.765066729667095));
#39108=CARTESIAN_POINT('Ctrl Pts',(-1.91287765805174,-1.,-0.765348465884739));
#39109=CARTESIAN_POINT('Ctrl Pts',(-1.90669961402362,-1.,-0.765584196937936));
#39110=CARTESIAN_POINT('Ctrl Pts',(-1.90052930393599,-1.,-0.765772772593395));
#39111=CARTESIAN_POINT('Ctrl Pts',(-1.89436577771389,-1.,-0.765913193856979));
#39112=CARTESIAN_POINT('Ctrl Pts',(-1.88820926433409,-1.,-0.76600483706209));
#39113=CARTESIAN_POINT('Ctrl Pts',(-1.88206215302561,-1.,-0.766047794851868));
#39114=CARTESIAN_POINT('Ctrl Pts',(-1.87592888967886,-1.,-0.766042837036759));
#39115=CARTESIAN_POINT('Ctrl Pts',(-1.86981398314345,-1.,-0.765990708546111));
#39116=CARTESIAN_POINT('Ctrl Pts',(-1.86372027063314,-1.,-0.765891519092557));
#39117=CARTESIAN_POINT('Ctrl Pts',(-1.85764741390391,-1.,-0.765744212909305));
#39118=CARTESIAN_POINT('Ctrl Pts',(-1.85158945130054,-1.,-0.765545710619023));
#39119=CARTESIAN_POINT('Ctrl Pts',(-1.8455369887591,-1.,-0.765291664861971));
#39120=CARTESIAN_POINT('Ctrl Pts',(-1.83948181064823,-1.,-0.764978057881687));
#39121=CARTESIAN_POINT('Ctrl Pts',(-1.8334207722714,-1.,-0.764602549687845));
#39122=CARTESIAN_POINT('Ctrl Pts',(-1.8273599120008,-1.,-0.764165902606055));
#39123=CARTESIAN_POINT('Ctrl Pts',(-1.82131873145297,-1.,-0.763673465462854));
#39124=CARTESIAN_POINT('Ctrl Pts',(-1.81532118405566,-1.,-0.763132003836783));
#39125=CARTESIAN_POINT('Ctrl Pts',(-1.80938551463989,-1.,-0.762546129464036));
#39126=CARTESIAN_POINT('Ctrl Pts',(-1.80351583877334,-1.,-0.761915336443515));
#39127=CARTESIAN_POINT('Ctrl Pts',(-1.79768986997735,-1.,-0.761229695230359));
#39128=CARTESIAN_POINT('Ctrl Pts',(-1.79185815610802,-1.,-0.760469555880425));
#39129=CARTESIAN_POINT('Ctrl Pts',(-1.78596964884526,-1.,-0.759614401109868));
#39130=CARTESIAN_POINT('Ctrl Pts',(-1.77999411220912,-1.,-0.75865062667738));
#39131=CARTESIAN_POINT('Ctrl Pts',(-1.77394167108342,-1.,-0.757578264077238));
#39132=CARTESIAN_POINT('Ctrl Pts',(-1.76789396003141,-1.,-0.756421896028403));
#39133=CARTESIAN_POINT('Ctrl Pts',(-1.7619781724032,-1.,-0.755220979975262));
#39134=CARTESIAN_POINT('Ctrl Pts',(-1.75631083600175,-1.,-0.75400925402848));
#39135=CARTESIAN_POINT('Ctrl Pts',(-1.75095139468809,-1.,-0.752797683531377));
#39136=CARTESIAN_POINT('Ctrl Pts',(-1.74585086852298,-1.,-0.751555614163629));
#39137=CARTESIAN_POINT('Ctrl Pts',(-1.74080458266705,-1.,-0.75019343597954));
#39138=CARTESIAN_POINT('Ctrl Pts',(-1.73550351679848,-1.,-0.748582462954854));
#39139=CARTESIAN_POINT('Ctrl Pts',(-1.72958533647399,-1.,-0.746574710096436));
#39140=CARTESIAN_POINT('Ctrl Pts',(-1.7226822991693,-1.,-0.744021445433764));
#39141=CARTESIAN_POINT('Ctrl Pts',(-1.71447789751927,-1.,-0.740795162032087));
#39142=CARTESIAN_POINT('Ctrl Pts',(-1.70473309006121,-1.,-0.736799665724771));
#39143=CARTESIAN_POINT('Ctrl Pts',(-1.69326921975743,-1.,-0.731963238697195));
#39144=CARTESIAN_POINT('Ctrl Pts',(-1.67996158455503,-1.,-0.726235967997433));
#39145=CARTESIAN_POINT('Ctrl Pts',(-1.6647288055568,-1.,-0.719585433804282));
#39146=CARTESIAN_POINT('Ctrl Pts',(-1.64752408832016,-1.,-0.711993139355394));
#39147=CARTESIAN_POINT('Ctrl Pts',(-1.63216541664676,-1.,-0.705159151988319));
#39148=CARTESIAN_POINT('Ctrl Pts',(-1.61974673472612,-1.,-0.699605146405088));
#39149=CARTESIAN_POINT('Ctrl Pts',(-1.61106790958151,-1.,-0.695712097881194));
#39150=CARTESIAN_POINT('Ctrl Pts',(-1.60662857109684,-1.,-0.693717979106306));
#39151=CARTESIAN_POINT('',(-1.5055822144029,-1.,-0.892032620296855));
#39152=CARTESIAN_POINT('Origin',(0.,-1.,0.));
#39153=CARTESIAN_POINT('',(-1.81978687191668,-1.,-1.23627494547115));
#39154=CARTESIAN_POINT('Ctrl Pts',(-1.5055822144029,-1.,-0.892032620296855));
#39155=CARTESIAN_POINT('Ctrl Pts',(-1.50980486806688,-1.,-0.894452006964543));
#39156=CARTESIAN_POINT('Ctrl Pts',(-1.51805569590094,-1.,-0.899185047483511));
#39157=CARTESIAN_POINT('Ctrl Pts',(-1.52984849887993,-1.,-0.905967409625651));
#39158=CARTESIAN_POINT('Ctrl Pts',(-1.54440491149498,-1.,-0.914375919026456));
#39159=CARTESIAN_POINT('Ctrl Pts',(-1.56065988578893,-1.,-0.923832188944341));
#39160=CARTESIAN_POINT('Ctrl Pts',(-1.57499388382243,-1.,-0.932246680108685));
#39161=CARTESIAN_POINT('Ctrl Pts',(-1.58744937487176,-1.,-0.939646377893399));
#39162=CARTESIAN_POINT('Ctrl Pts',(-1.59810042043673,-1.,-0.946078063315257));
#39163=CARTESIAN_POINT('Ctrl Pts',(-1.60706069896936,-1.,-0.951613284356035));
#39164=CARTESIAN_POINT('Ctrl Pts',(-1.61449324337085,-1.,-0.956354422920671));
#39165=CARTESIAN_POINT('Ctrl Pts',(-1.62061638140221,-1.,-0.960438326101729));
#39166=CARTESIAN_POINT('Ctrl Pts',(-1.62571930670187,-1.,-0.964046107040536));
#39167=CARTESIAN_POINT('Ctrl Pts',(-1.63013849959461,-1.,-0.967387853230345));
#39168=CARTESIAN_POINT('Ctrl Pts',(-1.63420665729798,-1.,-0.970669715997509));
#39169=CARTESIAN_POINT('Ctrl Pts',(-1.63820952658144,-1.,-0.974066058287418));
#39170=CARTESIAN_POINT('Ctrl Pts',(-1.64233990826687,-1.,-0.977689794119416));
#39171=CARTESIAN_POINT('Ctrl Pts',(-1.64665139190656,-1.,-0.981562530939489));
#39172=CARTESIAN_POINT('Ctrl Pts',(-1.65110016612638,-1.,-0.985642622920821));
#39173=CARTESIAN_POINT('Ctrl Pts',(-1.65559044289699,-1.,-0.989855627854165));
#39174=CARTESIAN_POINT('Ctrl Pts',(-1.66001553809947,-1.,-0.994121836661306));
#39175=CARTESIAN_POINT('Ctrl Pts',(-1.66430758030376,-1.,-0.998389654952758));
#39176=CARTESIAN_POINT('Ctrl Pts',(-1.66846059277303,-1.,-1.00265091003727));
#39177=CARTESIAN_POINT('Ctrl Pts',(-1.67250335383293,-1.,-1.00692206696414));
#39178=CARTESIAN_POINT('Ctrl Pts',(-1.67648246776464,-1.,-1.01123236493511));
#39179=CARTESIAN_POINT('Ctrl Pts',(-1.68044289894798,-1.,-1.01561026162773));
#39180=CARTESIAN_POINT('Ctrl Pts',(-1.68440578021706,-1.,-1.02006795074201));
#39181=CARTESIAN_POINT('Ctrl Pts',(-1.68836910178447,-1.,-1.02460180535255));
#39182=CARTESIAN_POINT('Ctrl Pts',(-1.69231840863458,-1.,-1.02919977579147));
#39183=CARTESIAN_POINT('Ctrl Pts',(-1.69623414782771,-1.,-1.03384646003588));
#39184=CARTESIAN_POINT('Ctrl Pts',(-1.70010052930962,-1.,-1.03852922490789));
#39185=CARTESIAN_POINT('Ctrl Pts',(-1.70391338707982,-1.,-1.04324363334554));
#39186=CARTESIAN_POINT('Ctrl Pts',(-1.70767646263649,-1.,-1.04799085404995));
#39187=CARTESIAN_POINT('Ctrl Pts',(-1.71139783543989,-1.,-1.05277517202855));
#39188=CARTESIAN_POINT('Ctrl Pts',(-1.7150865442702,-1.,-1.05760163192479));
#39189=CARTESIAN_POINT('Ctrl Pts',(-1.71874858456904,-1.,-1.06247324680647));
#39190=CARTESIAN_POINT('Ctrl Pts',(-1.72238500928453,-1.,-1.06738966975462));
#39191=CARTESIAN_POINT('Ctrl Pts',(-1.72599406198488,-1.,-1.07234866990252));
#39192=CARTESIAN_POINT('Ctrl Pts',(-1.72957248977424,-1.,-1.0773470373727));
#39193=CARTESIAN_POINT('Ctrl Pts',(-1.73311705663407,-1.,-1.08238162784749));
#39194=CARTESIAN_POINT('Ctrl Pts',(-1.73662628326091,-1.,-1.08745056285427));
#39195=CARTESIAN_POINT('Ctrl Pts',(-1.74010053962247,-1.,-1.09255329056493));
#39196=CARTESIAN_POINT('Ctrl Pts',(-1.74354119236208,-1.,-1.09768999241225));
#39197=CARTESIAN_POINT('Ctrl Pts',(-1.74695004214923,-1.,-1.10286118991143));
#39198=CARTESIAN_POINT('Ctrl Pts',(-1.7503286607592,-1.,-1.10806728183007));
#39199=CARTESIAN_POINT('Ctrl Pts',(-1.7536777209463,-1.,-1.11330807582551));
#39200=CARTESIAN_POINT('Ctrl Pts',(-1.75699720772105,-1.,-1.11858293216763));
#39201=CARTESIAN_POINT('Ctrl Pts',(-1.76028671825096,-1.,-1.12389096855086));
#39202=CARTESIAN_POINT('Ctrl Pts',(-1.7635457196617,-1.,-1.12923123555075));
#39203=CARTESIAN_POINT('Ctrl Pts',(-1.76677384551862,-1.,-1.1346029180462));
#39204=CARTESIAN_POINT('Ctrl Pts',(-1.76997111386769,-1.,-1.14000548336975));
#39205=CARTESIAN_POINT('Ctrl Pts',(-1.77313777896194,-1.,-1.1454385822692));
#39206=CARTESIAN_POINT('Ctrl Pts',(-1.7762742255701,-1.,-1.15090197841515));
#39207=CARTESIAN_POINT('Ctrl Pts',(-1.77938085564275,-1.,-1.15639547194698));
#39208=CARTESIAN_POINT('Ctrl Pts',(-1.78245795881009,-1.,-1.16191881298499));
#39209=CARTESIAN_POINT('Ctrl Pts',(-1.78550566040443,-1.,-1.16747166312303));
#39210=CARTESIAN_POINT('Ctrl Pts',(-1.78852398877616,-1.,-1.17305363177328));
#39211=CARTESIAN_POINT('Ctrl Pts',(-1.79151291552689,-1.,-1.17866429440809));
#39212=CARTESIAN_POINT('Ctrl Pts',(-1.79447240321515,-1.,-1.18430321697432));
#39213=CARTESIAN_POINT('Ctrl Pts',(-1.79740245923478,-1.,-1.18996997934445));
#39214=CARTESIAN_POINT('Ctrl Pts',(-1.80030314369879,-1.,-1.19566418930242));
#39215=CARTESIAN_POINT('Ctrl Pts',(-1.80317454838603,-1.,-1.20138548938974));
#39216=CARTESIAN_POINT('Ctrl Pts',(-1.80601678480707,-1.,-1.20713356605475));
#39217=CARTESIAN_POINT('Ctrl Pts',(-1.80882996917129,-1.,-1.21290815708314));
#39218=CARTESIAN_POINT('Ctrl Pts',(-1.81161420806656,-1.,-1.21870906103557));
#39219=CARTESIAN_POINT('Ctrl Pts',(-1.81436959210434,-1.,-1.2245361330495));
#39220=CARTESIAN_POINT('Ctrl Pts',(-1.8165508718364,-1.,-1.2292186489137));
#39221=CARTESIAN_POINT('Ctrl Pts',(-1.81817389921279,-1.,-1.2327422452705));
#39222=CARTESIAN_POINT('Ctrl Pts',(-1.81925017193666,-1.,-1.23509651170476));
#39223=CARTESIAN_POINT('Ctrl Pts',(-1.81978687191668,-1.,-1.23627494547115));
#39224=CARTESIAN_POINT('',(-1.73811241238545,-1.,-1.34869019493419));
#39225=CARTESIAN_POINT('',(-1.81978687191668,-1.,-1.23627494547115));
#39226=CARTESIAN_POINT('',(-1.31362392696032,-1.,-1.15624053661742));
#39227=CARTESIAN_POINT('Ctrl Pts',(-1.73811241238545,-1.,-1.34869019493419));
#39228=CARTESIAN_POINT('Ctrl Pts',(-1.73682580585691,-1.,-1.34854391898045));
#39229=CARTESIAN_POINT('Ctrl Pts',(-1.73425417885907,-1.,-1.34824783112887));
#39230=CARTESIAN_POINT('Ctrl Pts',(-1.7304014965394,-1.,-1.34779309152035));
#39231=CARTESIAN_POINT('Ctrl Pts',(-1.72527410680674,-1.,-1.34716554819527));
#39232=CARTESIAN_POINT('Ctrl Pts',(-1.7188807715049,-1.,-1.34634568653227));
#39233=CARTESIAN_POINT('Ctrl Pts',(-1.71250340686822,-1.,-1.34549029589416));
#39234=CARTESIAN_POINT('Ctrl Pts',(-1.70614212266738,-1.,-1.34459924533831));
#39235=CARTESIAN_POINT('Ctrl Pts',(-1.69979707754427,-1.,-1.34367237124483));
#39236=CARTESIAN_POINT('Ctrl Pts',(-1.6934684849687,-1.,-1.34270948206319));
#39237=CARTESIAN_POINT('Ctrl Pts',(-1.68715660868764,-1.,-1.341710374848));
#39238=CARTESIAN_POINT('Ctrl Pts',(-1.68086176030362,-1.,-1.34067485185203));
#39239=CARTESIAN_POINT('Ctrl Pts',(-1.67458429426086,-1.,-1.3396027347034));
#39240=CARTESIAN_POINT('Ctrl Pts',(-1.66832460783989,-1.,-1.33849388654388));
#39241=CARTESIAN_POINT('Ctrl Pts',(-1.66208312541983,-1.,-1.33734820885262));
#39242=CARTESIAN_POINT('Ctrl Pts',(-1.65586025952593,-1.,-1.33616559745172));
#39243=CARTESIAN_POINT('Ctrl Pts',(-1.6496563728683,-1.,-1.33494590467993));
#39244=CARTESIAN_POINT('Ctrl Pts',(-1.6434717485603,-1.,-1.33368890676572));
#39245=CARTESIAN_POINT('Ctrl Pts',(-1.63730653475089,-1.,-1.33239425103724));
#39246=CARTESIAN_POINT('Ctrl Pts',(-1.63116079730923,-1.,-1.33106149345645));
#39247=CARTESIAN_POINT('Ctrl Pts',(-1.62503464209797,-1.,-1.3296901950568));
#39248=CARTESIAN_POINT('Ctrl Pts',(-1.61892832270724,-1.,-1.32828000610449));
#39249=CARTESIAN_POINT('Ctrl Pts',(-1.6128423401575,-1.,-1.32683074483356));
#39250=CARTESIAN_POINT('Ctrl Pts',(-1.60677758290954,-1.,-1.32534250785782));
#39251=CARTESIAN_POINT('Ctrl Pts',(-1.60073511858687,-1.,-1.32381550858256));
#39252=CARTESIAN_POINT('Ctrl Pts',(-1.59471591079403,-1.,-1.32224985747682));
#39253=CARTESIAN_POINT('Ctrl Pts',(-1.58872057258245,-1.,-1.32064537110892));
#39254=CARTESIAN_POINT('Ctrl Pts',(-1.58274907898834,-1.,-1.31900135021432));
#39255=CARTESIAN_POINT('Ctrl Pts',(-1.5768005650559,-1.,-1.31731642317187));
#39256=CARTESIAN_POINT('Ctrl Pts',(-1.57087397835723,-1.,-1.31558903860016));
#39257=CARTESIAN_POINT('Ctrl Pts',(-1.56496872402353,-1.,-1.31381795281002));
#39258=CARTESIAN_POINT('Ctrl Pts',(-1.55908521254821,-1.,-1.31200264341696));
#39259=CARTESIAN_POINT('Ctrl Pts',(-1.55322568759481,-1.,-1.31014393684222));
#39260=CARTESIAN_POINT('Ctrl Pts',(-1.54739413957185,-1.,-1.30824393907473));
#39261=CARTESIAN_POINT('Ctrl Pts',(-1.54159462645432,-1.,-1.30630475189556));
#39262=CARTESIAN_POINT('Ctrl Pts',(-1.53582981268977,-1.,-1.30432735639489));
#39263=CARTESIAN_POINT('Ctrl Pts',(-1.53009970283891,-1.,-1.30231064395568));
#39264=CARTESIAN_POINT('Ctrl Pts',(-1.52439957861062,-1.,-1.30024984366328));
#39265=CARTESIAN_POINT('Ctrl Pts',(-1.51872184912724,-1.,-1.29813791800747));
#39266=CARTESIAN_POINT('Ctrl Pts',(-1.51305994241402,-1.,-1.29596850710509));
#39267=CARTESIAN_POINT('Ctrl Pts',(-1.50741159078365,-1.,-1.29373841372842));
#39268=CARTESIAN_POINT('Ctrl Pts',(-1.50178230149776,-1.,-1.29145022885181));
#39269=CARTESIAN_POINT('Ctrl Pts',(-1.49618896881754,-1.,-1.28911506584254));
#39270=CARTESIAN_POINT('Ctrl Pts',(-1.4906522831278,-1.,-1.2867467611644));
#39271=CARTESIAN_POINT('Ctrl Pts',(-1.4851881711891,-1.,-1.28435533880201));
#39272=CARTESIAN_POINT('Ctrl Pts',(-1.47980070347095,-1.,-1.28194158939517));
#39273=CARTESIAN_POINT('Ctrl Pts',(-1.4744717526707,-1.,-1.2794891824849));
#39274=CARTESIAN_POINT('Ctrl Pts',(-1.46916035917133,-1.,-1.27696414831089));
#39275=CARTESIAN_POINT('Ctrl Pts',(-1.46382431332476,-1.,-1.27433119897822));
#39276=CARTESIAN_POINT('Ctrl Pts',(-1.45843906294697,-1.,-1.27156805265289));
#39277=CARTESIAN_POINT('Ctrl Pts',(-1.45301422764247,-1.,-1.2686778680489));
#39278=CARTESIAN_POINT('Ctrl Pts',(-1.44761985001662,-1.,-1.26570925118868));
#39279=CARTESIAN_POINT('Ctrl Pts',(-1.44236470511303,-1.,-1.26273903323859));
#39280=CARTESIAN_POINT('Ctrl Pts',(-1.43734919180848,-1.,-1.25983531012005));
#39281=CARTESIAN_POINT('Ctrl Pts',(-1.43262645609691,-1.,-1.25702687965755));
#39282=CARTESIAN_POINT('Ctrl Pts',(-1.42815938799387,-1.,-1.25426945222639));
#39283=CARTESIAN_POINT('Ctrl Pts',(-1.42378102115575,-1.,-1.2514145557001));
#39284=CARTESIAN_POINT('Ctrl Pts',(-1.41923722596025,-1.,-1.24824430986571));
#39285=CARTESIAN_POINT('Ctrl Pts',(-1.41422913175179,-1.,-1.24450600513056));
#39286=CARTESIAN_POINT('Ctrl Pts',(-1.40845295531283,-1.,-1.23994455029534));
#39287=CARTESIAN_POINT('Ctrl Pts',(-1.40164708206106,-1.,-1.23434087290423));
#39288=CARTESIAN_POINT('Ctrl Pts',(-1.39361389568796,-1.,-1.22752961899387));
#39289=CARTESIAN_POINT('Ctrl Pts',(-1.38420564527715,-1.,-1.21938737280852));
#39290=CARTESIAN_POINT('Ctrl Pts',(-1.37331915607905,-1.,-1.20982812925645));
#39291=CARTESIAN_POINT('Ctrl Pts',(-1.36088705043885,-1.,-1.1987959077932));
#39292=CARTESIAN_POINT('Ctrl Pts',(-1.34687054001093,-1.,-1.18625865667441));
#39293=CARTESIAN_POINT('Ctrl Pts',(-1.33437539347008,-1.,-1.17501305789857));
#39294=CARTESIAN_POINT('Ctrl Pts',(-1.32428080721772,-1.,-1.16589330093588));
#39295=CARTESIAN_POINT('Ctrl Pts',(-1.31722977216397,-1.,-1.15950888730809));
#39296=CARTESIAN_POINT('Ctrl Pts',(-1.31362392696032,-1.,-1.15624053661742));
#39297=CARTESIAN_POINT('',(-1.15624053661742,-1.,-1.31362392696033));
#39298=CARTESIAN_POINT('Origin',(0.,-1.,0.));
#39299=CARTESIAN_POINT('',(-1.34869019493419,-1.,-1.73811241238545));
#39300=CARTESIAN_POINT('Ctrl Pts',(-1.15624053661742,-1.,-1.31362392696033));
#39301=CARTESIAN_POINT('Ctrl Pts',(-1.15950888730433,-1.,-1.3172297721596));
#39302=CARTESIAN_POINT('Ctrl Pts',(-1.16589330092532,-1.,-1.32428080720544));
#39303=CARTESIAN_POINT('Ctrl Pts',(-1.17501305787994,-1.,-1.33437539344842));
#39304=CARTESIAN_POINT('Ctrl Pts',(-1.18625865664915,-1.,-1.34687053998157));
#39305=CARTESIAN_POINT('Ctrl Pts',(-1.1987959077656,-1.,-1.36088705040677));
#39306=CARTESIAN_POINT('Ctrl Pts',(-1.20982812923113,-1.,-1.37331915604962));
#39307=CARTESIAN_POINT('Ctrl Pts',(-1.21938737278853,-1.,-1.38420564525391));
#39308=CARTESIAN_POINT('Ctrl Pts',(-1.22752961898063,-1.,-1.39361389567257));
#39309=CARTESIAN_POINT('Ctrl Pts',(-1.23434087289768,-1.,-1.40164708205345));
#39310=CARTESIAN_POINT('Ctrl Pts',(-1.23994455029421,-1.,-1.40845295531151));
#39311=CARTESIAN_POINT('Ctrl Pts',(-1.24450600513278,-1.,-1.41422913175437));
#39312=CARTESIAN_POINT('Ctrl Pts',(-1.24824430986911,-1.,-1.41923722596421));
#39313=CARTESIAN_POINT('Ctrl Pts',(-1.25141455570299,-1.,-1.42378102115911));
#39314=CARTESIAN_POINT('Ctrl Pts',(-1.25426945222783,-1.,-1.42815938799555));
#39315=CARTESIAN_POINT('Ctrl Pts',(-1.25702687965744,-1.,-1.43262645609679));
#39316=CARTESIAN_POINT('Ctrl Pts',(-1.25983531011894,-1.,-1.43734919180719));
#39317=CARTESIAN_POINT('Ctrl Pts',(-1.26273903323723,-1.,-1.44236470511145));
#39318=CARTESIAN_POINT('Ctrl Pts',(-1.26570925118767,-1.,-1.44761985001544));
#39319=CARTESIAN_POINT('Ctrl Pts',(-1.26867786804854,-1.,-1.45301422764205));
#39320=CARTESIAN_POINT('Ctrl Pts',(-1.27156805265312,-1.,-1.45843906294725));
#39321=CARTESIAN_POINT('Ctrl Pts',(-1.27433119897877,-1.,-1.4638243133254));
#39322=CARTESIAN_POINT('Ctrl Pts',(-1.27696414831144,-1.,-1.46916035917197));
#39323=CARTESIAN_POINT('Ctrl Pts',(-1.27948918248524,-1.,-1.4744717526711));
#39324=CARTESIAN_POINT('Ctrl Pts',(-1.28194158939522,-1.,-1.47980070347102));
#39325=CARTESIAN_POINT('Ctrl Pts',(-1.28435533880184,-1.,-1.48518817118891));
#39326=CARTESIAN_POINT('Ctrl Pts',(-1.28674676116415,-1.,-1.4906522831275));
#39327=CARTESIAN_POINT('Ctrl Pts',(-1.28911506584232,-1.,-1.49618896881729));
#39328=CARTESIAN_POINT('Ctrl Pts',(-1.29145022885171,-1.,-1.50178230149764));
#39329=CARTESIAN_POINT('Ctrl Pts',(-1.29373841372843,-1.,-1.50741159078367));
#39330=CARTESIAN_POINT('Ctrl Pts',(-1.29596850710518,-1.,-1.51305994241412));
#39331=CARTESIAN_POINT('Ctrl Pts',(-1.29813791800757,-1.,-1.51872184912735));
#39332=CARTESIAN_POINT('Ctrl Pts',(-1.30024984366334,-1.,-1.5243995786107));
#39333=CARTESIAN_POINT('Ctrl Pts',(-1.3023106439557,-1.,-1.53009970283893));
#39334=CARTESIAN_POINT('Ctrl Pts',(-1.30432735639487,-1.,-1.53582981268976));
#39335=CARTESIAN_POINT('Ctrl Pts',(-1.30630475189553,-1.,-1.54159462645428));
#39336=CARTESIAN_POINT('Ctrl Pts',(-1.30824393907471,-1.,-1.54739413957183));
#39337=CARTESIAN_POINT('Ctrl Pts',(-1.31014393684221,-1.,-1.55322568759481));
#39338=CARTESIAN_POINT('Ctrl Pts',(-1.31200264341696,-1.,-1.55908521254822));
#39339=CARTESIAN_POINT('Ctrl Pts',(-1.31381795281002,-1.,-1.56496872402352));
#39340=CARTESIAN_POINT('Ctrl Pts',(-1.31558903860015,-1.,-1.57087397835721));
#39341=CARTESIAN_POINT('Ctrl Pts',(-1.31731642317183,-1.,-1.57680056505585));
#39342=CARTESIAN_POINT('Ctrl Pts',(-1.31900135021428,-1.,-1.58274907898829));
#39343=CARTESIAN_POINT('Ctrl Pts',(-1.32064537110891,-1.,-1.58872057258244));
#39344=CARTESIAN_POINT('Ctrl Pts',(-1.32224985747686,-1.,-1.59471591079408));
#39345=CARTESIAN_POINT('Ctrl Pts',(-1.32381550858266,-1.,-1.600735118587));
#39346=CARTESIAN_POINT('Ctrl Pts',(-1.32534250785794,-1.,-1.6067775829097));
#39347=CARTESIAN_POINT('Ctrl Pts',(-1.32683074483365,-1.,-1.61284234015762));
#39348=CARTESIAN_POINT('Ctrl Pts',(-1.32828000610448,-1.,-1.61892832270723));
#39349=CARTESIAN_POINT('Ctrl Pts',(-1.32969019505665,-1.,-1.62503464209777));
#39350=CARTESIAN_POINT('Ctrl Pts',(-1.33106149345618,-1.,-1.63116079730887));
#39351=CARTESIAN_POINT('Ctrl Pts',(-1.33239425103694,-1.,-1.6373065347505));
#39352=CARTESIAN_POINT('Ctrl Pts',(-1.33368890676554,-1.,-1.64347174856007));
#39353=CARTESIAN_POINT('Ctrl Pts',(-1.33494590468003,-1.,-1.64965637286843));
#39354=CARTESIAN_POINT('Ctrl Pts',(-1.33616559745217,-1.,-1.65586025952651));
#39355=CARTESIAN_POINT('Ctrl Pts',(-1.33734820885331,-1.,-1.66208312542073));
#39356=CARTESIAN_POINT('Ctrl Pts',(-1.33849388654458,-1.,-1.66832460784078));
#39357=CARTESIAN_POINT('Ctrl Pts',(-1.33960273470372,-1.,-1.67458429426126));
#39358=CARTESIAN_POINT('Ctrl Pts',(-1.3406748518516,-1.,-1.68086176030308));
#39359=CARTESIAN_POINT('Ctrl Pts',(-1.34171037484673,-1.,-1.68715660868602));
#39360=CARTESIAN_POINT('Ctrl Pts',(-1.34270948206139,-1.,-1.6934684849664));
#39361=CARTESIAN_POINT('Ctrl Pts',(-1.34367237124322,-1.,-1.69979707754221));
#39362=CARTESIAN_POINT('Ctrl Pts',(-1.34459924533783,-1.,-1.70614212266676));
#39363=CARTESIAN_POINT('Ctrl Pts',(-1.34549029589563,-1.,-1.71250340687011));
#39364=CARTESIAN_POINT('Ctrl Pts',(-1.34634568653586,-1.,-1.7188807715095));
#39365=CARTESIAN_POINT('Ctrl Pts',(-1.34716554820013,-1.,-1.72527410681298));
#39366=CARTESIAN_POINT('Ctrl Pts',(-1.3477930915247,-1.,-1.73040149654497));
#39367=CARTESIAN_POINT('Ctrl Pts',(-1.34824783113158,-1.,-1.73425417886255));
#39368=CARTESIAN_POINT('Ctrl Pts',(-1.34854391898145,-1.,-1.73682580585819));
#39369=CARTESIAN_POINT('Ctrl Pts',(-1.34869019493419,-1.,-1.73811241238545));
#39370=CARTESIAN_POINT('',(-1.23627494547115,-1.,-1.81978687191668));
#39371=CARTESIAN_POINT('',(-1.34869019493419,-1.,-1.73811241238545));
#39372=CARTESIAN_POINT('',(-0.892032620296855,-1.,-1.5055822144029));
#39373=CARTESIAN_POINT('Ctrl Pts',(-1.23627494547115,-1.,-1.81978687191668));
#39374=CARTESIAN_POINT('Ctrl Pts',(-1.23509651170384,-1.,-1.81925017193531));
#39375=CARTESIAN_POINT('Ctrl Pts',(-1.23274224526804,-1.,-1.81817389920914));
#39376=CARTESIAN_POINT('Ctrl Pts',(-1.22921864890975,-1.,-1.81655087183054));
#39377=CARTESIAN_POINT('Ctrl Pts',(-1.22453613304507,-1.,-1.81436959209778));
#39378=CARTESIAN_POINT('Ctrl Pts',(-1.2187090610323,-1.,-1.81161420806172));
#39379=CARTESIAN_POINT('Ctrl Pts',(-1.2129081570818,-1.,-1.80882996916931));
#39380=CARTESIAN_POINT('Ctrl Pts',(-1.20713356605519,-1.,-1.80601678480772));
#39381=CARTESIAN_POINT('Ctrl Pts',(-1.2013854893912,-1.,-1.8031745483882));
#39382=CARTESIAN_POINT('Ctrl Pts',(-1.19566418930405,-1.,-1.80030314370121));
#39383=CARTESIAN_POINT('Ctrl Pts',(-1.1899699793456,-1.,-1.79740245923649));
#39384=CARTESIAN_POINT('Ctrl Pts',(-1.18430321697471,-1.,-1.79447240321572));
#39385=CARTESIAN_POINT('Ctrl Pts',(-1.17866429440781,-1.,-1.79151291552646));
#39386=CARTESIAN_POINT('Ctrl Pts',(-1.17305363177265,-1.,-1.78852398877523));
#39387=CARTESIAN_POINT('Ctrl Pts',(-1.16747166312239,-1.,-1.78550566040349));
#39388=CARTESIAN_POINT('Ctrl Pts',(-1.16191881298458,-1.,-1.78245795880949));
#39389=CARTESIAN_POINT('Ctrl Pts',(-1.15639547194689,-1.,-1.77938085564261));
#39390=CARTESIAN_POINT('Ctrl Pts',(-1.15090197841531,-1.,-1.77627422557034));
#39391=CARTESIAN_POINT('Ctrl Pts',(-1.14543858226948,-1.,-1.77313777896234));
#39392=CARTESIAN_POINT('Ctrl Pts',(-1.14000548337,-1.,-1.76997111386806));
#39393=CARTESIAN_POINT('Ctrl Pts',(-1.13460291804635,-1.,-1.76677384551883));
#39394=CARTESIAN_POINT('Ctrl Pts',(-1.12923123555076,-1.,-1.76354571966171));
#39395=CARTESIAN_POINT('Ctrl Pts',(-1.12389096855078,-1.,-1.76028671825084));
#39396=CARTESIAN_POINT('Ctrl Pts',(-1.11858293216752,-1.,-1.75699720772089));
#39397=CARTESIAN_POINT('Ctrl Pts',(-1.11330807582542,-1.,-1.75367772094617));
#39398=CARTESIAN_POINT('Ctrl Pts',(-1.10806728183003,-1.,-1.75032866075914));
#39399=CARTESIAN_POINT('Ctrl Pts',(-1.10286118991144,-1.,-1.74695004214924));
#39400=CARTESIAN_POINT('Ctrl Pts',(-1.09768999241229,-1.,-1.74354119236212));
#39401=CARTESIAN_POINT('Ctrl Pts',(-1.09255329056496,-1.,-1.74010053962252));
#39402=CARTESIAN_POINT('Ctrl Pts',(-1.08745056285429,-1.,-1.73662628326093));
#39403=CARTESIAN_POINT('Ctrl Pts',(-1.08238162784749,-1.,-1.73311705663407));
#39404=CARTESIAN_POINT('Ctrl Pts',(-1.0773470373727,-1.,-1.72957248977424));
#39405=CARTESIAN_POINT('Ctrl Pts',(-1.07234866990252,-1.,-1.72599406198489));
#39406=CARTESIAN_POINT('Ctrl Pts',(-1.06738966975463,-1.,-1.72238500928456));
#39407=CARTESIAN_POINT('Ctrl Pts',(-1.0624732468065,-1.,-1.71874858456908));
#39408=CARTESIAN_POINT('Ctrl Pts',(-1.05760163192481,-1.,-1.71508654427022));
#39409=CARTESIAN_POINT('Ctrl Pts',(-1.05277517202854,-1.,-1.71139783543986));
#39410=CARTESIAN_POINT('Ctrl Pts',(-1.0479908540499,-1.,-1.70767646263641));
#39411=CARTESIAN_POINT('Ctrl Pts',(-1.04324363334546,-1.,-1.70391338707969));
#39412=CARTESIAN_POINT('Ctrl Pts',(-1.03852922490782,-1.,-1.70010052930951));
#39413=CARTESIAN_POINT('Ctrl Pts',(-1.03384646003587,-1.,-1.69623414782769));
#39414=CARTESIAN_POINT('Ctrl Pts',(-1.02919977579155,-1.,-1.69231840863471));
#39415=CARTESIAN_POINT('Ctrl Pts',(-1.02460180535272,-1.,-1.68836910178475));
#39416=CARTESIAN_POINT('Ctrl Pts',(-1.02006795074222,-1.,-1.68440578021739));
#39417=CARTESIAN_POINT('Ctrl Pts',(-1.01561026162787,-1.,-1.6804428989482));
#39418=CARTESIAN_POINT('Ctrl Pts',(-1.01123236493507,-1.,-1.67648246776457));
#39419=CARTESIAN_POINT('Ctrl Pts',(-1.00692206696387,-1.,-1.67250335383248));
#39420=CARTESIAN_POINT('Ctrl Pts',(-1.00265091003682,-1.,-1.66846059277231));
#39421=CARTESIAN_POINT('Ctrl Pts',(-0.998389654952317,-1.,-1.66430758030304));
#39422=CARTESIAN_POINT('Ctrl Pts',(-0.994121836661116,-1.,-1.66001553809916));
#39423=CARTESIAN_POINT('Ctrl Pts',(-0.98985562785445,-1.,-1.65559044289746));
#39424=CARTESIAN_POINT('Ctrl Pts',(-0.985642622921626,-1.,-1.6511001661277));
#39425=CARTESIAN_POINT('Ctrl Pts',(-0.981562530940574,-1.,-1.64665139190834));
#39426=CARTESIAN_POINT('Ctrl Pts',(-0.977689794120297,-1.,-1.64233990826831));
#39427=CARTESIAN_POINT('Ctrl Pts',(-0.974066058287501,-1.,-1.63820952658157));
#39428=CARTESIAN_POINT('Ctrl Pts',(-0.970669715996356,-1.,-1.63420665729609));
#39429=CARTESIAN_POINT('Ctrl Pts',(-0.967387853228041,-1.,-1.63013849959083));
#39430=CARTESIAN_POINT('Ctrl Pts',(-0.964046107037821,-1.,-1.6257193066974));
#39431=CARTESIAN_POINT('Ctrl Pts',(-0.960438326099958,-1.,-1.62061638139929));
#39432=CARTESIAN_POINT('Ctrl Pts',(-0.956354422921573,-1.,-1.61449324337233));
#39433=CARTESIAN_POINT('Ctrl Pts',(-0.951613284361248,-1.,-1.60706069897794));
#39434=CARTESIAN_POINT('Ctrl Pts',(-0.946078063325796,-1.,-1.59810042045408));
#39435=CARTESIAN_POINT('Ctrl Pts',(-0.939646377909319,-1.,-1.58744937489796));
#39436=CARTESIAN_POINT('Ctrl Pts',(-0.932246680128849,-1.,-1.57499388385561));
#39437=CARTESIAN_POINT('Ctrl Pts',(-0.923832188966322,-1.,-1.56065988582509));
#39438=CARTESIAN_POINT('Ctrl Pts',(-0.91437591904658,-1.,-1.54440491152808));
#39439=CARTESIAN_POINT('Ctrl Pts',(-0.905967409640499,-1.,-1.52984849890434));
#39440=CARTESIAN_POINT('Ctrl Pts',(-0.89918504749193,-1.,-1.51805569591479));
#39441=CARTESIAN_POINT('Ctrl Pts',(-0.894452006967538,-1.,-1.50980486807181));
#39442=CARTESIAN_POINT('Ctrl Pts',(-0.892032620296855,-1.,-1.5055822144029));
#39443=CARTESIAN_POINT('',(-0.693717979106305,-1.,-1.60662857109684));
#39444=CARTESIAN_POINT('Origin',(0.,-1.,0.));
#39445=CARTESIAN_POINT('',(-0.745574324794401,-1.,-2.0698113262342));
#39446=CARTESIAN_POINT('Ctrl Pts',(-0.693717979106305,-1.,-1.60662857109684));
#39447=CARTESIAN_POINT('Ctrl Pts',(-0.69571209787897,-1.,-1.61106790957619));
#39448=CARTESIAN_POINT('Ctrl Pts',(-0.699605146398837,-1.,-1.61974673471117));
#39449=CARTESIAN_POINT('Ctrl Pts',(-0.705159151977294,-1.,-1.6321654166204));
#39450=CARTESIAN_POINT('Ctrl Pts',(-0.711993139340447,-1.,-1.64752408828442));
#39451=CARTESIAN_POINT('Ctrl Pts',(-0.71958543378795,-1.,-1.66472880551777));
#39452=CARTESIAN_POINT('Ctrl Pts',(-0.726235967982445,-1.,-1.67996158451922));
#39453=CARTESIAN_POINT('Ctrl Pts',(-0.731963238685357,-1.,-1.69326921972915));
#39454=CARTESIAN_POINT('Ctrl Pts',(-0.736799665716932,-1.,-1.70473309004249));
#39455=CARTESIAN_POINT('Ctrl Pts',(-0.74079516202821,-1.,-1.71447789751001));
#39456=CARTESIAN_POINT('Ctrl Pts',(-0.744021445433093,-1.,-1.72268229916769));
#39457=CARTESIAN_POINT('Ctrl Pts',(-0.746574710097752,-1.,-1.72958533647714));
#39458=CARTESIAN_POINT('Ctrl Pts',(-0.74858246295687,-1.,-1.7355035168033));
#39459=CARTESIAN_POINT('Ctrl Pts',(-0.750193435981249,-1.,-1.74080458267114));
#39460=CARTESIAN_POINT('Ctrl Pts',(-0.751555614164482,-1.,-1.74585086852502));
#39461=CARTESIAN_POINT('Ctrl Pts',(-0.752797683531314,-1.,-1.75095139468794));
#39462=CARTESIAN_POINT('Ctrl Pts',(-0.754009254027829,-1.,-1.75631083600019));
#39463=CARTESIAN_POINT('Ctrl Pts',(-0.755220979974461,-1.,-1.76197817240128));
#39464=CARTESIAN_POINT('Ctrl Pts',(-0.75642189602781,-1.,-1.76789396002998));
#39465=CARTESIAN_POINT('Ctrl Pts',(-0.757578264077029,-1.,-1.77394167108292));
#39466=CARTESIAN_POINT('Ctrl Pts',(-0.758650626677518,-1.,-1.77999411220945));
#39467=CARTESIAN_POINT('Ctrl Pts',(-0.759614401110189,-1.,-1.78596964884604));
#39468=CARTESIAN_POINT('Ctrl Pts',(-0.760469555880749,-1.,-1.7918581561088));
#39469=CARTESIAN_POINT('Ctrl Pts',(-0.761229695230558,-1.,-1.79768986997783));
#39470=CARTESIAN_POINT('Ctrl Pts',(-0.761915336443547,-1.,-1.80351583877342));
#39471=CARTESIAN_POINT('Ctrl Pts',(-0.762546129463938,-1.,-1.80938551463965));
#39472=CARTESIAN_POINT('Ctrl Pts',(-0.763132003836634,-1.,-1.8153211840553));
#39473=CARTESIAN_POINT('Ctrl Pts',(-0.763673465462726,-1.,-1.82131873145266));
#39474=CARTESIAN_POINT('Ctrl Pts',(-0.764165902605995,-1.,-1.82735991200065));
#39475=CARTESIAN_POINT('Ctrl Pts',(-0.764602549687853,-1.,-1.83342077227142));
#39476=CARTESIAN_POINT('Ctrl Pts',(-0.764978057881737,-1.,-1.83948181064835));
#39477=CARTESIAN_POINT('Ctrl Pts',(-0.765291664862029,-1.,-1.84553698875924));
#39478=CARTESIAN_POINT('Ctrl Pts',(-0.765545710619062,-1.,-1.85158945130063));
#39479=CARTESIAN_POINT('Ctrl Pts',(-0.765744212909318,-1.,-1.85764741390394));
#39480=CARTESIAN_POINT('Ctrl Pts',(-0.765891519092547,-1.,-1.86372027063312));
#39481=CARTESIAN_POINT('Ctrl Pts',(-0.765990708546091,-1.,-1.86981398314341));
#39482=CARTESIAN_POINT('Ctrl Pts',(-0.766042837036744,-1.,-1.87592888967883));
#39483=CARTESIAN_POINT('Ctrl Pts',(-0.766047794851865,-1.,-1.88206215302561));
#39484=CARTESIAN_POINT('Ctrl Pts',(-0.766004837062091,-1.,-1.88820926433409));
#39485=CARTESIAN_POINT('Ctrl Pts',(-0.765913193856978,-1.,-1.89436577771388));
#39486=CARTESIAN_POINT('Ctrl Pts',(-0.765772772593386,-1.,-1.90052930393596));
#39487=CARTESIAN_POINT('Ctrl Pts',(-0.765584196937919,-1.,-1.90669961402356));
#39488=CARTESIAN_POINT('Ctrl Pts',(-0.765348465884722,-1.,-1.91287765805169));
#39489=CARTESIAN_POINT('Ctrl Pts',(-0.765066729667088,-1.,-1.91906491634196));
#39490=CARTESIAN_POINT('Ctrl Pts',(-0.764740025488211,-1.,-1.92526263537048));
#39491=CARTESIAN_POINT('Ctrl Pts',(-0.764369010673941,-1.,-1.93147105496382));
#39492=CARTESIAN_POINT('Ctrl Pts',(-0.763954049121458,-1.,-1.93768964875886));
#39493=CARTESIAN_POINT('Ctrl Pts',(-0.763495333538629,-1.,-1.9439174661764));
#39494=CARTESIAN_POINT('Ctrl Pts',(-0.762992990878769,-1.,-1.95015342590024));
#39495=CARTESIAN_POINT('Ctrl Pts',(-0.762447203806179,-1.,-1.95639665309869));
#39496=CARTESIAN_POINT('Ctrl Pts',(-0.761858300014423,-1.,-1.96264672744186));
#39497=CARTESIAN_POINT('Ctrl Pts',(-0.76122669048382,-1.,-1.96890351582499));
#39498=CARTESIAN_POINT('Ctrl Pts',(-0.760552825409757,-1.,-1.97516705321494));
#39499=CARTESIAN_POINT('Ctrl Pts',(-0.75983714745219,-1.,-1.98143741418172));
#39500=CARTESIAN_POINT('Ctrl Pts',(-0.759080037802488,-1.,-1.98771456680874));
#39501=CARTESIAN_POINT('Ctrl Pts',(-0.758281796766761,-1.,-1.99399831098817));
#39502=CARTESIAN_POINT('Ctrl Pts',(-0.757442676862724,-1.,-2.00028834739178));
#39503=CARTESIAN_POINT('Ctrl Pts',(-0.75656290464667,-1.,-2.0065843158773));
#39504=CARTESIAN_POINT('Ctrl Pts',(-0.755642704957865,-1.,-2.01288584328084));
#39505=CARTESIAN_POINT('Ctrl Pts',(-0.754682330722816,-1.,-2.01919259405809));
#39506=CARTESIAN_POINT('Ctrl Pts',(-0.753682061112768,-1.,-2.02550428623313));
#39507=CARTESIAN_POINT('Ctrl Pts',(-0.752642180487211,-1.,-2.03182068456221));
#39508=CARTESIAN_POINT('Ctrl Pts',(-0.751562963361115,-1.,-2.03814160092099));
#39509=CARTESIAN_POINT('Ctrl Pts',(-0.750444657875576,-1.,-2.04446689147979));
#39510=CARTESIAN_POINT('Ctrl Pts',(-0.749287468665046,-1.,-2.05079645592154));
#39511=CARTESIAN_POINT('Ctrl Pts',(-0.748091554183802,-1.,-2.05713023031006));
#39512=CARTESIAN_POINT('Ctrl Pts',(-0.747103932787919,-1.,-2.06220058927826));
#39513=CARTESIAN_POINT('Ctrl Pts',(-0.7463458715442,-1.,-2.06600523016815));
#39514=CARTESIAN_POINT('Ctrl Pts',(-0.745832791378367,-1.,-2.06854248895728));
#39515=CARTESIAN_POINT('Ctrl Pts',(-0.745574324794401,-1.,-2.0698113262342));
#39516=CARTESIAN_POINT('',(-0.61342227326009,-1.,-2.11275013067528));
#39517=CARTESIAN_POINT('',(-0.745574324794401,-1.,-2.0698113262342));
#39518=CARTESIAN_POINT('',(-0.383122945602004,-1.,-1.7075470150345));
#39519=CARTESIAN_POINT('Ctrl Pts',(-0.61342227326009,-1.,-2.11275013067528));
#39520=CARTESIAN_POINT('Ctrl Pts',(-0.6124673655618,-1.,-2.11187554259986));
#39521=CARTESIAN_POINT('Ctrl Pts',(-0.610560911689899,-1.,-2.11012443807238));
#39522=CARTESIAN_POINT('Ctrl Pts',(-0.607711315454876,-1.,-2.1074919961518));
#39523=CARTESIAN_POINT('Ctrl Pts',(-0.60393203073603,-1.,-2.10397049886949));
#39524=CARTESIAN_POINT('Ctrl Pts',(-0.599241616420533,-1.,-2.0995493086477));
#39525=CARTESIAN_POINT('Ctrl Pts',(-0.594585006052162,-1.,-2.0951087622027));
#39526=CARTESIAN_POINT('Ctrl Pts',(-0.589962365403406,-1.,-2.09064881812129));
#39527=CARTESIAN_POINT('Ctrl Pts',(-0.585373918991617,-1.,-2.08616943727951));
#39528=CARTESIAN_POINT('Ctrl Pts',(-0.580819952108063,-1.,-2.08167059018418));
#39529=CARTESIAN_POINT('Ctrl Pts',(-0.576300797416844,-1.,-2.07715226767559));
#39530=CARTESIAN_POINT('Ctrl Pts',(-0.571816823242603,-1.,-2.07261449292824));
#39531=CARTESIAN_POINT('Ctrl Pts',(-0.567368421181087,-1.,-2.06805732997334));
#39532=CARTESIAN_POINT('Ctrl Pts',(-0.562955993082261,-1.,-2.06348090160589));
#39533=CARTESIAN_POINT('Ctrl Pts',(-0.558579940185151,-1.,-2.05888537756462));
#39534=CARTESIAN_POINT('Ctrl Pts',(-0.554240657463906,-1.,-2.05427091604413));
#39535=CARTESIAN_POINT('Ctrl Pts',(-0.549938525150295,-1.,-2.04963761077958));
#39536=CARTESIAN_POINT('Ctrl Pts',(-0.54567390381743,-1.,-2.04498544714588));
#39537=CARTESIAN_POINT('Ctrl Pts',(-0.541447120615659,-1.,-2.04031422690527));
#39538=CARTESIAN_POINT('Ctrl Pts',(-0.537258489833262,-1.,-2.03562362954037));
#39539=CARTESIAN_POINT('Ctrl Pts',(-0.533108355132977,-1.,-2.03091336214426));
#39540=CARTESIAN_POINT('Ctrl Pts',(-0.528997127241914,-1.,-2.0261832908329));
#39541=CARTESIAN_POINT('Ctrl Pts',(-0.524925318333476,-1.,-2.02143356304698));
#39542=CARTESIAN_POINT('Ctrl Pts',(-0.52089359039937,-1.,-2.01666477917286));
#39543=CARTESIAN_POINT('Ctrl Pts',(-0.516902681728687,-1.,-2.01187773939242));
#39544=CARTESIAN_POINT('Ctrl Pts',(-0.512953306961792,-1.,-2.00707309946949));
#39545=CARTESIAN_POINT('Ctrl Pts',(-0.509046069886157,-1.,-2.00225107134734));
#39546=CARTESIAN_POINT('Ctrl Pts',(-0.505181361323026,-1.,-1.99741107463572));
#39547=CARTESIAN_POINT('Ctrl Pts',(-0.501359287727146,-1.,-1.99255149126155));
#39548=CARTESIAN_POINT('Ctrl Pts',(-0.497579909545574,-1.,-1.98767044752932));
#39549=CARTESIAN_POINT('Ctrl Pts',(-0.493843476541495,-1.,-1.98276658761821));
#39550=CARTESIAN_POINT('Ctrl Pts',(-0.490150627860952,-1.,-1.97783973019229));
#39551=CARTESIAN_POINT('Ctrl Pts',(-0.486502692907659,-1.,-1.97289186263272));
#39552=CARTESIAN_POINT('Ctrl Pts',(-0.482901662120691,-1.,-1.96792703422362));
#39553=CARTESIAN_POINT('Ctrl Pts',(-0.479349583074855,-1.,-1.96294933055943));
#39554=CARTESIAN_POINT('Ctrl Pts',(-0.475848034683176,-1.,-1.95796111148177));
#39555=CARTESIAN_POINT('Ctrl Pts',(-0.472397672264072,-1.,-1.95296148278133));
#39556=CARTESIAN_POINT('Ctrl Pts',(-0.468997482913135,-1.,-1.94794381136514));
#39557=CARTESIAN_POINT('Ctrl Pts',(-0.46564546202603,-1.,-1.9428979419619));
#39558=CARTESIAN_POINT('Ctrl Pts',(-0.462340031009056,-1.,-1.93781486640821));
#39559=CARTESIAN_POINT('Ctrl Pts',(-0.459081234547926,-1.,-1.93269066517934));
#39560=CARTESIAN_POINT('Ctrl Pts',(-0.455872005174371,-1.,-1.92753067150476));
#39561=CARTESIAN_POINT('Ctrl Pts',(-0.452719478359432,-1.,-1.92235380648502));
#39562=CARTESIAN_POINT('Ctrl Pts',(-0.449632260106662,-1.,-1.91718342555755));
#39563=CARTESIAN_POINT('Ctrl Pts',(-0.446617343485711,-1.,-1.9120369998112));
#39564=CARTESIAN_POINT('Ctrl Pts',(-0.443677556849151,-1.,-1.90691756144898));
#39565=CARTESIAN_POINT('Ctrl Pts',(-0.440807833704038,-1.,-1.90180124389086));
#39566=CARTESIAN_POINT('Ctrl Pts',(-0.437995003948244,-1.,-1.89663648956466));
#39567=CARTESIAN_POINT('Ctrl Pts',(-0.435225660963383,-1.,-1.89136993975504));
#39568=CARTESIAN_POINT('Ctrl Pts',(-0.432493038548748,-1.,-1.88596913666793));
#39569=CARTESIAN_POINT('Ctrl Pts',(-0.429803062482344,-1.,-1.88044229001832));
#39570=CARTESIAN_POINT('Ctrl Pts',(-0.427183828519102,-1.,-1.87486989291484));
#39571=CARTESIAN_POINT('Ctrl Pts',(-0.424678177291359,-1.,-1.86937803944323));
#39572=CARTESIAN_POINT('Ctrl Pts',(-0.422327307418275,-1.,-1.86408083334028));
#39573=CARTESIAN_POINT('Ctrl Pts',(-0.420157287975619,-1.,-1.85903281096686));
#39574=CARTESIAN_POINT('Ctrl Pts',(-0.418164129143534,-1.,-1.85417632856234));
#39575=CARTESIAN_POINT('Ctrl Pts',(-0.416300022038864,-1.,-1.84929312929882));
#39576=CARTESIAN_POINT('Ctrl Pts',(-0.41448743825434,-1.,-1.8440575707371));
#39577=CARTESIAN_POINT('Ctrl Pts',(-0.412633125322162,-1.,-1.83808953475839));
#39578=CARTESIAN_POINT('Ctrl Pts',(-0.410641256301675,-1.,-1.83100408895216));
#39579=CARTESIAN_POINT('Ctrl Pts',(-0.408428948108533,-1.,-1.8224702267854));
#39580=CARTESIAN_POINT('Ctrl Pts',(-0.405933518411838,-1.,-1.81223801813988));
#39581=CARTESIAN_POINT('Ctrl Pts',(-0.403107976170441,-1.,-1.80012077176221));
#39582=CARTESIAN_POINT('Ctrl Pts',(-0.39991940378308,-1.,-1.78598826347533));
#39583=CARTESIAN_POINT('Ctrl Pts',(-0.39634619612042,-1.,-1.7697556004756));
#39584=CARTESIAN_POINT('Ctrl Pts',(-0.392375812294307,-1.,-1.75137405313962));
#39585=CARTESIAN_POINT('Ctrl Pts',(-0.388877023509191,-1.,-1.7349317097561));
#39586=CARTESIAN_POINT('Ctrl Pts',(-0.38607079032701,-1.,-1.72162022246158));
#39587=CARTESIAN_POINT('Ctrl Pts',(-0.384119047315542,-1.,-1.71231062891958));
#39588=CARTESIAN_POINT('Ctrl Pts',(-0.383122945602004,-1.,-1.7075470150345));
#39589=CARTESIAN_POINT('',(-0.163289472382896,-1.,-1.74236521665491));
#39590=CARTESIAN_POINT('Origin',(0.,-1.,0.));
#39591=CARTESIAN_POINT('',(-0.0694764450219581,-1.,-2.19890268624765));
#39592=CARTESIAN_POINT('Ctrl Pts',(-0.163289472382896,-1.,-1.74236521665491));
#39593=CARTESIAN_POINT('Ctrl Pts',(-0.163814161002002,-1.,-1.7472034950333));
#39594=CARTESIAN_POINT('Ctrl Pts',(-0.164834765707158,-1.,-1.75666056638427));
#39595=CARTESIAN_POINT('Ctrl Pts',(-0.1662793551464,-1.,-1.77018771684844));
#39596=CARTESIAN_POINT('Ctrl Pts',(-0.168032772805197,-1.,-1.7869064998507));
#39597=CARTESIAN_POINT('Ctrl Pts',(-0.169936923904608,-1.,-1.80561530629706));
#39598=CARTESIAN_POINT('Ctrl Pts',(-0.171554770204119,-1.,-1.82215766811545));
#39599=CARTESIAN_POINT('Ctrl Pts',(-0.1728894428919,-1.,-1.83658380527692));
#39600=CARTESIAN_POINT('Ctrl Pts',(-0.173946627587731,-1.,-1.8489811319852));
#39601=CARTESIAN_POINT('Ctrl Pts',(-0.17473525927603,-1.,-1.85948367088837));
#39602=CARTESIAN_POINT('Ctrl Pts',(-0.175268337590758,-1.,-1.86828349694799));
#39603=CARTESIAN_POINT('Ctrl Pts',(-0.175563480746485,-1.,-1.87563767773588));
#39604=CARTESIAN_POINT('Ctrl Pts',(-0.175644148889699,-1.,-1.88188663145367));
#39605=CARTESIAN_POINT('Ctrl Pts',(-0.175538155840648,-1.,-1.88742606273259));
#39606=CARTESIAN_POINT('Ctrl Pts',(-0.175274276190844,-1.,-1.892646301985));
#39607=CARTESIAN_POINT('Ctrl Pts',(-0.174879405091263,-1.,-1.89788101117132));
#39608=CARTESIAN_POINT('Ctrl Pts',(-0.174375518661085,-1.,-1.90335253862834));
#39609=CARTESIAN_POINT('Ctrl Pts',(-0.173776635257817,-1.,-1.90911693975267));
#39610=CARTESIAN_POINT('Ctrl Pts',(-0.173090695383496,-1.,-1.91511429159527));
#39611=CARTESIAN_POINT('Ctrl Pts',(-0.172321621259514,-1.,-1.9212233439798));
#39612=CARTESIAN_POINT('Ctrl Pts',(-0.171471191532988,-1.,-1.92731093582036));
#39613=CARTESIAN_POINT('Ctrl Pts',(-0.170541253116202,-1.,-1.93329183155539));
#39614=CARTESIAN_POINT('Ctrl Pts',(-0.169534904817491,-1.,-1.93915639211581));
#39615=CARTESIAN_POINT('Ctrl Pts',(-0.168455741607556,-1.,-1.94493757756931));
#39616=CARTESIAN_POINT('Ctrl Pts',(-0.167307501784475,-1.,-1.95069027794294));
#39617=CARTESIAN_POINT('Ctrl Pts',(-0.166093592002812,-1.,-1.9564675971873));
#39618=CARTESIAN_POINT('Ctrl Pts',(-0.164816568920269,-1.,-1.96229379940136));
#39619=CARTESIAN_POINT('Ctrl Pts',(-0.163478185457734,-1.,-1.96816512677967));
#39620=CARTESIAN_POINT('Ctrl Pts',(-0.162079693556289,-1.,-1.97406280235188));
#39621=CARTESIAN_POINT('Ctrl Pts',(-0.160622060784611,-1.,-1.97996195437559));
#39622=CARTESIAN_POINT('Ctrl Pts',(-0.159106226437299,-1.,-1.98584238283292));
#39623=CARTESIAN_POINT('Ctrl Pts',(-0.157533331459227,-1.,-1.99169810931908));
#39624=CARTESIAN_POINT('Ctrl Pts',(-0.155904629548783,-1.,-1.99753284771497));
#39625=CARTESIAN_POINT('Ctrl Pts',(-0.154221403049722,-1.,-2.00335565310543));
#39626=CARTESIAN_POINT('Ctrl Pts',(-0.15248488362145,-1.,-2.00917680318424));
#39627=CARTESIAN_POINT('Ctrl Pts',(-0.150696157673078,-1.,-2.01500291940238));
#39628=CARTESIAN_POINT('Ctrl Pts',(-0.148856124775337,-1.,-2.02083464969894));
#39629=CARTESIAN_POINT('Ctrl Pts',(-0.146965557332583,-1.,-2.02666926182017));
#39630=CARTESIAN_POINT('Ctrl Pts',(-0.145025140186057,-1.,-2.03250223739942));
#39631=CARTESIAN_POINT('Ctrl Pts',(-0.143035515058209,-1.,-2.03832911025912));
#39632=CARTESIAN_POINT('Ctrl Pts',(-0.140997332152546,-1.,-2.04414757947916));
#39633=CARTESIAN_POINT('Ctrl Pts',(-0.138911255368966,-1.,-2.04995762001328));
#39634=CARTESIAN_POINT('Ctrl Pts',(-0.136777941218044,-1.,-2.05576044414264));
#39635=CARTESIAN_POINT('Ctrl Pts',(-0.134598026192106,-1.,-2.06155781517842));
#39636=CARTESIAN_POINT('Ctrl Pts',(-0.13237211154771,-1.,-2.06735123910326));
#39637=CARTESIAN_POINT('Ctrl Pts',(-0.130100748328403,-1.,-2.07314114713063));
#39638=CARTESIAN_POINT('Ctrl Pts',(-0.12778444527612,-1.,-2.07892715110987));
#39639=CARTESIAN_POINT('Ctrl Pts',(-0.125423679412061,-1.,-2.08470840653643));
#39640=CARTESIAN_POINT('Ctrl Pts',(-0.123018905621083,-1.,-2.09048392424825));
#39641=CARTESIAN_POINT('Ctrl Pts',(-0.120570567965122,-1.,-2.0962529286773));
#39642=CARTESIAN_POINT('Ctrl Pts',(-0.118079107988355,-1.,-2.102015121329));
#39643=CARTESIAN_POINT('Ctrl Pts',(-0.115544957687926,-1.,-2.10777050261309));
#39644=CARTESIAN_POINT('Ctrl Pts',(-0.112968534419737,-1.,-2.11351924490306));
#39645=CARTESIAN_POINT('Ctrl Pts',(-0.110350236135025,-1.,-2.11926155590865));
#39646=CARTESIAN_POINT('Ctrl Pts',(-0.10769043523109,-1.,-2.12499752307));
#39647=CARTESIAN_POINT('Ctrl Pts',(-0.104989479152739,-1.,-2.13072704887293));
#39648=CARTESIAN_POINT('Ctrl Pts',(-0.1022477005561,-1.,-2.13644992667165));
#39649=CARTESIAN_POINT('Ctrl Pts',(-0.0994654261990915,-1.,-2.14216588396025));
#39650=CARTESIAN_POINT('Ctrl Pts',(-0.0966429852305459,-1.,-2.14787463531795));
#39651=CARTESIAN_POINT('Ctrl Pts',(-0.0937807218867643,-1.,-2.1535759397817));
#39652=CARTESIAN_POINT('Ctrl Pts',(-0.0908789888107265,-1.,-2.15926961544516));
#39653=CARTESIAN_POINT('Ctrl Pts',(-0.0879381291386923,-1.,-2.16495552645014));
#39654=CARTESIAN_POINT('Ctrl Pts',(-0.0849584620835372,-1.,-2.17063357870952));
#39655=CARTESIAN_POINT('Ctrl Pts',(-0.0819402680872765,-1.,-2.176303712113));
#39656=CARTESIAN_POINT('Ctrl Pts',(-0.0788837727685243,-1.,-2.18196589448887));
#39657=CARTESIAN_POINT('Ctrl Pts',(-0.0757891465836148,-1.,-2.1876201139953));
#39658=CARTESIAN_POINT('Ctrl Pts',(-0.0732830357306725,-1.,-2.19213712013662));
#39659=CARTESIAN_POINT('Ctrl Pts',(-0.0713863779526154,-1.,-2.19552129484002));
#39660=CARTESIAN_POINT('Ctrl Pts',(-0.070114353632549,-1.,-2.19777582085423));
#39661=CARTESIAN_POINT('Ctrl Pts',(-0.0694764450219581,-1.,-2.19890268624765));
#39662=CARTESIAN_POINT('',(0.0694764450219584,-1.,-2.19890268624765));
#39663=CARTESIAN_POINT('',(-0.0694764450219581,-1.,-2.19890268624765));
#39664=CARTESIAN_POINT('',(0.163289472382896,-1.,-1.74236521665491));
#39665=CARTESIAN_POINT('Ctrl Pts',(0.0694764450219584,-1.,-2.19890268624765));
#39666=CARTESIAN_POINT('Ctrl Pts',(0.0701143536324926,-1.,-2.19777582085261));
#39667=CARTESIAN_POINT('Ctrl Pts',(0.0713863779524627,-1.,-2.19552129483562));
#39668=CARTESIAN_POINT('Ctrl Pts',(0.0732830357304276,-1.,-2.19213712012956));
#39669=CARTESIAN_POINT('Ctrl Pts',(0.0757891465833411,-1.,-2.1876201139874));
#39670=CARTESIAN_POINT('Ctrl Pts',(0.0788837727683228,-1.,-2.18196589448304));
#39671=CARTESIAN_POINT('Ctrl Pts',(0.0819402680871939,-1.,-2.1763037121106));
#39672=CARTESIAN_POINT('Ctrl Pts',(0.0849584620835643,-1.,-2.17063357871031));
#39673=CARTESIAN_POINT('Ctrl Pts',(0.0879381291387823,-1.,-2.16495552645275));
#39674=CARTESIAN_POINT('Ctrl Pts',(0.0908789888108266,-1.,-2.15926961544808));
#39675=CARTESIAN_POINT('Ctrl Pts',(0.0937807218868345,-1.,-2.15357593978377));
#39676=CARTESIAN_POINT('Ctrl Pts',(0.0966429852305689,-1.,-2.14787463531864));
#39677=CARTESIAN_POINT('Ctrl Pts',(0.0994654261990743,-1.,-2.14216588395974));
#39678=CARTESIAN_POINT('Ctrl Pts',(0.102247700556064,-1.,-2.13644992667052));
#39679=CARTESIAN_POINT('Ctrl Pts',(0.104989479152703,-1.,-2.1307270488718));
#39680=CARTESIAN_POINT('Ctrl Pts',(0.107690435231068,-1.,-2.12499752306927));
#39681=CARTESIAN_POINT('Ctrl Pts',(0.11035023613502,-1.,-2.11926155590849));
#39682=CARTESIAN_POINT('Ctrl Pts',(0.112968534419746,-1.,-2.11351924490335));
#39683=CARTESIAN_POINT('Ctrl Pts',(0.11554495768794,-1.,-2.10777050261359));
#39684=CARTESIAN_POINT('Ctrl Pts',(0.118079107988368,-1.,-2.10201512132945));
#39685=CARTESIAN_POINT('Ctrl Pts',(0.120570567965129,-1.,-2.09625292867756));
#39686=CARTESIAN_POINT('Ctrl Pts',(0.123018905621083,-1.,-2.09048392424826));
#39687=CARTESIAN_POINT('Ctrl Pts',(0.125423679412058,-1.,-2.08470840653628));
#39688=CARTESIAN_POINT('Ctrl Pts',(0.127784445276116,-1.,-2.07892715110967));
#39689=CARTESIAN_POINT('Ctrl Pts',(0.1301007483284,-1.,-2.07314114713047));
#39690=CARTESIAN_POINT('Ctrl Pts',(0.13237211154771,-1.,-2.06735123910319));
#39691=CARTESIAN_POINT('Ctrl Pts',(0.134598026192107,-1.,-2.06155781517844));
#39692=CARTESIAN_POINT('Ctrl Pts',(0.136777941218044,-1.,-2.0557604441427));
#39693=CARTESIAN_POINT('Ctrl Pts',(0.138911255368966,-1.,-2.04995762001333));
#39694=CARTESIAN_POINT('Ctrl Pts',(0.140997332152545,-1.,-2.04414757947919));
#39695=CARTESIAN_POINT('Ctrl Pts',(0.143035515058208,-1.,-2.03832911025913));
#39696=CARTESIAN_POINT('Ctrl Pts',(0.145025140186058,-1.,-2.03250223739941));
#39697=CARTESIAN_POINT('Ctrl Pts',(0.146965557332586,-1.,-2.02666926182017));
#39698=CARTESIAN_POINT('Ctrl Pts',(0.148856124775343,-1.,-2.02083464969897));
#39699=CARTESIAN_POINT('Ctrl Pts',(0.150696157673084,-1.,-2.01500291940243));
#39700=CARTESIAN_POINT('Ctrl Pts',(0.152484883621452,-1.,-2.00917680318426));
#39701=CARTESIAN_POINT('Ctrl Pts',(0.154221403049719,-1.,-2.00335565310539));
#39702=CARTESIAN_POINT('Ctrl Pts',(0.155904629548774,-1.,-1.99753284771487));
#39703=CARTESIAN_POINT('Ctrl Pts',(0.157533331459215,-1.,-1.99169810931893));
#39704=CARTESIAN_POINT('Ctrl Pts',(0.159106226437288,-1.,-1.98584238283279));
#39705=CARTESIAN_POINT('Ctrl Pts',(0.16062206078461,-1.,-1.97996195437557));
#39706=CARTESIAN_POINT('Ctrl Pts',(0.162079693556302,-1.,-1.97406280235204));
#39707=CARTESIAN_POINT('Ctrl Pts',(0.16347818545776,-1.,-1.96816512678));
#39708=CARTESIAN_POINT('Ctrl Pts',(0.1648165689203,-1.,-1.96229379940174));
#39709=CARTESIAN_POINT('Ctrl Pts',(0.166093592002833,-1.,-1.95646759718755));
#39710=CARTESIAN_POINT('Ctrl Pts',(0.167307501784469,-1.,-1.95069027794286));
#39711=CARTESIAN_POINT('Ctrl Pts',(0.168455741607516,-1.,-1.94493757756879));
#39712=CARTESIAN_POINT('Ctrl Pts',(0.169534904817425,-1.,-1.93915639211497));
#39713=CARTESIAN_POINT('Ctrl Pts',(0.170541253116136,-1.,-1.93329183155455));
#39714=CARTESIAN_POINT('Ctrl Pts',(0.17147119153296,-1.,-1.92731093582));
#39715=CARTESIAN_POINT('Ctrl Pts',(0.172321621259557,-1.,-1.92122334398034));
#39716=CARTESIAN_POINT('Ctrl Pts',(0.173090695383619,-1.,-1.91511429159681));
#39717=CARTESIAN_POINT('Ctrl Pts',(0.173776635257984,-1.,-1.90911693975475));
#39718=CARTESIAN_POINT('Ctrl Pts',(0.174375518661222,-1.,-1.90335253863003));
#39719=CARTESIAN_POINT('Ctrl Pts',(0.174879405091277,-1.,-1.89788101117148));
#39720=CARTESIAN_POINT('Ctrl Pts',(0.175274276190664,-1.,-1.89264630198279));
#39721=CARTESIAN_POINT('Ctrl Pts',(0.175538155840286,-1.,-1.88742606272818));
#39722=CARTESIAN_POINT('Ctrl Pts',(0.175644148889271,-1.,-1.88188663144846));
#39723=CARTESIAN_POINT('Ctrl Pts',(0.175563480746205,-1.,-1.87563767773249));
#39724=CARTESIAN_POINT('Ctrl Pts',(0.175268337590901,-1.,-1.86828349694972));
#39725=CARTESIAN_POINT('Ctrl Pts',(0.174735259276856,-1.,-1.85948367089838));
#39726=CARTESIAN_POINT('Ctrl Pts',(0.173946627589401,-1.,-1.84898113200543));
#39727=CARTESIAN_POINT('Ctrl Pts',(0.17288944289442,-1.,-1.83658380530747));
#39728=CARTESIAN_POINT('Ctrl Pts',(0.171554770207306,-1.,-1.82215766815414));
#39729=CARTESIAN_POINT('Ctrl Pts',(0.169936923908078,-1.,-1.80561530633924));
#39730=CARTESIAN_POINT('Ctrl Pts',(0.16803277280837,-1.,-1.78690649988931));
#39731=CARTESIAN_POINT('Ctrl Pts',(0.166279355148738,-1.,-1.77018771687692));
#39732=CARTESIAN_POINT('Ctrl Pts',(0.164834765708484,-1.,-1.75666056640041));
#39733=CARTESIAN_POINT('Ctrl Pts',(0.163814161002474,-1.,-1.74720349503904));
#39734=CARTESIAN_POINT('Ctrl Pts',(0.163289472382896,-1.,-1.74236521665491));
#39735=CARTESIAN_POINT('',(0.383122945602004,-1.,-1.7075470150345));
#39736=CARTESIAN_POINT('Origin',(0.,-1.,0.));
#39737=CARTESIAN_POINT('',(0.61342227326009,-1.,-2.11275013067528));
#39738=CARTESIAN_POINT('Ctrl Pts',(0.383122945602004,-1.,-1.7075470150345));
#39739=CARTESIAN_POINT('Ctrl Pts',(0.384119047314215,-1.,-1.71231062891398));
#39740=CARTESIAN_POINT('Ctrl Pts',(0.386070790323281,-1.,-1.72162022244582));
#39741=CARTESIAN_POINT('Ctrl Pts',(0.388877023502615,-1.,-1.73493170972829));
#39742=CARTESIAN_POINT('Ctrl Pts',(0.392375812285395,-1.,-1.75137405310193));
#39743=CARTESIAN_POINT('Ctrl Pts',(0.396346196110688,-1.,-1.76975560043442));
#39744=CARTESIAN_POINT('Ctrl Pts',(0.399919403774155,-1.,-1.78598826343754));
#39745=CARTESIAN_POINT('Ctrl Pts',(0.403107976163396,-1.,-1.80012077173238));
#39746=CARTESIAN_POINT('Ctrl Pts',(0.405933518407175,-1.,-1.81223801812013));
#39747=CARTESIAN_POINT('Ctrl Pts',(0.408428948106227,-1.,-1.82247022677562));
#39748=CARTESIAN_POINT('Ctrl Pts',(0.410641256301276,-1.,-1.83100408895047));
#39749=CARTESIAN_POINT('Ctrl Pts',(0.412633125322945,-1.,-1.8380895347617));
#39750=CARTESIAN_POINT('Ctrl Pts',(0.414487438255542,-1.,-1.84405757074218));
#39751=CARTESIAN_POINT('Ctrl Pts',(0.416300022039885,-1.,-1.84929312930314));
#39752=CARTESIAN_POINT('Ctrl Pts',(0.418164129144045,-1.,-1.8541763285645));
#39753=CARTESIAN_POINT('Ctrl Pts',(0.420157287975583,-1.,-1.8590328109667));
#39754=CARTESIAN_POINT('Ctrl Pts',(0.422327307417884,-1.,-1.86408083333863));
#39755=CARTESIAN_POINT('Ctrl Pts',(0.424678177290876,-1.,-1.8693780394412));
#39756=CARTESIAN_POINT('Ctrl Pts',(0.427183828518743,-1.,-1.87486989291334));
#39757=CARTESIAN_POINT('Ctrl Pts',(0.429803062482217,-1.,-1.88044229001779));
#39758=CARTESIAN_POINT('Ctrl Pts',(0.432493038548833,-1.,-1.88596913666828));
#39759=CARTESIAN_POINT('Ctrl Pts',(0.43522566096358,-1.,-1.89136993975585));
#39760=CARTESIAN_POINT('Ctrl Pts',(0.437995003948443,-1.,-1.89663648956549));
#39761=CARTESIAN_POINT('Ctrl Pts',(0.44080783370416,-1.,-1.90180124389137));
#39762=CARTESIAN_POINT('Ctrl Pts',(0.44367755684917,-1.,-1.90691756144906));
#39763=CARTESIAN_POINT('Ctrl Pts',(0.446617343485651,-1.,-1.91203699981095));
#39764=CARTESIAN_POINT('Ctrl Pts',(0.449632260106572,-1.,-1.91718342555717));
#39765=CARTESIAN_POINT('Ctrl Pts',(0.452719478359356,-1.,-1.9223538064847));
#39766=CARTESIAN_POINT('Ctrl Pts',(0.455872005174335,-1.,-1.92753067150461));
#39767=CARTESIAN_POINT('Ctrl Pts',(0.459081234547931,-1.,-1.93269066517936));
#39768=CARTESIAN_POINT('Ctrl Pts',(0.462340031009087,-1.,-1.93781486640834));
#39769=CARTESIAN_POINT('Ctrl Pts',(0.465645462026064,-1.,-1.94289794196205));
#39770=CARTESIAN_POINT('Ctrl Pts',(0.468997482913158,-1.,-1.94794381136524));
#39771=CARTESIAN_POINT('Ctrl Pts',(0.472397672264079,-1.,-1.95296148278136));
#39772=CARTESIAN_POINT('Ctrl Pts',(0.475848034683171,-1.,-1.95796111148175));
#39773=CARTESIAN_POINT('Ctrl Pts',(0.479349583074846,-1.,-1.96294933055938));
#39774=CARTESIAN_POINT('Ctrl Pts',(0.482901662120686,-1.,-1.96792703422358));
#39775=CARTESIAN_POINT('Ctrl Pts',(0.486502692907661,-1.,-1.97289186263272));
#39776=CARTESIAN_POINT('Ctrl Pts',(0.490150627860955,-1.,-1.97783973019229));
#39777=CARTESIAN_POINT('Ctrl Pts',(0.493843476541492,-1.,-1.9827665876182));
#39778=CARTESIAN_POINT('Ctrl Pts',(0.497579909545564,-1.,-1.98767044752929));
#39779=CARTESIAN_POINT('Ctrl Pts',(0.501359287727129,-1.,-1.9925514912615));
#39780=CARTESIAN_POINT('Ctrl Pts',(0.505181361323011,-1.,-1.99741107463567));
#39781=CARTESIAN_POINT('Ctrl Pts',(0.509046069886152,-1.,-2.00225107134733));
#39782=CARTESIAN_POINT('Ctrl Pts',(0.512953306961813,-1.,-2.00707309946955));
#39783=CARTESIAN_POINT('Ctrl Pts',(0.516902681728733,-1.,-2.01187773939257));
#39784=CARTESIAN_POINT('Ctrl Pts',(0.520893590399428,-1.,-2.01666477917306));
#39785=CARTESIAN_POINT('Ctrl Pts',(0.524925318333518,-1.,-2.02143356304712));
#39786=CARTESIAN_POINT('Ctrl Pts',(0.52899712724191,-1.,-2.02618329083289));
#39787=CARTESIAN_POINT('Ctrl Pts',(0.533108355132905,-1.,-2.03091336214401));
#39788=CARTESIAN_POINT('Ctrl Pts',(0.537258489833134,-1.,-2.03562362953993));
#39789=CARTESIAN_POINT('Ctrl Pts',(0.54144712061552,-1.,-2.0403142269048));
#39790=CARTESIAN_POINT('Ctrl Pts',(0.545673903817348,-1.,-2.0449854471456));
#39791=CARTESIAN_POINT('Ctrl Pts',(0.549938525150342,-1.,-2.04963761077974));
#39792=CARTESIAN_POINT('Ctrl Pts',(0.554240657464109,-1.,-2.05427091604482));
#39793=CARTESIAN_POINT('Ctrl Pts',(0.558579940185467,-1.,-2.05888537756571));
#39794=CARTESIAN_POINT('Ctrl Pts',(0.562955993082574,-1.,-2.06348090160697));
#39795=CARTESIAN_POINT('Ctrl Pts',(0.567368421181229,-1.,-2.06805732997383));
#39796=CARTESIAN_POINT('Ctrl Pts',(0.571816823242411,-1.,-2.07261449292758));
#39797=CARTESIAN_POINT('Ctrl Pts',(0.576300797416274,-1.,-2.07715226767361));
#39798=CARTESIAN_POINT('Ctrl Pts',(0.580819952107256,-1.,-2.08167059018138));
#39799=CARTESIAN_POINT('Ctrl Pts',(0.585373918990895,-1.,-2.086169437277));
#39800=CARTESIAN_POINT('Ctrl Pts',(0.589962365403189,-1.,-2.09064881812053));
#39801=CARTESIAN_POINT('Ctrl Pts',(0.594585006052823,-1.,-2.09510876220501));
#39802=CARTESIAN_POINT('Ctrl Pts',(0.599241616422144,-1.,-2.09954930865331));
#39803=CARTESIAN_POINT('Ctrl Pts',(0.603932030738212,-1.,-2.10397049887709));
#39804=CARTESIAN_POINT('Ctrl Pts',(0.607711315456826,-1.,-2.10749199615859));
#39805=CARTESIAN_POINT('Ctrl Pts',(0.610560911691113,-1.,-2.11012443807661));
#39806=CARTESIAN_POINT('Ctrl Pts',(0.61246736556225,-1.,-2.11187554260142));
#39807=CARTESIAN_POINT('Ctrl Pts',(0.61342227326009,-1.,-2.11275013067528));
#39808=CARTESIAN_POINT('',(0.745574324794401,-1.,-2.0698113262342));
#39809=CARTESIAN_POINT('',(0.61342227326009,-1.,-2.11275013067528));
#39810=CARTESIAN_POINT('',(0.693717979106306,-1.,-1.60662857109684));
#39811=CARTESIAN_POINT('Ctrl Pts',(0.745574324794401,-1.,-2.0698113262342));
#39812=CARTESIAN_POINT('Ctrl Pts',(0.74583279137781,-1.,-2.06854248895575));
#39813=CARTESIAN_POINT('Ctrl Pts',(0.746345871542695,-1.,-2.06600523016401));
#39814=CARTESIAN_POINT('Ctrl Pts',(0.747103932785504,-1.,-2.06220058927162));
#39815=CARTESIAN_POINT('Ctrl Pts',(0.748091554181101,-1.,-2.05713023030263));
#39816=CARTESIAN_POINT('Ctrl Pts',(0.749287468663053,-1.,-2.05079645591606));
#39817=CARTESIAN_POINT('Ctrl Pts',(0.750444657874758,-1.,-2.04446689147754));
#39818=CARTESIAN_POINT('Ctrl Pts',(0.751562963361383,-1.,-2.03814160092173));
#39819=CARTESIAN_POINT('Ctrl Pts',(0.752642180488104,-1.,-2.03182068456467));
#39820=CARTESIAN_POINT('Ctrl Pts',(0.753682061113765,-1.,-2.02550428623587));
#39821=CARTESIAN_POINT('Ctrl Pts',(0.75468233072352,-1.,-2.01919259406003));
#39822=CARTESIAN_POINT('Ctrl Pts',(0.7556427049581,-1.,-2.01288584328149));
#39823=CARTESIAN_POINT('Ctrl Pts',(0.756562904646496,-1.,-2.00658431587682));
#39824=CARTESIAN_POINT('Ctrl Pts',(0.757442676862341,-1.,-2.00028834739072));
#39825=CARTESIAN_POINT('Ctrl Pts',(0.758281796766377,-1.,-1.9939983109871));
#39826=CARTESIAN_POINT('Ctrl Pts',(0.759080037802242,-1.,-1.98771456680806));
#39827=CARTESIAN_POINT('Ctrl Pts',(0.759837147452135,-1.,-1.98143741418156));
#39828=CARTESIAN_POINT('Ctrl Pts',(0.760552825409855,-1.,-1.97516705321521));
#39829=CARTESIAN_POINT('Ctrl Pts',(0.761226690483986,-1.,-1.96890351582545));
#39830=CARTESIAN_POINT('Ctrl Pts',(0.761858300014575,-1.,-1.96264672744229));
#39831=CARTESIAN_POINT('Ctrl Pts',(0.762447203806263,-1.,-1.95639665309893));
#39832=CARTESIAN_POINT('Ctrl Pts',(0.762992990878774,-1.,-1.95015342590025));
#39833=CARTESIAN_POINT('Ctrl Pts',(0.76349533353858,-1.,-1.94391746617626));
#39834=CARTESIAN_POINT('Ctrl Pts',(0.763954049121393,-1.,-1.93768964875867));
#39835=CARTESIAN_POINT('Ctrl Pts',(0.764369010673889,-1.,-1.93147105496367));
#39836=CARTESIAN_POINT('Ctrl Pts',(0.764740025488189,-1.,-1.92526263537041));
#39837=CARTESIAN_POINT('Ctrl Pts',(0.765066729667095,-1.,-1.91906491634197));
#39838=CARTESIAN_POINT('Ctrl Pts',(0.765348465884739,-1.,-1.91287765805174));
#39839=CARTESIAN_POINT('Ctrl Pts',(0.765584196937936,-1.,-1.90669961402362));
#39840=CARTESIAN_POINT('Ctrl Pts',(0.765772772593395,-1.,-1.90052930393599));
#39841=CARTESIAN_POINT('Ctrl Pts',(0.765913193856979,-1.,-1.89436577771389));
#39842=CARTESIAN_POINT('Ctrl Pts',(0.76600483706209,-1.,-1.88820926433409));
#39843=CARTESIAN_POINT('Ctrl Pts',(0.766047794851868,-1.,-1.88206215302561));
#39844=CARTESIAN_POINT('Ctrl Pts',(0.766042837036759,-1.,-1.87592888967886));
#39845=CARTESIAN_POINT('Ctrl Pts',(0.765990708546111,-1.,-1.86981398314345));
#39846=CARTESIAN_POINT('Ctrl Pts',(0.765891519092557,-1.,-1.86372027063315));
#39847=CARTESIAN_POINT('Ctrl Pts',(0.765744212909305,-1.,-1.85764741390391));
#39848=CARTESIAN_POINT('Ctrl Pts',(0.765545710619023,-1.,-1.85158945130054));
#39849=CARTESIAN_POINT('Ctrl Pts',(0.765291664861971,-1.,-1.84553698875911));
#39850=CARTESIAN_POINT('Ctrl Pts',(0.764978057881687,-1.,-1.83948181064823));
#39851=CARTESIAN_POINT('Ctrl Pts',(0.764602549687845,-1.,-1.8334207722714));
#39852=CARTESIAN_POINT('Ctrl Pts',(0.764165902606055,-1.,-1.8273599120008));
#39853=CARTESIAN_POINT('Ctrl Pts',(0.763673465462854,-1.,-1.82131873145297));
#39854=CARTESIAN_POINT('Ctrl Pts',(0.763132003836783,-1.,-1.81532118405566));
#39855=CARTESIAN_POINT('Ctrl Pts',(0.762546129464036,-1.,-1.80938551463989));
#39856=CARTESIAN_POINT('Ctrl Pts',(0.761915336443515,-1.,-1.80351583877334));
#39857=CARTESIAN_POINT('Ctrl Pts',(0.761229695230359,-1.,-1.79768986997735));
#39858=CARTESIAN_POINT('Ctrl Pts',(0.760469555880425,-1.,-1.79185815610802));
#39859=CARTESIAN_POINT('Ctrl Pts',(0.759614401109868,-1.,-1.78596964884527));
#39860=CARTESIAN_POINT('Ctrl Pts',(0.75865062667738,-1.,-1.77999411220912));
#39861=CARTESIAN_POINT('Ctrl Pts',(0.757578264077238,-1.,-1.77394167108342));
#39862=CARTESIAN_POINT('Ctrl Pts',(0.756421896028403,-1.,-1.76789396003141));
#39863=CARTESIAN_POINT('Ctrl Pts',(0.755220979975262,-1.,-1.7619781724032));
#39864=CARTESIAN_POINT('Ctrl Pts',(0.75400925402848,-1.,-1.75631083600175));
#39865=CARTESIAN_POINT('Ctrl Pts',(0.752797683531377,-1.,-1.75095139468809));
#39866=CARTESIAN_POINT('Ctrl Pts',(0.751555614163629,-1.,-1.74585086852298));
#39867=CARTESIAN_POINT('Ctrl Pts',(0.75019343597954,-1.,-1.74080458266705));
#39868=CARTESIAN_POINT('Ctrl Pts',(0.748582462954854,-1.,-1.73550351679848));
#39869=CARTESIAN_POINT('Ctrl Pts',(0.746574710096436,-1.,-1.72958533647399));
#39870=CARTESIAN_POINT('Ctrl Pts',(0.744021445433764,-1.,-1.7226822991693));
#39871=CARTESIAN_POINT('Ctrl Pts',(0.740795162032087,-1.,-1.71447789751927));
#39872=CARTESIAN_POINT('Ctrl Pts',(0.736799665724771,-1.,-1.70473309006121));
#39873=CARTESIAN_POINT('Ctrl Pts',(0.731963238697195,-1.,-1.69326921975743));
#39874=CARTESIAN_POINT('Ctrl Pts',(0.726235967997433,-1.,-1.67996158455503));
#39875=CARTESIAN_POINT('Ctrl Pts',(0.719585433804282,-1.,-1.6647288055568));
#39876=CARTESIAN_POINT('Ctrl Pts',(0.711993139355394,-1.,-1.64752408832016));
#39877=CARTESIAN_POINT('Ctrl Pts',(0.705159151988319,-1.,-1.63216541664676));
#39878=CARTESIAN_POINT('Ctrl Pts',(0.699605146405088,-1.,-1.61974673472612));
#39879=CARTESIAN_POINT('Ctrl Pts',(0.695712097881194,-1.,-1.61106790958151));
#39880=CARTESIAN_POINT('Ctrl Pts',(0.693717979106306,-1.,-1.60662857109684));
#39881=CARTESIAN_POINT('',(0.892032620296855,-1.,-1.5055822144029));
#39882=CARTESIAN_POINT('Origin',(0.,-1.,0.));
#39883=CARTESIAN_POINT('',(1.23627494547115,-1.,-1.81978687191668));
#39884=CARTESIAN_POINT('Ctrl Pts',(0.892032620296855,-1.,-1.5055822144029));
#39885=CARTESIAN_POINT('Ctrl Pts',(0.894452006964543,-1.,-1.50980486806688));
#39886=CARTESIAN_POINT('Ctrl Pts',(0.89918504748351,-1.,-1.51805569590094));
#39887=CARTESIAN_POINT('Ctrl Pts',(0.905967409625651,-1.,-1.52984849887993));
#39888=CARTESIAN_POINT('Ctrl Pts',(0.914375919026456,-1.,-1.54440491149498));
#39889=CARTESIAN_POINT('Ctrl Pts',(0.923832188944341,-1.,-1.56065988578893));
#39890=CARTESIAN_POINT('Ctrl Pts',(0.932246680108685,-1.,-1.57499388382243));
#39891=CARTESIAN_POINT('Ctrl Pts',(0.939646377893399,-1.,-1.58744937487176));
#39892=CARTESIAN_POINT('Ctrl Pts',(0.946078063315257,-1.,-1.59810042043673));
#39893=CARTESIAN_POINT('Ctrl Pts',(0.951613284356035,-1.,-1.60706069896936));
#39894=CARTESIAN_POINT('Ctrl Pts',(0.95635442292067,-1.,-1.61449324337085));
#39895=CARTESIAN_POINT('Ctrl Pts',(0.960438326101728,-1.,-1.62061638140221));
#39896=CARTESIAN_POINT('Ctrl Pts',(0.964046107040535,-1.,-1.62571930670187));
#39897=CARTESIAN_POINT('Ctrl Pts',(0.967387853230345,-1.,-1.63013849959462));
#39898=CARTESIAN_POINT('Ctrl Pts',(0.970669715997509,-1.,-1.63420665729798));
#39899=CARTESIAN_POINT('Ctrl Pts',(0.974066058287418,-1.,-1.63820952658144));
#39900=CARTESIAN_POINT('Ctrl Pts',(0.977689794119416,-1.,-1.64233990826687));
#39901=CARTESIAN_POINT('Ctrl Pts',(0.981562530939489,-1.,-1.64665139190656));
#39902=CARTESIAN_POINT('Ctrl Pts',(0.98564262292082,-1.,-1.65110016612638));
#39903=CARTESIAN_POINT('Ctrl Pts',(0.989855627854164,-1.,-1.65559044289699));
#39904=CARTESIAN_POINT('Ctrl Pts',(0.994121836661305,-1.,-1.66001553809947));
#39905=CARTESIAN_POINT('Ctrl Pts',(0.998389654952757,-1.,-1.66430758030376));
#39906=CARTESIAN_POINT('Ctrl Pts',(1.00265091003727,-1.,-1.66846059277303));
#39907=CARTESIAN_POINT('Ctrl Pts',(1.00692206696414,-1.,-1.67250335383293));
#39908=CARTESIAN_POINT('Ctrl Pts',(1.01123236493511,-1.,-1.67648246776464));
#39909=CARTESIAN_POINT('Ctrl Pts',(1.01561026162773,-1.,-1.68044289894798));
#39910=CARTESIAN_POINT('Ctrl Pts',(1.02006795074201,-1.,-1.68440578021706));
#39911=CARTESIAN_POINT('Ctrl Pts',(1.02460180535255,-1.,-1.68836910178447));
#39912=CARTESIAN_POINT('Ctrl Pts',(1.02919977579147,-1.,-1.69231840863458));
#39913=CARTESIAN_POINT('Ctrl Pts',(1.03384646003588,-1.,-1.69623414782771));
#39914=CARTESIAN_POINT('Ctrl Pts',(1.03852922490789,-1.,-1.70010052930962));
#39915=CARTESIAN_POINT('Ctrl Pts',(1.04324363334554,-1.,-1.70391338707982));
#39916=CARTESIAN_POINT('Ctrl Pts',(1.04799085404995,-1.,-1.70767646263649));
#39917=CARTESIAN_POINT('Ctrl Pts',(1.05277517202855,-1.,-1.71139783543989));
#39918=CARTESIAN_POINT('Ctrl Pts',(1.05760163192479,-1.,-1.7150865442702));
#39919=CARTESIAN_POINT('Ctrl Pts',(1.06247324680647,-1.,-1.71874858456904));
#39920=CARTESIAN_POINT('Ctrl Pts',(1.06738966975462,-1.,-1.72238500928453));
#39921=CARTESIAN_POINT('Ctrl Pts',(1.07234866990252,-1.,-1.72599406198488));
#39922=CARTESIAN_POINT('Ctrl Pts',(1.0773470373727,-1.,-1.72957248977424));
#39923=CARTESIAN_POINT('Ctrl Pts',(1.08238162784749,-1.,-1.73311705663407));
#39924=CARTESIAN_POINT('Ctrl Pts',(1.08745056285427,-1.,-1.73662628326091));
#39925=CARTESIAN_POINT('Ctrl Pts',(1.09255329056493,-1.,-1.74010053962247));
#39926=CARTESIAN_POINT('Ctrl Pts',(1.09768999241225,-1.,-1.74354119236208));
#39927=CARTESIAN_POINT('Ctrl Pts',(1.10286118991143,-1.,-1.74695004214923));
#39928=CARTESIAN_POINT('Ctrl Pts',(1.10806728183007,-1.,-1.7503286607592));
#39929=CARTESIAN_POINT('Ctrl Pts',(1.11330807582551,-1.,-1.7536777209463));
#39930=CARTESIAN_POINT('Ctrl Pts',(1.11858293216763,-1.,-1.75699720772105));
#39931=CARTESIAN_POINT('Ctrl Pts',(1.12389096855086,-1.,-1.76028671825096));
#39932=CARTESIAN_POINT('Ctrl Pts',(1.12923123555075,-1.,-1.7635457196617));
#39933=CARTESIAN_POINT('Ctrl Pts',(1.1346029180462,-1.,-1.76677384551862));
#39934=CARTESIAN_POINT('Ctrl Pts',(1.14000548336975,-1.,-1.76997111386769));
#39935=CARTESIAN_POINT('Ctrl Pts',(1.1454385822692,-1.,-1.77313777896194));
#39936=CARTESIAN_POINT('Ctrl Pts',(1.15090197841514,-1.,-1.7762742255701));
#39937=CARTESIAN_POINT('Ctrl Pts',(1.15639547194698,-1.,-1.77938085564275));
#39938=CARTESIAN_POINT('Ctrl Pts',(1.16191881298499,-1.,-1.78245795881009));
#39939=CARTESIAN_POINT('Ctrl Pts',(1.16747166312303,-1.,-1.78550566040443));
#39940=CARTESIAN_POINT('Ctrl Pts',(1.17305363177328,-1.,-1.78852398877617));
#39941=CARTESIAN_POINT('Ctrl Pts',(1.17866429440809,-1.,-1.79151291552689));
#39942=CARTESIAN_POINT('Ctrl Pts',(1.18430321697432,-1.,-1.79447240321515));
#39943=CARTESIAN_POINT('Ctrl Pts',(1.18996997934445,-1.,-1.79740245923478));
#39944=CARTESIAN_POINT('Ctrl Pts',(1.19566418930242,-1.,-1.80030314369879));
#39945=CARTESIAN_POINT('Ctrl Pts',(1.20138548938974,-1.,-1.80317454838603));
#39946=CARTESIAN_POINT('Ctrl Pts',(1.20713356605475,-1.,-1.80601678480707));
#39947=CARTESIAN_POINT('Ctrl Pts',(1.21290815708314,-1.,-1.80882996917129));
#39948=CARTESIAN_POINT('Ctrl Pts',(1.21870906103557,-1.,-1.81161420806656));
#39949=CARTESIAN_POINT('Ctrl Pts',(1.2245361330495,-1.,-1.81436959210434));
#39950=CARTESIAN_POINT('Ctrl Pts',(1.2292186489137,-1.,-1.8165508718364));
#39951=CARTESIAN_POINT('Ctrl Pts',(1.2327422452705,-1.,-1.81817389921279));
#39952=CARTESIAN_POINT('Ctrl Pts',(1.23509651170476,-1.,-1.81925017193666));
#39953=CARTESIAN_POINT('Ctrl Pts',(1.23627494547115,-1.,-1.81978687191668));
#39954=CARTESIAN_POINT('',(1.34869019493419,-1.,-1.73811241238545));
#39955=CARTESIAN_POINT('',(1.23627494547115,-1.,-1.81978687191668));
#39956=CARTESIAN_POINT('',(1.15624053661742,-1.,-1.31362392696032));
#39957=CARTESIAN_POINT('Ctrl Pts',(1.34869019493419,-1.,-1.73811241238545));
#39958=CARTESIAN_POINT('Ctrl Pts',(1.34854391898045,-1.,-1.73682580585691));
#39959=CARTESIAN_POINT('Ctrl Pts',(1.34824783112887,-1.,-1.73425417885907));
#39960=CARTESIAN_POINT('Ctrl Pts',(1.34779309152035,-1.,-1.7304014965394));
#39961=CARTESIAN_POINT('Ctrl Pts',(1.34716554819527,-1.,-1.72527410680674));
#39962=CARTESIAN_POINT('Ctrl Pts',(1.34634568653227,-1.,-1.7188807715049));
#39963=CARTESIAN_POINT('Ctrl Pts',(1.34549029589416,-1.,-1.71250340686822));
#39964=CARTESIAN_POINT('Ctrl Pts',(1.34459924533831,-1.,-1.70614212266738));
#39965=CARTESIAN_POINT('Ctrl Pts',(1.34367237124483,-1.,-1.69979707754427));
#39966=CARTESIAN_POINT('Ctrl Pts',(1.34270948206319,-1.,-1.6934684849687));
#39967=CARTESIAN_POINT('Ctrl Pts',(1.341710374848,-1.,-1.68715660868764));
#39968=CARTESIAN_POINT('Ctrl Pts',(1.34067485185203,-1.,-1.68086176030362));
#39969=CARTESIAN_POINT('Ctrl Pts',(1.3396027347034,-1.,-1.67458429426086));
#39970=CARTESIAN_POINT('Ctrl Pts',(1.33849388654388,-1.,-1.66832460783989));
#39971=CARTESIAN_POINT('Ctrl Pts',(1.33734820885262,-1.,-1.66208312541983));
#39972=CARTESIAN_POINT('Ctrl Pts',(1.33616559745172,-1.,-1.65586025952593));
#39973=CARTESIAN_POINT('Ctrl Pts',(1.33494590467993,-1.,-1.6496563728683));
#39974=CARTESIAN_POINT('Ctrl Pts',(1.33368890676572,-1.,-1.6434717485603));
#39975=CARTESIAN_POINT('Ctrl Pts',(1.33239425103724,-1.,-1.63730653475089));
#39976=CARTESIAN_POINT('Ctrl Pts',(1.33106149345645,-1.,-1.63116079730923));
#39977=CARTESIAN_POINT('Ctrl Pts',(1.3296901950568,-1.,-1.62503464209797));
#39978=CARTESIAN_POINT('Ctrl Pts',(1.32828000610449,-1.,-1.61892832270724));
#39979=CARTESIAN_POINT('Ctrl Pts',(1.32683074483356,-1.,-1.6128423401575));
#39980=CARTESIAN_POINT('Ctrl Pts',(1.32534250785782,-1.,-1.60677758290954));
#39981=CARTESIAN_POINT('Ctrl Pts',(1.32381550858256,-1.,-1.60073511858687));
#39982=CARTESIAN_POINT('Ctrl Pts',(1.32224985747682,-1.,-1.59471591079403));
#39983=CARTESIAN_POINT('Ctrl Pts',(1.32064537110892,-1.,-1.58872057258245));
#39984=CARTESIAN_POINT('Ctrl Pts',(1.31900135021432,-1.,-1.58274907898834));
#39985=CARTESIAN_POINT('Ctrl Pts',(1.31731642317187,-1.,-1.5768005650559));
#39986=CARTESIAN_POINT('Ctrl Pts',(1.31558903860016,-1.,-1.57087397835723));
#39987=CARTESIAN_POINT('Ctrl Pts',(1.31381795281002,-1.,-1.56496872402353));
#39988=CARTESIAN_POINT('Ctrl Pts',(1.31200264341696,-1.,-1.55908521254821));
#39989=CARTESIAN_POINT('Ctrl Pts',(1.31014393684222,-1.,-1.55322568759481));
#39990=CARTESIAN_POINT('Ctrl Pts',(1.30824393907473,-1.,-1.54739413957185));
#39991=CARTESIAN_POINT('Ctrl Pts',(1.30630475189556,-1.,-1.54159462645432));
#39992=CARTESIAN_POINT('Ctrl Pts',(1.30432735639489,-1.,-1.53582981268977));
#39993=CARTESIAN_POINT('Ctrl Pts',(1.30231064395568,-1.,-1.53009970283891));
#39994=CARTESIAN_POINT('Ctrl Pts',(1.30024984366328,-1.,-1.52439957861062));
#39995=CARTESIAN_POINT('Ctrl Pts',(1.29813791800747,-1.,-1.51872184912724));
#39996=CARTESIAN_POINT('Ctrl Pts',(1.29596850710509,-1.,-1.51305994241402));
#39997=CARTESIAN_POINT('Ctrl Pts',(1.29373841372842,-1.,-1.50741159078365));
#39998=CARTESIAN_POINT('Ctrl Pts',(1.29145022885181,-1.,-1.50178230149776));
#39999=CARTESIAN_POINT('Ctrl Pts',(1.28911506584254,-1.,-1.49618896881754));
#40000=CARTESIAN_POINT('Ctrl Pts',(1.2867467611644,-1.,-1.4906522831278));
#40001=CARTESIAN_POINT('Ctrl Pts',(1.28435533880201,-1.,-1.4851881711891));
#40002=CARTESIAN_POINT('Ctrl Pts',(1.28194158939517,-1.,-1.47980070347096));
#40003=CARTESIAN_POINT('Ctrl Pts',(1.2794891824849,-1.,-1.4744717526707));
#40004=CARTESIAN_POINT('Ctrl Pts',(1.27696414831089,-1.,-1.46916035917133));
#40005=CARTESIAN_POINT('Ctrl Pts',(1.27433119897822,-1.,-1.46382431332476));
#40006=CARTESIAN_POINT('Ctrl Pts',(1.27156805265289,-1.,-1.45843906294697));
#40007=CARTESIAN_POINT('Ctrl Pts',(1.2686778680489,-1.,-1.45301422764247));
#40008=CARTESIAN_POINT('Ctrl Pts',(1.26570925118868,-1.,-1.44761985001662));
#40009=CARTESIAN_POINT('Ctrl Pts',(1.26273903323858,-1.,-1.44236470511303));
#40010=CARTESIAN_POINT('Ctrl Pts',(1.25983531012005,-1.,-1.43734919180848));
#40011=CARTESIAN_POINT('Ctrl Pts',(1.25702687965755,-1.,-1.43262645609691));
#40012=CARTESIAN_POINT('Ctrl Pts',(1.25426945222639,-1.,-1.42815938799387));
#40013=CARTESIAN_POINT('Ctrl Pts',(1.2514145557001,-1.,-1.42378102115575));
#40014=CARTESIAN_POINT('Ctrl Pts',(1.24824430986571,-1.,-1.41923722596025));
#40015=CARTESIAN_POINT('Ctrl Pts',(1.24450600513056,-1.,-1.41422913175179));
#40016=CARTESIAN_POINT('Ctrl Pts',(1.23994455029534,-1.,-1.40845295531283));
#40017=CARTESIAN_POINT('Ctrl Pts',(1.23434087290423,-1.,-1.40164708206106));
#40018=CARTESIAN_POINT('Ctrl Pts',(1.22752961899387,-1.,-1.39361389568796));
#40019=CARTESIAN_POINT('Ctrl Pts',(1.21938737280852,-1.,-1.38420564527715));
#40020=CARTESIAN_POINT('Ctrl Pts',(1.20982812925645,-1.,-1.37331915607905));
#40021=CARTESIAN_POINT('Ctrl Pts',(1.1987959077932,-1.,-1.36088705043885));
#40022=CARTESIAN_POINT('Ctrl Pts',(1.18625865667441,-1.,-1.34687054001093));
#40023=CARTESIAN_POINT('Ctrl Pts',(1.17501305789857,-1.,-1.33437539347008));
#40024=CARTESIAN_POINT('Ctrl Pts',(1.16589330093588,-1.,-1.32428080721772));
#40025=CARTESIAN_POINT('Ctrl Pts',(1.15950888730809,-1.,-1.31722977216397));
#40026=CARTESIAN_POINT('Ctrl Pts',(1.15624053661742,-1.,-1.31362392696032));
#40027=CARTESIAN_POINT('',(1.31362392696032,-1.,-1.15624053661742));
#40028=CARTESIAN_POINT('Origin',(0.,-1.,0.));
#40029=CARTESIAN_POINT('',(1.73811241238545,-1.,-1.34869019493419));
#40030=CARTESIAN_POINT('Ctrl Pts',(1.31362392696032,-1.,-1.15624053661742));
#40031=CARTESIAN_POINT('Ctrl Pts',(1.3172297721596,-1.,-1.15950888730433));
#40032=CARTESIAN_POINT('Ctrl Pts',(1.32428080720544,-1.,-1.16589330092532));
#40033=CARTESIAN_POINT('Ctrl Pts',(1.33437539344842,-1.,-1.17501305787994));
#40034=CARTESIAN_POINT('Ctrl Pts',(1.34687053998157,-1.,-1.18625865664915));
#40035=CARTESIAN_POINT('Ctrl Pts',(1.36088705040677,-1.,-1.1987959077656));
#40036=CARTESIAN_POINT('Ctrl Pts',(1.37331915604962,-1.,-1.20982812923113));
#40037=CARTESIAN_POINT('Ctrl Pts',(1.38420564525391,-1.,-1.21938737278853));
#40038=CARTESIAN_POINT('Ctrl Pts',(1.39361389567257,-1.,-1.22752961898063));
#40039=CARTESIAN_POINT('Ctrl Pts',(1.40164708205345,-1.,-1.23434087289768));
#40040=CARTESIAN_POINT('Ctrl Pts',(1.40845295531151,-1.,-1.23994455029421));
#40041=CARTESIAN_POINT('Ctrl Pts',(1.41422913175437,-1.,-1.24450600513278));
#40042=CARTESIAN_POINT('Ctrl Pts',(1.41923722596421,-1.,-1.24824430986911));
#40043=CARTESIAN_POINT('Ctrl Pts',(1.42378102115911,-1.,-1.25141455570299));
#40044=CARTESIAN_POINT('Ctrl Pts',(1.42815938799555,-1.,-1.25426945222783));
#40045=CARTESIAN_POINT('Ctrl Pts',(1.43262645609679,-1.,-1.25702687965744));
#40046=CARTESIAN_POINT('Ctrl Pts',(1.43734919180719,-1.,-1.25983531011894));
#40047=CARTESIAN_POINT('Ctrl Pts',(1.44236470511145,-1.,-1.26273903323723));
#40048=CARTESIAN_POINT('Ctrl Pts',(1.44761985001544,-1.,-1.26570925118767));
#40049=CARTESIAN_POINT('Ctrl Pts',(1.45301422764205,-1.,-1.26867786804854));
#40050=CARTESIAN_POINT('Ctrl Pts',(1.45843906294725,-1.,-1.27156805265312));
#40051=CARTESIAN_POINT('Ctrl Pts',(1.4638243133254,-1.,-1.27433119897877));
#40052=CARTESIAN_POINT('Ctrl Pts',(1.46916035917197,-1.,-1.27696414831144));
#40053=CARTESIAN_POINT('Ctrl Pts',(1.4744717526711,-1.,-1.27948918248524));
#40054=CARTESIAN_POINT('Ctrl Pts',(1.47980070347102,-1.,-1.28194158939522));
#40055=CARTESIAN_POINT('Ctrl Pts',(1.48518817118891,-1.,-1.28435533880184));
#40056=CARTESIAN_POINT('Ctrl Pts',(1.4906522831275,-1.,-1.28674676116415));
#40057=CARTESIAN_POINT('Ctrl Pts',(1.49618896881729,-1.,-1.28911506584232));
#40058=CARTESIAN_POINT('Ctrl Pts',(1.50178230149764,-1.,-1.29145022885171));
#40059=CARTESIAN_POINT('Ctrl Pts',(1.50741159078367,-1.,-1.29373841372843));
#40060=CARTESIAN_POINT('Ctrl Pts',(1.51305994241412,-1.,-1.29596850710518));
#40061=CARTESIAN_POINT('Ctrl Pts',(1.51872184912735,-1.,-1.29813791800757));
#40062=CARTESIAN_POINT('Ctrl Pts',(1.5243995786107,-1.,-1.30024984366334));
#40063=CARTESIAN_POINT('Ctrl Pts',(1.53009970283893,-1.,-1.3023106439557));
#40064=CARTESIAN_POINT('Ctrl Pts',(1.53582981268976,-1.,-1.30432735639487));
#40065=CARTESIAN_POINT('Ctrl Pts',(1.54159462645428,-1.,-1.30630475189553));
#40066=CARTESIAN_POINT('Ctrl Pts',(1.54739413957183,-1.,-1.30824393907471));
#40067=CARTESIAN_POINT('Ctrl Pts',(1.55322568759481,-1.,-1.31014393684221));
#40068=CARTESIAN_POINT('Ctrl Pts',(1.55908521254822,-1.,-1.31200264341696));
#40069=CARTESIAN_POINT('Ctrl Pts',(1.56496872402352,-1.,-1.31381795281002));
#40070=CARTESIAN_POINT('Ctrl Pts',(1.57087397835721,-1.,-1.31558903860015));
#40071=CARTESIAN_POINT('Ctrl Pts',(1.57680056505585,-1.,-1.31731642317183));
#40072=CARTESIAN_POINT('Ctrl Pts',(1.58274907898829,-1.,-1.31900135021428));
#40073=CARTESIAN_POINT('Ctrl Pts',(1.58872057258244,-1.,-1.32064537110891));
#40074=CARTESIAN_POINT('Ctrl Pts',(1.59471591079408,-1.,-1.32224985747686));
#40075=CARTESIAN_POINT('Ctrl Pts',(1.600735118587,-1.,-1.32381550858266));
#40076=CARTESIAN_POINT('Ctrl Pts',(1.6067775829097,-1.,-1.32534250785794));
#40077=CARTESIAN_POINT('Ctrl Pts',(1.61284234015762,-1.,-1.32683074483365));
#40078=CARTESIAN_POINT('Ctrl Pts',(1.61892832270723,-1.,-1.32828000610448));
#40079=CARTESIAN_POINT('Ctrl Pts',(1.62503464209777,-1.,-1.32969019505665));
#40080=CARTESIAN_POINT('Ctrl Pts',(1.63116079730887,-1.,-1.33106149345618));
#40081=CARTESIAN_POINT('Ctrl Pts',(1.63730653475049,-1.,-1.33239425103694));
#40082=CARTESIAN_POINT('Ctrl Pts',(1.64347174856007,-1.,-1.33368890676554));
#40083=CARTESIAN_POINT('Ctrl Pts',(1.64965637286843,-1.,-1.33494590468003));
#40084=CARTESIAN_POINT('Ctrl Pts',(1.65586025952651,-1.,-1.33616559745217));
#40085=CARTESIAN_POINT('Ctrl Pts',(1.66208312542073,-1.,-1.33734820885331));
#40086=CARTESIAN_POINT('Ctrl Pts',(1.66832460784078,-1.,-1.33849388654458));
#40087=CARTESIAN_POINT('Ctrl Pts',(1.67458429426126,-1.,-1.33960273470372));
#40088=CARTESIAN_POINT('Ctrl Pts',(1.68086176030308,-1.,-1.3406748518516));
#40089=CARTESIAN_POINT('Ctrl Pts',(1.68715660868602,-1.,-1.34171037484673));
#40090=CARTESIAN_POINT('Ctrl Pts',(1.6934684849664,-1.,-1.34270948206139));
#40091=CARTESIAN_POINT('Ctrl Pts',(1.69979707754221,-1.,-1.34367237124322));
#40092=CARTESIAN_POINT('Ctrl Pts',(1.70614212266676,-1.,-1.34459924533783));
#40093=CARTESIAN_POINT('Ctrl Pts',(1.71250340687011,-1.,-1.34549029589563));
#40094=CARTESIAN_POINT('Ctrl Pts',(1.7188807715095,-1.,-1.34634568653586));
#40095=CARTESIAN_POINT('Ctrl Pts',(1.72527410681298,-1.,-1.34716554820013));
#40096=CARTESIAN_POINT('Ctrl Pts',(1.73040149654497,-1.,-1.3477930915247));
#40097=CARTESIAN_POINT('Ctrl Pts',(1.73425417886254,-1.,-1.34824783113158));
#40098=CARTESIAN_POINT('Ctrl Pts',(1.73682580585819,-1.,-1.34854391898145));
#40099=CARTESIAN_POINT('Ctrl Pts',(1.73811241238545,-1.,-1.34869019493419));
#40100=CARTESIAN_POINT('',(1.81978687191668,-1.,-1.23627494547115));
#40101=CARTESIAN_POINT('',(1.73811241238545,-1.,-1.34869019493419));
#40102=CARTESIAN_POINT('',(1.5055822144029,-1.,-0.892032620296855));
#40103=CARTESIAN_POINT('Ctrl Pts',(1.81978687191668,-1.,-1.23627494547115));
#40104=CARTESIAN_POINT('Ctrl Pts',(1.81925017193531,-1.,-1.23509651170384));
#40105=CARTESIAN_POINT('Ctrl Pts',(1.81817389920914,-1.,-1.23274224526804));
#40106=CARTESIAN_POINT('Ctrl Pts',(1.81655087183054,-1.,-1.22921864890975));
#40107=CARTESIAN_POINT('Ctrl Pts',(1.81436959209778,-1.,-1.22453613304507));
#40108=CARTESIAN_POINT('Ctrl Pts',(1.81161420806172,-1.,-1.2187090610323));
#40109=CARTESIAN_POINT('Ctrl Pts',(1.80882996916931,-1.,-1.2129081570818));
#40110=CARTESIAN_POINT('Ctrl Pts',(1.80601678480772,-1.,-1.20713356605519));
#40111=CARTESIAN_POINT('Ctrl Pts',(1.8031745483882,-1.,-1.2013854893912));
#40112=CARTESIAN_POINT('Ctrl Pts',(1.80030314370121,-1.,-1.19566418930405));
#40113=CARTESIAN_POINT('Ctrl Pts',(1.79740245923649,-1.,-1.1899699793456));
#40114=CARTESIAN_POINT('Ctrl Pts',(1.79447240321572,-1.,-1.18430321697471));
#40115=CARTESIAN_POINT('Ctrl Pts',(1.79151291552646,-1.,-1.17866429440781));
#40116=CARTESIAN_POINT('Ctrl Pts',(1.78852398877523,-1.,-1.17305363177265));
#40117=CARTESIAN_POINT('Ctrl Pts',(1.78550566040349,-1.,-1.16747166312239));
#40118=CARTESIAN_POINT('Ctrl Pts',(1.78245795880949,-1.,-1.16191881298458));
#40119=CARTESIAN_POINT('Ctrl Pts',(1.77938085564261,-1.,-1.15639547194689));
#40120=CARTESIAN_POINT('Ctrl Pts',(1.77627422557034,-1.,-1.15090197841531));
#40121=CARTESIAN_POINT('Ctrl Pts',(1.77313777896234,-1.,-1.14543858226948));
#40122=CARTESIAN_POINT('Ctrl Pts',(1.76997111386806,-1.,-1.14000548337));
#40123=CARTESIAN_POINT('Ctrl Pts',(1.76677384551883,-1.,-1.13460291804635));
#40124=CARTESIAN_POINT('Ctrl Pts',(1.76354571966171,-1.,-1.12923123555076));
#40125=CARTESIAN_POINT('Ctrl Pts',(1.76028671825084,-1.,-1.12389096855078));
#40126=CARTESIAN_POINT('Ctrl Pts',(1.75699720772089,-1.,-1.11858293216752));
#40127=CARTESIAN_POINT('Ctrl Pts',(1.75367772094617,-1.,-1.11330807582542));
#40128=CARTESIAN_POINT('Ctrl Pts',(1.75032866075914,-1.,-1.10806728183003));
#40129=CARTESIAN_POINT('Ctrl Pts',(1.74695004214924,-1.,-1.10286118991144));
#40130=CARTESIAN_POINT('Ctrl Pts',(1.74354119236212,-1.,-1.09768999241229));
#40131=CARTESIAN_POINT('Ctrl Pts',(1.74010053962252,-1.,-1.09255329056496));
#40132=CARTESIAN_POINT('Ctrl Pts',(1.73662628326093,-1.,-1.08745056285429));
#40133=CARTESIAN_POINT('Ctrl Pts',(1.73311705663407,-1.,-1.08238162784749));
#40134=CARTESIAN_POINT('Ctrl Pts',(1.72957248977424,-1.,-1.0773470373727));
#40135=CARTESIAN_POINT('Ctrl Pts',(1.72599406198489,-1.,-1.07234866990252));
#40136=CARTESIAN_POINT('Ctrl Pts',(1.72238500928456,-1.,-1.06738966975463));
#40137=CARTESIAN_POINT('Ctrl Pts',(1.71874858456908,-1.,-1.0624732468065));
#40138=CARTESIAN_POINT('Ctrl Pts',(1.71508654427022,-1.,-1.05760163192481));
#40139=CARTESIAN_POINT('Ctrl Pts',(1.71139783543986,-1.,-1.05277517202854));
#40140=CARTESIAN_POINT('Ctrl Pts',(1.70767646263641,-1.,-1.0479908540499));
#40141=CARTESIAN_POINT('Ctrl Pts',(1.70391338707969,-1.,-1.04324363334546));
#40142=CARTESIAN_POINT('Ctrl Pts',(1.70010052930951,-1.,-1.03852922490782));
#40143=CARTESIAN_POINT('Ctrl Pts',(1.69623414782769,-1.,-1.03384646003587));
#40144=CARTESIAN_POINT('Ctrl Pts',(1.69231840863471,-1.,-1.02919977579155));
#40145=CARTESIAN_POINT('Ctrl Pts',(1.68836910178475,-1.,-1.02460180535272));
#40146=CARTESIAN_POINT('Ctrl Pts',(1.68440578021739,-1.,-1.02006795074222));
#40147=CARTESIAN_POINT('Ctrl Pts',(1.6804428989482,-1.,-1.01561026162787));
#40148=CARTESIAN_POINT('Ctrl Pts',(1.67648246776457,-1.,-1.01123236493507));
#40149=CARTESIAN_POINT('Ctrl Pts',(1.67250335383248,-1.,-1.00692206696387));
#40150=CARTESIAN_POINT('Ctrl Pts',(1.66846059277231,-1.,-1.00265091003682));
#40151=CARTESIAN_POINT('Ctrl Pts',(1.66430758030304,-1.,-0.998389654952317));
#40152=CARTESIAN_POINT('Ctrl Pts',(1.66001553809916,-1.,-0.994121836661116));
#40153=CARTESIAN_POINT('Ctrl Pts',(1.65559044289746,-1.,-0.98985562785445));
#40154=CARTESIAN_POINT('Ctrl Pts',(1.6511001661277,-1.,-0.985642622921626));
#40155=CARTESIAN_POINT('Ctrl Pts',(1.64665139190834,-1.,-0.981562530940574));
#40156=CARTESIAN_POINT('Ctrl Pts',(1.64233990826831,-1.,-0.977689794120297));
#40157=CARTESIAN_POINT('Ctrl Pts',(1.63820952658157,-1.,-0.974066058287501));
#40158=CARTESIAN_POINT('Ctrl Pts',(1.63420665729609,-1.,-0.970669715996356));
#40159=CARTESIAN_POINT('Ctrl Pts',(1.63013849959083,-1.,-0.967387853228041));
#40160=CARTESIAN_POINT('Ctrl Pts',(1.6257193066974,-1.,-0.964046107037821));
#40161=CARTESIAN_POINT('Ctrl Pts',(1.62061638139929,-1.,-0.960438326099958));
#40162=CARTESIAN_POINT('Ctrl Pts',(1.61449324337233,-1.,-0.956354422921573));
#40163=CARTESIAN_POINT('Ctrl Pts',(1.60706069897794,-1.,-0.951613284361248));
#40164=CARTESIAN_POINT('Ctrl Pts',(1.59810042045408,-1.,-0.946078063325796));
#40165=CARTESIAN_POINT('Ctrl Pts',(1.58744937489796,-1.,-0.939646377909319));
#40166=CARTESIAN_POINT('Ctrl Pts',(1.57499388385561,-1.,-0.932246680128849));
#40167=CARTESIAN_POINT('Ctrl Pts',(1.56065988582509,-1.,-0.923832188966322));
#40168=CARTESIAN_POINT('Ctrl Pts',(1.54440491152807,-1.,-0.91437591904658));
#40169=CARTESIAN_POINT('Ctrl Pts',(1.52984849890434,-1.,-0.905967409640499));
#40170=CARTESIAN_POINT('Ctrl Pts',(1.51805569591479,-1.,-0.89918504749193));
#40171=CARTESIAN_POINT('Ctrl Pts',(1.50980486807181,-1.,-0.894452006967538));
#40172=CARTESIAN_POINT('Ctrl Pts',(1.5055822144029,-1.,-0.892032620296855));
#40173=CARTESIAN_POINT('',(1.60662857109684,-1.,-0.693717979106306));
#40174=CARTESIAN_POINT('Origin',(0.,-1.,0.));
#40175=CARTESIAN_POINT('',(2.0698113262342,-1.,-0.745574324794401));
#40176=CARTESIAN_POINT('Ctrl Pts',(1.60662857109684,-1.,-0.693717979106306));
#40177=CARTESIAN_POINT('Ctrl Pts',(1.61106790957619,-1.,-0.69571209787897));
#40178=CARTESIAN_POINT('Ctrl Pts',(1.61974673471117,-1.,-0.699605146398837));
#40179=CARTESIAN_POINT('Ctrl Pts',(1.6321654166204,-1.,-0.705159151977294));
#40180=CARTESIAN_POINT('Ctrl Pts',(1.64752408828442,-1.,-0.711993139340448));
#40181=CARTESIAN_POINT('Ctrl Pts',(1.66472880551777,-1.,-0.71958543378795));
#40182=CARTESIAN_POINT('Ctrl Pts',(1.67996158451922,-1.,-0.726235967982445));
#40183=CARTESIAN_POINT('Ctrl Pts',(1.69326921972915,-1.,-0.731963238685357));
#40184=CARTESIAN_POINT('Ctrl Pts',(1.70473309004249,-1.,-0.736799665716932));
#40185=CARTESIAN_POINT('Ctrl Pts',(1.71447789751001,-1.,-0.74079516202821));
#40186=CARTESIAN_POINT('Ctrl Pts',(1.72268229916769,-1.,-0.744021445433094));
#40187=CARTESIAN_POINT('Ctrl Pts',(1.72958533647714,-1.,-0.746574710097752));
#40188=CARTESIAN_POINT('Ctrl Pts',(1.7355035168033,-1.,-0.74858246295687));
#40189=CARTESIAN_POINT('Ctrl Pts',(1.74080458267114,-1.,-0.75019343598125));
#40190=CARTESIAN_POINT('Ctrl Pts',(1.74585086852502,-1.,-0.751555614164483));
#40191=CARTESIAN_POINT('Ctrl Pts',(1.75095139468794,-1.,-0.752797683531314));
#40192=CARTESIAN_POINT('Ctrl Pts',(1.75631083600019,-1.,-0.754009254027829));
#40193=CARTESIAN_POINT('Ctrl Pts',(1.76197817240128,-1.,-0.755220979974462));
#40194=CARTESIAN_POINT('Ctrl Pts',(1.76789396002998,-1.,-0.75642189602781));
#40195=CARTESIAN_POINT('Ctrl Pts',(1.77394167108292,-1.,-0.757578264077029));
#40196=CARTESIAN_POINT('Ctrl Pts',(1.77999411220945,-1.,-0.758650626677519));
#40197=CARTESIAN_POINT('Ctrl Pts',(1.78596964884604,-1.,-0.75961440111019));
#40198=CARTESIAN_POINT('Ctrl Pts',(1.7918581561088,-1.,-0.760469555880749));
#40199=CARTESIAN_POINT('Ctrl Pts',(1.79768986997783,-1.,-0.761229695230558));
#40200=CARTESIAN_POINT('Ctrl Pts',(1.80351583877342,-1.,-0.761915336443547));
#40201=CARTESIAN_POINT('Ctrl Pts',(1.80938551463965,-1.,-0.762546129463938));
#40202=CARTESIAN_POINT('Ctrl Pts',(1.8153211840553,-1.,-0.763132003836634));
#40203=CARTESIAN_POINT('Ctrl Pts',(1.82131873145266,-1.,-0.763673465462727));
#40204=CARTESIAN_POINT('Ctrl Pts',(1.82735991200065,-1.,-0.764165902605995));
#40205=CARTESIAN_POINT('Ctrl Pts',(1.83342077227142,-1.,-0.764602549687853));
#40206=CARTESIAN_POINT('Ctrl Pts',(1.83948181064835,-1.,-0.764978057881738));
#40207=CARTESIAN_POINT('Ctrl Pts',(1.84553698875924,-1.,-0.765291664862029));
#40208=CARTESIAN_POINT('Ctrl Pts',(1.85158945130063,-1.,-0.765545710619063));
#40209=CARTESIAN_POINT('Ctrl Pts',(1.85764741390394,-1.,-0.765744212909319));
#40210=CARTESIAN_POINT('Ctrl Pts',(1.86372027063312,-1.,-0.765891519092547));
#40211=CARTESIAN_POINT('Ctrl Pts',(1.86981398314341,-1.,-0.765990708546091));
#40212=CARTESIAN_POINT('Ctrl Pts',(1.87592888967883,-1.,-0.766042837036744));
#40213=CARTESIAN_POINT('Ctrl Pts',(1.88206215302561,-1.,-0.766047794851865));
#40214=CARTESIAN_POINT('Ctrl Pts',(1.88820926433409,-1.,-0.766004837062091));
#40215=CARTESIAN_POINT('Ctrl Pts',(1.89436577771388,-1.,-0.765913193856978));
#40216=CARTESIAN_POINT('Ctrl Pts',(1.90052930393596,-1.,-0.765772772593386));
#40217=CARTESIAN_POINT('Ctrl Pts',(1.90669961402356,-1.,-0.765584196937919));
#40218=CARTESIAN_POINT('Ctrl Pts',(1.91287765805169,-1.,-0.765348465884722));
#40219=CARTESIAN_POINT('Ctrl Pts',(1.91906491634196,-1.,-0.765066729667089));
#40220=CARTESIAN_POINT('Ctrl Pts',(1.92526263537048,-1.,-0.764740025488212));
#40221=CARTESIAN_POINT('Ctrl Pts',(1.93147105496382,-1.,-0.764369010673941));
#40222=CARTESIAN_POINT('Ctrl Pts',(1.93768964875886,-1.,-0.763954049121459));
#40223=CARTESIAN_POINT('Ctrl Pts',(1.9439174661764,-1.,-0.763495333538629));
#40224=CARTESIAN_POINT('Ctrl Pts',(1.95015342590024,-1.,-0.762992990878769));
#40225=CARTESIAN_POINT('Ctrl Pts',(1.95639665309869,-1.,-0.762447203806179));
#40226=CARTESIAN_POINT('Ctrl Pts',(1.96264672744186,-1.,-0.761858300014424));
#40227=CARTESIAN_POINT('Ctrl Pts',(1.96890351582499,-1.,-0.761226690483821));
#40228=CARTESIAN_POINT('Ctrl Pts',(1.97516705321494,-1.,-0.760552825409757));
#40229=CARTESIAN_POINT('Ctrl Pts',(1.98143741418172,-1.,-0.75983714745219));
#40230=CARTESIAN_POINT('Ctrl Pts',(1.98771456680874,-1.,-0.759080037802488));
#40231=CARTESIAN_POINT('Ctrl Pts',(1.99399831098817,-1.,-0.758281796766761));
#40232=CARTESIAN_POINT('Ctrl Pts',(2.00028834739178,-1.,-0.757442676862724));
#40233=CARTESIAN_POINT('Ctrl Pts',(2.0065843158773,-1.,-0.756562904646671));
#40234=CARTESIAN_POINT('Ctrl Pts',(2.01288584328084,-1.,-0.755642704957865));
#40235=CARTESIAN_POINT('Ctrl Pts',(2.01919259405809,-1.,-0.754682330722816));
#40236=CARTESIAN_POINT('Ctrl Pts',(2.02550428623313,-1.,-0.753682061112768));
#40237=CARTESIAN_POINT('Ctrl Pts',(2.03182068456221,-1.,-0.752642180487211));
#40238=CARTESIAN_POINT('Ctrl Pts',(2.03814160092099,-1.,-0.751562963361115));
#40239=CARTESIAN_POINT('Ctrl Pts',(2.04446689147979,-1.,-0.750444657875576));
#40240=CARTESIAN_POINT('Ctrl Pts',(2.05079645592154,-1.,-0.749287468665046));
#40241=CARTESIAN_POINT('Ctrl Pts',(2.05713023031006,-1.,-0.748091554183803));
#40242=CARTESIAN_POINT('Ctrl Pts',(2.06220058927826,-1.,-0.74710393278792));
#40243=CARTESIAN_POINT('Ctrl Pts',(2.06600523016815,-1.,-0.746345871544201));
#40244=CARTESIAN_POINT('Ctrl Pts',(2.06854248895728,-1.,-0.745832791378367));
#40245=CARTESIAN_POINT('Ctrl Pts',(2.0698113262342,-1.,-0.745574324794401));
#40246=CARTESIAN_POINT('',(2.11275013067528,-1.,-0.61342227326009));
#40247=CARTESIAN_POINT('',(2.0698113262342,-1.,-0.745574324794401));
#40248=CARTESIAN_POINT('',(1.7075470150345,-1.,-0.383122945602004));
#40249=CARTESIAN_POINT('Ctrl Pts',(2.11275013067528,-1.,-0.61342227326009));
#40250=CARTESIAN_POINT('Ctrl Pts',(2.11187554259986,-1.,-0.6124673655618));
#40251=CARTESIAN_POINT('Ctrl Pts',(2.11012443807238,-1.,-0.610560911689899));
#40252=CARTESIAN_POINT('Ctrl Pts',(2.1074919961518,-1.,-0.607711315454876));
#40253=CARTESIAN_POINT('Ctrl Pts',(2.10397049886949,-1.,-0.60393203073603));
#40254=CARTESIAN_POINT('Ctrl Pts',(2.0995493086477,-1.,-0.599241616420534));
#40255=CARTESIAN_POINT('Ctrl Pts',(2.0951087622027,-1.,-0.594585006052162));
#40256=CARTESIAN_POINT('Ctrl Pts',(2.09064881812129,-1.,-0.589962365403406));
#40257=CARTESIAN_POINT('Ctrl Pts',(2.08616943727951,-1.,-0.585373918991617));
#40258=CARTESIAN_POINT('Ctrl Pts',(2.08167059018418,-1.,-0.580819952108064));
#40259=CARTESIAN_POINT('Ctrl Pts',(2.07715226767559,-1.,-0.576300797416845));
#40260=CARTESIAN_POINT('Ctrl Pts',(2.07261449292824,-1.,-0.571816823242603));
#40261=CARTESIAN_POINT('Ctrl Pts',(2.06805732997334,-1.,-0.567368421181087));
#40262=CARTESIAN_POINT('Ctrl Pts',(2.06348090160589,-1.,-0.562955993082262));
#40263=CARTESIAN_POINT('Ctrl Pts',(2.05888537756462,-1.,-0.558579940185152));
#40264=CARTESIAN_POINT('Ctrl Pts',(2.05427091604413,-1.,-0.554240657463906));
#40265=CARTESIAN_POINT('Ctrl Pts',(2.04963761077958,-1.,-0.549938525150295));
#40266=CARTESIAN_POINT('Ctrl Pts',(2.04498544714588,-1.,-0.54567390381743));
#40267=CARTESIAN_POINT('Ctrl Pts',(2.04031422690527,-1.,-0.541447120615659));
#40268=CARTESIAN_POINT('Ctrl Pts',(2.03562362954037,-1.,-0.537258489833262));
#40269=CARTESIAN_POINT('Ctrl Pts',(2.03091336214426,-1.,-0.533108355132977));
#40270=CARTESIAN_POINT('Ctrl Pts',(2.0261832908329,-1.,-0.528997127241914));
#40271=CARTESIAN_POINT('Ctrl Pts',(2.02143356304698,-1.,-0.524925318333476));
#40272=CARTESIAN_POINT('Ctrl Pts',(2.01666477917286,-1.,-0.520893590399371));
#40273=CARTESIAN_POINT('Ctrl Pts',(2.01187773939242,-1.,-0.516902681728687));
#40274=CARTESIAN_POINT('Ctrl Pts',(2.00707309946949,-1.,-0.512953306961793));
#40275=CARTESIAN_POINT('Ctrl Pts',(2.00225107134734,-1.,-0.509046069886157));
#40276=CARTESIAN_POINT('Ctrl Pts',(1.99741107463572,-1.,-0.505181361323026));
#40277=CARTESIAN_POINT('Ctrl Pts',(1.99255149126155,-1.,-0.501359287727146));
#40278=CARTESIAN_POINT('Ctrl Pts',(1.98767044752932,-1.,-0.497579909545574));
#40279=CARTESIAN_POINT('Ctrl Pts',(1.98276658761821,-1.,-0.493843476541495));
#40280=CARTESIAN_POINT('Ctrl Pts',(1.97783973019229,-1.,-0.490150627860953));
#40281=CARTESIAN_POINT('Ctrl Pts',(1.97289186263272,-1.,-0.486502692907659));
#40282=CARTESIAN_POINT('Ctrl Pts',(1.96792703422362,-1.,-0.482901662120691));
#40283=CARTESIAN_POINT('Ctrl Pts',(1.96294933055943,-1.,-0.479349583074855));
#40284=CARTESIAN_POINT('Ctrl Pts',(1.95796111148177,-1.,-0.475848034683176));
#40285=CARTESIAN_POINT('Ctrl Pts',(1.95296148278133,-1.,-0.472397672264072));
#40286=CARTESIAN_POINT('Ctrl Pts',(1.94794381136514,-1.,-0.468997482913135));
#40287=CARTESIAN_POINT('Ctrl Pts',(1.9428979419619,-1.,-0.46564546202603));
#40288=CARTESIAN_POINT('Ctrl Pts',(1.93781486640821,-1.,-0.462340031009057));
#40289=CARTESIAN_POINT('Ctrl Pts',(1.93269066517934,-1.,-0.459081234547926));
#40290=CARTESIAN_POINT('Ctrl Pts',(1.92753067150476,-1.,-0.455872005174371));
#40291=CARTESIAN_POINT('Ctrl Pts',(1.92235380648502,-1.,-0.452719478359433));
#40292=CARTESIAN_POINT('Ctrl Pts',(1.91718342555755,-1.,-0.449632260106662));
#40293=CARTESIAN_POINT('Ctrl Pts',(1.9120369998112,-1.,-0.446617343485711));
#40294=CARTESIAN_POINT('Ctrl Pts',(1.90691756144898,-1.,-0.443677556849151));
#40295=CARTESIAN_POINT('Ctrl Pts',(1.90180124389086,-1.,-0.440807833704038));
#40296=CARTESIAN_POINT('Ctrl Pts',(1.89663648956466,-1.,-0.437995003948244));
#40297=CARTESIAN_POINT('Ctrl Pts',(1.89136993975504,-1.,-0.435225660963383));
#40298=CARTESIAN_POINT('Ctrl Pts',(1.88596913666793,-1.,-0.432493038548748));
#40299=CARTESIAN_POINT('Ctrl Pts',(1.88044229001832,-1.,-0.429803062482345));
#40300=CARTESIAN_POINT('Ctrl Pts',(1.87486989291484,-1.,-0.427183828519102));
#40301=CARTESIAN_POINT('Ctrl Pts',(1.86937803944323,-1.,-0.424678177291359));
#40302=CARTESIAN_POINT('Ctrl Pts',(1.86408083334028,-1.,-0.422327307418275));
#40303=CARTESIAN_POINT('Ctrl Pts',(1.85903281096686,-1.,-0.42015728797562));
#40304=CARTESIAN_POINT('Ctrl Pts',(1.85417632856234,-1.,-0.418164129143534));
#40305=CARTESIAN_POINT('Ctrl Pts',(1.84929312929882,-1.,-0.416300022038864));
#40306=CARTESIAN_POINT('Ctrl Pts',(1.8440575707371,-1.,-0.41448743825434));
#40307=CARTESIAN_POINT('Ctrl Pts',(1.83808953475839,-1.,-0.412633125322162));
#40308=CARTESIAN_POINT('Ctrl Pts',(1.83100408895216,-1.,-0.410641256301675));
#40309=CARTESIAN_POINT('Ctrl Pts',(1.8224702267854,-1.,-0.408428948108534));
#40310=CARTESIAN_POINT('Ctrl Pts',(1.81223801813988,-1.,-0.405933518411838));
#40311=CARTESIAN_POINT('Ctrl Pts',(1.80012077176221,-1.,-0.403107976170441));
#40312=CARTESIAN_POINT('Ctrl Pts',(1.78598826347533,-1.,-0.399919403783081));
#40313=CARTESIAN_POINT('Ctrl Pts',(1.7697556004756,-1.,-0.39634619612042));
#40314=CARTESIAN_POINT('Ctrl Pts',(1.75137405313962,-1.,-0.392375812294307));
#40315=CARTESIAN_POINT('Ctrl Pts',(1.7349317097561,-1.,-0.388877023509192));
#40316=CARTESIAN_POINT('Ctrl Pts',(1.72162022246158,-1.,-0.38607079032701));
#40317=CARTESIAN_POINT('Ctrl Pts',(1.71231062891958,-1.,-0.384119047315542));
#40318=CARTESIAN_POINT('Ctrl Pts',(1.7075470150345,-1.,-0.383122945602004));
#40319=CARTESIAN_POINT('',(1.74236521665491,-1.,-0.163289472382896));
#40320=CARTESIAN_POINT('Origin',(0.,-1.,0.));
#40321=CARTESIAN_POINT('',(2.19890268624765,-1.,-0.0694764450219582));
#40322=CARTESIAN_POINT('Ctrl Pts',(1.74236521665491,-1.,-0.163289472382896));
#40323=CARTESIAN_POINT('Ctrl Pts',(1.7472034950333,-1.,-0.163814161002002));
#40324=CARTESIAN_POINT('Ctrl Pts',(1.75666056638427,-1.,-0.164834765707159));
#40325=CARTESIAN_POINT('Ctrl Pts',(1.77018771684844,-1.,-0.1662793551464));
#40326=CARTESIAN_POINT('Ctrl Pts',(1.7869064998507,-1.,-0.168032772805197));
#40327=CARTESIAN_POINT('Ctrl Pts',(1.80561530629706,-1.,-0.169936923904608));
#40328=CARTESIAN_POINT('Ctrl Pts',(1.82215766811545,-1.,-0.171554770204119));
#40329=CARTESIAN_POINT('Ctrl Pts',(1.83658380527692,-1.,-0.1728894428919));
#40330=CARTESIAN_POINT('Ctrl Pts',(1.8489811319852,-1.,-0.173946627587732));
#40331=CARTESIAN_POINT('Ctrl Pts',(1.85948367088837,-1.,-0.17473525927603));
#40332=CARTESIAN_POINT('Ctrl Pts',(1.86828349694799,-1.,-0.175268337590758));
#40333=CARTESIAN_POINT('Ctrl Pts',(1.87563767773588,-1.,-0.175563480746485));
#40334=CARTESIAN_POINT('Ctrl Pts',(1.88188663145367,-1.,-0.175644148889699));
#40335=CARTESIAN_POINT('Ctrl Pts',(1.88742606273259,-1.,-0.175538155840648));
#40336=CARTESIAN_POINT('Ctrl Pts',(1.892646301985,-1.,-0.175274276190844));
#40337=CARTESIAN_POINT('Ctrl Pts',(1.89788101117132,-1.,-0.174879405091263));
#40338=CARTESIAN_POINT('Ctrl Pts',(1.90335253862834,-1.,-0.174375518661085));
#40339=CARTESIAN_POINT('Ctrl Pts',(1.90911693975267,-1.,-0.173776635257817));
#40340=CARTESIAN_POINT('Ctrl Pts',(1.91511429159527,-1.,-0.173090695383496));
#40341=CARTESIAN_POINT('Ctrl Pts',(1.9212233439798,-1.,-0.172321621259514));
#40342=CARTESIAN_POINT('Ctrl Pts',(1.92731093582036,-1.,-0.171471191532988));
#40343=CARTESIAN_POINT('Ctrl Pts',(1.93329183155539,-1.,-0.170541253116202));
#40344=CARTESIAN_POINT('Ctrl Pts',(1.93915639211581,-1.,-0.169534904817491));
#40345=CARTESIAN_POINT('Ctrl Pts',(1.94493757756931,-1.,-0.168455741607556));
#40346=CARTESIAN_POINT('Ctrl Pts',(1.95069027794294,-1.,-0.167307501784476));
#40347=CARTESIAN_POINT('Ctrl Pts',(1.9564675971873,-1.,-0.166093592002813));
#40348=CARTESIAN_POINT('Ctrl Pts',(1.96229379940136,-1.,-0.164816568920269));
#40349=CARTESIAN_POINT('Ctrl Pts',(1.96816512677967,-1.,-0.163478185457734));
#40350=CARTESIAN_POINT('Ctrl Pts',(1.97406280235188,-1.,-0.162079693556289));
#40351=CARTESIAN_POINT('Ctrl Pts',(1.97996195437559,-1.,-0.160622060784611));
#40352=CARTESIAN_POINT('Ctrl Pts',(1.98584238283292,-1.,-0.159106226437299));
#40353=CARTESIAN_POINT('Ctrl Pts',(1.99169810931908,-1.,-0.157533331459227));
#40354=CARTESIAN_POINT('Ctrl Pts',(1.99753284771497,-1.,-0.155904629548784));
#40355=CARTESIAN_POINT('Ctrl Pts',(2.00335565310543,-1.,-0.154221403049722));
#40356=CARTESIAN_POINT('Ctrl Pts',(2.00917680318424,-1.,-0.15248488362145));
#40357=CARTESIAN_POINT('Ctrl Pts',(2.01500291940238,-1.,-0.150696157673078));
#40358=CARTESIAN_POINT('Ctrl Pts',(2.02083464969894,-1.,-0.148856124775337));
#40359=CARTESIAN_POINT('Ctrl Pts',(2.02666926182017,-1.,-0.146965557332583));
#40360=CARTESIAN_POINT('Ctrl Pts',(2.03250223739942,-1.,-0.145025140186058));
#40361=CARTESIAN_POINT('Ctrl Pts',(2.03832911025912,-1.,-0.143035515058209));
#40362=CARTESIAN_POINT('Ctrl Pts',(2.04414757947916,-1.,-0.140997332152546));
#40363=CARTESIAN_POINT('Ctrl Pts',(2.04995762001328,-1.,-0.138911255368966));
#40364=CARTESIAN_POINT('Ctrl Pts',(2.05576044414264,-1.,-0.136777941218044));
#40365=CARTESIAN_POINT('Ctrl Pts',(2.06155781517842,-1.,-0.134598026192106));
#40366=CARTESIAN_POINT('Ctrl Pts',(2.06735123910326,-1.,-0.132372111547711));
#40367=CARTESIAN_POINT('Ctrl Pts',(2.07314114713063,-1.,-0.130100748328404));
#40368=CARTESIAN_POINT('Ctrl Pts',(2.07892715110987,-1.,-0.12778444527612));
#40369=CARTESIAN_POINT('Ctrl Pts',(2.08470840653643,-1.,-0.125423679412062));
#40370=CARTESIAN_POINT('Ctrl Pts',(2.09048392424825,-1.,-0.123018905621083));
#40371=CARTESIAN_POINT('Ctrl Pts',(2.0962529286773,-1.,-0.120570567965122));
#40372=CARTESIAN_POINT('Ctrl Pts',(2.102015121329,-1.,-0.118079107988356));
#40373=CARTESIAN_POINT('Ctrl Pts',(2.10777050261309,-1.,-0.115544957687927));
#40374=CARTESIAN_POINT('Ctrl Pts',(2.11351924490306,-1.,-0.112968534419737));
#40375=CARTESIAN_POINT('Ctrl Pts',(2.11926155590865,-1.,-0.110350236135025));
#40376=CARTESIAN_POINT('Ctrl Pts',(2.12499752307,-1.,-0.10769043523109));
#40377=CARTESIAN_POINT('Ctrl Pts',(2.13072704887293,-1.,-0.10498947915274));
#40378=CARTESIAN_POINT('Ctrl Pts',(2.13644992667165,-1.,-0.102247700556101));
#40379=CARTESIAN_POINT('Ctrl Pts',(2.14216588396025,-1.,-0.0994654261990917));
#40380=CARTESIAN_POINT('Ctrl Pts',(2.14787463531795,-1.,-0.096642985230546));
#40381=CARTESIAN_POINT('Ctrl Pts',(2.1535759397817,-1.,-0.0937807218867645));
#40382=CARTESIAN_POINT('Ctrl Pts',(2.15926961544516,-1.,-0.0908789888107267));
#40383=CARTESIAN_POINT('Ctrl Pts',(2.16495552645014,-1.,-0.0879381291386924));
#40384=CARTESIAN_POINT('Ctrl Pts',(2.17063357870952,-1.,-0.0849584620835374));
#40385=CARTESIAN_POINT('Ctrl Pts',(2.176303712113,-1.,-0.0819402680872767));
#40386=CARTESIAN_POINT('Ctrl Pts',(2.18196589448887,-1.,-0.0788837727685244));
#40387=CARTESIAN_POINT('Ctrl Pts',(2.1876201139953,-1.,-0.0757891465836149));
#40388=CARTESIAN_POINT('Ctrl Pts',(2.19213712013662,-1.,-0.0732830357306726));
#40389=CARTESIAN_POINT('Ctrl Pts',(2.19552129484002,-1.,-0.0713863779526155));
#40390=CARTESIAN_POINT('Ctrl Pts',(2.19777582085423,-1.,-0.0701143536325491));
#40391=CARTESIAN_POINT('Ctrl Pts',(2.19890268624765,-1.,-0.0694764450219582));
#40392=CARTESIAN_POINT('',(2.19890268624765,-1.,0.0694764450219582));
#40393=CARTESIAN_POINT('',(2.19890268624765,-1.,-0.0694764450219582));
#40394=CARTESIAN_POINT('',(1.74236521665491,-1.,0.163289472382896));
#40395=CARTESIAN_POINT('Ctrl Pts',(2.19890268624765,-1.,0.0694764450219582));
#40396=CARTESIAN_POINT('Ctrl Pts',(2.19777582085261,-1.,0.0701143536324925));
#40397=CARTESIAN_POINT('Ctrl Pts',(2.19552129483562,-1.,0.0713863779524626));
#40398=CARTESIAN_POINT('Ctrl Pts',(2.19213712012956,-1.,0.0732830357304275));
#40399=CARTESIAN_POINT('Ctrl Pts',(2.1876201139874,-1.,0.075789146583341));
#40400=CARTESIAN_POINT('Ctrl Pts',(2.18196589448304,-1.,0.0788837727683226));
#40401=CARTESIAN_POINT('Ctrl Pts',(2.1763037121106,-1.,0.0819402680871938));
#40402=CARTESIAN_POINT('Ctrl Pts',(2.17063357871031,-1.,0.0849584620835642));
#40403=CARTESIAN_POINT('Ctrl Pts',(2.16495552645275,-1.,0.0879381291387821));
#40404=CARTESIAN_POINT('Ctrl Pts',(2.15926961544808,-1.,0.0908789888108265));
#40405=CARTESIAN_POINT('Ctrl Pts',(2.15357593978377,-1.,0.0937807218868344));
#40406=CARTESIAN_POINT('Ctrl Pts',(2.14787463531864,-1.,0.0966429852305688));
#40407=CARTESIAN_POINT('Ctrl Pts',(2.14216588395974,-1.,0.0994654261990741));
#40408=CARTESIAN_POINT('Ctrl Pts',(2.13644992667052,-1.,0.102247700556063));
#40409=CARTESIAN_POINT('Ctrl Pts',(2.1307270488718,-1.,0.104989479152703));
#40410=CARTESIAN_POINT('Ctrl Pts',(2.12499752306927,-1.,0.107690435231068));
#40411=CARTESIAN_POINT('Ctrl Pts',(2.11926155590849,-1.,0.11035023613502));
#40412=CARTESIAN_POINT('Ctrl Pts',(2.11351924490335,-1.,0.112968534419746));
#40413=CARTESIAN_POINT('Ctrl Pts',(2.10777050261359,-1.,0.11554495768794));
#40414=CARTESIAN_POINT('Ctrl Pts',(2.10201512132945,-1.,0.118079107988368));
#40415=CARTESIAN_POINT('Ctrl Pts',(2.09625292867756,-1.,0.120570567965129));
#40416=CARTESIAN_POINT('Ctrl Pts',(2.09048392424826,-1.,0.123018905621083));
#40417=CARTESIAN_POINT('Ctrl Pts',(2.08470840653628,-1.,0.125423679412058));
#40418=CARTESIAN_POINT('Ctrl Pts',(2.07892715110967,-1.,0.127784445276116));
#40419=CARTESIAN_POINT('Ctrl Pts',(2.07314114713047,-1.,0.1301007483284));
#40420=CARTESIAN_POINT('Ctrl Pts',(2.06735123910319,-1.,0.132372111547709));
#40421=CARTESIAN_POINT('Ctrl Pts',(2.06155781517844,-1.,0.134598026192107));
#40422=CARTESIAN_POINT('Ctrl Pts',(2.0557604441427,-1.,0.136777941218044));
#40423=CARTESIAN_POINT('Ctrl Pts',(2.04995762001333,-1.,0.138911255368966));
#40424=CARTESIAN_POINT('Ctrl Pts',(2.04414757947919,-1.,0.140997332152545));
#40425=CARTESIAN_POINT('Ctrl Pts',(2.03832911025913,-1.,0.143035515058208));
#40426=CARTESIAN_POINT('Ctrl Pts',(2.03250223739941,-1.,0.145025140186058));
#40427=CARTESIAN_POINT('Ctrl Pts',(2.02666926182017,-1.,0.146965557332586));
#40428=CARTESIAN_POINT('Ctrl Pts',(2.02083464969897,-1.,0.148856124775342));
#40429=CARTESIAN_POINT('Ctrl Pts',(2.01500291940243,-1.,0.150696157673084));
#40430=CARTESIAN_POINT('Ctrl Pts',(2.00917680318426,-1.,0.152484883621452));
#40431=CARTESIAN_POINT('Ctrl Pts',(2.00335565310539,-1.,0.154221403049719));
#40432=CARTESIAN_POINT('Ctrl Pts',(1.99753284771487,-1.,0.155904629548774));
#40433=CARTESIAN_POINT('Ctrl Pts',(1.99169810931893,-1.,0.157533331459215));
#40434=CARTESIAN_POINT('Ctrl Pts',(1.98584238283279,-1.,0.159106226437288));
#40435=CARTESIAN_POINT('Ctrl Pts',(1.97996195437557,-1.,0.16062206078461));
#40436=CARTESIAN_POINT('Ctrl Pts',(1.97406280235204,-1.,0.162079693556302));
#40437=CARTESIAN_POINT('Ctrl Pts',(1.96816512678,-1.,0.16347818545776));
#40438=CARTESIAN_POINT('Ctrl Pts',(1.96229379940174,-1.,0.1648165689203));
#40439=CARTESIAN_POINT('Ctrl Pts',(1.95646759718755,-1.,0.166093592002832));
#40440=CARTESIAN_POINT('Ctrl Pts',(1.95069027794286,-1.,0.167307501784469));
#40441=CARTESIAN_POINT('Ctrl Pts',(1.94493757756879,-1.,0.168455741607515));
#40442=CARTESIAN_POINT('Ctrl Pts',(1.93915639211497,-1.,0.169534904817425));
#40443=CARTESIAN_POINT('Ctrl Pts',(1.93329183155455,-1.,0.170541253116136));
#40444=CARTESIAN_POINT('Ctrl Pts',(1.92731093582,-1.,0.17147119153296));
#40445=CARTESIAN_POINT('Ctrl Pts',(1.92122334398034,-1.,0.172321621259556));
#40446=CARTESIAN_POINT('Ctrl Pts',(1.91511429159681,-1.,0.173090695383619));
#40447=CARTESIAN_POINT('Ctrl Pts',(1.90911693975475,-1.,0.173776635257983));
#40448=CARTESIAN_POINT('Ctrl Pts',(1.90335253863003,-1.,0.174375518661222));
#40449=CARTESIAN_POINT('Ctrl Pts',(1.89788101117148,-1.,0.174879405091277));
#40450=CARTESIAN_POINT('Ctrl Pts',(1.89264630198279,-1.,0.175274276190664));
#40451=CARTESIAN_POINT('Ctrl Pts',(1.88742606272818,-1.,0.175538155840286));
#40452=CARTESIAN_POINT('Ctrl Pts',(1.88188663144846,-1.,0.175644148889271));
#40453=CARTESIAN_POINT('Ctrl Pts',(1.87563767773249,-1.,0.175563480746205));
#40454=CARTESIAN_POINT('Ctrl Pts',(1.86828349694972,-1.,0.1752683375909));
#40455=CARTESIAN_POINT('Ctrl Pts',(1.85948367089838,-1.,0.174735259276856));
#40456=CARTESIAN_POINT('Ctrl Pts',(1.84898113200543,-1.,0.173946627589401));
#40457=CARTESIAN_POINT('Ctrl Pts',(1.83658380530747,-1.,0.17288944289442));
#40458=CARTESIAN_POINT('Ctrl Pts',(1.82215766815414,-1.,0.171554770207306));
#40459=CARTESIAN_POINT('Ctrl Pts',(1.80561530633924,-1.,0.169936923908078));
#40460=CARTESIAN_POINT('Ctrl Pts',(1.78690649988931,-1.,0.16803277280837));
#40461=CARTESIAN_POINT('Ctrl Pts',(1.77018771687692,-1.,0.166279355148738));
#40462=CARTESIAN_POINT('Ctrl Pts',(1.75666056640041,-1.,0.164834765708484));
#40463=CARTESIAN_POINT('Ctrl Pts',(1.74720349503904,-1.,0.163814161002474));
#40464=CARTESIAN_POINT('Ctrl Pts',(1.74236521665491,-1.,0.163289472382896));
#40465=CARTESIAN_POINT('',(1.7075470150345,-1.,0.383122945602004));
#40466=CARTESIAN_POINT('Origin',(0.,-1.,0.));
#40467=CARTESIAN_POINT('',(2.11275013067528,-1.,0.613422273260091));
#40468=CARTESIAN_POINT('Ctrl Pts',(1.7075470150345,-1.,0.383122945602004));
#40469=CARTESIAN_POINT('Ctrl Pts',(1.71231062891398,-1.,0.384119047314215));
#40470=CARTESIAN_POINT('Ctrl Pts',(1.72162022244582,-1.,0.386070790323281));
#40471=CARTESIAN_POINT('Ctrl Pts',(1.73493170972829,-1.,0.388877023502615));
#40472=CARTESIAN_POINT('Ctrl Pts',(1.75137405310193,-1.,0.392375812285396));
#40473=CARTESIAN_POINT('Ctrl Pts',(1.76975560043442,-1.,0.396346196110688));
#40474=CARTESIAN_POINT('Ctrl Pts',(1.78598826343754,-1.,0.399919403774156));
#40475=CARTESIAN_POINT('Ctrl Pts',(1.80012077173238,-1.,0.403107976163396));
#40476=CARTESIAN_POINT('Ctrl Pts',(1.81223801812013,-1.,0.405933518407176));
#40477=CARTESIAN_POINT('Ctrl Pts',(1.82247022677562,-1.,0.408428948106228));
#40478=CARTESIAN_POINT('Ctrl Pts',(1.83100408895047,-1.,0.410641256301276));
#40479=CARTESIAN_POINT('Ctrl Pts',(1.8380895347617,-1.,0.412633125322945));
#40480=CARTESIAN_POINT('Ctrl Pts',(1.84405757074218,-1.,0.414487438255542));
#40481=CARTESIAN_POINT('Ctrl Pts',(1.84929312930314,-1.,0.416300022039885));
#40482=CARTESIAN_POINT('Ctrl Pts',(1.8541763285645,-1.,0.418164129144046));
#40483=CARTESIAN_POINT('Ctrl Pts',(1.8590328109667,-1.,0.420157287975583));
#40484=CARTESIAN_POINT('Ctrl Pts',(1.86408083333863,-1.,0.422327307417885));
#40485=CARTESIAN_POINT('Ctrl Pts',(1.8693780394412,-1.,0.424678177290876));
#40486=CARTESIAN_POINT('Ctrl Pts',(1.87486989291333,-1.,0.427183828518743));
#40487=CARTESIAN_POINT('Ctrl Pts',(1.88044229001778,-1.,0.429803062482217));
#40488=CARTESIAN_POINT('Ctrl Pts',(1.88596913666828,-1.,0.432493038548833));
#40489=CARTESIAN_POINT('Ctrl Pts',(1.89136993975585,-1.,0.43522566096358));
#40490=CARTESIAN_POINT('Ctrl Pts',(1.89663648956549,-1.,0.437995003948443));
#40491=CARTESIAN_POINT('Ctrl Pts',(1.90180124389137,-1.,0.440807833704161));
#40492=CARTESIAN_POINT('Ctrl Pts',(1.90691756144906,-1.,0.443677556849171));
#40493=CARTESIAN_POINT('Ctrl Pts',(1.91203699981095,-1.,0.446617343485651));
#40494=CARTESIAN_POINT('Ctrl Pts',(1.91718342555717,-1.,0.449632260106572));
#40495=CARTESIAN_POINT('Ctrl Pts',(1.9223538064847,-1.,0.452719478359356));
#40496=CARTESIAN_POINT('Ctrl Pts',(1.92753067150461,-1.,0.455872005174336));
#40497=CARTESIAN_POINT('Ctrl Pts',(1.93269066517936,-1.,0.459081234547932));
#40498=CARTESIAN_POINT('Ctrl Pts',(1.93781486640834,-1.,0.462340031009087));
#40499=CARTESIAN_POINT('Ctrl Pts',(1.94289794196205,-1.,0.465645462026065));
#40500=CARTESIAN_POINT('Ctrl Pts',(1.94794381136524,-1.,0.468997482913158));
#40501=CARTESIAN_POINT('Ctrl Pts',(1.95296148278136,-1.,0.47239767226408));
#40502=CARTESIAN_POINT('Ctrl Pts',(1.95796111148175,-1.,0.475848034683172));
#40503=CARTESIAN_POINT('Ctrl Pts',(1.96294933055938,-1.,0.479349583074846));
#40504=CARTESIAN_POINT('Ctrl Pts',(1.96792703422358,-1.,0.482901662120687));
#40505=CARTESIAN_POINT('Ctrl Pts',(1.97289186263272,-1.,0.486502692907661));
#40506=CARTESIAN_POINT('Ctrl Pts',(1.97783973019229,-1.,0.490150627860955));
#40507=CARTESIAN_POINT('Ctrl Pts',(1.9827665876182,-1.,0.493843476541493));
#40508=CARTESIAN_POINT('Ctrl Pts',(1.98767044752929,-1.,0.497579909545564));
#40509=CARTESIAN_POINT('Ctrl Pts',(1.9925514912615,-1.,0.501359287727129));
#40510=CARTESIAN_POINT('Ctrl Pts',(1.99741107463567,-1.,0.505181361323011));
#40511=CARTESIAN_POINT('Ctrl Pts',(2.00225107134733,-1.,0.509046069886152));
#40512=CARTESIAN_POINT('Ctrl Pts',(2.00707309946955,-1.,0.512953306961814));
#40513=CARTESIAN_POINT('Ctrl Pts',(2.01187773939257,-1.,0.516902681728733));
#40514=CARTESIAN_POINT('Ctrl Pts',(2.01666477917305,-1.,0.520893590399429));
#40515=CARTESIAN_POINT('Ctrl Pts',(2.02143356304712,-1.,0.524925318333519));
#40516=CARTESIAN_POINT('Ctrl Pts',(2.02618329083289,-1.,0.528997127241911));
#40517=CARTESIAN_POINT('Ctrl Pts',(2.03091336214401,-1.,0.533108355132905));
#40518=CARTESIAN_POINT('Ctrl Pts',(2.03562362953993,-1.,0.537258489833135));
#40519=CARTESIAN_POINT('Ctrl Pts',(2.0403142269048,-1.,0.54144712061552));
#40520=CARTESIAN_POINT('Ctrl Pts',(2.0449854471456,-1.,0.545673903817349));
#40521=CARTESIAN_POINT('Ctrl Pts',(2.04963761077974,-1.,0.549938525150342));
#40522=CARTESIAN_POINT('Ctrl Pts',(2.05427091604482,-1.,0.55424065746411));
#40523=CARTESIAN_POINT('Ctrl Pts',(2.05888537756571,-1.,0.558579940185468));
#40524=CARTESIAN_POINT('Ctrl Pts',(2.06348090160697,-1.,0.562955993082574));
#40525=CARTESIAN_POINT('Ctrl Pts',(2.06805732997383,-1.,0.56736842118123));
#40526=CARTESIAN_POINT('Ctrl Pts',(2.07261449292757,-1.,0.571816823242411));
#40527=CARTESIAN_POINT('Ctrl Pts',(2.07715226767361,-1.,0.576300797416275));
#40528=CARTESIAN_POINT('Ctrl Pts',(2.08167059018138,-1.,0.580819952107257));
#40529=CARTESIAN_POINT('Ctrl Pts',(2.086169437277,-1.,0.585373918990895));
#40530=CARTESIAN_POINT('Ctrl Pts',(2.09064881812053,-1.,0.58996236540319));
#40531=CARTESIAN_POINT('Ctrl Pts',(2.09510876220501,-1.,0.594585006052824));
#40532=CARTESIAN_POINT('Ctrl Pts',(2.09954930865331,-1.,0.599241616422144));
#40533=CARTESIAN_POINT('Ctrl Pts',(2.10397049887709,-1.,0.603932030738212));
#40534=CARTESIAN_POINT('Ctrl Pts',(2.10749199615859,-1.,0.607711315456826));
#40535=CARTESIAN_POINT('Ctrl Pts',(2.11012443807661,-1.,0.610560911691114));
#40536=CARTESIAN_POINT('Ctrl Pts',(2.11187554260142,-1.,0.61246736556225));
#40537=CARTESIAN_POINT('Ctrl Pts',(2.11275013067528,-1.,0.613422273260091));
#40538=CARTESIAN_POINT('',(2.0698113262342,-1.,0.745574324794401));
#40539=CARTESIAN_POINT('',(2.11275013067528,-1.,0.613422273260091));
#40540=CARTESIAN_POINT('Ctrl Pts',(2.0698113262342,-1.,0.745574324794401));
#40541=CARTESIAN_POINT('Ctrl Pts',(2.06854248895575,-1.,0.74583279137781));
#40542=CARTESIAN_POINT('Ctrl Pts',(2.06600523016401,-1.,0.746345871542696));
#40543=CARTESIAN_POINT('Ctrl Pts',(2.06220058927162,-1.,0.747103932785504));
#40544=CARTESIAN_POINT('Ctrl Pts',(2.05713023030263,-1.,0.748091554181101));
#40545=CARTESIAN_POINT('Ctrl Pts',(2.05079645591606,-1.,0.749287468663053));
#40546=CARTESIAN_POINT('Ctrl Pts',(2.04446689147754,-1.,0.750444657874758));
#40547=CARTESIAN_POINT('Ctrl Pts',(2.03814160092173,-1.,0.751562963361384));
#40548=CARTESIAN_POINT('Ctrl Pts',(2.03182068456467,-1.,0.752642180488104));
#40549=CARTESIAN_POINT('Ctrl Pts',(2.02550428623587,-1.,0.753682061113766));
#40550=CARTESIAN_POINT('Ctrl Pts',(2.01919259406003,-1.,0.75468233072352));
#40551=CARTESIAN_POINT('Ctrl Pts',(2.01288584328149,-1.,0.755642704958101));
#40552=CARTESIAN_POINT('Ctrl Pts',(2.00658431587682,-1.,0.756562904646496));
#40553=CARTESIAN_POINT('Ctrl Pts',(2.00028834739072,-1.,0.757442676862342));
#40554=CARTESIAN_POINT('Ctrl Pts',(1.9939983109871,-1.,0.758281796766377));
#40555=CARTESIAN_POINT('Ctrl Pts',(1.98771456680806,-1.,0.759080037802243));
#40556=CARTESIAN_POINT('Ctrl Pts',(1.98143741418156,-1.,0.759837147452135));
#40557=CARTESIAN_POINT('Ctrl Pts',(1.97516705321521,-1.,0.760552825409856));
#40558=CARTESIAN_POINT('Ctrl Pts',(1.96890351582545,-1.,0.761226690483986));
#40559=CARTESIAN_POINT('Ctrl Pts',(1.96264672744229,-1.,0.761858300014575));
#40560=CARTESIAN_POINT('Ctrl Pts',(1.95639665309893,-1.,0.762447203806264));
#40561=CARTESIAN_POINT('Ctrl Pts',(1.95015342590025,-1.,0.762992990878774));
#40562=CARTESIAN_POINT('Ctrl Pts',(1.94391746617626,-1.,0.763495333538581));
#40563=CARTESIAN_POINT('Ctrl Pts',(1.93768964875867,-1.,0.763954049121394));
#40564=CARTESIAN_POINT('Ctrl Pts',(1.93147105496367,-1.,0.76436901067389));
#40565=CARTESIAN_POINT('Ctrl Pts',(1.92526263537041,-1.,0.764740025488189));
#40566=CARTESIAN_POINT('Ctrl Pts',(1.91906491634197,-1.,0.765066729667095));
#40567=CARTESIAN_POINT('Ctrl Pts',(1.91287765805174,-1.,0.765348465884739));
#40568=CARTESIAN_POINT('Ctrl Pts',(1.90669961402362,-1.,0.765584196937937));
#40569=CARTESIAN_POINT('Ctrl Pts',(1.90052930393599,-1.,0.765772772593395));
#40570=CARTESIAN_POINT('Ctrl Pts',(1.89436577771389,-1.,0.765913193856979));
#40571=CARTESIAN_POINT('Ctrl Pts',(1.88820926433409,-1.,0.76600483706209));
#40572=CARTESIAN_POINT('Ctrl Pts',(1.88206215302561,-1.,0.766047794851869));
#40573=CARTESIAN_POINT('Ctrl Pts',(1.87592888967886,-1.,0.766042837036759));
#40574=CARTESIAN_POINT('Ctrl Pts',(1.86981398314345,-1.,0.765990708546112));
#40575=CARTESIAN_POINT('Ctrl Pts',(1.86372027063314,-1.,0.765891519092557));
#40576=CARTESIAN_POINT('Ctrl Pts',(1.85764741390391,-1.,0.765744212909305));
#40577=CARTESIAN_POINT('Ctrl Pts',(1.85158945130054,-1.,0.765545710619023));
#40578=CARTESIAN_POINT('Ctrl Pts',(1.8455369887591,-1.,0.765291664861972));
#40579=CARTESIAN_POINT('Ctrl Pts',(1.83948181064823,-1.,0.764978057881688));
#40580=CARTESIAN_POINT('Ctrl Pts',(1.8334207722714,-1.,0.764602549687846));
#40581=CARTESIAN_POINT('Ctrl Pts',(1.8273599120008,-1.,0.764165902606056));
#40582=CARTESIAN_POINT('Ctrl Pts',(1.82131873145297,-1.,0.763673465462854));
#40583=CARTESIAN_POINT('Ctrl Pts',(1.81532118405566,-1.,0.763132003836783));
#40584=CARTESIAN_POINT('Ctrl Pts',(1.80938551463989,-1.,0.762546129464036));
#40585=CARTESIAN_POINT('Ctrl Pts',(1.80351583877334,-1.,0.761915336443516));
#40586=CARTESIAN_POINT('Ctrl Pts',(1.79768986997735,-1.,0.761229695230359));
#40587=CARTESIAN_POINT('Ctrl Pts',(1.79185815610802,-1.,0.760469555880425));
#40588=CARTESIAN_POINT('Ctrl Pts',(1.78596964884526,-1.,0.759614401109868));
#40589=CARTESIAN_POINT('Ctrl Pts',(1.77999411220912,-1.,0.75865062667738));
#40590=CARTESIAN_POINT('Ctrl Pts',(1.77394167108342,-1.,0.757578264077238));
#40591=CARTESIAN_POINT('Ctrl Pts',(1.76789396003141,-1.,0.756421896028403));
#40592=CARTESIAN_POINT('Ctrl Pts',(1.7619781724032,-1.,0.755220979975262));
#40593=CARTESIAN_POINT('Ctrl Pts',(1.75631083600175,-1.,0.75400925402848));
#40594=CARTESIAN_POINT('Ctrl Pts',(1.75095139468809,-1.,0.752797683531377));
#40595=CARTESIAN_POINT('Ctrl Pts',(1.74585086852298,-1.,0.751555614163629));
#40596=CARTESIAN_POINT('Ctrl Pts',(1.74080458266705,-1.,0.750193435979541));
#40597=CARTESIAN_POINT('Ctrl Pts',(1.73550351679848,-1.,0.748582462954855));
#40598=CARTESIAN_POINT('Ctrl Pts',(1.72958533647399,-1.,0.746574710096437));
#40599=CARTESIAN_POINT('Ctrl Pts',(1.7226822991693,-1.,0.744021445433765));
#40600=CARTESIAN_POINT('Ctrl Pts',(1.71447789751927,-1.,0.740795162032088));
#40601=CARTESIAN_POINT('Ctrl Pts',(1.70473309006121,-1.,0.736799665724771));
#40602=CARTESIAN_POINT('Ctrl Pts',(1.69326921975743,-1.,0.731963238697195));
#40603=CARTESIAN_POINT('Ctrl Pts',(1.67996158455503,-1.,0.726235967997433));
#40604=CARTESIAN_POINT('Ctrl Pts',(1.6647288055568,-1.,0.719585433804282));
#40605=CARTESIAN_POINT('Ctrl Pts',(1.64752408832016,-1.,0.711993139355394));
#40606=CARTESIAN_POINT('Ctrl Pts',(1.63216541664676,-1.,0.705159151988319));
#40607=CARTESIAN_POINT('Ctrl Pts',(1.61974673472612,-1.,0.699605146405088));
#40608=CARTESIAN_POINT('Ctrl Pts',(1.61106790958151,-1.,0.695712097881194));
#40609=CARTESIAN_POINT('Ctrl Pts',(1.60662857109684,-1.,0.693717979106306));
#40610=CARTESIAN_POINT('Origin',(0.,1.,0.));
#40611=CARTESIAN_POINT('',(-1.4,1.,1.71450551880629E-16));
#40612=CARTESIAN_POINT('',(-1.4,1.,1.71450551880629E-16));
#40613=CARTESIAN_POINT('Origin',(0.,1.,0.));
#40614=CARTESIAN_POINT('Ctrl Pts',(2.11275013067528,-1.,0.613422273260091));
#40615=CARTESIAN_POINT('Ctrl Pts',(2.11275013067528,1.,0.613422273260091));
#40616=CARTESIAN_POINT('Ctrl Pts',(2.11187554260142,-1.,0.61246736556225));
#40617=CARTESIAN_POINT('Ctrl Pts',(2.11187554260142,1.,0.61246736556225));
#40618=CARTESIAN_POINT('Ctrl Pts',(2.11012443807661,-1.,0.610560911691114));
#40619=CARTESIAN_POINT('Ctrl Pts',(2.11012443807661,1.,0.610560911691114));
#40620=CARTESIAN_POINT('Ctrl Pts',(2.10749199615859,-1.,0.607711315456826));
#40621=CARTESIAN_POINT('Ctrl Pts',(2.10749199615859,1.,0.607711315456826));
#40622=CARTESIAN_POINT('Ctrl Pts',(2.10397049887709,-1.,0.603932030738212));
#40623=CARTESIAN_POINT('Ctrl Pts',(2.10397049887709,1.,0.603932030738212));
#40624=CARTESIAN_POINT('Ctrl Pts',(2.09954930865331,-1.,0.599241616422144));
#40625=CARTESIAN_POINT('Ctrl Pts',(2.09954930865331,1.,0.599241616422144));
#40626=CARTESIAN_POINT('Ctrl Pts',(2.09510876220501,-1.,0.594585006052824));
#40627=CARTESIAN_POINT('Ctrl Pts',(2.09510876220501,1.,0.594585006052824));
#40628=CARTESIAN_POINT('Ctrl Pts',(2.09064881812053,-1.,0.58996236540319));
#40629=CARTESIAN_POINT('Ctrl Pts',(2.09064881812053,1.,0.58996236540319));
#40630=CARTESIAN_POINT('Ctrl Pts',(2.086169437277,-1.,0.585373918990895));
#40631=CARTESIAN_POINT('Ctrl Pts',(2.086169437277,1.,0.585373918990895));
#40632=CARTESIAN_POINT('Ctrl Pts',(2.08167059018138,-1.,0.580819952107257));
#40633=CARTESIAN_POINT('Ctrl Pts',(2.08167059018138,1.,0.580819952107257));
#40634=CARTESIAN_POINT('Ctrl Pts',(2.07715226767361,-1.,0.576300797416275));
#40635=CARTESIAN_POINT('Ctrl Pts',(2.07715226767361,1.,0.576300797416275));
#40636=CARTESIAN_POINT('Ctrl Pts',(2.07261449292757,-1.,0.571816823242411));
#40637=CARTESIAN_POINT('Ctrl Pts',(2.07261449292757,1.,0.571816823242411));
#40638=CARTESIAN_POINT('Ctrl Pts',(2.06805732997383,-1.,0.56736842118123));
#40639=CARTESIAN_POINT('Ctrl Pts',(2.06805732997383,1.,0.56736842118123));
#40640=CARTESIAN_POINT('Ctrl Pts',(2.06348090160697,-1.,0.562955993082574));
#40641=CARTESIAN_POINT('Ctrl Pts',(2.06348090160697,1.,0.562955993082574));
#40642=CARTESIAN_POINT('Ctrl Pts',(2.05888537756571,-1.,0.558579940185468));
#40643=CARTESIAN_POINT('Ctrl Pts',(2.05888537756571,1.,0.558579940185468));
#40644=CARTESIAN_POINT('Ctrl Pts',(2.05427091604482,-1.,0.55424065746411));
#40645=CARTESIAN_POINT('Ctrl Pts',(2.05427091604482,1.,0.55424065746411));
#40646=CARTESIAN_POINT('Ctrl Pts',(2.04963761077974,-1.,0.549938525150342));
#40647=CARTESIAN_POINT('Ctrl Pts',(2.04963761077974,1.,0.549938525150342));
#40648=CARTESIAN_POINT('Ctrl Pts',(2.0449854471456,-1.,0.545673903817349));
#40649=CARTESIAN_POINT('Ctrl Pts',(2.0449854471456,1.,0.545673903817349));
#40650=CARTESIAN_POINT('Ctrl Pts',(2.0403142269048,-1.,0.54144712061552));
#40651=CARTESIAN_POINT('Ctrl Pts',(2.0403142269048,1.,0.54144712061552));
#40652=CARTESIAN_POINT('Ctrl Pts',(2.03562362953993,-1.,0.537258489833135));
#40653=CARTESIAN_POINT('Ctrl Pts',(2.03562362953993,1.,0.537258489833135));
#40654=CARTESIAN_POINT('Ctrl Pts',(2.03091336214401,-1.,0.533108355132905));
#40655=CARTESIAN_POINT('Ctrl Pts',(2.03091336214401,1.,0.533108355132905));
#40656=CARTESIAN_POINT('Ctrl Pts',(2.02618329083289,-1.,0.528997127241911));
#40657=CARTESIAN_POINT('Ctrl Pts',(2.02618329083289,1.,0.528997127241911));
#40658=CARTESIAN_POINT('Ctrl Pts',(2.02143356304712,-1.,0.524925318333519));
#40659=CARTESIAN_POINT('Ctrl Pts',(2.02143356304712,1.,0.524925318333519));
#40660=CARTESIAN_POINT('Ctrl Pts',(2.01666477917305,-1.,0.520893590399429));
#40661=CARTESIAN_POINT('Ctrl Pts',(2.01666477917305,1.,0.520893590399429));
#40662=CARTESIAN_POINT('Ctrl Pts',(2.01187773939257,-1.,0.516902681728733));
#40663=CARTESIAN_POINT('Ctrl Pts',(2.01187773939257,1.,0.516902681728733));
#40664=CARTESIAN_POINT('Ctrl Pts',(2.00707309946955,-1.,0.512953306961814));
#40665=CARTESIAN_POINT('Ctrl Pts',(2.00707309946955,1.,0.512953306961814));
#40666=CARTESIAN_POINT('Ctrl Pts',(2.00225107134733,-1.,0.509046069886152));
#40667=CARTESIAN_POINT('Ctrl Pts',(2.00225107134733,1.,0.509046069886152));
#40668=CARTESIAN_POINT('Ctrl Pts',(1.99741107463567,-1.,0.505181361323011));
#40669=CARTESIAN_POINT('Ctrl Pts',(1.99741107463567,1.,0.505181361323011));
#40670=CARTESIAN_POINT('Ctrl Pts',(1.9925514912615,-1.,0.501359287727129));
#40671=CARTESIAN_POINT('Ctrl Pts',(1.9925514912615,1.,0.501359287727129));
#40672=CARTESIAN_POINT('Ctrl Pts',(1.98767044752929,-1.,0.497579909545564));
#40673=CARTESIAN_POINT('Ctrl Pts',(1.98767044752929,1.,0.497579909545564));
#40674=CARTESIAN_POINT('Ctrl Pts',(1.9827665876182,-1.,0.493843476541493));
#40675=CARTESIAN_POINT('Ctrl Pts',(1.9827665876182,1.,0.493843476541493));
#40676=CARTESIAN_POINT('Ctrl Pts',(1.97783973019229,-1.,0.490150627860955));
#40677=CARTESIAN_POINT('Ctrl Pts',(1.97783973019229,1.,0.490150627860955));
#40678=CARTESIAN_POINT('Ctrl Pts',(1.97289186263272,-1.,0.486502692907661));
#40679=CARTESIAN_POINT('Ctrl Pts',(1.97289186263272,1.,0.486502692907661));
#40680=CARTESIAN_POINT('Ctrl Pts',(1.96792703422358,-1.,0.482901662120687));
#40681=CARTESIAN_POINT('Ctrl Pts',(1.96792703422358,1.,0.482901662120687));
#40682=CARTESIAN_POINT('Ctrl Pts',(1.96294933055938,-1.,0.479349583074846));
#40683=CARTESIAN_POINT('Ctrl Pts',(1.96294933055938,1.,0.479349583074846));
#40684=CARTESIAN_POINT('Ctrl Pts',(1.95796111148175,-1.,0.475848034683172));
#40685=CARTESIAN_POINT('Ctrl Pts',(1.95796111148175,1.,0.475848034683172));
#40686=CARTESIAN_POINT('Ctrl Pts',(1.95296148278136,-1.,0.47239767226408));
#40687=CARTESIAN_POINT('Ctrl Pts',(1.95296148278136,1.,0.47239767226408));
#40688=CARTESIAN_POINT('Ctrl Pts',(1.94794381136524,-1.,0.468997482913158));
#40689=CARTESIAN_POINT('Ctrl Pts',(1.94794381136524,1.,0.468997482913158));
#40690=CARTESIAN_POINT('Ctrl Pts',(1.94289794196205,-1.,0.465645462026065));
#40691=CARTESIAN_POINT('Ctrl Pts',(1.94289794196205,1.,0.465645462026065));
#40692=CARTESIAN_POINT('Ctrl Pts',(1.93781486640834,-1.,0.462340031009087));
#40693=CARTESIAN_POINT('Ctrl Pts',(1.93781486640834,1.,0.462340031009087));
#40694=CARTESIAN_POINT('Ctrl Pts',(1.93269066517936,-1.,0.459081234547932));
#40695=CARTESIAN_POINT('Ctrl Pts',(1.93269066517936,1.,0.459081234547932));
#40696=CARTESIAN_POINT('Ctrl Pts',(1.92753067150461,-1.,0.455872005174336));
#40697=CARTESIAN_POINT('Ctrl Pts',(1.92753067150461,1.,0.455872005174336));
#40698=CARTESIAN_POINT('Ctrl Pts',(1.9223538064847,-1.,0.452719478359356));
#40699=CARTESIAN_POINT('Ctrl Pts',(1.9223538064847,1.,0.452719478359356));
#40700=CARTESIAN_POINT('Ctrl Pts',(1.91718342555717,-1.,0.449632260106572));
#40701=CARTESIAN_POINT('Ctrl Pts',(1.91718342555717,1.,0.449632260106572));
#40702=CARTESIAN_POINT('Ctrl Pts',(1.91203699981095,-1.,0.446617343485651));
#40703=CARTESIAN_POINT('Ctrl Pts',(1.91203699981095,1.,0.446617343485651));
#40704=CARTESIAN_POINT('Ctrl Pts',(1.90691756144906,-1.,0.443677556849171));
#40705=CARTESIAN_POINT('Ctrl Pts',(1.90691756144906,1.,0.443677556849171));
#40706=CARTESIAN_POINT('Ctrl Pts',(1.90180124389137,-1.,0.440807833704161));
#40707=CARTESIAN_POINT('Ctrl Pts',(1.90180124389137,1.,0.440807833704161));
#40708=CARTESIAN_POINT('Ctrl Pts',(1.89663648956549,-1.,0.437995003948443));
#40709=CARTESIAN_POINT('Ctrl Pts',(1.89663648956549,1.,0.437995003948443));
#40710=CARTESIAN_POINT('Ctrl Pts',(1.89136993975585,-1.,0.43522566096358));
#40711=CARTESIAN_POINT('Ctrl Pts',(1.89136993975585,1.,0.43522566096358));
#40712=CARTESIAN_POINT('Ctrl Pts',(1.88596913666828,-1.,0.432493038548833));
#40713=CARTESIAN_POINT('Ctrl Pts',(1.88596913666828,1.,0.432493038548833));
#40714=CARTESIAN_POINT('Ctrl Pts',(1.88044229001778,-1.,0.429803062482217));
#40715=CARTESIAN_POINT('Ctrl Pts',(1.88044229001778,1.,0.429803062482217));
#40716=CARTESIAN_POINT('Ctrl Pts',(1.87486989291333,-1.,0.427183828518743));
#40717=CARTESIAN_POINT('Ctrl Pts',(1.87486989291333,1.,0.427183828518743));
#40718=CARTESIAN_POINT('Ctrl Pts',(1.8693780394412,-1.,0.424678177290876));
#40719=CARTESIAN_POINT('Ctrl Pts',(1.8693780394412,1.,0.424678177290876));
#40720=CARTESIAN_POINT('Ctrl Pts',(1.86408083333863,-1.,0.422327307417885));
#40721=CARTESIAN_POINT('Ctrl Pts',(1.86408083333863,1.,0.422327307417885));
#40722=CARTESIAN_POINT('Ctrl Pts',(1.8590328109667,-1.,0.420157287975583));
#40723=CARTESIAN_POINT('Ctrl Pts',(1.8590328109667,1.,0.420157287975583));
#40724=CARTESIAN_POINT('Ctrl Pts',(1.8541763285645,-1.,0.418164129144046));
#40725=CARTESIAN_POINT('Ctrl Pts',(1.8541763285645,1.,0.418164129144046));
#40726=CARTESIAN_POINT('Ctrl Pts',(1.84929312930314,-1.,0.416300022039885));
#40727=CARTESIAN_POINT('Ctrl Pts',(1.84929312930314,1.,0.416300022039885));
#40728=CARTESIAN_POINT('Ctrl Pts',(1.84405757074218,-1.,0.414487438255542));
#40729=CARTESIAN_POINT('Ctrl Pts',(1.84405757074218,1.,0.414487438255542));
#40730=CARTESIAN_POINT('Ctrl Pts',(1.8380895347617,-1.,0.412633125322945));
#40731=CARTESIAN_POINT('Ctrl Pts',(1.8380895347617,1.,0.412633125322945));
#40732=CARTESIAN_POINT('Ctrl Pts',(1.83100408895047,-1.,0.410641256301276));
#40733=CARTESIAN_POINT('Ctrl Pts',(1.83100408895047,1.,0.410641256301276));
#40734=CARTESIAN_POINT('Ctrl Pts',(1.82247022677562,-1.,0.408428948106228));
#40735=CARTESIAN_POINT('Ctrl Pts',(1.82247022677562,1.,0.408428948106228));
#40736=CARTESIAN_POINT('Ctrl Pts',(1.81223801812013,-1.,0.405933518407176));
#40737=CARTESIAN_POINT('Ctrl Pts',(1.81223801812013,1.,0.405933518407176));
#40738=CARTESIAN_POINT('Ctrl Pts',(1.80012077173238,-1.,0.403107976163396));
#40739=CARTESIAN_POINT('Ctrl Pts',(1.80012077173238,1.,0.403107976163396));
#40740=CARTESIAN_POINT('Ctrl Pts',(1.78598826343754,-1.,0.399919403774156));
#40741=CARTESIAN_POINT('Ctrl Pts',(1.78598826343754,1.,0.399919403774156));
#40742=CARTESIAN_POINT('Ctrl Pts',(1.76975560043442,-1.,0.396346196110688));
#40743=CARTESIAN_POINT('Ctrl Pts',(1.76975560043442,1.,0.396346196110688));
#40744=CARTESIAN_POINT('Ctrl Pts',(1.75137405310193,-1.,0.392375812285396));
#40745=CARTESIAN_POINT('Ctrl Pts',(1.75137405310193,1.,0.392375812285396));
#40746=CARTESIAN_POINT('Ctrl Pts',(1.73493170972829,-1.,0.388877023502615));
#40747=CARTESIAN_POINT('Ctrl Pts',(1.73493170972829,1.,0.388877023502615));
#40748=CARTESIAN_POINT('Ctrl Pts',(1.72162022244582,-1.,0.386070790323281));
#40749=CARTESIAN_POINT('Ctrl Pts',(1.72162022244582,1.,0.386070790323281));
#40750=CARTESIAN_POINT('Ctrl Pts',(1.71231062891398,-1.,0.384119047314215));
#40751=CARTESIAN_POINT('Ctrl Pts',(1.71231062891398,1.,0.384119047314215));
#40752=CARTESIAN_POINT('Ctrl Pts',(1.7075470150345,-1.,0.383122945602004));
#40753=CARTESIAN_POINT('Ctrl Pts',(1.7075470150345,1.,0.383122945602004));
#40754=CARTESIAN_POINT('',(1.7075470150345,1.,0.383122945602004));
#40755=CARTESIAN_POINT('',(1.7075470150345,0.,0.383122945602005));
#40756=CARTESIAN_POINT('',(2.11275013067528,1.,0.613422273260091));
#40757=CARTESIAN_POINT('Ctrl Pts',(2.11275013067528,1.,0.613422273260091));
#40758=CARTESIAN_POINT('Ctrl Pts',(2.11187554260142,1.,0.61246736556225));
#40759=CARTESIAN_POINT('Ctrl Pts',(2.11012443807661,1.,0.610560911691114));
#40760=CARTESIAN_POINT('Ctrl Pts',(2.10749199615859,1.,0.607711315456826));
#40761=CARTESIAN_POINT('Ctrl Pts',(2.10397049887709,1.,0.603932030738212));
#40762=CARTESIAN_POINT('Ctrl Pts',(2.09954930865331,1.,0.599241616422144));
#40763=CARTESIAN_POINT('Ctrl Pts',(2.09510876220501,1.,0.594585006052824));
#40764=CARTESIAN_POINT('Ctrl Pts',(2.09064881812053,1.,0.58996236540319));
#40765=CARTESIAN_POINT('Ctrl Pts',(2.086169437277,1.,0.585373918990895));
#40766=CARTESIAN_POINT('Ctrl Pts',(2.08167059018138,1.,0.580819952107257));
#40767=CARTESIAN_POINT('Ctrl Pts',(2.07715226767361,1.,0.576300797416275));
#40768=CARTESIAN_POINT('Ctrl Pts',(2.07261449292757,1.,0.571816823242411));
#40769=CARTESIAN_POINT('Ctrl Pts',(2.06805732997383,1.,0.56736842118123));
#40770=CARTESIAN_POINT('Ctrl Pts',(2.06348090160697,1.,0.562955993082574));
#40771=CARTESIAN_POINT('Ctrl Pts',(2.05888537756571,1.,0.558579940185468));
#40772=CARTESIAN_POINT('Ctrl Pts',(2.05427091604482,1.,0.55424065746411));
#40773=CARTESIAN_POINT('Ctrl Pts',(2.04963761077974,1.,0.549938525150342));
#40774=CARTESIAN_POINT('Ctrl Pts',(2.0449854471456,1.,0.545673903817349));
#40775=CARTESIAN_POINT('Ctrl Pts',(2.0403142269048,1.,0.54144712061552));
#40776=CARTESIAN_POINT('Ctrl Pts',(2.03562362953993,1.,0.537258489833135));
#40777=CARTESIAN_POINT('Ctrl Pts',(2.03091336214401,1.,0.533108355132905));
#40778=CARTESIAN_POINT('Ctrl Pts',(2.02618329083289,1.,0.528997127241911));
#40779=CARTESIAN_POINT('Ctrl Pts',(2.02143356304712,1.,0.524925318333519));
#40780=CARTESIAN_POINT('Ctrl Pts',(2.01666477917305,1.,0.520893590399429));
#40781=CARTESIAN_POINT('Ctrl Pts',(2.01187773939257,1.,0.516902681728733));
#40782=CARTESIAN_POINT('Ctrl Pts',(2.00707309946955,1.,0.512953306961814));
#40783=CARTESIAN_POINT('Ctrl Pts',(2.00225107134733,1.,0.509046069886152));
#40784=CARTESIAN_POINT('Ctrl Pts',(1.99741107463567,1.,0.505181361323011));
#40785=CARTESIAN_POINT('Ctrl Pts',(1.9925514912615,1.,0.501359287727129));
#40786=CARTESIAN_POINT('Ctrl Pts',(1.98767044752929,1.,0.497579909545564));
#40787=CARTESIAN_POINT('Ctrl Pts',(1.9827665876182,1.,0.493843476541493));
#40788=CARTESIAN_POINT('Ctrl Pts',(1.97783973019229,1.,0.490150627860955));
#40789=CARTESIAN_POINT('Ctrl Pts',(1.97289186263272,1.,0.486502692907661));
#40790=CARTESIAN_POINT('Ctrl Pts',(1.96792703422358,1.,0.482901662120687));
#40791=CARTESIAN_POINT('Ctrl Pts',(1.96294933055938,1.,0.479349583074846));
#40792=CARTESIAN_POINT('Ctrl Pts',(1.95796111148175,1.,0.475848034683172));
#40793=CARTESIAN_POINT('Ctrl Pts',(1.95296148278136,1.,0.47239767226408));
#40794=CARTESIAN_POINT('Ctrl Pts',(1.94794381136524,1.,0.468997482913158));
#40795=CARTESIAN_POINT('Ctrl Pts',(1.94289794196205,1.,0.465645462026065));
#40796=CARTESIAN_POINT('Ctrl Pts',(1.93781486640834,1.,0.462340031009087));
#40797=CARTESIAN_POINT('Ctrl Pts',(1.93269066517936,1.,0.459081234547932));
#40798=CARTESIAN_POINT('Ctrl Pts',(1.92753067150461,1.,0.455872005174336));
#40799=CARTESIAN_POINT('Ctrl Pts',(1.9223538064847,1.,0.452719478359356));
#40800=CARTESIAN_POINT('Ctrl Pts',(1.91718342555717,1.,0.449632260106572));
#40801=CARTESIAN_POINT('Ctrl Pts',(1.91203699981095,1.,0.446617343485651));
#40802=CARTESIAN_POINT('Ctrl Pts',(1.90691756144906,1.,0.443677556849171));
#40803=CARTESIAN_POINT('Ctrl Pts',(1.90180124389137,1.,0.440807833704161));
#40804=CARTESIAN_POINT('Ctrl Pts',(1.89663648956549,1.,0.437995003948443));
#40805=CARTESIAN_POINT('Ctrl Pts',(1.89136993975585,1.,0.43522566096358));
#40806=CARTESIAN_POINT('Ctrl Pts',(1.88596913666828,1.,0.432493038548833));
#40807=CARTESIAN_POINT('Ctrl Pts',(1.88044229001778,1.,0.429803062482217));
#40808=CARTESIAN_POINT('Ctrl Pts',(1.87486989291333,1.,0.427183828518743));
#40809=CARTESIAN_POINT('Ctrl Pts',(1.8693780394412,1.,0.424678177290876));
#40810=CARTESIAN_POINT('Ctrl Pts',(1.86408083333863,1.,0.422327307417885));
#40811=CARTESIAN_POINT('Ctrl Pts',(1.8590328109667,1.,0.420157287975583));
#40812=CARTESIAN_POINT('Ctrl Pts',(1.8541763285645,1.,0.418164129144046));
#40813=CARTESIAN_POINT('Ctrl Pts',(1.84929312930314,1.,0.416300022039885));
#40814=CARTESIAN_POINT('Ctrl Pts',(1.84405757074218,1.,0.414487438255542));
#40815=CARTESIAN_POINT('Ctrl Pts',(1.8380895347617,1.,0.412633125322945));
#40816=CARTESIAN_POINT('Ctrl Pts',(1.83100408895047,1.,0.410641256301276));
#40817=CARTESIAN_POINT('Ctrl Pts',(1.82247022677562,1.,0.408428948106228));
#40818=CARTESIAN_POINT('Ctrl Pts',(1.81223801812013,1.,0.405933518407176));
#40819=CARTESIAN_POINT('Ctrl Pts',(1.80012077173238,1.,0.403107976163396));
#40820=CARTESIAN_POINT('Ctrl Pts',(1.78598826343754,1.,0.399919403774156));
#40821=CARTESIAN_POINT('Ctrl Pts',(1.76975560043442,1.,0.396346196110688));
#40822=CARTESIAN_POINT('Ctrl Pts',(1.75137405310193,1.,0.392375812285396));
#40823=CARTESIAN_POINT('Ctrl Pts',(1.73493170972829,1.,0.388877023502615));
#40824=CARTESIAN_POINT('Ctrl Pts',(1.72162022244582,1.,0.386070790323281));
#40825=CARTESIAN_POINT('Ctrl Pts',(1.71231062891398,1.,0.384119047314215));
#40826=CARTESIAN_POINT('Ctrl Pts',(1.7075470150345,1.,0.383122945602004));
#40827=CARTESIAN_POINT('',(2.11275013067528,0.,0.613422273260091));
#40828=CARTESIAN_POINT('Origin',(2.0698113262342,0.,0.745574324794401));
#40829=CARTESIAN_POINT('',(2.0698113262342,1.,0.745574324794401));
#40830=CARTESIAN_POINT('',(2.11275013067528,1.,0.613422273260091));
#40831=CARTESIAN_POINT('',(2.0698113262342,0.,0.745574324794401));
#40832=CARTESIAN_POINT('Ctrl Pts',(1.60662857109684,-1.,0.693717979106306));
#40833=CARTESIAN_POINT('Ctrl Pts',(1.60662857109684,1.,0.693717979106306));
#40834=CARTESIAN_POINT('Ctrl Pts',(1.61106790958151,-1.,0.695712097881194));
#40835=CARTESIAN_POINT('Ctrl Pts',(1.61106790958151,1.,0.695712097881194));
#40836=CARTESIAN_POINT('Ctrl Pts',(1.61974673472612,-1.,0.699605146405088));
#40837=CARTESIAN_POINT('Ctrl Pts',(1.61974673472612,1.,0.699605146405088));
#40838=CARTESIAN_POINT('Ctrl Pts',(1.63216541664676,-1.,0.705159151988319));
#40839=CARTESIAN_POINT('Ctrl Pts',(1.63216541664676,1.,0.705159151988319));
#40840=CARTESIAN_POINT('Ctrl Pts',(1.64752408832016,-1.,0.711993139355394));
#40841=CARTESIAN_POINT('Ctrl Pts',(1.64752408832016,1.,0.711993139355394));
#40842=CARTESIAN_POINT('Ctrl Pts',(1.6647288055568,-1.,0.719585433804282));
#40843=CARTESIAN_POINT('Ctrl Pts',(1.6647288055568,1.,0.719585433804282));
#40844=CARTESIAN_POINT('Ctrl Pts',(1.67996158455503,-1.,0.726235967997433));
#40845=CARTESIAN_POINT('Ctrl Pts',(1.67996158455503,1.,0.726235967997433));
#40846=CARTESIAN_POINT('Ctrl Pts',(1.69326921975743,-1.,0.731963238697195));
#40847=CARTESIAN_POINT('Ctrl Pts',(1.69326921975743,1.,0.731963238697195));
#40848=CARTESIAN_POINT('Ctrl Pts',(1.70473309006121,-1.,0.736799665724771));
#40849=CARTESIAN_POINT('Ctrl Pts',(1.70473309006121,1.,0.736799665724771));
#40850=CARTESIAN_POINT('Ctrl Pts',(1.71447789751927,-1.,0.740795162032088));
#40851=CARTESIAN_POINT('Ctrl Pts',(1.71447789751927,1.,0.740795162032088));
#40852=CARTESIAN_POINT('Ctrl Pts',(1.7226822991693,-1.,0.744021445433765));
#40853=CARTESIAN_POINT('Ctrl Pts',(1.7226822991693,1.,0.744021445433765));
#40854=CARTESIAN_POINT('Ctrl Pts',(1.72958533647399,-1.,0.746574710096437));
#40855=CARTESIAN_POINT('Ctrl Pts',(1.72958533647399,1.,0.746574710096437));
#40856=CARTESIAN_POINT('Ctrl Pts',(1.73550351679848,-1.,0.748582462954855));
#40857=CARTESIAN_POINT('Ctrl Pts',(1.73550351679848,1.,0.748582462954855));
#40858=CARTESIAN_POINT('Ctrl Pts',(1.74080458266705,-1.,0.750193435979541));
#40859=CARTESIAN_POINT('Ctrl Pts',(1.74080458266705,1.,0.750193435979541));
#40860=CARTESIAN_POINT('Ctrl Pts',(1.74585086852298,-1.,0.751555614163629));
#40861=CARTESIAN_POINT('Ctrl Pts',(1.74585086852298,1.,0.751555614163629));
#40862=CARTESIAN_POINT('Ctrl Pts',(1.75095139468809,-1.,0.752797683531377));
#40863=CARTESIAN_POINT('Ctrl Pts',(1.75095139468809,1.,0.752797683531377));
#40864=CARTESIAN_POINT('Ctrl Pts',(1.75631083600175,-1.,0.75400925402848));
#40865=CARTESIAN_POINT('Ctrl Pts',(1.75631083600175,1.,0.75400925402848));
#40866=CARTESIAN_POINT('Ctrl Pts',(1.7619781724032,-1.,0.755220979975262));
#40867=CARTESIAN_POINT('Ctrl Pts',(1.7619781724032,1.,0.755220979975262));
#40868=CARTESIAN_POINT('Ctrl Pts',(1.76789396003141,-1.,0.756421896028403));
#40869=CARTESIAN_POINT('Ctrl Pts',(1.76789396003141,1.,0.756421896028403));
#40870=CARTESIAN_POINT('Ctrl Pts',(1.77394167108342,-1.,0.757578264077238));
#40871=CARTESIAN_POINT('Ctrl Pts',(1.77394167108342,1.,0.757578264077238));
#40872=CARTESIAN_POINT('Ctrl Pts',(1.77999411220912,-1.,0.75865062667738));
#40873=CARTESIAN_POINT('Ctrl Pts',(1.77999411220912,1.,0.75865062667738));
#40874=CARTESIAN_POINT('Ctrl Pts',(1.78596964884526,-1.,0.759614401109868));
#40875=CARTESIAN_POINT('Ctrl Pts',(1.78596964884526,1.,0.759614401109868));
#40876=CARTESIAN_POINT('Ctrl Pts',(1.79185815610802,-1.,0.760469555880425));
#40877=CARTESIAN_POINT('Ctrl Pts',(1.79185815610802,1.,0.760469555880425));
#40878=CARTESIAN_POINT('Ctrl Pts',(1.79768986997735,-1.,0.761229695230359));
#40879=CARTESIAN_POINT('Ctrl Pts',(1.79768986997735,1.,0.761229695230359));
#40880=CARTESIAN_POINT('Ctrl Pts',(1.80351583877334,-1.,0.761915336443516));
#40881=CARTESIAN_POINT('Ctrl Pts',(1.80351583877334,1.,0.761915336443516));
#40882=CARTESIAN_POINT('Ctrl Pts',(1.80938551463989,-1.,0.762546129464036));
#40883=CARTESIAN_POINT('Ctrl Pts',(1.80938551463989,1.,0.762546129464036));
#40884=CARTESIAN_POINT('Ctrl Pts',(1.81532118405566,-1.,0.763132003836783));
#40885=CARTESIAN_POINT('Ctrl Pts',(1.81532118405566,1.,0.763132003836783));
#40886=CARTESIAN_POINT('Ctrl Pts',(1.82131873145297,-1.,0.763673465462854));
#40887=CARTESIAN_POINT('Ctrl Pts',(1.82131873145297,1.,0.763673465462854));
#40888=CARTESIAN_POINT('Ctrl Pts',(1.8273599120008,-1.,0.764165902606056));
#40889=CARTESIAN_POINT('Ctrl Pts',(1.8273599120008,1.,0.764165902606056));
#40890=CARTESIAN_POINT('Ctrl Pts',(1.8334207722714,-1.,0.764602549687846));
#40891=CARTESIAN_POINT('Ctrl Pts',(1.8334207722714,1.,0.764602549687846));
#40892=CARTESIAN_POINT('Ctrl Pts',(1.83948181064823,-1.,0.764978057881688));
#40893=CARTESIAN_POINT('Ctrl Pts',(1.83948181064823,1.,0.764978057881688));
#40894=CARTESIAN_POINT('Ctrl Pts',(1.8455369887591,-1.,0.765291664861972));
#40895=CARTESIAN_POINT('Ctrl Pts',(1.8455369887591,1.,0.765291664861972));
#40896=CARTESIAN_POINT('Ctrl Pts',(1.85158945130054,-1.,0.765545710619023));
#40897=CARTESIAN_POINT('Ctrl Pts',(1.85158945130054,1.,0.765545710619023));
#40898=CARTESIAN_POINT('Ctrl Pts',(1.85764741390391,-1.,0.765744212909305));
#40899=CARTESIAN_POINT('Ctrl Pts',(1.85764741390391,1.,0.765744212909305));
#40900=CARTESIAN_POINT('Ctrl Pts',(1.86372027063314,-1.,0.765891519092557));
#40901=CARTESIAN_POINT('Ctrl Pts',(1.86372027063314,1.,0.765891519092557));
#40902=CARTESIAN_POINT('Ctrl Pts',(1.86981398314345,-1.,0.765990708546112));
#40903=CARTESIAN_POINT('Ctrl Pts',(1.86981398314345,1.,0.765990708546112));
#40904=CARTESIAN_POINT('Ctrl Pts',(1.87592888967886,-1.,0.766042837036759));
#40905=CARTESIAN_POINT('Ctrl Pts',(1.87592888967886,1.,0.766042837036759));
#40906=CARTESIAN_POINT('Ctrl Pts',(1.88206215302561,-1.,0.766047794851869));
#40907=CARTESIAN_POINT('Ctrl Pts',(1.88206215302561,1.,0.766047794851869));
#40908=CARTESIAN_POINT('Ctrl Pts',(1.88820926433409,-1.,0.76600483706209));
#40909=CARTESIAN_POINT('Ctrl Pts',(1.88820926433409,1.,0.76600483706209));
#40910=CARTESIAN_POINT('Ctrl Pts',(1.89436577771389,-1.,0.765913193856979));
#40911=CARTESIAN_POINT('Ctrl Pts',(1.89436577771389,1.,0.765913193856979));
#40912=CARTESIAN_POINT('Ctrl Pts',(1.90052930393599,-1.,0.765772772593395));
#40913=CARTESIAN_POINT('Ctrl Pts',(1.90052930393599,1.,0.765772772593395));
#40914=CARTESIAN_POINT('Ctrl Pts',(1.90669961402362,-1.,0.765584196937937));
#40915=CARTESIAN_POINT('Ctrl Pts',(1.90669961402362,1.,0.765584196937937));
#40916=CARTESIAN_POINT('Ctrl Pts',(1.91287765805174,-1.,0.765348465884739));
#40917=CARTESIAN_POINT('Ctrl Pts',(1.91287765805174,1.,0.765348465884739));
#40918=CARTESIAN_POINT('Ctrl Pts',(1.91906491634197,-1.,0.765066729667095));
#40919=CARTESIAN_POINT('Ctrl Pts',(1.91906491634197,1.,0.765066729667095));
#40920=CARTESIAN_POINT('Ctrl Pts',(1.92526263537041,-1.,0.764740025488189));
#40921=CARTESIAN_POINT('Ctrl Pts',(1.92526263537041,1.,0.764740025488189));
#40922=CARTESIAN_POINT('Ctrl Pts',(1.93147105496367,-1.,0.76436901067389));
#40923=CARTESIAN_POINT('Ctrl Pts',(1.93147105496367,1.,0.76436901067389));
#40924=CARTESIAN_POINT('Ctrl Pts',(1.93768964875867,-1.,0.763954049121394));
#40925=CARTESIAN_POINT('Ctrl Pts',(1.93768964875867,1.,0.763954049121394));
#40926=CARTESIAN_POINT('Ctrl Pts',(1.94391746617626,-1.,0.763495333538581));
#40927=CARTESIAN_POINT('Ctrl Pts',(1.94391746617626,1.,0.763495333538581));
#40928=CARTESIAN_POINT('Ctrl Pts',(1.95015342590025,-1.,0.762992990878774));
#40929=CARTESIAN_POINT('Ctrl Pts',(1.95015342590025,1.,0.762992990878774));
#40930=CARTESIAN_POINT('Ctrl Pts',(1.95639665309893,-1.,0.762447203806264));
#40931=CARTESIAN_POINT('Ctrl Pts',(1.95639665309893,1.,0.762447203806264));
#40932=CARTESIAN_POINT('Ctrl Pts',(1.96264672744229,-1.,0.761858300014575));
#40933=CARTESIAN_POINT('Ctrl Pts',(1.96264672744229,1.,0.761858300014575));
#40934=CARTESIAN_POINT('Ctrl Pts',(1.96890351582545,-1.,0.761226690483986));
#40935=CARTESIAN_POINT('Ctrl Pts',(1.96890351582545,1.,0.761226690483986));
#40936=CARTESIAN_POINT('Ctrl Pts',(1.97516705321521,-1.,0.760552825409856));
#40937=CARTESIAN_POINT('Ctrl Pts',(1.97516705321521,1.,0.760552825409856));
#40938=CARTESIAN_POINT('Ctrl Pts',(1.98143741418156,-1.,0.759837147452135));
#40939=CARTESIAN_POINT('Ctrl Pts',(1.98143741418156,1.,0.759837147452135));
#40940=CARTESIAN_POINT('Ctrl Pts',(1.98771456680806,-1.,0.759080037802243));
#40941=CARTESIAN_POINT('Ctrl Pts',(1.98771456680806,1.,0.759080037802243));
#40942=CARTESIAN_POINT('Ctrl Pts',(1.9939983109871,-1.,0.758281796766377));
#40943=CARTESIAN_POINT('Ctrl Pts',(1.9939983109871,1.,0.758281796766377));
#40944=CARTESIAN_POINT('Ctrl Pts',(2.00028834739072,-1.,0.757442676862342));
#40945=CARTESIAN_POINT('Ctrl Pts',(2.00028834739072,1.,0.757442676862342));
#40946=CARTESIAN_POINT('Ctrl Pts',(2.00658431587682,-1.,0.756562904646496));
#40947=CARTESIAN_POINT('Ctrl Pts',(2.00658431587682,1.,0.756562904646496));
#40948=CARTESIAN_POINT('Ctrl Pts',(2.01288584328149,-1.,0.755642704958101));
#40949=CARTESIAN_POINT('Ctrl Pts',(2.01288584328149,1.,0.755642704958101));
#40950=CARTESIAN_POINT('Ctrl Pts',(2.01919259406003,-1.,0.75468233072352));
#40951=CARTESIAN_POINT('Ctrl Pts',(2.01919259406003,1.,0.75468233072352));
#40952=CARTESIAN_POINT('Ctrl Pts',(2.02550428623587,-1.,0.753682061113766));
#40953=CARTESIAN_POINT('Ctrl Pts',(2.02550428623587,1.,0.753682061113766));
#40954=CARTESIAN_POINT('Ctrl Pts',(2.03182068456467,-1.,0.752642180488104));
#40955=CARTESIAN_POINT('Ctrl Pts',(2.03182068456467,1.,0.752642180488104));
#40956=CARTESIAN_POINT('Ctrl Pts',(2.03814160092173,-1.,0.751562963361384));
#40957=CARTESIAN_POINT('Ctrl Pts',(2.03814160092173,1.,0.751562963361384));
#40958=CARTESIAN_POINT('Ctrl Pts',(2.04446689147754,-1.,0.750444657874758));
#40959=CARTESIAN_POINT('Ctrl Pts',(2.04446689147754,1.,0.750444657874758));
#40960=CARTESIAN_POINT('Ctrl Pts',(2.05079645591606,-1.,0.749287468663053));
#40961=CARTESIAN_POINT('Ctrl Pts',(2.05079645591606,1.,0.749287468663053));
#40962=CARTESIAN_POINT('Ctrl Pts',(2.05713023030263,-1.,0.748091554181101));
#40963=CARTESIAN_POINT('Ctrl Pts',(2.05713023030263,1.,0.748091554181101));
#40964=CARTESIAN_POINT('Ctrl Pts',(2.06220058927162,-1.,0.747103932785504));
#40965=CARTESIAN_POINT('Ctrl Pts',(2.06220058927162,1.,0.747103932785504));
#40966=CARTESIAN_POINT('Ctrl Pts',(2.06600523016401,-1.,0.746345871542696));
#40967=CARTESIAN_POINT('Ctrl Pts',(2.06600523016401,1.,0.746345871542696));
#40968=CARTESIAN_POINT('Ctrl Pts',(2.06854248895575,-1.,0.74583279137781));
#40969=CARTESIAN_POINT('Ctrl Pts',(2.06854248895575,1.,0.74583279137781));
#40970=CARTESIAN_POINT('Ctrl Pts',(2.0698113262342,-1.,0.745574324794401));
#40971=CARTESIAN_POINT('Ctrl Pts',(2.0698113262342,1.,0.745574324794401));
#40972=CARTESIAN_POINT('',(1.60662857109684,1.,0.693717979106306));
#40973=CARTESIAN_POINT('Ctrl Pts',(1.60662857109684,1.,0.693717979106306));
#40974=CARTESIAN_POINT('Ctrl Pts',(1.61106790958151,1.,0.695712097881194));
#40975=CARTESIAN_POINT('Ctrl Pts',(1.61974673472612,1.,0.699605146405088));
#40976=CARTESIAN_POINT('Ctrl Pts',(1.63216541664676,1.,0.705159151988319));
#40977=CARTESIAN_POINT('Ctrl Pts',(1.64752408832016,1.,0.711993139355394));
#40978=CARTESIAN_POINT('Ctrl Pts',(1.6647288055568,1.,0.719585433804282));
#40979=CARTESIAN_POINT('Ctrl Pts',(1.67996158455503,1.,0.726235967997433));
#40980=CARTESIAN_POINT('Ctrl Pts',(1.69326921975743,1.,0.731963238697195));
#40981=CARTESIAN_POINT('Ctrl Pts',(1.70473309006121,1.,0.736799665724771));
#40982=CARTESIAN_POINT('Ctrl Pts',(1.71447789751927,1.,0.740795162032088));
#40983=CARTESIAN_POINT('Ctrl Pts',(1.7226822991693,1.,0.744021445433765));
#40984=CARTESIAN_POINT('Ctrl Pts',(1.72958533647399,1.,0.746574710096437));
#40985=CARTESIAN_POINT('Ctrl Pts',(1.73550351679848,1.,0.748582462954855));
#40986=CARTESIAN_POINT('Ctrl Pts',(1.74080458266705,1.,0.750193435979541));
#40987=CARTESIAN_POINT('Ctrl Pts',(1.74585086852298,1.,0.751555614163629));
#40988=CARTESIAN_POINT('Ctrl Pts',(1.75095139468809,1.,0.752797683531377));
#40989=CARTESIAN_POINT('Ctrl Pts',(1.75631083600175,1.,0.75400925402848));
#40990=CARTESIAN_POINT('Ctrl Pts',(1.7619781724032,1.,0.755220979975262));
#40991=CARTESIAN_POINT('Ctrl Pts',(1.76789396003141,1.,0.756421896028403));
#40992=CARTESIAN_POINT('Ctrl Pts',(1.77394167108342,1.,0.757578264077238));
#40993=CARTESIAN_POINT('Ctrl Pts',(1.77999411220912,1.,0.75865062667738));
#40994=CARTESIAN_POINT('Ctrl Pts',(1.78596964884526,1.,0.759614401109868));
#40995=CARTESIAN_POINT('Ctrl Pts',(1.79185815610802,1.,0.760469555880425));
#40996=CARTESIAN_POINT('Ctrl Pts',(1.79768986997735,1.,0.761229695230359));
#40997=CARTESIAN_POINT('Ctrl Pts',(1.80351583877334,1.,0.761915336443516));
#40998=CARTESIAN_POINT('Ctrl Pts',(1.80938551463989,1.,0.762546129464036));
#40999=CARTESIAN_POINT('Ctrl Pts',(1.81532118405566,1.,0.763132003836783));
#41000=CARTESIAN_POINT('Ctrl Pts',(1.82131873145297,1.,0.763673465462854));
#41001=CARTESIAN_POINT('Ctrl Pts',(1.8273599120008,1.,0.764165902606056));
#41002=CARTESIAN_POINT('Ctrl Pts',(1.8334207722714,1.,0.764602549687846));
#41003=CARTESIAN_POINT('Ctrl Pts',(1.83948181064823,1.,0.764978057881688));
#41004=CARTESIAN_POINT('Ctrl Pts',(1.8455369887591,1.,0.765291664861972));
#41005=CARTESIAN_POINT('Ctrl Pts',(1.85158945130054,1.,0.765545710619023));
#41006=CARTESIAN_POINT('Ctrl Pts',(1.85764741390391,1.,0.765744212909305));
#41007=CARTESIAN_POINT('Ctrl Pts',(1.86372027063314,1.,0.765891519092557));
#41008=CARTESIAN_POINT('Ctrl Pts',(1.86981398314345,1.,0.765990708546112));
#41009=CARTESIAN_POINT('Ctrl Pts',(1.87592888967886,1.,0.766042837036759));
#41010=CARTESIAN_POINT('Ctrl Pts',(1.88206215302561,1.,0.766047794851869));
#41011=CARTESIAN_POINT('Ctrl Pts',(1.88820926433409,1.,0.76600483706209));
#41012=CARTESIAN_POINT('Ctrl Pts',(1.89436577771389,1.,0.765913193856979));
#41013=CARTESIAN_POINT('Ctrl Pts',(1.90052930393599,1.,0.765772772593395));
#41014=CARTESIAN_POINT('Ctrl Pts',(1.90669961402362,1.,0.765584196937937));
#41015=CARTESIAN_POINT('Ctrl Pts',(1.91287765805174,1.,0.765348465884739));
#41016=CARTESIAN_POINT('Ctrl Pts',(1.91906491634197,1.,0.765066729667095));
#41017=CARTESIAN_POINT('Ctrl Pts',(1.92526263537041,1.,0.764740025488189));
#41018=CARTESIAN_POINT('Ctrl Pts',(1.93147105496367,1.,0.76436901067389));
#41019=CARTESIAN_POINT('Ctrl Pts',(1.93768964875867,1.,0.763954049121394));
#41020=CARTESIAN_POINT('Ctrl Pts',(1.94391746617626,1.,0.763495333538581));
#41021=CARTESIAN_POINT('Ctrl Pts',(1.95015342590025,1.,0.762992990878774));
#41022=CARTESIAN_POINT('Ctrl Pts',(1.95639665309893,1.,0.762447203806264));
#41023=CARTESIAN_POINT('Ctrl Pts',(1.96264672744229,1.,0.761858300014575));
#41024=CARTESIAN_POINT('Ctrl Pts',(1.96890351582545,1.,0.761226690483986));
#41025=CARTESIAN_POINT('Ctrl Pts',(1.97516705321521,1.,0.760552825409856));
#41026=CARTESIAN_POINT('Ctrl Pts',(1.98143741418156,1.,0.759837147452135));
#41027=CARTESIAN_POINT('Ctrl Pts',(1.98771456680806,1.,0.759080037802243));
#41028=CARTESIAN_POINT('Ctrl Pts',(1.9939983109871,1.,0.758281796766377));
#41029=CARTESIAN_POINT('Ctrl Pts',(2.00028834739072,1.,0.757442676862342));
#41030=CARTESIAN_POINT('Ctrl Pts',(2.00658431587682,1.,0.756562904646496));
#41031=CARTESIAN_POINT('Ctrl Pts',(2.01288584328149,1.,0.755642704958101));
#41032=CARTESIAN_POINT('Ctrl Pts',(2.01919259406003,1.,0.75468233072352));
#41033=CARTESIAN_POINT('Ctrl Pts',(2.02550428623587,1.,0.753682061113766));
#41034=CARTESIAN_POINT('Ctrl Pts',(2.03182068456467,1.,0.752642180488104));
#41035=CARTESIAN_POINT('Ctrl Pts',(2.03814160092173,1.,0.751562963361384));
#41036=CARTESIAN_POINT('Ctrl Pts',(2.04446689147754,1.,0.750444657874758));
#41037=CARTESIAN_POINT('Ctrl Pts',(2.05079645591606,1.,0.749287468663053));
#41038=CARTESIAN_POINT('Ctrl Pts',(2.05713023030263,1.,0.748091554181101));
#41039=CARTESIAN_POINT('Ctrl Pts',(2.06220058927162,1.,0.747103932785504));
#41040=CARTESIAN_POINT('Ctrl Pts',(2.06600523016401,1.,0.746345871542696));
#41041=CARTESIAN_POINT('Ctrl Pts',(2.06854248895575,1.,0.74583279137781));
#41042=CARTESIAN_POINT('Ctrl Pts',(2.0698113262342,1.,0.745574324794401));
#41043=CARTESIAN_POINT('',(1.60662857109684,0.,0.693717979106305));
#41044=CARTESIAN_POINT('Origin',(0.,0.,0.));
#41045=CARTESIAN_POINT('',(1.5055822144029,1.,0.892032620296856));
#41046=CARTESIAN_POINT('Origin',(0.,1.,0.));
#41047=CARTESIAN_POINT('',(1.5055822144029,0.,0.892032620296855));
#41048=CARTESIAN_POINT('Ctrl Pts',(1.81978687191668,-1.,1.23627494547115));
#41049=CARTESIAN_POINT('Ctrl Pts',(1.81978687191668,1.,1.23627494547115));
#41050=CARTESIAN_POINT('Ctrl Pts',(1.81925017193666,-1.,1.23509651170476));
#41051=CARTESIAN_POINT('Ctrl Pts',(1.81925017193666,1.,1.23509651170476));
#41052=CARTESIAN_POINT('Ctrl Pts',(1.81817389921279,-1.,1.2327422452705));
#41053=CARTESIAN_POINT('Ctrl Pts',(1.81817389921279,1.,1.2327422452705));
#41054=CARTESIAN_POINT('Ctrl Pts',(1.8165508718364,-1.,1.2292186489137));
#41055=CARTESIAN_POINT('Ctrl Pts',(1.8165508718364,1.,1.2292186489137));
#41056=CARTESIAN_POINT('Ctrl Pts',(1.81436959210434,-1.,1.2245361330495));
#41057=CARTESIAN_POINT('Ctrl Pts',(1.81436959210434,1.,1.2245361330495));
#41058=CARTESIAN_POINT('Ctrl Pts',(1.81161420806656,-1.,1.21870906103557));
#41059=CARTESIAN_POINT('Ctrl Pts',(1.81161420806656,1.,1.21870906103557));
#41060=CARTESIAN_POINT('Ctrl Pts',(1.80882996917129,-1.,1.21290815708314));
#41061=CARTESIAN_POINT('Ctrl Pts',(1.80882996917129,1.,1.21290815708314));
#41062=CARTESIAN_POINT('Ctrl Pts',(1.80601678480707,-1.,1.20713356605475));
#41063=CARTESIAN_POINT('Ctrl Pts',(1.80601678480707,1.,1.20713356605475));
#41064=CARTESIAN_POINT('Ctrl Pts',(1.80317454838603,-1.,1.20138548938974));
#41065=CARTESIAN_POINT('Ctrl Pts',(1.80317454838603,1.,1.20138548938974));
#41066=CARTESIAN_POINT('Ctrl Pts',(1.80030314369879,-1.,1.19566418930242));
#41067=CARTESIAN_POINT('Ctrl Pts',(1.80030314369879,1.,1.19566418930242));
#41068=CARTESIAN_POINT('Ctrl Pts',(1.79740245923478,-1.,1.18996997934445));
#41069=CARTESIAN_POINT('Ctrl Pts',(1.79740245923478,1.,1.18996997934445));
#41070=CARTESIAN_POINT('Ctrl Pts',(1.79447240321515,-1.,1.18430321697432));
#41071=CARTESIAN_POINT('Ctrl Pts',(1.79447240321515,1.,1.18430321697432));
#41072=CARTESIAN_POINT('Ctrl Pts',(1.79151291552689,-1.,1.17866429440809));
#41073=CARTESIAN_POINT('Ctrl Pts',(1.79151291552689,1.,1.17866429440809));
#41074=CARTESIAN_POINT('Ctrl Pts',(1.78852398877616,-1.,1.17305363177328));
#41075=CARTESIAN_POINT('Ctrl Pts',(1.78852398877616,1.,1.17305363177328));
#41076=CARTESIAN_POINT('Ctrl Pts',(1.78550566040443,-1.,1.16747166312303));
#41077=CARTESIAN_POINT('Ctrl Pts',(1.78550566040443,1.,1.16747166312303));
#41078=CARTESIAN_POINT('Ctrl Pts',(1.78245795881009,-1.,1.16191881298499));
#41079=CARTESIAN_POINT('Ctrl Pts',(1.78245795881009,1.,1.16191881298499));
#41080=CARTESIAN_POINT('Ctrl Pts',(1.77938085564275,-1.,1.15639547194698));
#41081=CARTESIAN_POINT('Ctrl Pts',(1.77938085564275,1.,1.15639547194698));
#41082=CARTESIAN_POINT('Ctrl Pts',(1.7762742255701,-1.,1.15090197841515));
#41083=CARTESIAN_POINT('Ctrl Pts',(1.7762742255701,1.,1.15090197841515));
#41084=CARTESIAN_POINT('Ctrl Pts',(1.77313777896194,-1.,1.1454385822692));
#41085=CARTESIAN_POINT('Ctrl Pts',(1.77313777896194,1.,1.1454385822692));
#41086=CARTESIAN_POINT('Ctrl Pts',(1.76997111386769,-1.,1.14000548336975));
#41087=CARTESIAN_POINT('Ctrl Pts',(1.76997111386769,1.,1.14000548336975));
#41088=CARTESIAN_POINT('Ctrl Pts',(1.76677384551862,-1.,1.1346029180462));
#41089=CARTESIAN_POINT('Ctrl Pts',(1.76677384551862,1.,1.1346029180462));
#41090=CARTESIAN_POINT('Ctrl Pts',(1.7635457196617,-1.,1.12923123555075));
#41091=CARTESIAN_POINT('Ctrl Pts',(1.7635457196617,1.,1.12923123555075));
#41092=CARTESIAN_POINT('Ctrl Pts',(1.76028671825096,-1.,1.12389096855086));
#41093=CARTESIAN_POINT('Ctrl Pts',(1.76028671825096,1.,1.12389096855086));
#41094=CARTESIAN_POINT('Ctrl Pts',(1.75699720772105,-1.,1.11858293216763));
#41095=CARTESIAN_POINT('Ctrl Pts',(1.75699720772105,1.,1.11858293216763));
#41096=CARTESIAN_POINT('Ctrl Pts',(1.7536777209463,-1.,1.11330807582551));
#41097=CARTESIAN_POINT('Ctrl Pts',(1.7536777209463,1.,1.11330807582551));
#41098=CARTESIAN_POINT('Ctrl Pts',(1.7503286607592,-1.,1.10806728183007));
#41099=CARTESIAN_POINT('Ctrl Pts',(1.7503286607592,1.,1.10806728183007));
#41100=CARTESIAN_POINT('Ctrl Pts',(1.74695004214923,-1.,1.10286118991143));
#41101=CARTESIAN_POINT('Ctrl Pts',(1.74695004214923,1.,1.10286118991143));
#41102=CARTESIAN_POINT('Ctrl Pts',(1.74354119236208,-1.,1.09768999241226));
#41103=CARTESIAN_POINT('Ctrl Pts',(1.74354119236208,1.,1.09768999241226));
#41104=CARTESIAN_POINT('Ctrl Pts',(1.74010053962247,-1.,1.09255329056493));
#41105=CARTESIAN_POINT('Ctrl Pts',(1.74010053962247,1.,1.09255329056493));
#41106=CARTESIAN_POINT('Ctrl Pts',(1.73662628326091,-1.,1.08745056285427));
#41107=CARTESIAN_POINT('Ctrl Pts',(1.73662628326091,1.,1.08745056285427));
#41108=CARTESIAN_POINT('Ctrl Pts',(1.73311705663407,-1.,1.08238162784749));
#41109=CARTESIAN_POINT('Ctrl Pts',(1.73311705663407,1.,1.08238162784749));
#41110=CARTESIAN_POINT('Ctrl Pts',(1.72957248977424,-1.,1.0773470373727));
#41111=CARTESIAN_POINT('Ctrl Pts',(1.72957248977424,1.,1.0773470373727));
#41112=CARTESIAN_POINT('Ctrl Pts',(1.72599406198488,-1.,1.07234866990252));
#41113=CARTESIAN_POINT('Ctrl Pts',(1.72599406198488,1.,1.07234866990252));
#41114=CARTESIAN_POINT('Ctrl Pts',(1.72238500928453,-1.,1.06738966975462));
#41115=CARTESIAN_POINT('Ctrl Pts',(1.72238500928453,1.,1.06738966975462));
#41116=CARTESIAN_POINT('Ctrl Pts',(1.71874858456904,-1.,1.06247324680647));
#41117=CARTESIAN_POINT('Ctrl Pts',(1.71874858456904,1.,1.06247324680647));
#41118=CARTESIAN_POINT('Ctrl Pts',(1.7150865442702,-1.,1.05760163192479));
#41119=CARTESIAN_POINT('Ctrl Pts',(1.7150865442702,1.,1.05760163192479));
#41120=CARTESIAN_POINT('Ctrl Pts',(1.71139783543989,-1.,1.05277517202855));
#41121=CARTESIAN_POINT('Ctrl Pts',(1.71139783543989,1.,1.05277517202855));
#41122=CARTESIAN_POINT('Ctrl Pts',(1.70767646263649,-1.,1.04799085404995));
#41123=CARTESIAN_POINT('Ctrl Pts',(1.70767646263649,1.,1.04799085404995));
#41124=CARTESIAN_POINT('Ctrl Pts',(1.70391338707982,-1.,1.04324363334554));
#41125=CARTESIAN_POINT('Ctrl Pts',(1.70391338707982,1.,1.04324363334554));
#41126=CARTESIAN_POINT('Ctrl Pts',(1.70010052930962,-1.,1.03852922490789));
#41127=CARTESIAN_POINT('Ctrl Pts',(1.70010052930962,1.,1.03852922490789));
#41128=CARTESIAN_POINT('Ctrl Pts',(1.69623414782771,-1.,1.03384646003588));
#41129=CARTESIAN_POINT('Ctrl Pts',(1.69623414782771,1.,1.03384646003588));
#41130=CARTESIAN_POINT('Ctrl Pts',(1.69231840863458,-1.,1.02919977579147));
#41131=CARTESIAN_POINT('Ctrl Pts',(1.69231840863458,1.,1.02919977579147));
#41132=CARTESIAN_POINT('Ctrl Pts',(1.68836910178447,-1.,1.02460180535255));
#41133=CARTESIAN_POINT('Ctrl Pts',(1.68836910178447,1.,1.02460180535255));
#41134=CARTESIAN_POINT('Ctrl Pts',(1.68440578021706,-1.,1.02006795074201));
#41135=CARTESIAN_POINT('Ctrl Pts',(1.68440578021706,1.,1.02006795074201));
#41136=CARTESIAN_POINT('Ctrl Pts',(1.68044289894798,-1.,1.01561026162773));
#41137=CARTESIAN_POINT('Ctrl Pts',(1.68044289894798,1.,1.01561026162773));
#41138=CARTESIAN_POINT('Ctrl Pts',(1.67648246776464,-1.,1.01123236493511));
#41139=CARTESIAN_POINT('Ctrl Pts',(1.67648246776464,1.,1.01123236493511));
#41140=CARTESIAN_POINT('Ctrl Pts',(1.67250335383293,-1.,1.00692206696414));
#41141=CARTESIAN_POINT('Ctrl Pts',(1.67250335383293,1.,1.00692206696414));
#41142=CARTESIAN_POINT('Ctrl Pts',(1.66846059277303,-1.,1.00265091003727));
#41143=CARTESIAN_POINT('Ctrl Pts',(1.66846059277303,1.,1.00265091003727));
#41144=CARTESIAN_POINT('Ctrl Pts',(1.66430758030376,-1.,0.998389654952758));
#41145=CARTESIAN_POINT('Ctrl Pts',(1.66430758030376,1.,0.998389654952758));
#41146=CARTESIAN_POINT('Ctrl Pts',(1.66001553809947,-1.,0.994121836661306));
#41147=CARTESIAN_POINT('Ctrl Pts',(1.66001553809947,1.,0.994121836661306));
#41148=CARTESIAN_POINT('Ctrl Pts',(1.65559044289699,-1.,0.989855627854165));
#41149=CARTESIAN_POINT('Ctrl Pts',(1.65559044289699,1.,0.989855627854165));
#41150=CARTESIAN_POINT('Ctrl Pts',(1.65110016612638,-1.,0.985642622920821));
#41151=CARTESIAN_POINT('Ctrl Pts',(1.65110016612638,1.,0.985642622920821));
#41152=CARTESIAN_POINT('Ctrl Pts',(1.64665139190656,-1.,0.981562530939489));
#41153=CARTESIAN_POINT('Ctrl Pts',(1.64665139190656,1.,0.981562530939489));
#41154=CARTESIAN_POINT('Ctrl Pts',(1.64233990826687,-1.,0.977689794119417));
#41155=CARTESIAN_POINT('Ctrl Pts',(1.64233990826687,1.,0.977689794119417));
#41156=CARTESIAN_POINT('Ctrl Pts',(1.63820952658144,-1.,0.974066058287419));
#41157=CARTESIAN_POINT('Ctrl Pts',(1.63820952658144,1.,0.974066058287419));
#41158=CARTESIAN_POINT('Ctrl Pts',(1.63420665729798,-1.,0.970669715997509));
#41159=CARTESIAN_POINT('Ctrl Pts',(1.63420665729798,1.,0.970669715997509));
#41160=CARTESIAN_POINT('Ctrl Pts',(1.63013849959461,-1.,0.967387853230345));
#41161=CARTESIAN_POINT('Ctrl Pts',(1.63013849959461,1.,0.967387853230345));
#41162=CARTESIAN_POINT('Ctrl Pts',(1.62571930670187,-1.,0.964046107040536));
#41163=CARTESIAN_POINT('Ctrl Pts',(1.62571930670187,1.,0.964046107040536));
#41164=CARTESIAN_POINT('Ctrl Pts',(1.62061638140221,-1.,0.960438326101729));
#41165=CARTESIAN_POINT('Ctrl Pts',(1.62061638140221,1.,0.960438326101729));
#41166=CARTESIAN_POINT('Ctrl Pts',(1.61449324337085,-1.,0.956354422920671));
#41167=CARTESIAN_POINT('Ctrl Pts',(1.61449324337085,1.,0.956354422920671));
#41168=CARTESIAN_POINT('Ctrl Pts',(1.60706069896936,-1.,0.951613284356035));
#41169=CARTESIAN_POINT('Ctrl Pts',(1.60706069896936,1.,0.951613284356035));
#41170=CARTESIAN_POINT('Ctrl Pts',(1.59810042043673,-1.,0.946078063315257));
#41171=CARTESIAN_POINT('Ctrl Pts',(1.59810042043673,1.,0.946078063315257));
#41172=CARTESIAN_POINT('Ctrl Pts',(1.58744937487176,-1.,0.939646377893399));
#41173=CARTESIAN_POINT('Ctrl Pts',(1.58744937487176,1.,0.939646377893399));
#41174=CARTESIAN_POINT('Ctrl Pts',(1.57499388382243,-1.,0.932246680108685));
#41175=CARTESIAN_POINT('Ctrl Pts',(1.57499388382243,1.,0.932246680108685));
#41176=CARTESIAN_POINT('Ctrl Pts',(1.56065988578893,-1.,0.923832188944341));
#41177=CARTESIAN_POINT('Ctrl Pts',(1.56065988578893,1.,0.923832188944341));
#41178=CARTESIAN_POINT('Ctrl Pts',(1.54440491149498,-1.,0.914375919026456));
#41179=CARTESIAN_POINT('Ctrl Pts',(1.54440491149498,1.,0.914375919026456));
#41180=CARTESIAN_POINT('Ctrl Pts',(1.52984849887993,-1.,0.905967409625651));
#41181=CARTESIAN_POINT('Ctrl Pts',(1.52984849887993,1.,0.905967409625651));
#41182=CARTESIAN_POINT('Ctrl Pts',(1.51805569590094,-1.,0.899185047483511));
#41183=CARTESIAN_POINT('Ctrl Pts',(1.51805569590094,1.,0.899185047483511));
#41184=CARTESIAN_POINT('Ctrl Pts',(1.50980486806688,-1.,0.894452006964544));
#41185=CARTESIAN_POINT('Ctrl Pts',(1.50980486806688,1.,0.894452006964544));
#41186=CARTESIAN_POINT('Ctrl Pts',(1.5055822144029,-1.,0.892032620296856));
#41187=CARTESIAN_POINT('Ctrl Pts',(1.5055822144029,1.,0.892032620296856));
#41188=CARTESIAN_POINT('',(1.81978687191668,1.,1.23627494547115));
#41189=CARTESIAN_POINT('Ctrl Pts',(1.81978687191668,1.,1.23627494547115));
#41190=CARTESIAN_POINT('Ctrl Pts',(1.81925017193666,1.,1.23509651170476));
#41191=CARTESIAN_POINT('Ctrl Pts',(1.81817389921279,1.,1.2327422452705));
#41192=CARTESIAN_POINT('Ctrl Pts',(1.8165508718364,1.,1.2292186489137));
#41193=CARTESIAN_POINT('Ctrl Pts',(1.81436959210434,1.,1.2245361330495));
#41194=CARTESIAN_POINT('Ctrl Pts',(1.81161420806656,1.,1.21870906103557));
#41195=CARTESIAN_POINT('Ctrl Pts',(1.80882996917129,1.,1.21290815708314));
#41196=CARTESIAN_POINT('Ctrl Pts',(1.80601678480707,1.,1.20713356605475));
#41197=CARTESIAN_POINT('Ctrl Pts',(1.80317454838603,1.,1.20138548938974));
#41198=CARTESIAN_POINT('Ctrl Pts',(1.80030314369879,1.,1.19566418930242));
#41199=CARTESIAN_POINT('Ctrl Pts',(1.79740245923478,1.,1.18996997934445));
#41200=CARTESIAN_POINT('Ctrl Pts',(1.79447240321515,1.,1.18430321697432));
#41201=CARTESIAN_POINT('Ctrl Pts',(1.79151291552689,1.,1.17866429440809));
#41202=CARTESIAN_POINT('Ctrl Pts',(1.78852398877616,1.,1.17305363177328));
#41203=CARTESIAN_POINT('Ctrl Pts',(1.78550566040443,1.,1.16747166312303));
#41204=CARTESIAN_POINT('Ctrl Pts',(1.78245795881009,1.,1.16191881298499));
#41205=CARTESIAN_POINT('Ctrl Pts',(1.77938085564275,1.,1.15639547194698));
#41206=CARTESIAN_POINT('Ctrl Pts',(1.7762742255701,1.,1.15090197841515));
#41207=CARTESIAN_POINT('Ctrl Pts',(1.77313777896194,1.,1.1454385822692));
#41208=CARTESIAN_POINT('Ctrl Pts',(1.76997111386769,1.,1.14000548336975));
#41209=CARTESIAN_POINT('Ctrl Pts',(1.76677384551862,1.,1.1346029180462));
#41210=CARTESIAN_POINT('Ctrl Pts',(1.7635457196617,1.,1.12923123555075));
#41211=CARTESIAN_POINT('Ctrl Pts',(1.76028671825096,1.,1.12389096855086));
#41212=CARTESIAN_POINT('Ctrl Pts',(1.75699720772105,1.,1.11858293216763));
#41213=CARTESIAN_POINT('Ctrl Pts',(1.7536777209463,1.,1.11330807582551));
#41214=CARTESIAN_POINT('Ctrl Pts',(1.7503286607592,1.,1.10806728183007));
#41215=CARTESIAN_POINT('Ctrl Pts',(1.74695004214923,1.,1.10286118991143));
#41216=CARTESIAN_POINT('Ctrl Pts',(1.74354119236208,1.,1.09768999241226));
#41217=CARTESIAN_POINT('Ctrl Pts',(1.74010053962247,1.,1.09255329056493));
#41218=CARTESIAN_POINT('Ctrl Pts',(1.73662628326091,1.,1.08745056285427));
#41219=CARTESIAN_POINT('Ctrl Pts',(1.73311705663407,1.,1.08238162784749));
#41220=CARTESIAN_POINT('Ctrl Pts',(1.72957248977424,1.,1.0773470373727));
#41221=CARTESIAN_POINT('Ctrl Pts',(1.72599406198488,1.,1.07234866990252));
#41222=CARTESIAN_POINT('Ctrl Pts',(1.72238500928453,1.,1.06738966975462));
#41223=CARTESIAN_POINT('Ctrl Pts',(1.71874858456904,1.,1.06247324680647));
#41224=CARTESIAN_POINT('Ctrl Pts',(1.7150865442702,1.,1.05760163192479));
#41225=CARTESIAN_POINT('Ctrl Pts',(1.71139783543989,1.,1.05277517202855));
#41226=CARTESIAN_POINT('Ctrl Pts',(1.70767646263649,1.,1.04799085404995));
#41227=CARTESIAN_POINT('Ctrl Pts',(1.70391338707982,1.,1.04324363334554));
#41228=CARTESIAN_POINT('Ctrl Pts',(1.70010052930962,1.,1.03852922490789));
#41229=CARTESIAN_POINT('Ctrl Pts',(1.69623414782771,1.,1.03384646003588));
#41230=CARTESIAN_POINT('Ctrl Pts',(1.69231840863458,1.,1.02919977579147));
#41231=CARTESIAN_POINT('Ctrl Pts',(1.68836910178447,1.,1.02460180535255));
#41232=CARTESIAN_POINT('Ctrl Pts',(1.68440578021706,1.,1.02006795074201));
#41233=CARTESIAN_POINT('Ctrl Pts',(1.68044289894798,1.,1.01561026162773));
#41234=CARTESIAN_POINT('Ctrl Pts',(1.67648246776464,1.,1.01123236493511));
#41235=CARTESIAN_POINT('Ctrl Pts',(1.67250335383293,1.,1.00692206696414));
#41236=CARTESIAN_POINT('Ctrl Pts',(1.66846059277303,1.,1.00265091003727));
#41237=CARTESIAN_POINT('Ctrl Pts',(1.66430758030376,1.,0.998389654952758));
#41238=CARTESIAN_POINT('Ctrl Pts',(1.66001553809947,1.,0.994121836661306));
#41239=CARTESIAN_POINT('Ctrl Pts',(1.65559044289699,1.,0.989855627854165));
#41240=CARTESIAN_POINT('Ctrl Pts',(1.65110016612638,1.,0.985642622920821));
#41241=CARTESIAN_POINT('Ctrl Pts',(1.64665139190656,1.,0.981562530939489));
#41242=CARTESIAN_POINT('Ctrl Pts',(1.64233990826687,1.,0.977689794119417));
#41243=CARTESIAN_POINT('Ctrl Pts',(1.63820952658144,1.,0.974066058287419));
#41244=CARTESIAN_POINT('Ctrl Pts',(1.63420665729798,1.,0.970669715997509));
#41245=CARTESIAN_POINT('Ctrl Pts',(1.63013849959461,1.,0.967387853230345));
#41246=CARTESIAN_POINT('Ctrl Pts',(1.62571930670187,1.,0.964046107040536));
#41247=CARTESIAN_POINT('Ctrl Pts',(1.62061638140221,1.,0.960438326101729));
#41248=CARTESIAN_POINT('Ctrl Pts',(1.61449324337085,1.,0.956354422920671));
#41249=CARTESIAN_POINT('Ctrl Pts',(1.60706069896936,1.,0.951613284356035));
#41250=CARTESIAN_POINT('Ctrl Pts',(1.59810042043673,1.,0.946078063315257));
#41251=CARTESIAN_POINT('Ctrl Pts',(1.58744937487176,1.,0.939646377893399));
#41252=CARTESIAN_POINT('Ctrl Pts',(1.57499388382243,1.,0.932246680108685));
#41253=CARTESIAN_POINT('Ctrl Pts',(1.56065988578893,1.,0.923832188944341));
#41254=CARTESIAN_POINT('Ctrl Pts',(1.54440491149498,1.,0.914375919026456));
#41255=CARTESIAN_POINT('Ctrl Pts',(1.52984849887993,1.,0.905967409625651));
#41256=CARTESIAN_POINT('Ctrl Pts',(1.51805569590094,1.,0.899185047483511));
#41257=CARTESIAN_POINT('Ctrl Pts',(1.50980486806688,1.,0.894452006964544));
#41258=CARTESIAN_POINT('Ctrl Pts',(1.5055822144029,1.,0.892032620296856));
#41259=CARTESIAN_POINT('',(1.81978687191668,0.,1.23627494547115));
#41260=CARTESIAN_POINT('Origin',(1.73811241238545,0.,1.34869019493419));
#41261=CARTESIAN_POINT('',(1.73811241238545,1.,1.34869019493419));
#41262=CARTESIAN_POINT('',(1.81978687191668,1.,1.23627494547115));
#41263=CARTESIAN_POINT('',(1.73811241238545,0.,1.34869019493419));
#41264=CARTESIAN_POINT('Ctrl Pts',(1.31362392696032,-1.,1.15624053661742));
#41265=CARTESIAN_POINT('Ctrl Pts',(1.31362392696032,1.,1.15624053661742));
#41266=CARTESIAN_POINT('Ctrl Pts',(1.31722977216397,-1.,1.15950888730809));
#41267=CARTESIAN_POINT('Ctrl Pts',(1.31722977216397,1.,1.15950888730809));
#41268=CARTESIAN_POINT('Ctrl Pts',(1.32428080721772,-1.,1.16589330093588));
#41269=CARTESIAN_POINT('Ctrl Pts',(1.32428080721772,1.,1.16589330093588));
#41270=CARTESIAN_POINT('Ctrl Pts',(1.33437539347008,-1.,1.17501305789857));
#41271=CARTESIAN_POINT('Ctrl Pts',(1.33437539347008,1.,1.17501305789857));
#41272=CARTESIAN_POINT('Ctrl Pts',(1.34687054001093,-1.,1.18625865667441));
#41273=CARTESIAN_POINT('Ctrl Pts',(1.34687054001093,1.,1.18625865667441));
#41274=CARTESIAN_POINT('Ctrl Pts',(1.36088705043885,-1.,1.1987959077932));
#41275=CARTESIAN_POINT('Ctrl Pts',(1.36088705043885,1.,1.1987959077932));
#41276=CARTESIAN_POINT('Ctrl Pts',(1.37331915607905,-1.,1.20982812925645));
#41277=CARTESIAN_POINT('Ctrl Pts',(1.37331915607905,1.,1.20982812925645));
#41278=CARTESIAN_POINT('Ctrl Pts',(1.38420564527715,-1.,1.21938737280852));
#41279=CARTESIAN_POINT('Ctrl Pts',(1.38420564527715,1.,1.21938737280852));
#41280=CARTESIAN_POINT('Ctrl Pts',(1.39361389568796,-1.,1.22752961899387));
#41281=CARTESIAN_POINT('Ctrl Pts',(1.39361389568796,1.,1.22752961899387));
#41282=CARTESIAN_POINT('Ctrl Pts',(1.40164708206106,-1.,1.23434087290423));
#41283=CARTESIAN_POINT('Ctrl Pts',(1.40164708206106,1.,1.23434087290423));
#41284=CARTESIAN_POINT('Ctrl Pts',(1.40845295531283,-1.,1.23994455029534));
#41285=CARTESIAN_POINT('Ctrl Pts',(1.40845295531283,1.,1.23994455029534));
#41286=CARTESIAN_POINT('Ctrl Pts',(1.41422913175179,-1.,1.24450600513056));
#41287=CARTESIAN_POINT('Ctrl Pts',(1.41422913175179,1.,1.24450600513056));
#41288=CARTESIAN_POINT('Ctrl Pts',(1.41923722596025,-1.,1.24824430986571));
#41289=CARTESIAN_POINT('Ctrl Pts',(1.41923722596025,1.,1.24824430986571));
#41290=CARTESIAN_POINT('Ctrl Pts',(1.42378102115575,-1.,1.2514145557001));
#41291=CARTESIAN_POINT('Ctrl Pts',(1.42378102115575,1.,1.2514145557001));
#41292=CARTESIAN_POINT('Ctrl Pts',(1.42815938799387,-1.,1.25426945222639));
#41293=CARTESIAN_POINT('Ctrl Pts',(1.42815938799387,1.,1.25426945222639));
#41294=CARTESIAN_POINT('Ctrl Pts',(1.43262645609691,-1.,1.25702687965755));
#41295=CARTESIAN_POINT('Ctrl Pts',(1.43262645609691,1.,1.25702687965755));
#41296=CARTESIAN_POINT('Ctrl Pts',(1.43734919180847,-1.,1.25983531012005));
#41297=CARTESIAN_POINT('Ctrl Pts',(1.43734919180847,1.,1.25983531012005));
#41298=CARTESIAN_POINT('Ctrl Pts',(1.44236470511303,-1.,1.26273903323859));
#41299=CARTESIAN_POINT('Ctrl Pts',(1.44236470511303,1.,1.26273903323859));
#41300=CARTESIAN_POINT('Ctrl Pts',(1.44761985001662,-1.,1.26570925118868));
#41301=CARTESIAN_POINT('Ctrl Pts',(1.44761985001662,1.,1.26570925118868));
#41302=CARTESIAN_POINT('Ctrl Pts',(1.45301422764247,-1.,1.2686778680489));
#41303=CARTESIAN_POINT('Ctrl Pts',(1.45301422764247,1.,1.2686778680489));
#41304=CARTESIAN_POINT('Ctrl Pts',(1.45843906294697,-1.,1.27156805265289));
#41305=CARTESIAN_POINT('Ctrl Pts',(1.45843906294697,1.,1.27156805265289));
#41306=CARTESIAN_POINT('Ctrl Pts',(1.46382431332476,-1.,1.27433119897822));
#41307=CARTESIAN_POINT('Ctrl Pts',(1.46382431332476,1.,1.27433119897822));
#41308=CARTESIAN_POINT('Ctrl Pts',(1.46916035917133,-1.,1.2769641483109));
#41309=CARTESIAN_POINT('Ctrl Pts',(1.46916035917133,1.,1.2769641483109));
#41310=CARTESIAN_POINT('Ctrl Pts',(1.4744717526707,-1.,1.2794891824849));
#41311=CARTESIAN_POINT('Ctrl Pts',(1.4744717526707,1.,1.2794891824849));
#41312=CARTESIAN_POINT('Ctrl Pts',(1.47980070347095,-1.,1.28194158939517));
#41313=CARTESIAN_POINT('Ctrl Pts',(1.47980070347095,1.,1.28194158939517));
#41314=CARTESIAN_POINT('Ctrl Pts',(1.4851881711891,-1.,1.28435533880201));
#41315=CARTESIAN_POINT('Ctrl Pts',(1.4851881711891,1.,1.28435533880201));
#41316=CARTESIAN_POINT('Ctrl Pts',(1.4906522831278,-1.,1.2867467611644));
#41317=CARTESIAN_POINT('Ctrl Pts',(1.4906522831278,1.,1.2867467611644));
#41318=CARTESIAN_POINT('Ctrl Pts',(1.49618896881754,-1.,1.28911506584254));
#41319=CARTESIAN_POINT('Ctrl Pts',(1.49618896881754,1.,1.28911506584254));
#41320=CARTESIAN_POINT('Ctrl Pts',(1.50178230149776,-1.,1.29145022885181));
#41321=CARTESIAN_POINT('Ctrl Pts',(1.50178230149776,1.,1.29145022885181));
#41322=CARTESIAN_POINT('Ctrl Pts',(1.50741159078365,-1.,1.29373841372842));
#41323=CARTESIAN_POINT('Ctrl Pts',(1.50741159078365,1.,1.29373841372842));
#41324=CARTESIAN_POINT('Ctrl Pts',(1.51305994241402,-1.,1.29596850710509));
#41325=CARTESIAN_POINT('Ctrl Pts',(1.51305994241402,1.,1.29596850710509));
#41326=CARTESIAN_POINT('Ctrl Pts',(1.51872184912724,-1.,1.29813791800747));
#41327=CARTESIAN_POINT('Ctrl Pts',(1.51872184912724,1.,1.29813791800747));
#41328=CARTESIAN_POINT('Ctrl Pts',(1.52439957861062,-1.,1.30024984366328));
#41329=CARTESIAN_POINT('Ctrl Pts',(1.52439957861062,1.,1.30024984366328));
#41330=CARTESIAN_POINT('Ctrl Pts',(1.53009970283891,-1.,1.30231064395568));
#41331=CARTESIAN_POINT('Ctrl Pts',(1.53009970283891,1.,1.30231064395568));
#41332=CARTESIAN_POINT('Ctrl Pts',(1.53582981268977,-1.,1.30432735639489));
#41333=CARTESIAN_POINT('Ctrl Pts',(1.53582981268977,1.,1.30432735639489));
#41334=CARTESIAN_POINT('Ctrl Pts',(1.54159462645432,-1.,1.30630475189556));
#41335=CARTESIAN_POINT('Ctrl Pts',(1.54159462645432,1.,1.30630475189556));
#41336=CARTESIAN_POINT('Ctrl Pts',(1.54739413957185,-1.,1.30824393907473));
#41337=CARTESIAN_POINT('Ctrl Pts',(1.54739413957185,1.,1.30824393907473));
#41338=CARTESIAN_POINT('Ctrl Pts',(1.55322568759481,-1.,1.31014393684222));
#41339=CARTESIAN_POINT('Ctrl Pts',(1.55322568759481,1.,1.31014393684222));
#41340=CARTESIAN_POINT('Ctrl Pts',(1.55908521254821,-1.,1.31200264341696));
#41341=CARTESIAN_POINT('Ctrl Pts',(1.55908521254821,1.,1.31200264341696));
#41342=CARTESIAN_POINT('Ctrl Pts',(1.56496872402353,-1.,1.31381795281002));
#41343=CARTESIAN_POINT('Ctrl Pts',(1.56496872402353,1.,1.31381795281002));
#41344=CARTESIAN_POINT('Ctrl Pts',(1.57087397835723,-1.,1.31558903860016));
#41345=CARTESIAN_POINT('Ctrl Pts',(1.57087397835723,1.,1.31558903860016));
#41346=CARTESIAN_POINT('Ctrl Pts',(1.5768005650559,-1.,1.31731642317187));
#41347=CARTESIAN_POINT('Ctrl Pts',(1.5768005650559,1.,1.31731642317187));
#41348=CARTESIAN_POINT('Ctrl Pts',(1.58274907898834,-1.,1.31900135021432));
#41349=CARTESIAN_POINT('Ctrl Pts',(1.58274907898834,1.,1.31900135021432));
#41350=CARTESIAN_POINT('Ctrl Pts',(1.58872057258245,-1.,1.32064537110892));
#41351=CARTESIAN_POINT('Ctrl Pts',(1.58872057258245,1.,1.32064537110892));
#41352=CARTESIAN_POINT('Ctrl Pts',(1.59471591079403,-1.,1.32224985747682));
#41353=CARTESIAN_POINT('Ctrl Pts',(1.59471591079403,1.,1.32224985747682));
#41354=CARTESIAN_POINT('Ctrl Pts',(1.60073511858687,-1.,1.32381550858256));
#41355=CARTESIAN_POINT('Ctrl Pts',(1.60073511858687,1.,1.32381550858256));
#41356=CARTESIAN_POINT('Ctrl Pts',(1.60677758290954,-1.,1.32534250785782));
#41357=CARTESIAN_POINT('Ctrl Pts',(1.60677758290954,1.,1.32534250785782));
#41358=CARTESIAN_POINT('Ctrl Pts',(1.6128423401575,-1.,1.32683074483356));
#41359=CARTESIAN_POINT('Ctrl Pts',(1.6128423401575,1.,1.32683074483356));
#41360=CARTESIAN_POINT('Ctrl Pts',(1.61892832270724,-1.,1.32828000610449));
#41361=CARTESIAN_POINT('Ctrl Pts',(1.61892832270724,1.,1.32828000610449));
#41362=CARTESIAN_POINT('Ctrl Pts',(1.62503464209797,-1.,1.3296901950568));
#41363=CARTESIAN_POINT('Ctrl Pts',(1.62503464209797,1.,1.3296901950568));
#41364=CARTESIAN_POINT('Ctrl Pts',(1.63116079730923,-1.,1.33106149345645));
#41365=CARTESIAN_POINT('Ctrl Pts',(1.63116079730923,1.,1.33106149345645));
#41366=CARTESIAN_POINT('Ctrl Pts',(1.63730653475089,-1.,1.33239425103724));
#41367=CARTESIAN_POINT('Ctrl Pts',(1.63730653475089,1.,1.33239425103724));
#41368=CARTESIAN_POINT('Ctrl Pts',(1.6434717485603,-1.,1.33368890676572));
#41369=CARTESIAN_POINT('Ctrl Pts',(1.6434717485603,1.,1.33368890676572));
#41370=CARTESIAN_POINT('Ctrl Pts',(1.6496563728683,-1.,1.33494590467993));
#41371=CARTESIAN_POINT('Ctrl Pts',(1.6496563728683,1.,1.33494590467993));
#41372=CARTESIAN_POINT('Ctrl Pts',(1.65586025952593,-1.,1.33616559745172));
#41373=CARTESIAN_POINT('Ctrl Pts',(1.65586025952593,1.,1.33616559745172));
#41374=CARTESIAN_POINT('Ctrl Pts',(1.66208312541983,-1.,1.33734820885262));
#41375=CARTESIAN_POINT('Ctrl Pts',(1.66208312541983,1.,1.33734820885262));
#41376=CARTESIAN_POINT('Ctrl Pts',(1.66832460783989,-1.,1.33849388654388));
#41377=CARTESIAN_POINT('Ctrl Pts',(1.66832460783989,1.,1.33849388654388));
#41378=CARTESIAN_POINT('Ctrl Pts',(1.67458429426086,-1.,1.3396027347034));
#41379=CARTESIAN_POINT('Ctrl Pts',(1.67458429426086,1.,1.3396027347034));
#41380=CARTESIAN_POINT('Ctrl Pts',(1.68086176030362,-1.,1.34067485185203));
#41381=CARTESIAN_POINT('Ctrl Pts',(1.68086176030362,1.,1.34067485185203));
#41382=CARTESIAN_POINT('Ctrl Pts',(1.68715660868764,-1.,1.341710374848));
#41383=CARTESIAN_POINT('Ctrl Pts',(1.68715660868764,1.,1.341710374848));
#41384=CARTESIAN_POINT('Ctrl Pts',(1.6934684849687,-1.,1.34270948206319));
#41385=CARTESIAN_POINT('Ctrl Pts',(1.6934684849687,1.,1.34270948206319));
#41386=CARTESIAN_POINT('Ctrl Pts',(1.69979707754427,-1.,1.34367237124483));
#41387=CARTESIAN_POINT('Ctrl Pts',(1.69979707754427,1.,1.34367237124483));
#41388=CARTESIAN_POINT('Ctrl Pts',(1.70614212266738,-1.,1.34459924533831));
#41389=CARTESIAN_POINT('Ctrl Pts',(1.70614212266738,1.,1.34459924533831));
#41390=CARTESIAN_POINT('Ctrl Pts',(1.71250340686822,-1.,1.34549029589416));
#41391=CARTESIAN_POINT('Ctrl Pts',(1.71250340686822,1.,1.34549029589416));
#41392=CARTESIAN_POINT('Ctrl Pts',(1.7188807715049,-1.,1.34634568653227));
#41393=CARTESIAN_POINT('Ctrl Pts',(1.7188807715049,1.,1.34634568653227));
#41394=CARTESIAN_POINT('Ctrl Pts',(1.72527410680674,-1.,1.34716554819527));
#41395=CARTESIAN_POINT('Ctrl Pts',(1.72527410680674,1.,1.34716554819527));
#41396=CARTESIAN_POINT('Ctrl Pts',(1.7304014965394,-1.,1.34779309152035));
#41397=CARTESIAN_POINT('Ctrl Pts',(1.7304014965394,1.,1.34779309152035));
#41398=CARTESIAN_POINT('Ctrl Pts',(1.73425417885907,-1.,1.34824783112887));
#41399=CARTESIAN_POINT('Ctrl Pts',(1.73425417885907,1.,1.34824783112887));
#41400=CARTESIAN_POINT('Ctrl Pts',(1.73682580585691,-1.,1.34854391898045));
#41401=CARTESIAN_POINT('Ctrl Pts',(1.73682580585691,1.,1.34854391898045));
#41402=CARTESIAN_POINT('Ctrl Pts',(1.73811241238545,-1.,1.34869019493419));
#41403=CARTESIAN_POINT('Ctrl Pts',(1.73811241238545,1.,1.34869019493419));
#41404=CARTESIAN_POINT('',(1.31362392696032,1.,1.15624053661742));
#41405=CARTESIAN_POINT('Ctrl Pts',(1.31362392696032,1.,1.15624053661742));
#41406=CARTESIAN_POINT('Ctrl Pts',(1.31722977216397,1.,1.15950888730809));
#41407=CARTESIAN_POINT('Ctrl Pts',(1.32428080721772,1.,1.16589330093588));
#41408=CARTESIAN_POINT('Ctrl Pts',(1.33437539347008,1.,1.17501305789857));
#41409=CARTESIAN_POINT('Ctrl Pts',(1.34687054001093,1.,1.18625865667441));
#41410=CARTESIAN_POINT('Ctrl Pts',(1.36088705043885,1.,1.1987959077932));
#41411=CARTESIAN_POINT('Ctrl Pts',(1.37331915607905,1.,1.20982812925645));
#41412=CARTESIAN_POINT('Ctrl Pts',(1.38420564527715,1.,1.21938737280852));
#41413=CARTESIAN_POINT('Ctrl Pts',(1.39361389568796,1.,1.22752961899387));
#41414=CARTESIAN_POINT('Ctrl Pts',(1.40164708206106,1.,1.23434087290423));
#41415=CARTESIAN_POINT('Ctrl Pts',(1.40845295531283,1.,1.23994455029534));
#41416=CARTESIAN_POINT('Ctrl Pts',(1.41422913175179,1.,1.24450600513056));
#41417=CARTESIAN_POINT('Ctrl Pts',(1.41923722596025,1.,1.24824430986571));
#41418=CARTESIAN_POINT('Ctrl Pts',(1.42378102115575,1.,1.2514145557001));
#41419=CARTESIAN_POINT('Ctrl Pts',(1.42815938799387,1.,1.25426945222639));
#41420=CARTESIAN_POINT('Ctrl Pts',(1.43262645609691,1.,1.25702687965755));
#41421=CARTESIAN_POINT('Ctrl Pts',(1.43734919180847,1.,1.25983531012005));
#41422=CARTESIAN_POINT('Ctrl Pts',(1.44236470511303,1.,1.26273903323859));
#41423=CARTESIAN_POINT('Ctrl Pts',(1.44761985001662,1.,1.26570925118868));
#41424=CARTESIAN_POINT('Ctrl Pts',(1.45301422764247,1.,1.2686778680489));
#41425=CARTESIAN_POINT('Ctrl Pts',(1.45843906294697,1.,1.27156805265289));
#41426=CARTESIAN_POINT('Ctrl Pts',(1.46382431332476,1.,1.27433119897822));
#41427=CARTESIAN_POINT('Ctrl Pts',(1.46916035917133,1.,1.2769641483109));
#41428=CARTESIAN_POINT('Ctrl Pts',(1.4744717526707,1.,1.2794891824849));
#41429=CARTESIAN_POINT('Ctrl Pts',(1.47980070347095,1.,1.28194158939517));
#41430=CARTESIAN_POINT('Ctrl Pts',(1.4851881711891,1.,1.28435533880201));
#41431=CARTESIAN_POINT('Ctrl Pts',(1.4906522831278,1.,1.2867467611644));
#41432=CARTESIAN_POINT('Ctrl Pts',(1.49618896881754,1.,1.28911506584254));
#41433=CARTESIAN_POINT('Ctrl Pts',(1.50178230149776,1.,1.29145022885181));
#41434=CARTESIAN_POINT('Ctrl Pts',(1.50741159078365,1.,1.29373841372842));
#41435=CARTESIAN_POINT('Ctrl Pts',(1.51305994241402,1.,1.29596850710509));
#41436=CARTESIAN_POINT('Ctrl Pts',(1.51872184912724,1.,1.29813791800747));
#41437=CARTESIAN_POINT('Ctrl Pts',(1.52439957861062,1.,1.30024984366328));
#41438=CARTESIAN_POINT('Ctrl Pts',(1.53009970283891,1.,1.30231064395568));
#41439=CARTESIAN_POINT('Ctrl Pts',(1.53582981268977,1.,1.30432735639489));
#41440=CARTESIAN_POINT('Ctrl Pts',(1.54159462645432,1.,1.30630475189556));
#41441=CARTESIAN_POINT('Ctrl Pts',(1.54739413957185,1.,1.30824393907473));
#41442=CARTESIAN_POINT('Ctrl Pts',(1.55322568759481,1.,1.31014393684222));
#41443=CARTESIAN_POINT('Ctrl Pts',(1.55908521254821,1.,1.31200264341696));
#41444=CARTESIAN_POINT('Ctrl Pts',(1.56496872402353,1.,1.31381795281002));
#41445=CARTESIAN_POINT('Ctrl Pts',(1.57087397835723,1.,1.31558903860016));
#41446=CARTESIAN_POINT('Ctrl Pts',(1.5768005650559,1.,1.31731642317187));
#41447=CARTESIAN_POINT('Ctrl Pts',(1.58274907898834,1.,1.31900135021432));
#41448=CARTESIAN_POINT('Ctrl Pts',(1.58872057258245,1.,1.32064537110892));
#41449=CARTESIAN_POINT('Ctrl Pts',(1.59471591079403,1.,1.32224985747682));
#41450=CARTESIAN_POINT('Ctrl Pts',(1.60073511858687,1.,1.32381550858256));
#41451=CARTESIAN_POINT('Ctrl Pts',(1.60677758290954,1.,1.32534250785782));
#41452=CARTESIAN_POINT('Ctrl Pts',(1.6128423401575,1.,1.32683074483356));
#41453=CARTESIAN_POINT('Ctrl Pts',(1.61892832270724,1.,1.32828000610449));
#41454=CARTESIAN_POINT('Ctrl Pts',(1.62503464209797,1.,1.3296901950568));
#41455=CARTESIAN_POINT('Ctrl Pts',(1.63116079730923,1.,1.33106149345645));
#41456=CARTESIAN_POINT('Ctrl Pts',(1.63730653475089,1.,1.33239425103724));
#41457=CARTESIAN_POINT('Ctrl Pts',(1.6434717485603,1.,1.33368890676572));
#41458=CARTESIAN_POINT('Ctrl Pts',(1.6496563728683,1.,1.33494590467993));
#41459=CARTESIAN_POINT('Ctrl Pts',(1.65586025952593,1.,1.33616559745172));
#41460=CARTESIAN_POINT('Ctrl Pts',(1.66208312541983,1.,1.33734820885262));
#41461=CARTESIAN_POINT('Ctrl Pts',(1.66832460783989,1.,1.33849388654388));
#41462=CARTESIAN_POINT('Ctrl Pts',(1.67458429426086,1.,1.3396027347034));
#41463=CARTESIAN_POINT('Ctrl Pts',(1.68086176030362,1.,1.34067485185203));
#41464=CARTESIAN_POINT('Ctrl Pts',(1.68715660868764,1.,1.341710374848));
#41465=CARTESIAN_POINT('Ctrl Pts',(1.6934684849687,1.,1.34270948206319));
#41466=CARTESIAN_POINT('Ctrl Pts',(1.69979707754427,1.,1.34367237124483));
#41467=CARTESIAN_POINT('Ctrl Pts',(1.70614212266738,1.,1.34459924533831));
#41468=CARTESIAN_POINT('Ctrl Pts',(1.71250340686822,1.,1.34549029589416));
#41469=CARTESIAN_POINT('Ctrl Pts',(1.7188807715049,1.,1.34634568653227));
#41470=CARTESIAN_POINT('Ctrl Pts',(1.72527410680674,1.,1.34716554819527));
#41471=CARTESIAN_POINT('Ctrl Pts',(1.7304014965394,1.,1.34779309152035));
#41472=CARTESIAN_POINT('Ctrl Pts',(1.73425417885907,1.,1.34824783112887));
#41473=CARTESIAN_POINT('Ctrl Pts',(1.73682580585691,1.,1.34854391898045));
#41474=CARTESIAN_POINT('Ctrl Pts',(1.73811241238545,1.,1.34869019493419));
#41475=CARTESIAN_POINT('',(1.31362392696032,0.,1.15624053661742));
#41476=CARTESIAN_POINT('Origin',(0.,0.,0.));
#41477=CARTESIAN_POINT('',(1.15624053661742,1.,1.31362392696033));
#41478=CARTESIAN_POINT('Origin',(0.,1.,0.));
#41479=CARTESIAN_POINT('',(1.15624053661742,0.,1.31362392696032));
#41480=CARTESIAN_POINT('Ctrl Pts',(1.34869019493419,-1.,1.73811241238545));
#41481=CARTESIAN_POINT('Ctrl Pts',(1.34869019493419,1.,1.73811241238545));
#41482=CARTESIAN_POINT('Ctrl Pts',(1.34854391898145,-1.,1.73682580585819));
#41483=CARTESIAN_POINT('Ctrl Pts',(1.34854391898145,1.,1.73682580585819));
#41484=CARTESIAN_POINT('Ctrl Pts',(1.34824783113158,-1.,1.73425417886255));
#41485=CARTESIAN_POINT('Ctrl Pts',(1.34824783113158,1.,1.73425417886255));
#41486=CARTESIAN_POINT('Ctrl Pts',(1.3477930915247,-1.,1.73040149654497));
#41487=CARTESIAN_POINT('Ctrl Pts',(1.3477930915247,1.,1.73040149654497));
#41488=CARTESIAN_POINT('Ctrl Pts',(1.34716554820013,-1.,1.72527410681298));
#41489=CARTESIAN_POINT('Ctrl Pts',(1.34716554820013,1.,1.72527410681298));
#41490=CARTESIAN_POINT('Ctrl Pts',(1.34634568653586,-1.,1.7188807715095));
#41491=CARTESIAN_POINT('Ctrl Pts',(1.34634568653586,1.,1.7188807715095));
#41492=CARTESIAN_POINT('Ctrl Pts',(1.34549029589563,-1.,1.71250340687011));
#41493=CARTESIAN_POINT('Ctrl Pts',(1.34549029589563,1.,1.71250340687011));
#41494=CARTESIAN_POINT('Ctrl Pts',(1.34459924533783,-1.,1.70614212266676));
#41495=CARTESIAN_POINT('Ctrl Pts',(1.34459924533783,1.,1.70614212266676));
#41496=CARTESIAN_POINT('Ctrl Pts',(1.34367237124322,-1.,1.69979707754221));
#41497=CARTESIAN_POINT('Ctrl Pts',(1.34367237124322,1.,1.69979707754221));
#41498=CARTESIAN_POINT('Ctrl Pts',(1.34270948206139,-1.,1.6934684849664));
#41499=CARTESIAN_POINT('Ctrl Pts',(1.34270948206139,1.,1.6934684849664));
#41500=CARTESIAN_POINT('Ctrl Pts',(1.34171037484673,-1.,1.68715660868602));
#41501=CARTESIAN_POINT('Ctrl Pts',(1.34171037484673,1.,1.68715660868602));
#41502=CARTESIAN_POINT('Ctrl Pts',(1.3406748518516,-1.,1.68086176030308));
#41503=CARTESIAN_POINT('Ctrl Pts',(1.3406748518516,1.,1.68086176030308));
#41504=CARTESIAN_POINT('Ctrl Pts',(1.33960273470372,-1.,1.67458429426126));
#41505=CARTESIAN_POINT('Ctrl Pts',(1.33960273470372,1.,1.67458429426126));
#41506=CARTESIAN_POINT('Ctrl Pts',(1.33849388654458,-1.,1.66832460784078));
#41507=CARTESIAN_POINT('Ctrl Pts',(1.33849388654458,1.,1.66832460784078));
#41508=CARTESIAN_POINT('Ctrl Pts',(1.33734820885331,-1.,1.66208312542073));
#41509=CARTESIAN_POINT('Ctrl Pts',(1.33734820885331,1.,1.66208312542073));
#41510=CARTESIAN_POINT('Ctrl Pts',(1.33616559745217,-1.,1.65586025952651));
#41511=CARTESIAN_POINT('Ctrl Pts',(1.33616559745217,1.,1.65586025952651));
#41512=CARTESIAN_POINT('Ctrl Pts',(1.33494590468003,-1.,1.64965637286843));
#41513=CARTESIAN_POINT('Ctrl Pts',(1.33494590468003,1.,1.64965637286843));
#41514=CARTESIAN_POINT('Ctrl Pts',(1.33368890676554,-1.,1.64347174856007));
#41515=CARTESIAN_POINT('Ctrl Pts',(1.33368890676554,1.,1.64347174856007));
#41516=CARTESIAN_POINT('Ctrl Pts',(1.33239425103694,-1.,1.6373065347505));
#41517=CARTESIAN_POINT('Ctrl Pts',(1.33239425103694,1.,1.6373065347505));
#41518=CARTESIAN_POINT('Ctrl Pts',(1.33106149345618,-1.,1.63116079730887));
#41519=CARTESIAN_POINT('Ctrl Pts',(1.33106149345618,1.,1.63116079730887));
#41520=CARTESIAN_POINT('Ctrl Pts',(1.32969019505665,-1.,1.62503464209777));
#41521=CARTESIAN_POINT('Ctrl Pts',(1.32969019505665,1.,1.62503464209777));
#41522=CARTESIAN_POINT('Ctrl Pts',(1.32828000610448,-1.,1.61892832270723));
#41523=CARTESIAN_POINT('Ctrl Pts',(1.32828000610448,1.,1.61892832270723));
#41524=CARTESIAN_POINT('Ctrl Pts',(1.32683074483365,-1.,1.61284234015762));
#41525=CARTESIAN_POINT('Ctrl Pts',(1.32683074483365,1.,1.61284234015762));
#41526=CARTESIAN_POINT('Ctrl Pts',(1.32534250785794,-1.,1.6067775829097));
#41527=CARTESIAN_POINT('Ctrl Pts',(1.32534250785794,1.,1.6067775829097));
#41528=CARTESIAN_POINT('Ctrl Pts',(1.32381550858266,-1.,1.600735118587));
#41529=CARTESIAN_POINT('Ctrl Pts',(1.32381550858266,1.,1.600735118587));
#41530=CARTESIAN_POINT('Ctrl Pts',(1.32224985747686,-1.,1.59471591079408));
#41531=CARTESIAN_POINT('Ctrl Pts',(1.32224985747686,1.,1.59471591079408));
#41532=CARTESIAN_POINT('Ctrl Pts',(1.32064537110891,-1.,1.58872057258244));
#41533=CARTESIAN_POINT('Ctrl Pts',(1.32064537110891,1.,1.58872057258244));
#41534=CARTESIAN_POINT('Ctrl Pts',(1.31900135021428,-1.,1.58274907898829));
#41535=CARTESIAN_POINT('Ctrl Pts',(1.31900135021428,1.,1.58274907898829));
#41536=CARTESIAN_POINT('Ctrl Pts',(1.31731642317183,-1.,1.57680056505585));
#41537=CARTESIAN_POINT('Ctrl Pts',(1.31731642317183,1.,1.57680056505585));
#41538=CARTESIAN_POINT('Ctrl Pts',(1.31558903860015,-1.,1.57087397835721));
#41539=CARTESIAN_POINT('Ctrl Pts',(1.31558903860015,1.,1.57087397835721));
#41540=CARTESIAN_POINT('Ctrl Pts',(1.31381795281002,-1.,1.56496872402352));
#41541=CARTESIAN_POINT('Ctrl Pts',(1.31381795281002,1.,1.56496872402352));
#41542=CARTESIAN_POINT('Ctrl Pts',(1.31200264341696,-1.,1.55908521254822));
#41543=CARTESIAN_POINT('Ctrl Pts',(1.31200264341696,1.,1.55908521254822));
#41544=CARTESIAN_POINT('Ctrl Pts',(1.31014393684221,-1.,1.55322568759481));
#41545=CARTESIAN_POINT('Ctrl Pts',(1.31014393684221,1.,1.55322568759481));
#41546=CARTESIAN_POINT('Ctrl Pts',(1.30824393907471,-1.,1.54739413957183));
#41547=CARTESIAN_POINT('Ctrl Pts',(1.30824393907471,1.,1.54739413957183));
#41548=CARTESIAN_POINT('Ctrl Pts',(1.30630475189553,-1.,1.54159462645428));
#41549=CARTESIAN_POINT('Ctrl Pts',(1.30630475189553,1.,1.54159462645428));
#41550=CARTESIAN_POINT('Ctrl Pts',(1.30432735639487,-1.,1.53582981268976));
#41551=CARTESIAN_POINT('Ctrl Pts',(1.30432735639487,1.,1.53582981268976));
#41552=CARTESIAN_POINT('Ctrl Pts',(1.3023106439557,-1.,1.53009970283893));
#41553=CARTESIAN_POINT('Ctrl Pts',(1.3023106439557,1.,1.53009970283893));
#41554=CARTESIAN_POINT('Ctrl Pts',(1.30024984366334,-1.,1.5243995786107));
#41555=CARTESIAN_POINT('Ctrl Pts',(1.30024984366334,1.,1.5243995786107));
#41556=CARTESIAN_POINT('Ctrl Pts',(1.29813791800757,-1.,1.51872184912735));
#41557=CARTESIAN_POINT('Ctrl Pts',(1.29813791800757,1.,1.51872184912735));
#41558=CARTESIAN_POINT('Ctrl Pts',(1.29596850710518,-1.,1.51305994241412));
#41559=CARTESIAN_POINT('Ctrl Pts',(1.29596850710518,1.,1.51305994241412));
#41560=CARTESIAN_POINT('Ctrl Pts',(1.29373841372843,-1.,1.50741159078367));
#41561=CARTESIAN_POINT('Ctrl Pts',(1.29373841372843,1.,1.50741159078367));
#41562=CARTESIAN_POINT('Ctrl Pts',(1.29145022885171,-1.,1.50178230149764));
#41563=CARTESIAN_POINT('Ctrl Pts',(1.29145022885171,1.,1.50178230149764));
#41564=CARTESIAN_POINT('Ctrl Pts',(1.28911506584232,-1.,1.49618896881729));
#41565=CARTESIAN_POINT('Ctrl Pts',(1.28911506584232,1.,1.49618896881729));
#41566=CARTESIAN_POINT('Ctrl Pts',(1.28674676116415,-1.,1.4906522831275));
#41567=CARTESIAN_POINT('Ctrl Pts',(1.28674676116415,1.,1.4906522831275));
#41568=CARTESIAN_POINT('Ctrl Pts',(1.28435533880184,-1.,1.48518817118891));
#41569=CARTESIAN_POINT('Ctrl Pts',(1.28435533880184,1.,1.48518817118891));
#41570=CARTESIAN_POINT('Ctrl Pts',(1.28194158939522,-1.,1.47980070347102));
#41571=CARTESIAN_POINT('Ctrl Pts',(1.28194158939522,1.,1.47980070347102));
#41572=CARTESIAN_POINT('Ctrl Pts',(1.27948918248524,-1.,1.4744717526711));
#41573=CARTESIAN_POINT('Ctrl Pts',(1.27948918248524,1.,1.4744717526711));
#41574=CARTESIAN_POINT('Ctrl Pts',(1.27696414831144,-1.,1.46916035917197));
#41575=CARTESIAN_POINT('Ctrl Pts',(1.27696414831144,1.,1.46916035917197));
#41576=CARTESIAN_POINT('Ctrl Pts',(1.27433119897877,-1.,1.4638243133254));
#41577=CARTESIAN_POINT('Ctrl Pts',(1.27433119897877,1.,1.4638243133254));
#41578=CARTESIAN_POINT('Ctrl Pts',(1.27156805265312,-1.,1.45843906294725));
#41579=CARTESIAN_POINT('Ctrl Pts',(1.27156805265312,1.,1.45843906294725));
#41580=CARTESIAN_POINT('Ctrl Pts',(1.26867786804854,-1.,1.45301422764205));
#41581=CARTESIAN_POINT('Ctrl Pts',(1.26867786804854,1.,1.45301422764205));
#41582=CARTESIAN_POINT('Ctrl Pts',(1.26570925118767,-1.,1.44761985001544));
#41583=CARTESIAN_POINT('Ctrl Pts',(1.26570925118767,1.,1.44761985001544));
#41584=CARTESIAN_POINT('Ctrl Pts',(1.26273903323723,-1.,1.44236470511145));
#41585=CARTESIAN_POINT('Ctrl Pts',(1.26273903323723,1.,1.44236470511145));
#41586=CARTESIAN_POINT('Ctrl Pts',(1.25983531011894,-1.,1.43734919180719));
#41587=CARTESIAN_POINT('Ctrl Pts',(1.25983531011894,1.,1.43734919180719));
#41588=CARTESIAN_POINT('Ctrl Pts',(1.25702687965744,-1.,1.43262645609679));
#41589=CARTESIAN_POINT('Ctrl Pts',(1.25702687965744,1.,1.43262645609679));
#41590=CARTESIAN_POINT('Ctrl Pts',(1.25426945222783,-1.,1.42815938799555));
#41591=CARTESIAN_POINT('Ctrl Pts',(1.25426945222783,1.,1.42815938799555));
#41592=CARTESIAN_POINT('Ctrl Pts',(1.25141455570299,-1.,1.42378102115911));
#41593=CARTESIAN_POINT('Ctrl Pts',(1.25141455570299,1.,1.42378102115911));
#41594=CARTESIAN_POINT('Ctrl Pts',(1.24824430986911,-1.,1.41923722596421));
#41595=CARTESIAN_POINT('Ctrl Pts',(1.24824430986911,1.,1.41923722596421));
#41596=CARTESIAN_POINT('Ctrl Pts',(1.24450600513278,-1.,1.41422913175437));
#41597=CARTESIAN_POINT('Ctrl Pts',(1.24450600513278,1.,1.41422913175437));
#41598=CARTESIAN_POINT('Ctrl Pts',(1.23994455029421,-1.,1.40845295531151));
#41599=CARTESIAN_POINT('Ctrl Pts',(1.23994455029421,1.,1.40845295531151));
#41600=CARTESIAN_POINT('Ctrl Pts',(1.23434087289768,-1.,1.40164708205345));
#41601=CARTESIAN_POINT('Ctrl Pts',(1.23434087289768,1.,1.40164708205345));
#41602=CARTESIAN_POINT('Ctrl Pts',(1.22752961898063,-1.,1.39361389567257));
#41603=CARTESIAN_POINT('Ctrl Pts',(1.22752961898063,1.,1.39361389567257));
#41604=CARTESIAN_POINT('Ctrl Pts',(1.21938737278853,-1.,1.38420564525391));
#41605=CARTESIAN_POINT('Ctrl Pts',(1.21938737278853,1.,1.38420564525391));
#41606=CARTESIAN_POINT('Ctrl Pts',(1.20982812923113,-1.,1.37331915604962));
#41607=CARTESIAN_POINT('Ctrl Pts',(1.20982812923113,1.,1.37331915604962));
#41608=CARTESIAN_POINT('Ctrl Pts',(1.1987959077656,-1.,1.36088705040677));
#41609=CARTESIAN_POINT('Ctrl Pts',(1.1987959077656,1.,1.36088705040677));
#41610=CARTESIAN_POINT('Ctrl Pts',(1.18625865664915,-1.,1.34687053998157));
#41611=CARTESIAN_POINT('Ctrl Pts',(1.18625865664915,1.,1.34687053998157));
#41612=CARTESIAN_POINT('Ctrl Pts',(1.17501305787994,-1.,1.33437539344842));
#41613=CARTESIAN_POINT('Ctrl Pts',(1.17501305787994,1.,1.33437539344842));
#41614=CARTESIAN_POINT('Ctrl Pts',(1.16589330092532,-1.,1.32428080720544));
#41615=CARTESIAN_POINT('Ctrl Pts',(1.16589330092532,1.,1.32428080720544));
#41616=CARTESIAN_POINT('Ctrl Pts',(1.15950888730433,-1.,1.3172297721596));
#41617=CARTESIAN_POINT('Ctrl Pts',(1.15950888730433,1.,1.3172297721596));
#41618=CARTESIAN_POINT('Ctrl Pts',(1.15624053661742,-1.,1.31362392696033));
#41619=CARTESIAN_POINT('Ctrl Pts',(1.15624053661742,1.,1.31362392696033));
#41620=CARTESIAN_POINT('',(1.34869019493419,1.,1.73811241238545));
#41621=CARTESIAN_POINT('Ctrl Pts',(1.34869019493419,1.,1.73811241238545));
#41622=CARTESIAN_POINT('Ctrl Pts',(1.34854391898145,1.,1.73682580585819));
#41623=CARTESIAN_POINT('Ctrl Pts',(1.34824783113158,1.,1.73425417886255));
#41624=CARTESIAN_POINT('Ctrl Pts',(1.3477930915247,1.,1.73040149654497));
#41625=CARTESIAN_POINT('Ctrl Pts',(1.34716554820013,1.,1.72527410681298));
#41626=CARTESIAN_POINT('Ctrl Pts',(1.34634568653586,1.,1.7188807715095));
#41627=CARTESIAN_POINT('Ctrl Pts',(1.34549029589563,1.,1.71250340687011));
#41628=CARTESIAN_POINT('Ctrl Pts',(1.34459924533783,1.,1.70614212266676));
#41629=CARTESIAN_POINT('Ctrl Pts',(1.34367237124322,1.,1.69979707754221));
#41630=CARTESIAN_POINT('Ctrl Pts',(1.34270948206139,1.,1.6934684849664));
#41631=CARTESIAN_POINT('Ctrl Pts',(1.34171037484673,1.,1.68715660868602));
#41632=CARTESIAN_POINT('Ctrl Pts',(1.3406748518516,1.,1.68086176030308));
#41633=CARTESIAN_POINT('Ctrl Pts',(1.33960273470372,1.,1.67458429426126));
#41634=CARTESIAN_POINT('Ctrl Pts',(1.33849388654458,1.,1.66832460784078));
#41635=CARTESIAN_POINT('Ctrl Pts',(1.33734820885331,1.,1.66208312542073));
#41636=CARTESIAN_POINT('Ctrl Pts',(1.33616559745217,1.,1.65586025952651));
#41637=CARTESIAN_POINT('Ctrl Pts',(1.33494590468003,1.,1.64965637286843));
#41638=CARTESIAN_POINT('Ctrl Pts',(1.33368890676554,1.,1.64347174856007));
#41639=CARTESIAN_POINT('Ctrl Pts',(1.33239425103694,1.,1.6373065347505));
#41640=CARTESIAN_POINT('Ctrl Pts',(1.33106149345618,1.,1.63116079730887));
#41641=CARTESIAN_POINT('Ctrl Pts',(1.32969019505665,1.,1.62503464209777));
#41642=CARTESIAN_POINT('Ctrl Pts',(1.32828000610448,1.,1.61892832270723));
#41643=CARTESIAN_POINT('Ctrl Pts',(1.32683074483365,1.,1.61284234015762));
#41644=CARTESIAN_POINT('Ctrl Pts',(1.32534250785794,1.,1.6067775829097));
#41645=CARTESIAN_POINT('Ctrl Pts',(1.32381550858266,1.,1.600735118587));
#41646=CARTESIAN_POINT('Ctrl Pts',(1.32224985747686,1.,1.59471591079408));
#41647=CARTESIAN_POINT('Ctrl Pts',(1.32064537110891,1.,1.58872057258244));
#41648=CARTESIAN_POINT('Ctrl Pts',(1.31900135021428,1.,1.58274907898829));
#41649=CARTESIAN_POINT('Ctrl Pts',(1.31731642317183,1.,1.57680056505585));
#41650=CARTESIAN_POINT('Ctrl Pts',(1.31558903860015,1.,1.57087397835721));
#41651=CARTESIAN_POINT('Ctrl Pts',(1.31381795281002,1.,1.56496872402352));
#41652=CARTESIAN_POINT('Ctrl Pts',(1.31200264341696,1.,1.55908521254822));
#41653=CARTESIAN_POINT('Ctrl Pts',(1.31014393684221,1.,1.55322568759481));
#41654=CARTESIAN_POINT('Ctrl Pts',(1.30824393907471,1.,1.54739413957183));
#41655=CARTESIAN_POINT('Ctrl Pts',(1.30630475189553,1.,1.54159462645428));
#41656=CARTESIAN_POINT('Ctrl Pts',(1.30432735639487,1.,1.53582981268976));
#41657=CARTESIAN_POINT('Ctrl Pts',(1.3023106439557,1.,1.53009970283893));
#41658=CARTESIAN_POINT('Ctrl Pts',(1.30024984366334,1.,1.5243995786107));
#41659=CARTESIAN_POINT('Ctrl Pts',(1.29813791800757,1.,1.51872184912735));
#41660=CARTESIAN_POINT('Ctrl Pts',(1.29596850710518,1.,1.51305994241412));
#41661=CARTESIAN_POINT('Ctrl Pts',(1.29373841372843,1.,1.50741159078367));
#41662=CARTESIAN_POINT('Ctrl Pts',(1.29145022885171,1.,1.50178230149764));
#41663=CARTESIAN_POINT('Ctrl Pts',(1.28911506584232,1.,1.49618896881729));
#41664=CARTESIAN_POINT('Ctrl Pts',(1.28674676116415,1.,1.4906522831275));
#41665=CARTESIAN_POINT('Ctrl Pts',(1.28435533880184,1.,1.48518817118891));
#41666=CARTESIAN_POINT('Ctrl Pts',(1.28194158939522,1.,1.47980070347102));
#41667=CARTESIAN_POINT('Ctrl Pts',(1.27948918248524,1.,1.4744717526711));
#41668=CARTESIAN_POINT('Ctrl Pts',(1.27696414831144,1.,1.46916035917197));
#41669=CARTESIAN_POINT('Ctrl Pts',(1.27433119897877,1.,1.4638243133254));
#41670=CARTESIAN_POINT('Ctrl Pts',(1.27156805265312,1.,1.45843906294725));
#41671=CARTESIAN_POINT('Ctrl Pts',(1.26867786804854,1.,1.45301422764205));
#41672=CARTESIAN_POINT('Ctrl Pts',(1.26570925118767,1.,1.44761985001544));
#41673=CARTESIAN_POINT('Ctrl Pts',(1.26273903323723,1.,1.44236470511145));
#41674=CARTESIAN_POINT('Ctrl Pts',(1.25983531011894,1.,1.43734919180719));
#41675=CARTESIAN_POINT('Ctrl Pts',(1.25702687965744,1.,1.43262645609679));
#41676=CARTESIAN_POINT('Ctrl Pts',(1.25426945222783,1.,1.42815938799555));
#41677=CARTESIAN_POINT('Ctrl Pts',(1.25141455570299,1.,1.42378102115911));
#41678=CARTESIAN_POINT('Ctrl Pts',(1.24824430986911,1.,1.41923722596421));
#41679=CARTESIAN_POINT('Ctrl Pts',(1.24450600513278,1.,1.41422913175437));
#41680=CARTESIAN_POINT('Ctrl Pts',(1.23994455029421,1.,1.40845295531151));
#41681=CARTESIAN_POINT('Ctrl Pts',(1.23434087289768,1.,1.40164708205345));
#41682=CARTESIAN_POINT('Ctrl Pts',(1.22752961898063,1.,1.39361389567257));
#41683=CARTESIAN_POINT('Ctrl Pts',(1.21938737278853,1.,1.38420564525391));
#41684=CARTESIAN_POINT('Ctrl Pts',(1.20982812923113,1.,1.37331915604962));
#41685=CARTESIAN_POINT('Ctrl Pts',(1.1987959077656,1.,1.36088705040677));
#41686=CARTESIAN_POINT('Ctrl Pts',(1.18625865664915,1.,1.34687053998157));
#41687=CARTESIAN_POINT('Ctrl Pts',(1.17501305787994,1.,1.33437539344842));
#41688=CARTESIAN_POINT('Ctrl Pts',(1.16589330092532,1.,1.32428080720544));
#41689=CARTESIAN_POINT('Ctrl Pts',(1.15950888730433,1.,1.3172297721596));
#41690=CARTESIAN_POINT('Ctrl Pts',(1.15624053661742,1.,1.31362392696033));
#41691=CARTESIAN_POINT('',(1.34869019493419,0.,1.73811241238545));
#41692=CARTESIAN_POINT('Origin',(1.23627494547115,0.,1.81978687191668));
#41693=CARTESIAN_POINT('',(1.23627494547115,1.,1.81978687191668));
#41694=CARTESIAN_POINT('',(1.34869019493419,1.,1.73811241238545));
#41695=CARTESIAN_POINT('',(1.23627494547115,0.,1.81978687191668));
#41696=CARTESIAN_POINT('Ctrl Pts',(0.892032620296855,-1.,1.5055822144029));
#41697=CARTESIAN_POINT('Ctrl Pts',(0.892032620296855,1.,1.5055822144029));
#41698=CARTESIAN_POINT('Ctrl Pts',(0.894452006967538,-1.,1.50980486807181));
#41699=CARTESIAN_POINT('Ctrl Pts',(0.894452006967538,1.,1.50980486807181));
#41700=CARTESIAN_POINT('Ctrl Pts',(0.89918504749193,-1.,1.51805569591479));
#41701=CARTESIAN_POINT('Ctrl Pts',(0.89918504749193,1.,1.51805569591479));
#41702=CARTESIAN_POINT('Ctrl Pts',(0.905967409640498,-1.,1.52984849890434));
#41703=CARTESIAN_POINT('Ctrl Pts',(0.905967409640498,1.,1.52984849890434));
#41704=CARTESIAN_POINT('Ctrl Pts',(0.914375919046579,-1.,1.54440491152808));
#41705=CARTESIAN_POINT('Ctrl Pts',(0.914375919046579,1.,1.54440491152808));
#41706=CARTESIAN_POINT('Ctrl Pts',(0.923832188966322,-1.,1.56065988582509));
#41707=CARTESIAN_POINT('Ctrl Pts',(0.923832188966322,1.,1.56065988582509));
#41708=CARTESIAN_POINT('Ctrl Pts',(0.932246680128848,-1.,1.57499388385561));
#41709=CARTESIAN_POINT('Ctrl Pts',(0.932246680128848,1.,1.57499388385561));
#41710=CARTESIAN_POINT('Ctrl Pts',(0.939646377909319,-1.,1.58744937489796));
#41711=CARTESIAN_POINT('Ctrl Pts',(0.939646377909319,1.,1.58744937489796));
#41712=CARTESIAN_POINT('Ctrl Pts',(0.946078063325795,-1.,1.59810042045408));
#41713=CARTESIAN_POINT('Ctrl Pts',(0.946078063325795,1.,1.59810042045408));
#41714=CARTESIAN_POINT('Ctrl Pts',(0.951613284361247,-1.,1.60706069897794));
#41715=CARTESIAN_POINT('Ctrl Pts',(0.951613284361247,1.,1.60706069897794));
#41716=CARTESIAN_POINT('Ctrl Pts',(0.956354422921572,-1.,1.61449324337233));
#41717=CARTESIAN_POINT('Ctrl Pts',(0.956354422921572,1.,1.61449324337233));
#41718=CARTESIAN_POINT('Ctrl Pts',(0.960438326099958,-1.,1.62061638139929));
#41719=CARTESIAN_POINT('Ctrl Pts',(0.960438326099958,1.,1.62061638139929));
#41720=CARTESIAN_POINT('Ctrl Pts',(0.964046107037821,-1.,1.6257193066974));
#41721=CARTESIAN_POINT('Ctrl Pts',(0.964046107037821,1.,1.6257193066974));
#41722=CARTESIAN_POINT('Ctrl Pts',(0.967387853228041,-1.,1.63013849959083));
#41723=CARTESIAN_POINT('Ctrl Pts',(0.967387853228041,1.,1.63013849959083));
#41724=CARTESIAN_POINT('Ctrl Pts',(0.970669715996356,-1.,1.63420665729609));
#41725=CARTESIAN_POINT('Ctrl Pts',(0.970669715996356,1.,1.63420665729609));
#41726=CARTESIAN_POINT('Ctrl Pts',(0.974066058287501,-1.,1.63820952658157));
#41727=CARTESIAN_POINT('Ctrl Pts',(0.974066058287501,1.,1.63820952658157));
#41728=CARTESIAN_POINT('Ctrl Pts',(0.977689794120296,-1.,1.64233990826831));
#41729=CARTESIAN_POINT('Ctrl Pts',(0.977689794120296,1.,1.64233990826831));
#41730=CARTESIAN_POINT('Ctrl Pts',(0.981562530940574,-1.,1.64665139190834));
#41731=CARTESIAN_POINT('Ctrl Pts',(0.981562530940574,1.,1.64665139190834));
#41732=CARTESIAN_POINT('Ctrl Pts',(0.985642622921626,-1.,1.6511001661277));
#41733=CARTESIAN_POINT('Ctrl Pts',(0.985642622921626,1.,1.6511001661277));
#41734=CARTESIAN_POINT('Ctrl Pts',(0.98985562785445,-1.,1.65559044289746));
#41735=CARTESIAN_POINT('Ctrl Pts',(0.98985562785445,1.,1.65559044289746));
#41736=CARTESIAN_POINT('Ctrl Pts',(0.994121836661115,-1.,1.66001553809916));
#41737=CARTESIAN_POINT('Ctrl Pts',(0.994121836661115,1.,1.66001553809916));
#41738=CARTESIAN_POINT('Ctrl Pts',(0.998389654952317,-1.,1.66430758030304));
#41739=CARTESIAN_POINT('Ctrl Pts',(0.998389654952317,1.,1.66430758030304));
#41740=CARTESIAN_POINT('Ctrl Pts',(1.00265091003682,-1.,1.66846059277231));
#41741=CARTESIAN_POINT('Ctrl Pts',(1.00265091003682,1.,1.66846059277231));
#41742=CARTESIAN_POINT('Ctrl Pts',(1.00692206696387,-1.,1.67250335383248));
#41743=CARTESIAN_POINT('Ctrl Pts',(1.00692206696387,1.,1.67250335383248));
#41744=CARTESIAN_POINT('Ctrl Pts',(1.01123236493507,-1.,1.67648246776457));
#41745=CARTESIAN_POINT('Ctrl Pts',(1.01123236493507,1.,1.67648246776457));
#41746=CARTESIAN_POINT('Ctrl Pts',(1.01561026162786,-1.,1.6804428989482));
#41747=CARTESIAN_POINT('Ctrl Pts',(1.01561026162786,1.,1.6804428989482));
#41748=CARTESIAN_POINT('Ctrl Pts',(1.02006795074222,-1.,1.68440578021739));
#41749=CARTESIAN_POINT('Ctrl Pts',(1.02006795074222,1.,1.68440578021739));
#41750=CARTESIAN_POINT('Ctrl Pts',(1.02460180535272,-1.,1.68836910178475));
#41751=CARTESIAN_POINT('Ctrl Pts',(1.02460180535272,1.,1.68836910178475));
#41752=CARTESIAN_POINT('Ctrl Pts',(1.02919977579155,-1.,1.69231840863471));
#41753=CARTESIAN_POINT('Ctrl Pts',(1.02919977579155,1.,1.69231840863471));
#41754=CARTESIAN_POINT('Ctrl Pts',(1.03384646003587,-1.,1.69623414782769));
#41755=CARTESIAN_POINT('Ctrl Pts',(1.03384646003587,1.,1.69623414782769));
#41756=CARTESIAN_POINT('Ctrl Pts',(1.03852922490782,-1.,1.70010052930951));
#41757=CARTESIAN_POINT('Ctrl Pts',(1.03852922490782,1.,1.70010052930951));
#41758=CARTESIAN_POINT('Ctrl Pts',(1.04324363334546,-1.,1.70391338707969));
#41759=CARTESIAN_POINT('Ctrl Pts',(1.04324363334546,1.,1.70391338707969));
#41760=CARTESIAN_POINT('Ctrl Pts',(1.0479908540499,-1.,1.70767646263641));
#41761=CARTESIAN_POINT('Ctrl Pts',(1.0479908540499,1.,1.70767646263641));
#41762=CARTESIAN_POINT('Ctrl Pts',(1.05277517202853,-1.,1.71139783543986));
#41763=CARTESIAN_POINT('Ctrl Pts',(1.05277517202853,1.,1.71139783543986));
#41764=CARTESIAN_POINT('Ctrl Pts',(1.05760163192481,-1.,1.71508654427022));
#41765=CARTESIAN_POINT('Ctrl Pts',(1.05760163192481,1.,1.71508654427022));
#41766=CARTESIAN_POINT('Ctrl Pts',(1.06247324680649,-1.,1.71874858456908));
#41767=CARTESIAN_POINT('Ctrl Pts',(1.06247324680649,1.,1.71874858456908));
#41768=CARTESIAN_POINT('Ctrl Pts',(1.06738966975463,-1.,1.72238500928456));
#41769=CARTESIAN_POINT('Ctrl Pts',(1.06738966975463,1.,1.72238500928456));
#41770=CARTESIAN_POINT('Ctrl Pts',(1.07234866990252,-1.,1.72599406198489));
#41771=CARTESIAN_POINT('Ctrl Pts',(1.07234866990252,1.,1.72599406198489));
#41772=CARTESIAN_POINT('Ctrl Pts',(1.0773470373727,-1.,1.72957248977424));
#41773=CARTESIAN_POINT('Ctrl Pts',(1.0773470373727,1.,1.72957248977424));
#41774=CARTESIAN_POINT('Ctrl Pts',(1.08238162784749,-1.,1.73311705663407));
#41775=CARTESIAN_POINT('Ctrl Pts',(1.08238162784749,1.,1.73311705663407));
#41776=CARTESIAN_POINT('Ctrl Pts',(1.08745056285429,-1.,1.73662628326093));
#41777=CARTESIAN_POINT('Ctrl Pts',(1.08745056285429,1.,1.73662628326093));
#41778=CARTESIAN_POINT('Ctrl Pts',(1.09255329056496,-1.,1.74010053962252));
#41779=CARTESIAN_POINT('Ctrl Pts',(1.09255329056496,1.,1.74010053962252));
#41780=CARTESIAN_POINT('Ctrl Pts',(1.09768999241229,-1.,1.74354119236212));
#41781=CARTESIAN_POINT('Ctrl Pts',(1.09768999241229,1.,1.74354119236212));
#41782=CARTESIAN_POINT('Ctrl Pts',(1.10286118991144,-1.,1.74695004214924));
#41783=CARTESIAN_POINT('Ctrl Pts',(1.10286118991144,1.,1.74695004214924));
#41784=CARTESIAN_POINT('Ctrl Pts',(1.10806728183003,-1.,1.75032866075914));
#41785=CARTESIAN_POINT('Ctrl Pts',(1.10806728183003,1.,1.75032866075914));
#41786=CARTESIAN_POINT('Ctrl Pts',(1.11330807582542,-1.,1.75367772094617));
#41787=CARTESIAN_POINT('Ctrl Pts',(1.11330807582542,1.,1.75367772094617));
#41788=CARTESIAN_POINT('Ctrl Pts',(1.11858293216752,-1.,1.75699720772089));
#41789=CARTESIAN_POINT('Ctrl Pts',(1.11858293216752,1.,1.75699720772089));
#41790=CARTESIAN_POINT('Ctrl Pts',(1.12389096855078,-1.,1.76028671825084));
#41791=CARTESIAN_POINT('Ctrl Pts',(1.12389096855078,1.,1.76028671825084));
#41792=CARTESIAN_POINT('Ctrl Pts',(1.12923123555076,-1.,1.76354571966171));
#41793=CARTESIAN_POINT('Ctrl Pts',(1.12923123555076,1.,1.76354571966171));
#41794=CARTESIAN_POINT('Ctrl Pts',(1.13460291804634,-1.,1.76677384551883));
#41795=CARTESIAN_POINT('Ctrl Pts',(1.13460291804634,1.,1.76677384551883));
#41796=CARTESIAN_POINT('Ctrl Pts',(1.14000548337,-1.,1.76997111386806));
#41797=CARTESIAN_POINT('Ctrl Pts',(1.14000548337,1.,1.76997111386806));
#41798=CARTESIAN_POINT('Ctrl Pts',(1.14543858226948,-1.,1.77313777896234));
#41799=CARTESIAN_POINT('Ctrl Pts',(1.14543858226948,1.,1.77313777896234));
#41800=CARTESIAN_POINT('Ctrl Pts',(1.15090197841531,-1.,1.77627422557034));
#41801=CARTESIAN_POINT('Ctrl Pts',(1.15090197841531,1.,1.77627422557034));
#41802=CARTESIAN_POINT('Ctrl Pts',(1.15639547194689,-1.,1.77938085564261));
#41803=CARTESIAN_POINT('Ctrl Pts',(1.15639547194689,1.,1.77938085564261));
#41804=CARTESIAN_POINT('Ctrl Pts',(1.16191881298458,-1.,1.78245795880949));
#41805=CARTESIAN_POINT('Ctrl Pts',(1.16191881298458,1.,1.78245795880949));
#41806=CARTESIAN_POINT('Ctrl Pts',(1.16747166312239,-1.,1.78550566040349));
#41807=CARTESIAN_POINT('Ctrl Pts',(1.16747166312239,1.,1.78550566040349));
#41808=CARTESIAN_POINT('Ctrl Pts',(1.17305363177265,-1.,1.78852398877523));
#41809=CARTESIAN_POINT('Ctrl Pts',(1.17305363177265,1.,1.78852398877523));
#41810=CARTESIAN_POINT('Ctrl Pts',(1.17866429440781,-1.,1.79151291552646));
#41811=CARTESIAN_POINT('Ctrl Pts',(1.17866429440781,1.,1.79151291552646));
#41812=CARTESIAN_POINT('Ctrl Pts',(1.18430321697471,-1.,1.79447240321572));
#41813=CARTESIAN_POINT('Ctrl Pts',(1.18430321697471,1.,1.79447240321572));
#41814=CARTESIAN_POINT('Ctrl Pts',(1.1899699793456,-1.,1.79740245923649));
#41815=CARTESIAN_POINT('Ctrl Pts',(1.1899699793456,1.,1.79740245923649));
#41816=CARTESIAN_POINT('Ctrl Pts',(1.19566418930405,-1.,1.80030314370121));
#41817=CARTESIAN_POINT('Ctrl Pts',(1.19566418930405,1.,1.80030314370121));
#41818=CARTESIAN_POINT('Ctrl Pts',(1.2013854893912,-1.,1.8031745483882));
#41819=CARTESIAN_POINT('Ctrl Pts',(1.2013854893912,1.,1.8031745483882));
#41820=CARTESIAN_POINT('Ctrl Pts',(1.20713356605519,-1.,1.80601678480772));
#41821=CARTESIAN_POINT('Ctrl Pts',(1.20713356605519,1.,1.80601678480772));
#41822=CARTESIAN_POINT('Ctrl Pts',(1.2129081570818,-1.,1.80882996916931));
#41823=CARTESIAN_POINT('Ctrl Pts',(1.2129081570818,1.,1.80882996916931));
#41824=CARTESIAN_POINT('Ctrl Pts',(1.2187090610323,-1.,1.81161420806172));
#41825=CARTESIAN_POINT('Ctrl Pts',(1.2187090610323,1.,1.81161420806172));
#41826=CARTESIAN_POINT('Ctrl Pts',(1.22453613304507,-1.,1.81436959209778));
#41827=CARTESIAN_POINT('Ctrl Pts',(1.22453613304507,1.,1.81436959209778));
#41828=CARTESIAN_POINT('Ctrl Pts',(1.22921864890975,-1.,1.81655087183054));
#41829=CARTESIAN_POINT('Ctrl Pts',(1.22921864890975,1.,1.81655087183054));
#41830=CARTESIAN_POINT('Ctrl Pts',(1.23274224526804,-1.,1.81817389920914));
#41831=CARTESIAN_POINT('Ctrl Pts',(1.23274224526804,1.,1.81817389920914));
#41832=CARTESIAN_POINT('Ctrl Pts',(1.23509651170384,-1.,1.81925017193531));
#41833=CARTESIAN_POINT('Ctrl Pts',(1.23509651170384,1.,1.81925017193531));
#41834=CARTESIAN_POINT('Ctrl Pts',(1.23627494547115,-1.,1.81978687191668));
#41835=CARTESIAN_POINT('Ctrl Pts',(1.23627494547115,1.,1.81978687191668));
#41836=CARTESIAN_POINT('',(0.892032620296855,1.,1.5055822144029));
#41837=CARTESIAN_POINT('Ctrl Pts',(0.892032620296855,1.,1.5055822144029));
#41838=CARTESIAN_POINT('Ctrl Pts',(0.894452006967538,1.,1.50980486807181));
#41839=CARTESIAN_POINT('Ctrl Pts',(0.89918504749193,1.,1.51805569591479));
#41840=CARTESIAN_POINT('Ctrl Pts',(0.905967409640498,1.,1.52984849890434));
#41841=CARTESIAN_POINT('Ctrl Pts',(0.914375919046579,1.,1.54440491152808));
#41842=CARTESIAN_POINT('Ctrl Pts',(0.923832188966322,1.,1.56065988582509));
#41843=CARTESIAN_POINT('Ctrl Pts',(0.932246680128848,1.,1.57499388385561));
#41844=CARTESIAN_POINT('Ctrl Pts',(0.939646377909319,1.,1.58744937489796));
#41845=CARTESIAN_POINT('Ctrl Pts',(0.946078063325795,1.,1.59810042045408));
#41846=CARTESIAN_POINT('Ctrl Pts',(0.951613284361247,1.,1.60706069897794));
#41847=CARTESIAN_POINT('Ctrl Pts',(0.956354422921572,1.,1.61449324337233));
#41848=CARTESIAN_POINT('Ctrl Pts',(0.960438326099958,1.,1.62061638139929));
#41849=CARTESIAN_POINT('Ctrl Pts',(0.964046107037821,1.,1.6257193066974));
#41850=CARTESIAN_POINT('Ctrl Pts',(0.967387853228041,1.,1.63013849959083));
#41851=CARTESIAN_POINT('Ctrl Pts',(0.970669715996356,1.,1.63420665729609));
#41852=CARTESIAN_POINT('Ctrl Pts',(0.974066058287501,1.,1.63820952658157));
#41853=CARTESIAN_POINT('Ctrl Pts',(0.977689794120296,1.,1.64233990826831));
#41854=CARTESIAN_POINT('Ctrl Pts',(0.981562530940574,1.,1.64665139190834));
#41855=CARTESIAN_POINT('Ctrl Pts',(0.985642622921626,1.,1.6511001661277));
#41856=CARTESIAN_POINT('Ctrl Pts',(0.98985562785445,1.,1.65559044289746));
#41857=CARTESIAN_POINT('Ctrl Pts',(0.994121836661115,1.,1.66001553809916));
#41858=CARTESIAN_POINT('Ctrl Pts',(0.998389654952317,1.,1.66430758030304));
#41859=CARTESIAN_POINT('Ctrl Pts',(1.00265091003682,1.,1.66846059277231));
#41860=CARTESIAN_POINT('Ctrl Pts',(1.00692206696387,1.,1.67250335383248));
#41861=CARTESIAN_POINT('Ctrl Pts',(1.01123236493507,1.,1.67648246776457));
#41862=CARTESIAN_POINT('Ctrl Pts',(1.01561026162786,1.,1.6804428989482));
#41863=CARTESIAN_POINT('Ctrl Pts',(1.02006795074222,1.,1.68440578021739));
#41864=CARTESIAN_POINT('Ctrl Pts',(1.02460180535272,1.,1.68836910178475));
#41865=CARTESIAN_POINT('Ctrl Pts',(1.02919977579155,1.,1.69231840863471));
#41866=CARTESIAN_POINT('Ctrl Pts',(1.03384646003587,1.,1.69623414782769));
#41867=CARTESIAN_POINT('Ctrl Pts',(1.03852922490782,1.,1.70010052930951));
#41868=CARTESIAN_POINT('Ctrl Pts',(1.04324363334546,1.,1.70391338707969));
#41869=CARTESIAN_POINT('Ctrl Pts',(1.0479908540499,1.,1.70767646263641));
#41870=CARTESIAN_POINT('Ctrl Pts',(1.05277517202853,1.,1.71139783543986));
#41871=CARTESIAN_POINT('Ctrl Pts',(1.05760163192481,1.,1.71508654427022));
#41872=CARTESIAN_POINT('Ctrl Pts',(1.06247324680649,1.,1.71874858456908));
#41873=CARTESIAN_POINT('Ctrl Pts',(1.06738966975463,1.,1.72238500928456));
#41874=CARTESIAN_POINT('Ctrl Pts',(1.07234866990252,1.,1.72599406198489));
#41875=CARTESIAN_POINT('Ctrl Pts',(1.0773470373727,1.,1.72957248977424));
#41876=CARTESIAN_POINT('Ctrl Pts',(1.08238162784749,1.,1.73311705663407));
#41877=CARTESIAN_POINT('Ctrl Pts',(1.08745056285429,1.,1.73662628326093));
#41878=CARTESIAN_POINT('Ctrl Pts',(1.09255329056496,1.,1.74010053962252));
#41879=CARTESIAN_POINT('Ctrl Pts',(1.09768999241229,1.,1.74354119236212));
#41880=CARTESIAN_POINT('Ctrl Pts',(1.10286118991144,1.,1.74695004214924));
#41881=CARTESIAN_POINT('Ctrl Pts',(1.10806728183003,1.,1.75032866075914));
#41882=CARTESIAN_POINT('Ctrl Pts',(1.11330807582542,1.,1.75367772094617));
#41883=CARTESIAN_POINT('Ctrl Pts',(1.11858293216752,1.,1.75699720772089));
#41884=CARTESIAN_POINT('Ctrl Pts',(1.12389096855078,1.,1.76028671825084));
#41885=CARTESIAN_POINT('Ctrl Pts',(1.12923123555076,1.,1.76354571966171));
#41886=CARTESIAN_POINT('Ctrl Pts',(1.13460291804634,1.,1.76677384551883));
#41887=CARTESIAN_POINT('Ctrl Pts',(1.14000548337,1.,1.76997111386806));
#41888=CARTESIAN_POINT('Ctrl Pts',(1.14543858226948,1.,1.77313777896234));
#41889=CARTESIAN_POINT('Ctrl Pts',(1.15090197841531,1.,1.77627422557034));
#41890=CARTESIAN_POINT('Ctrl Pts',(1.15639547194689,1.,1.77938085564261));
#41891=CARTESIAN_POINT('Ctrl Pts',(1.16191881298458,1.,1.78245795880949));
#41892=CARTESIAN_POINT('Ctrl Pts',(1.16747166312239,1.,1.78550566040349));
#41893=CARTESIAN_POINT('Ctrl Pts',(1.17305363177265,1.,1.78852398877523));
#41894=CARTESIAN_POINT('Ctrl Pts',(1.17866429440781,1.,1.79151291552646));
#41895=CARTESIAN_POINT('Ctrl Pts',(1.18430321697471,1.,1.79447240321572));
#41896=CARTESIAN_POINT('Ctrl Pts',(1.1899699793456,1.,1.79740245923649));
#41897=CARTESIAN_POINT('Ctrl Pts',(1.19566418930405,1.,1.80030314370121));
#41898=CARTESIAN_POINT('Ctrl Pts',(1.2013854893912,1.,1.8031745483882));
#41899=CARTESIAN_POINT('Ctrl Pts',(1.20713356605519,1.,1.80601678480772));
#41900=CARTESIAN_POINT('Ctrl Pts',(1.2129081570818,1.,1.80882996916931));
#41901=CARTESIAN_POINT('Ctrl Pts',(1.2187090610323,1.,1.81161420806172));
#41902=CARTESIAN_POINT('Ctrl Pts',(1.22453613304507,1.,1.81436959209778));
#41903=CARTESIAN_POINT('Ctrl Pts',(1.22921864890975,1.,1.81655087183054));
#41904=CARTESIAN_POINT('Ctrl Pts',(1.23274224526804,1.,1.81817389920914));
#41905=CARTESIAN_POINT('Ctrl Pts',(1.23509651170384,1.,1.81925017193531));
#41906=CARTESIAN_POINT('Ctrl Pts',(1.23627494547115,1.,1.81978687191668));
#41907=CARTESIAN_POINT('',(0.892032620296854,0.,1.5055822144029));
#41908=CARTESIAN_POINT('Origin',(0.,0.,0.));
#41909=CARTESIAN_POINT('',(0.693717979106305,1.,1.60662857109684));
#41910=CARTESIAN_POINT('Origin',(0.,1.,0.));
#41911=CARTESIAN_POINT('',(0.693717979106305,0.,1.60662857109684));
#41912=CARTESIAN_POINT('Ctrl Pts',(0.7455743247944,-1.,2.0698113262342));
#41913=CARTESIAN_POINT('Ctrl Pts',(0.7455743247944,1.,2.0698113262342));
#41914=CARTESIAN_POINT('Ctrl Pts',(0.745832791378367,-1.,2.06854248895728));
#41915=CARTESIAN_POINT('Ctrl Pts',(0.745832791378367,1.,2.06854248895728));
#41916=CARTESIAN_POINT('Ctrl Pts',(0.7463458715442,-1.,2.06600523016815));
#41917=CARTESIAN_POINT('Ctrl Pts',(0.7463458715442,1.,2.06600523016815));
#41918=CARTESIAN_POINT('Ctrl Pts',(0.747103932787919,-1.,2.06220058927826));
#41919=CARTESIAN_POINT('Ctrl Pts',(0.747103932787919,1.,2.06220058927826));
#41920=CARTESIAN_POINT('Ctrl Pts',(0.748091554183802,-1.,2.05713023031007));
#41921=CARTESIAN_POINT('Ctrl Pts',(0.748091554183802,1.,2.05713023031007));
#41922=CARTESIAN_POINT('Ctrl Pts',(0.749287468665046,-1.,2.05079645592154));
#41923=CARTESIAN_POINT('Ctrl Pts',(0.749287468665046,1.,2.05079645592154));
#41924=CARTESIAN_POINT('Ctrl Pts',(0.750444657875575,-1.,2.04446689147979));
#41925=CARTESIAN_POINT('Ctrl Pts',(0.750444657875575,1.,2.04446689147979));
#41926=CARTESIAN_POINT('Ctrl Pts',(0.751562963361115,-1.,2.03814160092099));
#41927=CARTESIAN_POINT('Ctrl Pts',(0.751562963361115,1.,2.03814160092099));
#41928=CARTESIAN_POINT('Ctrl Pts',(0.75264218048721,-1.,2.03182068456221));
#41929=CARTESIAN_POINT('Ctrl Pts',(0.75264218048721,1.,2.03182068456221));
#41930=CARTESIAN_POINT('Ctrl Pts',(0.753682061112768,-1.,2.02550428623313));
#41931=CARTESIAN_POINT('Ctrl Pts',(0.753682061112768,1.,2.02550428623313));
#41932=CARTESIAN_POINT('Ctrl Pts',(0.754682330722816,-1.,2.01919259405809));
#41933=CARTESIAN_POINT('Ctrl Pts',(0.754682330722816,1.,2.01919259405809));
#41934=CARTESIAN_POINT('Ctrl Pts',(0.755642704957865,-1.,2.01288584328084));
#41935=CARTESIAN_POINT('Ctrl Pts',(0.755642704957865,1.,2.01288584328084));
#41936=CARTESIAN_POINT('Ctrl Pts',(0.75656290464667,-1.,2.0065843158773));
#41937=CARTESIAN_POINT('Ctrl Pts',(0.75656290464667,1.,2.0065843158773));
#41938=CARTESIAN_POINT('Ctrl Pts',(0.757442676862724,-1.,2.00028834739178));
#41939=CARTESIAN_POINT('Ctrl Pts',(0.757442676862724,1.,2.00028834739178));
#41940=CARTESIAN_POINT('Ctrl Pts',(0.758281796766761,-1.,1.99399831098817));
#41941=CARTESIAN_POINT('Ctrl Pts',(0.758281796766761,1.,1.99399831098817));
#41942=CARTESIAN_POINT('Ctrl Pts',(0.759080037802488,-1.,1.98771456680874));
#41943=CARTESIAN_POINT('Ctrl Pts',(0.759080037802488,1.,1.98771456680874));
#41944=CARTESIAN_POINT('Ctrl Pts',(0.75983714745219,-1.,1.98143741418172));
#41945=CARTESIAN_POINT('Ctrl Pts',(0.75983714745219,1.,1.98143741418172));
#41946=CARTESIAN_POINT('Ctrl Pts',(0.760552825409757,-1.,1.97516705321494));
#41947=CARTESIAN_POINT('Ctrl Pts',(0.760552825409757,1.,1.97516705321494));
#41948=CARTESIAN_POINT('Ctrl Pts',(0.76122669048382,-1.,1.96890351582499));
#41949=CARTESIAN_POINT('Ctrl Pts',(0.76122669048382,1.,1.96890351582499));
#41950=CARTESIAN_POINT('Ctrl Pts',(0.761858300014423,-1.,1.96264672744186));
#41951=CARTESIAN_POINT('Ctrl Pts',(0.761858300014423,1.,1.96264672744186));
#41952=CARTESIAN_POINT('Ctrl Pts',(0.762447203806178,-1.,1.95639665309869));
#41953=CARTESIAN_POINT('Ctrl Pts',(0.762447203806178,1.,1.95639665309869));
#41954=CARTESIAN_POINT('Ctrl Pts',(0.762992990878769,-1.,1.95015342590024));
#41955=CARTESIAN_POINT('Ctrl Pts',(0.762992990878769,1.,1.95015342590024));
#41956=CARTESIAN_POINT('Ctrl Pts',(0.763495333538629,-1.,1.9439174661764));
#41957=CARTESIAN_POINT('Ctrl Pts',(0.763495333538629,1.,1.9439174661764));
#41958=CARTESIAN_POINT('Ctrl Pts',(0.763954049121458,-1.,1.93768964875886));
#41959=CARTESIAN_POINT('Ctrl Pts',(0.763954049121458,1.,1.93768964875886));
#41960=CARTESIAN_POINT('Ctrl Pts',(0.76436901067394,-1.,1.93147105496382));
#41961=CARTESIAN_POINT('Ctrl Pts',(0.76436901067394,1.,1.93147105496382));
#41962=CARTESIAN_POINT('Ctrl Pts',(0.764740025488211,-1.,1.92526263537048));
#41963=CARTESIAN_POINT('Ctrl Pts',(0.764740025488211,1.,1.92526263537048));
#41964=CARTESIAN_POINT('Ctrl Pts',(0.765066729667088,-1.,1.91906491634196));
#41965=CARTESIAN_POINT('Ctrl Pts',(0.765066729667088,1.,1.91906491634196));
#41966=CARTESIAN_POINT('Ctrl Pts',(0.765348465884722,-1.,1.91287765805169));
#41967=CARTESIAN_POINT('Ctrl Pts',(0.765348465884722,1.,1.91287765805169));
#41968=CARTESIAN_POINT('Ctrl Pts',(0.765584196937919,-1.,1.90669961402356));
#41969=CARTESIAN_POINT('Ctrl Pts',(0.765584196937919,1.,1.90669961402356));
#41970=CARTESIAN_POINT('Ctrl Pts',(0.765772772593386,-1.,1.90052930393596));
#41971=CARTESIAN_POINT('Ctrl Pts',(0.765772772593386,1.,1.90052930393596));
#41972=CARTESIAN_POINT('Ctrl Pts',(0.765913193856978,-1.,1.89436577771388));
#41973=CARTESIAN_POINT('Ctrl Pts',(0.765913193856978,1.,1.89436577771388));
#41974=CARTESIAN_POINT('Ctrl Pts',(0.766004837062091,-1.,1.88820926433409));
#41975=CARTESIAN_POINT('Ctrl Pts',(0.766004837062091,1.,1.88820926433409));
#41976=CARTESIAN_POINT('Ctrl Pts',(0.766047794851864,-1.,1.88206215302561));
#41977=CARTESIAN_POINT('Ctrl Pts',(0.766047794851864,1.,1.88206215302561));
#41978=CARTESIAN_POINT('Ctrl Pts',(0.766042837036744,-1.,1.87592888967883));
#41979=CARTESIAN_POINT('Ctrl Pts',(0.766042837036744,1.,1.87592888967883));
#41980=CARTESIAN_POINT('Ctrl Pts',(0.765990708546091,-1.,1.86981398314341));
#41981=CARTESIAN_POINT('Ctrl Pts',(0.765990708546091,1.,1.86981398314341));
#41982=CARTESIAN_POINT('Ctrl Pts',(0.765891519092547,-1.,1.86372027063312));
#41983=CARTESIAN_POINT('Ctrl Pts',(0.765891519092547,1.,1.86372027063312));
#41984=CARTESIAN_POINT('Ctrl Pts',(0.765744212909318,-1.,1.85764741390394));
#41985=CARTESIAN_POINT('Ctrl Pts',(0.765744212909318,1.,1.85764741390394));
#41986=CARTESIAN_POINT('Ctrl Pts',(0.765545710619062,-1.,1.85158945130063));
#41987=CARTESIAN_POINT('Ctrl Pts',(0.765545710619062,1.,1.85158945130063));
#41988=CARTESIAN_POINT('Ctrl Pts',(0.765291664862029,-1.,1.84553698875924));
#41989=CARTESIAN_POINT('Ctrl Pts',(0.765291664862029,1.,1.84553698875924));
#41990=CARTESIAN_POINT('Ctrl Pts',(0.764978057881737,-1.,1.83948181064835));
#41991=CARTESIAN_POINT('Ctrl Pts',(0.764978057881737,1.,1.83948181064835));
#41992=CARTESIAN_POINT('Ctrl Pts',(0.764602549687853,-1.,1.83342077227142));
#41993=CARTESIAN_POINT('Ctrl Pts',(0.764602549687853,1.,1.83342077227142));
#41994=CARTESIAN_POINT('Ctrl Pts',(0.764165902605995,-1.,1.82735991200065));
#41995=CARTESIAN_POINT('Ctrl Pts',(0.764165902605995,1.,1.82735991200065));
#41996=CARTESIAN_POINT('Ctrl Pts',(0.763673465462726,-1.,1.82131873145266));
#41997=CARTESIAN_POINT('Ctrl Pts',(0.763673465462726,1.,1.82131873145266));
#41998=CARTESIAN_POINT('Ctrl Pts',(0.763132003836634,-1.,1.8153211840553));
#41999=CARTESIAN_POINT('Ctrl Pts',(0.763132003836634,1.,1.8153211840553));
#42000=CARTESIAN_POINT('Ctrl Pts',(0.762546129463938,-1.,1.80938551463965));
#42001=CARTESIAN_POINT('Ctrl Pts',(0.762546129463938,1.,1.80938551463965));
#42002=CARTESIAN_POINT('Ctrl Pts',(0.761915336443547,-1.,1.80351583877342));
#42003=CARTESIAN_POINT('Ctrl Pts',(0.761915336443547,1.,1.80351583877342));
#42004=CARTESIAN_POINT('Ctrl Pts',(0.761229695230558,-1.,1.79768986997783));
#42005=CARTESIAN_POINT('Ctrl Pts',(0.761229695230558,1.,1.79768986997783));
#42006=CARTESIAN_POINT('Ctrl Pts',(0.760469555880749,-1.,1.7918581561088));
#42007=CARTESIAN_POINT('Ctrl Pts',(0.760469555880749,1.,1.7918581561088));
#42008=CARTESIAN_POINT('Ctrl Pts',(0.759614401110189,-1.,1.78596964884604));
#42009=CARTESIAN_POINT('Ctrl Pts',(0.759614401110189,1.,1.78596964884604));
#42010=CARTESIAN_POINT('Ctrl Pts',(0.758650626677518,-1.,1.77999411220945));
#42011=CARTESIAN_POINT('Ctrl Pts',(0.758650626677518,1.,1.77999411220945));
#42012=CARTESIAN_POINT('Ctrl Pts',(0.757578264077028,-1.,1.77394167108292));
#42013=CARTESIAN_POINT('Ctrl Pts',(0.757578264077028,1.,1.77394167108292));
#42014=CARTESIAN_POINT('Ctrl Pts',(0.75642189602781,-1.,1.76789396002998));
#42015=CARTESIAN_POINT('Ctrl Pts',(0.75642189602781,1.,1.76789396002998));
#42016=CARTESIAN_POINT('Ctrl Pts',(0.755220979974461,-1.,1.76197817240128));
#42017=CARTESIAN_POINT('Ctrl Pts',(0.755220979974461,1.,1.76197817240128));
#42018=CARTESIAN_POINT('Ctrl Pts',(0.754009254027828,-1.,1.75631083600019));
#42019=CARTESIAN_POINT('Ctrl Pts',(0.754009254027828,1.,1.75631083600019));
#42020=CARTESIAN_POINT('Ctrl Pts',(0.752797683531314,-1.,1.75095139468794));
#42021=CARTESIAN_POINT('Ctrl Pts',(0.752797683531314,1.,1.75095139468794));
#42022=CARTESIAN_POINT('Ctrl Pts',(0.751555614164482,-1.,1.74585086852502));
#42023=CARTESIAN_POINT('Ctrl Pts',(0.751555614164482,1.,1.74585086852502));
#42024=CARTESIAN_POINT('Ctrl Pts',(0.750193435981249,-1.,1.74080458267114));
#42025=CARTESIAN_POINT('Ctrl Pts',(0.750193435981249,1.,1.74080458267114));
#42026=CARTESIAN_POINT('Ctrl Pts',(0.74858246295687,-1.,1.7355035168033));
#42027=CARTESIAN_POINT('Ctrl Pts',(0.74858246295687,1.,1.7355035168033));
#42028=CARTESIAN_POINT('Ctrl Pts',(0.746574710097752,-1.,1.72958533647714));
#42029=CARTESIAN_POINT('Ctrl Pts',(0.746574710097752,1.,1.72958533647714));
#42030=CARTESIAN_POINT('Ctrl Pts',(0.744021445433093,-1.,1.72268229916769));
#42031=CARTESIAN_POINT('Ctrl Pts',(0.744021445433093,1.,1.72268229916769));
#42032=CARTESIAN_POINT('Ctrl Pts',(0.74079516202821,-1.,1.71447789751001));
#42033=CARTESIAN_POINT('Ctrl Pts',(0.74079516202821,1.,1.71447789751001));
#42034=CARTESIAN_POINT('Ctrl Pts',(0.736799665716932,-1.,1.70473309004249));
#42035=CARTESIAN_POINT('Ctrl Pts',(0.736799665716932,1.,1.70473309004249));
#42036=CARTESIAN_POINT('Ctrl Pts',(0.731963238685357,-1.,1.69326921972915));
#42037=CARTESIAN_POINT('Ctrl Pts',(0.731963238685357,1.,1.69326921972915));
#42038=CARTESIAN_POINT('Ctrl Pts',(0.726235967982445,-1.,1.67996158451922));
#42039=CARTESIAN_POINT('Ctrl Pts',(0.726235967982445,1.,1.67996158451922));
#42040=CARTESIAN_POINT('Ctrl Pts',(0.719585433787949,-1.,1.66472880551777));
#42041=CARTESIAN_POINT('Ctrl Pts',(0.719585433787949,1.,1.66472880551777));
#42042=CARTESIAN_POINT('Ctrl Pts',(0.711993139340447,-1.,1.64752408828442));
#42043=CARTESIAN_POINT('Ctrl Pts',(0.711993139340447,1.,1.64752408828442));
#42044=CARTESIAN_POINT('Ctrl Pts',(0.705159151977294,-1.,1.6321654166204));
#42045=CARTESIAN_POINT('Ctrl Pts',(0.705159151977294,1.,1.6321654166204));
#42046=CARTESIAN_POINT('Ctrl Pts',(0.699605146398836,-1.,1.61974673471117));
#42047=CARTESIAN_POINT('Ctrl Pts',(0.699605146398836,1.,1.61974673471117));
#42048=CARTESIAN_POINT('Ctrl Pts',(0.69571209787897,-1.,1.61106790957619));
#42049=CARTESIAN_POINT('Ctrl Pts',(0.69571209787897,1.,1.61106790957619));
#42050=CARTESIAN_POINT('Ctrl Pts',(0.693717979106305,-1.,1.60662857109684));
#42051=CARTESIAN_POINT('Ctrl Pts',(0.693717979106305,1.,1.60662857109684));
#42052=CARTESIAN_POINT('',(0.7455743247944,1.,2.0698113262342));
#42053=CARTESIAN_POINT('Ctrl Pts',(0.7455743247944,1.,2.0698113262342));
#42054=CARTESIAN_POINT('Ctrl Pts',(0.745832791378367,1.,2.06854248895728));
#42055=CARTESIAN_POINT('Ctrl Pts',(0.7463458715442,1.,2.06600523016815));
#42056=CARTESIAN_POINT('Ctrl Pts',(0.747103932787919,1.,2.06220058927826));
#42057=CARTESIAN_POINT('Ctrl Pts',(0.748091554183802,1.,2.05713023031007));
#42058=CARTESIAN_POINT('Ctrl Pts',(0.749287468665046,1.,2.05079645592154));
#42059=CARTESIAN_POINT('Ctrl Pts',(0.750444657875575,1.,2.04446689147979));
#42060=CARTESIAN_POINT('Ctrl Pts',(0.751562963361115,1.,2.03814160092099));
#42061=CARTESIAN_POINT('Ctrl Pts',(0.75264218048721,1.,2.03182068456221));
#42062=CARTESIAN_POINT('Ctrl Pts',(0.753682061112768,1.,2.02550428623313));
#42063=CARTESIAN_POINT('Ctrl Pts',(0.754682330722816,1.,2.01919259405809));
#42064=CARTESIAN_POINT('Ctrl Pts',(0.755642704957865,1.,2.01288584328084));
#42065=CARTESIAN_POINT('Ctrl Pts',(0.75656290464667,1.,2.0065843158773));
#42066=CARTESIAN_POINT('Ctrl Pts',(0.757442676862724,1.,2.00028834739178));
#42067=CARTESIAN_POINT('Ctrl Pts',(0.758281796766761,1.,1.99399831098817));
#42068=CARTESIAN_POINT('Ctrl Pts',(0.759080037802488,1.,1.98771456680874));
#42069=CARTESIAN_POINT('Ctrl Pts',(0.75983714745219,1.,1.98143741418172));
#42070=CARTESIAN_POINT('Ctrl Pts',(0.760552825409757,1.,1.97516705321494));
#42071=CARTESIAN_POINT('Ctrl Pts',(0.76122669048382,1.,1.96890351582499));
#42072=CARTESIAN_POINT('Ctrl Pts',(0.761858300014423,1.,1.96264672744186));
#42073=CARTESIAN_POINT('Ctrl Pts',(0.762447203806178,1.,1.95639665309869));
#42074=CARTESIAN_POINT('Ctrl Pts',(0.762992990878769,1.,1.95015342590024));
#42075=CARTESIAN_POINT('Ctrl Pts',(0.763495333538629,1.,1.9439174661764));
#42076=CARTESIAN_POINT('Ctrl Pts',(0.763954049121458,1.,1.93768964875886));
#42077=CARTESIAN_POINT('Ctrl Pts',(0.76436901067394,1.,1.93147105496382));
#42078=CARTESIAN_POINT('Ctrl Pts',(0.764740025488211,1.,1.92526263537048));
#42079=CARTESIAN_POINT('Ctrl Pts',(0.765066729667088,1.,1.91906491634196));
#42080=CARTESIAN_POINT('Ctrl Pts',(0.765348465884722,1.,1.91287765805169));
#42081=CARTESIAN_POINT('Ctrl Pts',(0.765584196937919,1.,1.90669961402356));
#42082=CARTESIAN_POINT('Ctrl Pts',(0.765772772593386,1.,1.90052930393596));
#42083=CARTESIAN_POINT('Ctrl Pts',(0.765913193856978,1.,1.89436577771388));
#42084=CARTESIAN_POINT('Ctrl Pts',(0.766004837062091,1.,1.88820926433409));
#42085=CARTESIAN_POINT('Ctrl Pts',(0.766047794851864,1.,1.88206215302561));
#42086=CARTESIAN_POINT('Ctrl Pts',(0.766042837036744,1.,1.87592888967883));
#42087=CARTESIAN_POINT('Ctrl Pts',(0.765990708546091,1.,1.86981398314341));
#42088=CARTESIAN_POINT('Ctrl Pts',(0.765891519092547,1.,1.86372027063312));
#42089=CARTESIAN_POINT('Ctrl Pts',(0.765744212909318,1.,1.85764741390394));
#42090=CARTESIAN_POINT('Ctrl Pts',(0.765545710619062,1.,1.85158945130063));
#42091=CARTESIAN_POINT('Ctrl Pts',(0.765291664862029,1.,1.84553698875924));
#42092=CARTESIAN_POINT('Ctrl Pts',(0.764978057881737,1.,1.83948181064835));
#42093=CARTESIAN_POINT('Ctrl Pts',(0.764602549687853,1.,1.83342077227142));
#42094=CARTESIAN_POINT('Ctrl Pts',(0.764165902605995,1.,1.82735991200065));
#42095=CARTESIAN_POINT('Ctrl Pts',(0.763673465462726,1.,1.82131873145266));
#42096=CARTESIAN_POINT('Ctrl Pts',(0.763132003836634,1.,1.8153211840553));
#42097=CARTESIAN_POINT('Ctrl Pts',(0.762546129463938,1.,1.80938551463965));
#42098=CARTESIAN_POINT('Ctrl Pts',(0.761915336443547,1.,1.80351583877342));
#42099=CARTESIAN_POINT('Ctrl Pts',(0.761229695230558,1.,1.79768986997783));
#42100=CARTESIAN_POINT('Ctrl Pts',(0.760469555880749,1.,1.7918581561088));
#42101=CARTESIAN_POINT('Ctrl Pts',(0.759614401110189,1.,1.78596964884604));
#42102=CARTESIAN_POINT('Ctrl Pts',(0.758650626677518,1.,1.77999411220945));
#42103=CARTESIAN_POINT('Ctrl Pts',(0.757578264077028,1.,1.77394167108292));
#42104=CARTESIAN_POINT('Ctrl Pts',(0.75642189602781,1.,1.76789396002998));
#42105=CARTESIAN_POINT('Ctrl Pts',(0.755220979974461,1.,1.76197817240128));
#42106=CARTESIAN_POINT('Ctrl Pts',(0.754009254027828,1.,1.75631083600019));
#42107=CARTESIAN_POINT('Ctrl Pts',(0.752797683531314,1.,1.75095139468794));
#42108=CARTESIAN_POINT('Ctrl Pts',(0.751555614164482,1.,1.74585086852502));
#42109=CARTESIAN_POINT('Ctrl Pts',(0.750193435981249,1.,1.74080458267114));
#42110=CARTESIAN_POINT('Ctrl Pts',(0.74858246295687,1.,1.7355035168033));
#42111=CARTESIAN_POINT('Ctrl Pts',(0.746574710097752,1.,1.72958533647714));
#42112=CARTESIAN_POINT('Ctrl Pts',(0.744021445433093,1.,1.72268229916769));
#42113=CARTESIAN_POINT('Ctrl Pts',(0.74079516202821,1.,1.71447789751001));
#42114=CARTESIAN_POINT('Ctrl Pts',(0.736799665716932,1.,1.70473309004249));
#42115=CARTESIAN_POINT('Ctrl Pts',(0.731963238685357,1.,1.69326921972915));
#42116=CARTESIAN_POINT('Ctrl Pts',(0.726235967982445,1.,1.67996158451922));
#42117=CARTESIAN_POINT('Ctrl Pts',(0.719585433787949,1.,1.66472880551777));
#42118=CARTESIAN_POINT('Ctrl Pts',(0.711993139340447,1.,1.64752408828442));
#42119=CARTESIAN_POINT('Ctrl Pts',(0.705159151977294,1.,1.6321654166204));
#42120=CARTESIAN_POINT('Ctrl Pts',(0.699605146398836,1.,1.61974673471117));
#42121=CARTESIAN_POINT('Ctrl Pts',(0.69571209787897,1.,1.61106790957619));
#42122=CARTESIAN_POINT('Ctrl Pts',(0.693717979106305,1.,1.60662857109684));
#42123=CARTESIAN_POINT('',(0.7455743247944,0.,2.0698113262342));
#42124=CARTESIAN_POINT('Origin',(0.61342227326009,0.,2.11275013067528));
#42125=CARTESIAN_POINT('',(0.61342227326009,1.,2.11275013067528));
#42126=CARTESIAN_POINT('',(0.7455743247944,1.,2.0698113262342));
#42127=CARTESIAN_POINT('',(0.61342227326009,0.,2.11275013067528));
#42128=CARTESIAN_POINT('Ctrl Pts',(0.383122945602004,-1.,1.7075470150345));
#42129=CARTESIAN_POINT('Ctrl Pts',(0.383122945602004,1.,1.7075470150345));
#42130=CARTESIAN_POINT('Ctrl Pts',(0.384119047315541,-1.,1.71231062891958));
#42131=CARTESIAN_POINT('Ctrl Pts',(0.384119047315541,1.,1.71231062891958));
#42132=CARTESIAN_POINT('Ctrl Pts',(0.38607079032701,-1.,1.72162022246158));
#42133=CARTESIAN_POINT('Ctrl Pts',(0.38607079032701,1.,1.72162022246158));
#42134=CARTESIAN_POINT('Ctrl Pts',(0.388877023509191,-1.,1.7349317097561));
#42135=CARTESIAN_POINT('Ctrl Pts',(0.388877023509191,1.,1.7349317097561));
#42136=CARTESIAN_POINT('Ctrl Pts',(0.392375812294307,-1.,1.75137405313962));
#42137=CARTESIAN_POINT('Ctrl Pts',(0.392375812294307,1.,1.75137405313962));
#42138=CARTESIAN_POINT('Ctrl Pts',(0.39634619612042,-1.,1.7697556004756));
#42139=CARTESIAN_POINT('Ctrl Pts',(0.39634619612042,1.,1.7697556004756));
#42140=CARTESIAN_POINT('Ctrl Pts',(0.39991940378308,-1.,1.78598826347533));
#42141=CARTESIAN_POINT('Ctrl Pts',(0.39991940378308,1.,1.78598826347533));
#42142=CARTESIAN_POINT('Ctrl Pts',(0.403107976170441,-1.,1.80012077176221));
#42143=CARTESIAN_POINT('Ctrl Pts',(0.403107976170441,1.,1.80012077176221));
#42144=CARTESIAN_POINT('Ctrl Pts',(0.405933518411838,-1.,1.81223801813988));
#42145=CARTESIAN_POINT('Ctrl Pts',(0.405933518411838,1.,1.81223801813988));
#42146=CARTESIAN_POINT('Ctrl Pts',(0.408428948108533,-1.,1.8224702267854));
#42147=CARTESIAN_POINT('Ctrl Pts',(0.408428948108533,1.,1.8224702267854));
#42148=CARTESIAN_POINT('Ctrl Pts',(0.410641256301674,-1.,1.83100408895216));
#42149=CARTESIAN_POINT('Ctrl Pts',(0.410641256301674,1.,1.83100408895216));
#42150=CARTESIAN_POINT('Ctrl Pts',(0.412633125322161,-1.,1.83808953475839));
#42151=CARTESIAN_POINT('Ctrl Pts',(0.412633125322161,1.,1.83808953475839));
#42152=CARTESIAN_POINT('Ctrl Pts',(0.41448743825434,-1.,1.8440575707371));
#42153=CARTESIAN_POINT('Ctrl Pts',(0.41448743825434,1.,1.8440575707371));
#42154=CARTESIAN_POINT('Ctrl Pts',(0.416300022038864,-1.,1.84929312929882));
#42155=CARTESIAN_POINT('Ctrl Pts',(0.416300022038864,1.,1.84929312929882));
#42156=CARTESIAN_POINT('Ctrl Pts',(0.418164129143534,-1.,1.85417632856234));
#42157=CARTESIAN_POINT('Ctrl Pts',(0.418164129143534,1.,1.85417632856234));
#42158=CARTESIAN_POINT('Ctrl Pts',(0.420157287975619,-1.,1.85903281096686));
#42159=CARTESIAN_POINT('Ctrl Pts',(0.420157287975619,1.,1.85903281096686));
#42160=CARTESIAN_POINT('Ctrl Pts',(0.422327307418275,-1.,1.86408083334028));
#42161=CARTESIAN_POINT('Ctrl Pts',(0.422327307418275,1.,1.86408083334028));
#42162=CARTESIAN_POINT('Ctrl Pts',(0.424678177291358,-1.,1.86937803944323));
#42163=CARTESIAN_POINT('Ctrl Pts',(0.424678177291358,1.,1.86937803944323));
#42164=CARTESIAN_POINT('Ctrl Pts',(0.427183828519102,-1.,1.87486989291484));
#42165=CARTESIAN_POINT('Ctrl Pts',(0.427183828519102,1.,1.87486989291484));
#42166=CARTESIAN_POINT('Ctrl Pts',(0.429803062482344,-1.,1.88044229001832));
#42167=CARTESIAN_POINT('Ctrl Pts',(0.429803062482344,1.,1.88044229001832));
#42168=CARTESIAN_POINT('Ctrl Pts',(0.432493038548748,-1.,1.88596913666793));
#42169=CARTESIAN_POINT('Ctrl Pts',(0.432493038548748,1.,1.88596913666793));
#42170=CARTESIAN_POINT('Ctrl Pts',(0.435225660963383,-1.,1.89136993975504));
#42171=CARTESIAN_POINT('Ctrl Pts',(0.435225660963383,1.,1.89136993975504));
#42172=CARTESIAN_POINT('Ctrl Pts',(0.437995003948244,-1.,1.89663648956466));
#42173=CARTESIAN_POINT('Ctrl Pts',(0.437995003948244,1.,1.89663648956466));
#42174=CARTESIAN_POINT('Ctrl Pts',(0.440807833704038,-1.,1.90180124389086));
#42175=CARTESIAN_POINT('Ctrl Pts',(0.440807833704038,1.,1.90180124389086));
#42176=CARTESIAN_POINT('Ctrl Pts',(0.44367755684915,-1.,1.90691756144898));
#42177=CARTESIAN_POINT('Ctrl Pts',(0.44367755684915,1.,1.90691756144898));
#42178=CARTESIAN_POINT('Ctrl Pts',(0.446617343485711,-1.,1.9120369998112));
#42179=CARTESIAN_POINT('Ctrl Pts',(0.446617343485711,1.,1.9120369998112));
#42180=CARTESIAN_POINT('Ctrl Pts',(0.449632260106662,-1.,1.91718342555755));
#42181=CARTESIAN_POINT('Ctrl Pts',(0.449632260106662,1.,1.91718342555755));
#42182=CARTESIAN_POINT('Ctrl Pts',(0.452719478359432,-1.,1.92235380648502));
#42183=CARTESIAN_POINT('Ctrl Pts',(0.452719478359432,1.,1.92235380648502));
#42184=CARTESIAN_POINT('Ctrl Pts',(0.45587200517437,-1.,1.92753067150476));
#42185=CARTESIAN_POINT('Ctrl Pts',(0.45587200517437,1.,1.92753067150476));
#42186=CARTESIAN_POINT('Ctrl Pts',(0.459081234547926,-1.,1.93269066517934));
#42187=CARTESIAN_POINT('Ctrl Pts',(0.459081234547926,1.,1.93269066517934));
#42188=CARTESIAN_POINT('Ctrl Pts',(0.462340031009056,-1.,1.93781486640821));
#42189=CARTESIAN_POINT('Ctrl Pts',(0.462340031009056,1.,1.93781486640821));
#42190=CARTESIAN_POINT('Ctrl Pts',(0.46564546202603,-1.,1.9428979419619));
#42191=CARTESIAN_POINT('Ctrl Pts',(0.46564546202603,1.,1.9428979419619));
#42192=CARTESIAN_POINT('Ctrl Pts',(0.468997482913135,-1.,1.94794381136514));
#42193=CARTESIAN_POINT('Ctrl Pts',(0.468997482913135,1.,1.94794381136514));
#42194=CARTESIAN_POINT('Ctrl Pts',(0.472397672264072,-1.,1.95296148278133));
#42195=CARTESIAN_POINT('Ctrl Pts',(0.472397672264072,1.,1.95296148278133));
#42196=CARTESIAN_POINT('Ctrl Pts',(0.475848034683176,-1.,1.95796111148177));
#42197=CARTESIAN_POINT('Ctrl Pts',(0.475848034683176,1.,1.95796111148177));
#42198=CARTESIAN_POINT('Ctrl Pts',(0.479349583074855,-1.,1.96294933055943));
#42199=CARTESIAN_POINT('Ctrl Pts',(0.479349583074855,1.,1.96294933055943));
#42200=CARTESIAN_POINT('Ctrl Pts',(0.48290166212069,-1.,1.96792703422362));
#42201=CARTESIAN_POINT('Ctrl Pts',(0.48290166212069,1.,1.96792703422362));
#42202=CARTESIAN_POINT('Ctrl Pts',(0.486502692907658,-1.,1.97289186263272));
#42203=CARTESIAN_POINT('Ctrl Pts',(0.486502692907658,1.,1.97289186263272));
#42204=CARTESIAN_POINT('Ctrl Pts',(0.490150627860952,-1.,1.97783973019229));
#42205=CARTESIAN_POINT('Ctrl Pts',(0.490150627860952,1.,1.97783973019229));
#42206=CARTESIAN_POINT('Ctrl Pts',(0.493843476541494,-1.,1.98276658761821));
#42207=CARTESIAN_POINT('Ctrl Pts',(0.493843476541494,1.,1.98276658761821));
#42208=CARTESIAN_POINT('Ctrl Pts',(0.497579909545574,-1.,1.98767044752932));
#42209=CARTESIAN_POINT('Ctrl Pts',(0.497579909545574,1.,1.98767044752932));
#42210=CARTESIAN_POINT('Ctrl Pts',(0.501359287727146,-1.,1.99255149126155));
#42211=CARTESIAN_POINT('Ctrl Pts',(0.501359287727146,1.,1.99255149126155));
#42212=CARTESIAN_POINT('Ctrl Pts',(0.505181361323026,-1.,1.99741107463572));
#42213=CARTESIAN_POINT('Ctrl Pts',(0.505181361323026,1.,1.99741107463572));
#42214=CARTESIAN_POINT('Ctrl Pts',(0.509046069886157,-1.,2.00225107134734));
#42215=CARTESIAN_POINT('Ctrl Pts',(0.509046069886157,1.,2.00225107134734));
#42216=CARTESIAN_POINT('Ctrl Pts',(0.512953306961792,-1.,2.00707309946949));
#42217=CARTESIAN_POINT('Ctrl Pts',(0.512953306961792,1.,2.00707309946949));
#42218=CARTESIAN_POINT('Ctrl Pts',(0.516902681728687,-1.,2.01187773939242));
#42219=CARTESIAN_POINT('Ctrl Pts',(0.516902681728687,1.,2.01187773939242));
#42220=CARTESIAN_POINT('Ctrl Pts',(0.52089359039937,-1.,2.01666477917286));
#42221=CARTESIAN_POINT('Ctrl Pts',(0.52089359039937,1.,2.01666477917286));
#42222=CARTESIAN_POINT('Ctrl Pts',(0.524925318333476,-1.,2.02143356304698));
#42223=CARTESIAN_POINT('Ctrl Pts',(0.524925318333476,1.,2.02143356304698));
#42224=CARTESIAN_POINT('Ctrl Pts',(0.528997127241914,-1.,2.0261832908329));
#42225=CARTESIAN_POINT('Ctrl Pts',(0.528997127241914,1.,2.0261832908329));
#42226=CARTESIAN_POINT('Ctrl Pts',(0.533108355132976,-1.,2.03091336214426));
#42227=CARTESIAN_POINT('Ctrl Pts',(0.533108355132976,1.,2.03091336214426));
#42228=CARTESIAN_POINT('Ctrl Pts',(0.537258489833262,-1.,2.03562362954037));
#42229=CARTESIAN_POINT('Ctrl Pts',(0.537258489833262,1.,2.03562362954037));
#42230=CARTESIAN_POINT('Ctrl Pts',(0.541447120615659,-1.,2.04031422690527));
#42231=CARTESIAN_POINT('Ctrl Pts',(0.541447120615659,1.,2.04031422690527));
#42232=CARTESIAN_POINT('Ctrl Pts',(0.54567390381743,-1.,2.04498544714588));
#42233=CARTESIAN_POINT('Ctrl Pts',(0.54567390381743,1.,2.04498544714588));
#42234=CARTESIAN_POINT('Ctrl Pts',(0.549938525150295,-1.,2.04963761077958));
#42235=CARTESIAN_POINT('Ctrl Pts',(0.549938525150295,1.,2.04963761077958));
#42236=CARTESIAN_POINT('Ctrl Pts',(0.554240657463906,-1.,2.05427091604413));
#42237=CARTESIAN_POINT('Ctrl Pts',(0.554240657463906,1.,2.05427091604413));
#42238=CARTESIAN_POINT('Ctrl Pts',(0.558579940185151,-1.,2.05888537756462));
#42239=CARTESIAN_POINT('Ctrl Pts',(0.558579940185151,1.,2.05888537756462));
#42240=CARTESIAN_POINT('Ctrl Pts',(0.562955993082261,-1.,2.06348090160589));
#42241=CARTESIAN_POINT('Ctrl Pts',(0.562955993082261,1.,2.06348090160589));
#42242=CARTESIAN_POINT('Ctrl Pts',(0.567368421181087,-1.,2.06805732997334));
#42243=CARTESIAN_POINT('Ctrl Pts',(0.567368421181087,1.,2.06805732997334));
#42244=CARTESIAN_POINT('Ctrl Pts',(0.571816823242602,-1.,2.07261449292824));
#42245=CARTESIAN_POINT('Ctrl Pts',(0.571816823242602,1.,2.07261449292824));
#42246=CARTESIAN_POINT('Ctrl Pts',(0.576300797416844,-1.,2.07715226767559));
#42247=CARTESIAN_POINT('Ctrl Pts',(0.576300797416844,1.,2.07715226767559));
#42248=CARTESIAN_POINT('Ctrl Pts',(0.580819952108063,-1.,2.08167059018418));
#42249=CARTESIAN_POINT('Ctrl Pts',(0.580819952108063,1.,2.08167059018418));
#42250=CARTESIAN_POINT('Ctrl Pts',(0.585373918991617,-1.,2.08616943727951));
#42251=CARTESIAN_POINT('Ctrl Pts',(0.585373918991617,1.,2.08616943727951));
#42252=CARTESIAN_POINT('Ctrl Pts',(0.589962365403406,-1.,2.09064881812129));
#42253=CARTESIAN_POINT('Ctrl Pts',(0.589962365403406,1.,2.09064881812129));
#42254=CARTESIAN_POINT('Ctrl Pts',(0.594585006052162,-1.,2.0951087622027));
#42255=CARTESIAN_POINT('Ctrl Pts',(0.594585006052162,1.,2.0951087622027));
#42256=CARTESIAN_POINT('Ctrl Pts',(0.599241616420533,-1.,2.0995493086477));
#42257=CARTESIAN_POINT('Ctrl Pts',(0.599241616420533,1.,2.0995493086477));
#42258=CARTESIAN_POINT('Ctrl Pts',(0.60393203073603,-1.,2.10397049886949));
#42259=CARTESIAN_POINT('Ctrl Pts',(0.60393203073603,1.,2.10397049886949));
#42260=CARTESIAN_POINT('Ctrl Pts',(0.607711315454876,-1.,2.1074919961518));
#42261=CARTESIAN_POINT('Ctrl Pts',(0.607711315454876,1.,2.1074919961518));
#42262=CARTESIAN_POINT('Ctrl Pts',(0.610560911689898,-1.,2.11012443807238));
#42263=CARTESIAN_POINT('Ctrl Pts',(0.610560911689898,1.,2.11012443807238));
#42264=CARTESIAN_POINT('Ctrl Pts',(0.6124673655618,-1.,2.11187554259986));
#42265=CARTESIAN_POINT('Ctrl Pts',(0.6124673655618,1.,2.11187554259986));
#42266=CARTESIAN_POINT('Ctrl Pts',(0.61342227326009,-1.,2.11275013067528));
#42267=CARTESIAN_POINT('Ctrl Pts',(0.61342227326009,1.,2.11275013067528));
#42268=CARTESIAN_POINT('',(0.383122945602004,1.,1.7075470150345));
#42269=CARTESIAN_POINT('Ctrl Pts',(0.383122945602004,1.,1.7075470150345));
#42270=CARTESIAN_POINT('Ctrl Pts',(0.384119047315541,1.,1.71231062891958));
#42271=CARTESIAN_POINT('Ctrl Pts',(0.38607079032701,1.,1.72162022246158));
#42272=CARTESIAN_POINT('Ctrl Pts',(0.388877023509191,1.,1.7349317097561));
#42273=CARTESIAN_POINT('Ctrl Pts',(0.392375812294307,1.,1.75137405313962));
#42274=CARTESIAN_POINT('Ctrl Pts',(0.39634619612042,1.,1.7697556004756));
#42275=CARTESIAN_POINT('Ctrl Pts',(0.39991940378308,1.,1.78598826347533));
#42276=CARTESIAN_POINT('Ctrl Pts',(0.403107976170441,1.,1.80012077176221));
#42277=CARTESIAN_POINT('Ctrl Pts',(0.405933518411838,1.,1.81223801813988));
#42278=CARTESIAN_POINT('Ctrl Pts',(0.408428948108533,1.,1.8224702267854));
#42279=CARTESIAN_POINT('Ctrl Pts',(0.410641256301674,1.,1.83100408895216));
#42280=CARTESIAN_POINT('Ctrl Pts',(0.412633125322161,1.,1.83808953475839));
#42281=CARTESIAN_POINT('Ctrl Pts',(0.41448743825434,1.,1.8440575707371));
#42282=CARTESIAN_POINT('Ctrl Pts',(0.416300022038864,1.,1.84929312929882));
#42283=CARTESIAN_POINT('Ctrl Pts',(0.418164129143534,1.,1.85417632856234));
#42284=CARTESIAN_POINT('Ctrl Pts',(0.420157287975619,1.,1.85903281096686));
#42285=CARTESIAN_POINT('Ctrl Pts',(0.422327307418275,1.,1.86408083334028));
#42286=CARTESIAN_POINT('Ctrl Pts',(0.424678177291358,1.,1.86937803944323));
#42287=CARTESIAN_POINT('Ctrl Pts',(0.427183828519102,1.,1.87486989291484));
#42288=CARTESIAN_POINT('Ctrl Pts',(0.429803062482344,1.,1.88044229001832));
#42289=CARTESIAN_POINT('Ctrl Pts',(0.432493038548748,1.,1.88596913666793));
#42290=CARTESIAN_POINT('Ctrl Pts',(0.435225660963383,1.,1.89136993975504));
#42291=CARTESIAN_POINT('Ctrl Pts',(0.437995003948244,1.,1.89663648956466));
#42292=CARTESIAN_POINT('Ctrl Pts',(0.440807833704038,1.,1.90180124389086));
#42293=CARTESIAN_POINT('Ctrl Pts',(0.44367755684915,1.,1.90691756144898));
#42294=CARTESIAN_POINT('Ctrl Pts',(0.446617343485711,1.,1.9120369998112));
#42295=CARTESIAN_POINT('Ctrl Pts',(0.449632260106662,1.,1.91718342555755));
#42296=CARTESIAN_POINT('Ctrl Pts',(0.452719478359432,1.,1.92235380648502));
#42297=CARTESIAN_POINT('Ctrl Pts',(0.45587200517437,1.,1.92753067150476));
#42298=CARTESIAN_POINT('Ctrl Pts',(0.459081234547926,1.,1.93269066517934));
#42299=CARTESIAN_POINT('Ctrl Pts',(0.462340031009056,1.,1.93781486640821));
#42300=CARTESIAN_POINT('Ctrl Pts',(0.46564546202603,1.,1.9428979419619));
#42301=CARTESIAN_POINT('Ctrl Pts',(0.468997482913135,1.,1.94794381136514));
#42302=CARTESIAN_POINT('Ctrl Pts',(0.472397672264072,1.,1.95296148278133));
#42303=CARTESIAN_POINT('Ctrl Pts',(0.475848034683176,1.,1.95796111148177));
#42304=CARTESIAN_POINT('Ctrl Pts',(0.479349583074855,1.,1.96294933055943));
#42305=CARTESIAN_POINT('Ctrl Pts',(0.48290166212069,1.,1.96792703422362));
#42306=CARTESIAN_POINT('Ctrl Pts',(0.486502692907658,1.,1.97289186263272));
#42307=CARTESIAN_POINT('Ctrl Pts',(0.490150627860952,1.,1.97783973019229));
#42308=CARTESIAN_POINT('Ctrl Pts',(0.493843476541494,1.,1.98276658761821));
#42309=CARTESIAN_POINT('Ctrl Pts',(0.497579909545574,1.,1.98767044752932));
#42310=CARTESIAN_POINT('Ctrl Pts',(0.501359287727146,1.,1.99255149126155));
#42311=CARTESIAN_POINT('Ctrl Pts',(0.505181361323026,1.,1.99741107463572));
#42312=CARTESIAN_POINT('Ctrl Pts',(0.509046069886157,1.,2.00225107134734));
#42313=CARTESIAN_POINT('Ctrl Pts',(0.512953306961792,1.,2.00707309946949));
#42314=CARTESIAN_POINT('Ctrl Pts',(0.516902681728687,1.,2.01187773939242));
#42315=CARTESIAN_POINT('Ctrl Pts',(0.52089359039937,1.,2.01666477917286));
#42316=CARTESIAN_POINT('Ctrl Pts',(0.524925318333476,1.,2.02143356304698));
#42317=CARTESIAN_POINT('Ctrl Pts',(0.528997127241914,1.,2.0261832908329));
#42318=CARTESIAN_POINT('Ctrl Pts',(0.533108355132976,1.,2.03091336214426));
#42319=CARTESIAN_POINT('Ctrl Pts',(0.537258489833262,1.,2.03562362954037));
#42320=CARTESIAN_POINT('Ctrl Pts',(0.541447120615659,1.,2.04031422690527));
#42321=CARTESIAN_POINT('Ctrl Pts',(0.54567390381743,1.,2.04498544714588));
#42322=CARTESIAN_POINT('Ctrl Pts',(0.549938525150295,1.,2.04963761077958));
#42323=CARTESIAN_POINT('Ctrl Pts',(0.554240657463906,1.,2.05427091604413));
#42324=CARTESIAN_POINT('Ctrl Pts',(0.558579940185151,1.,2.05888537756462));
#42325=CARTESIAN_POINT('Ctrl Pts',(0.562955993082261,1.,2.06348090160589));
#42326=CARTESIAN_POINT('Ctrl Pts',(0.567368421181087,1.,2.06805732997334));
#42327=CARTESIAN_POINT('Ctrl Pts',(0.571816823242602,1.,2.07261449292824));
#42328=CARTESIAN_POINT('Ctrl Pts',(0.576300797416844,1.,2.07715226767559));
#42329=CARTESIAN_POINT('Ctrl Pts',(0.580819952108063,1.,2.08167059018418));
#42330=CARTESIAN_POINT('Ctrl Pts',(0.585373918991617,1.,2.08616943727951));
#42331=CARTESIAN_POINT('Ctrl Pts',(0.589962365403406,1.,2.09064881812129));
#42332=CARTESIAN_POINT('Ctrl Pts',(0.594585006052162,1.,2.0951087622027));
#42333=CARTESIAN_POINT('Ctrl Pts',(0.599241616420533,1.,2.0995493086477));
#42334=CARTESIAN_POINT('Ctrl Pts',(0.60393203073603,1.,2.10397049886949));
#42335=CARTESIAN_POINT('Ctrl Pts',(0.607711315454876,1.,2.1074919961518));
#42336=CARTESIAN_POINT('Ctrl Pts',(0.610560911689898,1.,2.11012443807238));
#42337=CARTESIAN_POINT('Ctrl Pts',(0.6124673655618,1.,2.11187554259986));
#42338=CARTESIAN_POINT('Ctrl Pts',(0.61342227326009,1.,2.11275013067528));
#42339=CARTESIAN_POINT('',(0.383122945602003,0.,1.7075470150345));
#42340=CARTESIAN_POINT('Origin',(0.,0.,0.));
#42341=CARTESIAN_POINT('',(0.163289472382896,1.,1.74236521665491));
#42342=CARTESIAN_POINT('Origin',(0.,1.,0.));
#42343=CARTESIAN_POINT('',(0.163289472382896,0.,1.74236521665491));
#42344=CARTESIAN_POINT('Ctrl Pts',(0.0694764450219578,-1.,2.19890268624765));
#42345=CARTESIAN_POINT('Ctrl Pts',(0.0694764450219578,1.,2.19890268624765));
#42346=CARTESIAN_POINT('Ctrl Pts',(0.0701143536325487,-1.,2.19777582085423));
#42347=CARTESIAN_POINT('Ctrl Pts',(0.0701143536325487,1.,2.19777582085423));
#42348=CARTESIAN_POINT('Ctrl Pts',(0.0713863779526151,-1.,2.19552129484002));
#42349=CARTESIAN_POINT('Ctrl Pts',(0.0713863779526151,1.,2.19552129484002));
#42350=CARTESIAN_POINT('Ctrl Pts',(0.0732830357306722,-1.,2.19213712013662));
#42351=CARTESIAN_POINT('Ctrl Pts',(0.0732830357306722,1.,2.19213712013662));
#42352=CARTESIAN_POINT('Ctrl Pts',(0.0757891465836145,-1.,2.1876201139953));
#42353=CARTESIAN_POINT('Ctrl Pts',(0.0757891465836145,1.,2.1876201139953));
#42354=CARTESIAN_POINT('Ctrl Pts',(0.078883772768524,-1.,2.18196589448887));
#42355=CARTESIAN_POINT('Ctrl Pts',(0.078883772768524,1.,2.18196589448887));
#42356=CARTESIAN_POINT('Ctrl Pts',(0.0819402680872763,-1.,2.176303712113));
#42357=CARTESIAN_POINT('Ctrl Pts',(0.0819402680872763,1.,2.176303712113));
#42358=CARTESIAN_POINT('Ctrl Pts',(0.084958462083537,-1.,2.17063357870952));
#42359=CARTESIAN_POINT('Ctrl Pts',(0.084958462083537,1.,2.17063357870952));
#42360=CARTESIAN_POINT('Ctrl Pts',(0.087938129138692,-1.,2.16495552645014));
#42361=CARTESIAN_POINT('Ctrl Pts',(0.087938129138692,1.,2.16495552645014));
#42362=CARTESIAN_POINT('Ctrl Pts',(0.0908789888107263,-1.,2.15926961544516));
#42363=CARTESIAN_POINT('Ctrl Pts',(0.0908789888107263,1.,2.15926961544516));
#42364=CARTESIAN_POINT('Ctrl Pts',(0.0937807218867641,-1.,2.1535759397817));
#42365=CARTESIAN_POINT('Ctrl Pts',(0.0937807218867641,1.,2.1535759397817));
#42366=CARTESIAN_POINT('Ctrl Pts',(0.0966429852305456,-1.,2.14787463531795));
#42367=CARTESIAN_POINT('Ctrl Pts',(0.0966429852305456,1.,2.14787463531795));
#42368=CARTESIAN_POINT('Ctrl Pts',(0.0994654261990913,-1.,2.14216588396025));
#42369=CARTESIAN_POINT('Ctrl Pts',(0.0994654261990913,1.,2.14216588396025));
#42370=CARTESIAN_POINT('Ctrl Pts',(0.1022477005561,-1.,2.13644992667165));
#42371=CARTESIAN_POINT('Ctrl Pts',(0.1022477005561,1.,2.13644992667165));
#42372=CARTESIAN_POINT('Ctrl Pts',(0.104989479152739,-1.,2.13072704887293));
#42373=CARTESIAN_POINT('Ctrl Pts',(0.104989479152739,1.,2.13072704887293));
#42374=CARTESIAN_POINT('Ctrl Pts',(0.10769043523109,-1.,2.12499752307));
#42375=CARTESIAN_POINT('Ctrl Pts',(0.10769043523109,1.,2.12499752307));
#42376=CARTESIAN_POINT('Ctrl Pts',(0.110350236135025,-1.,2.11926155590865));
#42377=CARTESIAN_POINT('Ctrl Pts',(0.110350236135025,1.,2.11926155590865));
#42378=CARTESIAN_POINT('Ctrl Pts',(0.112968534419737,-1.,2.11351924490306));
#42379=CARTESIAN_POINT('Ctrl Pts',(0.112968534419737,1.,2.11351924490306));
#42380=CARTESIAN_POINT('Ctrl Pts',(0.115544957687926,-1.,2.10777050261309));
#42381=CARTESIAN_POINT('Ctrl Pts',(0.115544957687926,1.,2.10777050261309));
#42382=CARTESIAN_POINT('Ctrl Pts',(0.118079107988355,-1.,2.102015121329));
#42383=CARTESIAN_POINT('Ctrl Pts',(0.118079107988355,1.,2.102015121329));
#42384=CARTESIAN_POINT('Ctrl Pts',(0.120570567965122,-1.,2.0962529286773));
#42385=CARTESIAN_POINT('Ctrl Pts',(0.120570567965122,1.,2.0962529286773));
#42386=CARTESIAN_POINT('Ctrl Pts',(0.123018905621083,-1.,2.09048392424825));
#42387=CARTESIAN_POINT('Ctrl Pts',(0.123018905621083,1.,2.09048392424825));
#42388=CARTESIAN_POINT('Ctrl Pts',(0.125423679412061,-1.,2.08470840653643));
#42389=CARTESIAN_POINT('Ctrl Pts',(0.125423679412061,1.,2.08470840653643));
#42390=CARTESIAN_POINT('Ctrl Pts',(0.12778444527612,-1.,2.07892715110987));
#42391=CARTESIAN_POINT('Ctrl Pts',(0.12778444527612,1.,2.07892715110987));
#42392=CARTESIAN_POINT('Ctrl Pts',(0.130100748328403,-1.,2.07314114713063));
#42393=CARTESIAN_POINT('Ctrl Pts',(0.130100748328403,1.,2.07314114713063));
#42394=CARTESIAN_POINT('Ctrl Pts',(0.13237211154771,-1.,2.06735123910326));
#42395=CARTESIAN_POINT('Ctrl Pts',(0.13237211154771,1.,2.06735123910326));
#42396=CARTESIAN_POINT('Ctrl Pts',(0.134598026192106,-1.,2.06155781517842));
#42397=CARTESIAN_POINT('Ctrl Pts',(0.134598026192106,1.,2.06155781517842));
#42398=CARTESIAN_POINT('Ctrl Pts',(0.136777941218043,-1.,2.05576044414264));
#42399=CARTESIAN_POINT('Ctrl Pts',(0.136777941218043,1.,2.05576044414264));
#42400=CARTESIAN_POINT('Ctrl Pts',(0.138911255368966,-1.,2.04995762001328));
#42401=CARTESIAN_POINT('Ctrl Pts',(0.138911255368966,1.,2.04995762001328));
#42402=CARTESIAN_POINT('Ctrl Pts',(0.140997332152546,-1.,2.04414757947916));
#42403=CARTESIAN_POINT('Ctrl Pts',(0.140997332152546,1.,2.04414757947916));
#42404=CARTESIAN_POINT('Ctrl Pts',(0.143035515058208,-1.,2.03832911025912));
#42405=CARTESIAN_POINT('Ctrl Pts',(0.143035515058208,1.,2.03832911025912));
#42406=CARTESIAN_POINT('Ctrl Pts',(0.145025140186057,-1.,2.03250223739942));
#42407=CARTESIAN_POINT('Ctrl Pts',(0.145025140186057,1.,2.03250223739942));
#42408=CARTESIAN_POINT('Ctrl Pts',(0.146965557332583,-1.,2.02666926182017));
#42409=CARTESIAN_POINT('Ctrl Pts',(0.146965557332583,1.,2.02666926182017));
#42410=CARTESIAN_POINT('Ctrl Pts',(0.148856124775337,-1.,2.02083464969894));
#42411=CARTESIAN_POINT('Ctrl Pts',(0.148856124775337,1.,2.02083464969894));
#42412=CARTESIAN_POINT('Ctrl Pts',(0.150696157673078,-1.,2.01500291940238));
#42413=CARTESIAN_POINT('Ctrl Pts',(0.150696157673078,1.,2.01500291940238));
#42414=CARTESIAN_POINT('Ctrl Pts',(0.152484883621449,-1.,2.00917680318424));
#42415=CARTESIAN_POINT('Ctrl Pts',(0.152484883621449,1.,2.00917680318424));
#42416=CARTESIAN_POINT('Ctrl Pts',(0.154221403049722,-1.,2.00335565310543));
#42417=CARTESIAN_POINT('Ctrl Pts',(0.154221403049722,1.,2.00335565310543));
#42418=CARTESIAN_POINT('Ctrl Pts',(0.155904629548783,-1.,1.99753284771497));
#42419=CARTESIAN_POINT('Ctrl Pts',(0.155904629548783,1.,1.99753284771497));
#42420=CARTESIAN_POINT('Ctrl Pts',(0.157533331459227,-1.,1.99169810931908));
#42421=CARTESIAN_POINT('Ctrl Pts',(0.157533331459227,1.,1.99169810931908));
#42422=CARTESIAN_POINT('Ctrl Pts',(0.159106226437299,-1.,1.98584238283292));
#42423=CARTESIAN_POINT('Ctrl Pts',(0.159106226437299,1.,1.98584238283292));
#42424=CARTESIAN_POINT('Ctrl Pts',(0.160622060784611,-1.,1.97996195437559));
#42425=CARTESIAN_POINT('Ctrl Pts',(0.160622060784611,1.,1.97996195437559));
#42426=CARTESIAN_POINT('Ctrl Pts',(0.162079693556288,-1.,1.97406280235188));
#42427=CARTESIAN_POINT('Ctrl Pts',(0.162079693556288,1.,1.97406280235188));
#42428=CARTESIAN_POINT('Ctrl Pts',(0.163478185457734,-1.,1.96816512677967));
#42429=CARTESIAN_POINT('Ctrl Pts',(0.163478185457734,1.,1.96816512677967));
#42430=CARTESIAN_POINT('Ctrl Pts',(0.164816568920269,-1.,1.96229379940136));
#42431=CARTESIAN_POINT('Ctrl Pts',(0.164816568920269,1.,1.96229379940136));
#42432=CARTESIAN_POINT('Ctrl Pts',(0.166093592002812,-1.,1.9564675971873));
#42433=CARTESIAN_POINT('Ctrl Pts',(0.166093592002812,1.,1.9564675971873));
#42434=CARTESIAN_POINT('Ctrl Pts',(0.167307501784475,-1.,1.95069027794294));
#42435=CARTESIAN_POINT('Ctrl Pts',(0.167307501784475,1.,1.95069027794294));
#42436=CARTESIAN_POINT('Ctrl Pts',(0.168455741607556,-1.,1.94493757756931));
#42437=CARTESIAN_POINT('Ctrl Pts',(0.168455741607556,1.,1.94493757756931));
#42438=CARTESIAN_POINT('Ctrl Pts',(0.16953490481749,-1.,1.93915639211581));
#42439=CARTESIAN_POINT('Ctrl Pts',(0.16953490481749,1.,1.93915639211581));
#42440=CARTESIAN_POINT('Ctrl Pts',(0.170541253116201,-1.,1.93329183155539));
#42441=CARTESIAN_POINT('Ctrl Pts',(0.170541253116201,1.,1.93329183155539));
#42442=CARTESIAN_POINT('Ctrl Pts',(0.171471191532988,-1.,1.92731093582036));
#42443=CARTESIAN_POINT('Ctrl Pts',(0.171471191532988,1.,1.92731093582036));
#42444=CARTESIAN_POINT('Ctrl Pts',(0.172321621259513,-1.,1.9212233439798));
#42445=CARTESIAN_POINT('Ctrl Pts',(0.172321621259513,1.,1.9212233439798));
#42446=CARTESIAN_POINT('Ctrl Pts',(0.173090695383496,-1.,1.91511429159527));
#42447=CARTESIAN_POINT('Ctrl Pts',(0.173090695383496,1.,1.91511429159527));
#42448=CARTESIAN_POINT('Ctrl Pts',(0.173776635257816,-1.,1.90911693975267));
#42449=CARTESIAN_POINT('Ctrl Pts',(0.173776635257816,1.,1.90911693975267));
#42450=CARTESIAN_POINT('Ctrl Pts',(0.174375518661085,-1.,1.90335253862834));
#42451=CARTESIAN_POINT('Ctrl Pts',(0.174375518661085,1.,1.90335253862834));
#42452=CARTESIAN_POINT('Ctrl Pts',(0.174879405091263,-1.,1.89788101117132));
#42453=CARTESIAN_POINT('Ctrl Pts',(0.174879405091263,1.,1.89788101117132));
#42454=CARTESIAN_POINT('Ctrl Pts',(0.175274276190844,-1.,1.892646301985));
#42455=CARTESIAN_POINT('Ctrl Pts',(0.175274276190844,1.,1.892646301985));
#42456=CARTESIAN_POINT('Ctrl Pts',(0.175538155840648,-1.,1.88742606273259));
#42457=CARTESIAN_POINT('Ctrl Pts',(0.175538155840648,1.,1.88742606273259));
#42458=CARTESIAN_POINT('Ctrl Pts',(0.175644148889698,-1.,1.88188663145367));
#42459=CARTESIAN_POINT('Ctrl Pts',(0.175644148889698,1.,1.88188663145367));
#42460=CARTESIAN_POINT('Ctrl Pts',(0.175563480746485,-1.,1.87563767773588));
#42461=CARTESIAN_POINT('Ctrl Pts',(0.175563480746485,1.,1.87563767773588));
#42462=CARTESIAN_POINT('Ctrl Pts',(0.175268337590757,-1.,1.86828349694799));
#42463=CARTESIAN_POINT('Ctrl Pts',(0.175268337590757,1.,1.86828349694799));
#42464=CARTESIAN_POINT('Ctrl Pts',(0.17473525927603,-1.,1.85948367088837));
#42465=CARTESIAN_POINT('Ctrl Pts',(0.17473525927603,1.,1.85948367088837));
#42466=CARTESIAN_POINT('Ctrl Pts',(0.173946627587731,-1.,1.8489811319852));
#42467=CARTESIAN_POINT('Ctrl Pts',(0.173946627587731,1.,1.8489811319852));
#42468=CARTESIAN_POINT('Ctrl Pts',(0.1728894428919,-1.,1.83658380527692));
#42469=CARTESIAN_POINT('Ctrl Pts',(0.1728894428919,1.,1.83658380527692));
#42470=CARTESIAN_POINT('Ctrl Pts',(0.171554770204119,-1.,1.82215766811545));
#42471=CARTESIAN_POINT('Ctrl Pts',(0.171554770204119,1.,1.82215766811545));
#42472=CARTESIAN_POINT('Ctrl Pts',(0.169936923904608,-1.,1.80561530629706));
#42473=CARTESIAN_POINT('Ctrl Pts',(0.169936923904608,1.,1.80561530629706));
#42474=CARTESIAN_POINT('Ctrl Pts',(0.168032772805197,-1.,1.7869064998507));
#42475=CARTESIAN_POINT('Ctrl Pts',(0.168032772805197,1.,1.7869064998507));
#42476=CARTESIAN_POINT('Ctrl Pts',(0.1662793551464,-1.,1.77018771684844));
#42477=CARTESIAN_POINT('Ctrl Pts',(0.1662793551464,1.,1.77018771684844));
#42478=CARTESIAN_POINT('Ctrl Pts',(0.164834765707158,-1.,1.75666056638427));
#42479=CARTESIAN_POINT('Ctrl Pts',(0.164834765707158,1.,1.75666056638427));
#42480=CARTESIAN_POINT('Ctrl Pts',(0.163814161002002,-1.,1.7472034950333));
#42481=CARTESIAN_POINT('Ctrl Pts',(0.163814161002002,1.,1.7472034950333));
#42482=CARTESIAN_POINT('Ctrl Pts',(0.163289472382896,-1.,1.74236521665491));
#42483=CARTESIAN_POINT('Ctrl Pts',(0.163289472382896,1.,1.74236521665491));
#42484=CARTESIAN_POINT('',(0.0694764450219578,1.,2.19890268624765));
#42485=CARTESIAN_POINT('Ctrl Pts',(0.0694764450219578,1.,2.19890268624765));
#42486=CARTESIAN_POINT('Ctrl Pts',(0.0701143536325487,1.,2.19777582085423));
#42487=CARTESIAN_POINT('Ctrl Pts',(0.0713863779526151,1.,2.19552129484002));
#42488=CARTESIAN_POINT('Ctrl Pts',(0.0732830357306722,1.,2.19213712013662));
#42489=CARTESIAN_POINT('Ctrl Pts',(0.0757891465836145,1.,2.1876201139953));
#42490=CARTESIAN_POINT('Ctrl Pts',(0.078883772768524,1.,2.18196589448887));
#42491=CARTESIAN_POINT('Ctrl Pts',(0.0819402680872763,1.,2.176303712113));
#42492=CARTESIAN_POINT('Ctrl Pts',(0.084958462083537,1.,2.17063357870952));
#42493=CARTESIAN_POINT('Ctrl Pts',(0.087938129138692,1.,2.16495552645014));
#42494=CARTESIAN_POINT('Ctrl Pts',(0.0908789888107263,1.,2.15926961544516));
#42495=CARTESIAN_POINT('Ctrl Pts',(0.0937807218867641,1.,2.1535759397817));
#42496=CARTESIAN_POINT('Ctrl Pts',(0.0966429852305456,1.,2.14787463531795));
#42497=CARTESIAN_POINT('Ctrl Pts',(0.0994654261990913,1.,2.14216588396025));
#42498=CARTESIAN_POINT('Ctrl Pts',(0.1022477005561,1.,2.13644992667165));
#42499=CARTESIAN_POINT('Ctrl Pts',(0.104989479152739,1.,2.13072704887293));
#42500=CARTESIAN_POINT('Ctrl Pts',(0.10769043523109,1.,2.12499752307));
#42501=CARTESIAN_POINT('Ctrl Pts',(0.110350236135025,1.,2.11926155590865));
#42502=CARTESIAN_POINT('Ctrl Pts',(0.112968534419737,1.,2.11351924490306));
#42503=CARTESIAN_POINT('Ctrl Pts',(0.115544957687926,1.,2.10777050261309));
#42504=CARTESIAN_POINT('Ctrl Pts',(0.118079107988355,1.,2.102015121329));
#42505=CARTESIAN_POINT('Ctrl Pts',(0.120570567965122,1.,2.0962529286773));
#42506=CARTESIAN_POINT('Ctrl Pts',(0.123018905621083,1.,2.09048392424825));
#42507=CARTESIAN_POINT('Ctrl Pts',(0.125423679412061,1.,2.08470840653643));
#42508=CARTESIAN_POINT('Ctrl Pts',(0.12778444527612,1.,2.07892715110987));
#42509=CARTESIAN_POINT('Ctrl Pts',(0.130100748328403,1.,2.07314114713063));
#42510=CARTESIAN_POINT('Ctrl Pts',(0.13237211154771,1.,2.06735123910326));
#42511=CARTESIAN_POINT('Ctrl Pts',(0.134598026192106,1.,2.06155781517842));
#42512=CARTESIAN_POINT('Ctrl Pts',(0.136777941218043,1.,2.05576044414264));
#42513=CARTESIAN_POINT('Ctrl Pts',(0.138911255368966,1.,2.04995762001328));
#42514=CARTESIAN_POINT('Ctrl Pts',(0.140997332152546,1.,2.04414757947916));
#42515=CARTESIAN_POINT('Ctrl Pts',(0.143035515058208,1.,2.03832911025912));
#42516=CARTESIAN_POINT('Ctrl Pts',(0.145025140186057,1.,2.03250223739942));
#42517=CARTESIAN_POINT('Ctrl Pts',(0.146965557332583,1.,2.02666926182017));
#42518=CARTESIAN_POINT('Ctrl Pts',(0.148856124775337,1.,2.02083464969894));
#42519=CARTESIAN_POINT('Ctrl Pts',(0.150696157673078,1.,2.01500291940238));
#42520=CARTESIAN_POINT('Ctrl Pts',(0.152484883621449,1.,2.00917680318424));
#42521=CARTESIAN_POINT('Ctrl Pts',(0.154221403049722,1.,2.00335565310543));
#42522=CARTESIAN_POINT('Ctrl Pts',(0.155904629548783,1.,1.99753284771497));
#42523=CARTESIAN_POINT('Ctrl Pts',(0.157533331459227,1.,1.99169810931908));
#42524=CARTESIAN_POINT('Ctrl Pts',(0.159106226437299,1.,1.98584238283292));
#42525=CARTESIAN_POINT('Ctrl Pts',(0.160622060784611,1.,1.97996195437559));
#42526=CARTESIAN_POINT('Ctrl Pts',(0.162079693556288,1.,1.97406280235188));
#42527=CARTESIAN_POINT('Ctrl Pts',(0.163478185457734,1.,1.96816512677967));
#42528=CARTESIAN_POINT('Ctrl Pts',(0.164816568920269,1.,1.96229379940136));
#42529=CARTESIAN_POINT('Ctrl Pts',(0.166093592002812,1.,1.9564675971873));
#42530=CARTESIAN_POINT('Ctrl Pts',(0.167307501784475,1.,1.95069027794294));
#42531=CARTESIAN_POINT('Ctrl Pts',(0.168455741607556,1.,1.94493757756931));
#42532=CARTESIAN_POINT('Ctrl Pts',(0.16953490481749,1.,1.93915639211581));
#42533=CARTESIAN_POINT('Ctrl Pts',(0.170541253116201,1.,1.93329183155539));
#42534=CARTESIAN_POINT('Ctrl Pts',(0.171471191532988,1.,1.92731093582036));
#42535=CARTESIAN_POINT('Ctrl Pts',(0.172321621259513,1.,1.9212233439798));
#42536=CARTESIAN_POINT('Ctrl Pts',(0.173090695383496,1.,1.91511429159527));
#42537=CARTESIAN_POINT('Ctrl Pts',(0.173776635257816,1.,1.90911693975267));
#42538=CARTESIAN_POINT('Ctrl Pts',(0.174375518661085,1.,1.90335253862834));
#42539=CARTESIAN_POINT('Ctrl Pts',(0.174879405091263,1.,1.89788101117132));
#42540=CARTESIAN_POINT('Ctrl Pts',(0.175274276190844,1.,1.892646301985));
#42541=CARTESIAN_POINT('Ctrl Pts',(0.175538155840648,1.,1.88742606273259));
#42542=CARTESIAN_POINT('Ctrl Pts',(0.175644148889698,1.,1.88188663145367));
#42543=CARTESIAN_POINT('Ctrl Pts',(0.175563480746485,1.,1.87563767773588));
#42544=CARTESIAN_POINT('Ctrl Pts',(0.175268337590757,1.,1.86828349694799));
#42545=CARTESIAN_POINT('Ctrl Pts',(0.17473525927603,1.,1.85948367088837));
#42546=CARTESIAN_POINT('Ctrl Pts',(0.173946627587731,1.,1.8489811319852));
#42547=CARTESIAN_POINT('Ctrl Pts',(0.1728894428919,1.,1.83658380527692));
#42548=CARTESIAN_POINT('Ctrl Pts',(0.171554770204119,1.,1.82215766811545));
#42549=CARTESIAN_POINT('Ctrl Pts',(0.169936923904608,1.,1.80561530629706));
#42550=CARTESIAN_POINT('Ctrl Pts',(0.168032772805197,1.,1.7869064998507));
#42551=CARTESIAN_POINT('Ctrl Pts',(0.1662793551464,1.,1.77018771684844));
#42552=CARTESIAN_POINT('Ctrl Pts',(0.164834765707158,1.,1.75666056638427));
#42553=CARTESIAN_POINT('Ctrl Pts',(0.163814161002002,1.,1.7472034950333));
#42554=CARTESIAN_POINT('Ctrl Pts',(0.163289472382896,1.,1.74236521665491));
#42555=CARTESIAN_POINT('',(0.0694764450219578,0.,2.19890268624765));
#42556=CARTESIAN_POINT('Origin',(-0.0694764450219586,0.,2.19890268624765));
#42557=CARTESIAN_POINT('',(-0.0694764450219586,1.,2.19890268624765));
#42558=CARTESIAN_POINT('',(0.0694764450219578,1.,2.19890268624765));
#42559=CARTESIAN_POINT('',(-0.0694764450219586,0.,2.19890268624765));
#42560=CARTESIAN_POINT('Ctrl Pts',(-0.163289472382896,-1.,1.74236521665491));
#42561=CARTESIAN_POINT('Ctrl Pts',(-0.163289472382896,1.,1.74236521665491));
#42562=CARTESIAN_POINT('Ctrl Pts',(-0.163814161002474,-1.,1.74720349503904));
#42563=CARTESIAN_POINT('Ctrl Pts',(-0.163814161002474,1.,1.74720349503904));
#42564=CARTESIAN_POINT('Ctrl Pts',(-0.164834765708484,-1.,1.75666056640041));
#42565=CARTESIAN_POINT('Ctrl Pts',(-0.164834765708484,1.,1.75666056640041));
#42566=CARTESIAN_POINT('Ctrl Pts',(-0.166279355148738,-1.,1.77018771687692));
#42567=CARTESIAN_POINT('Ctrl Pts',(-0.166279355148738,1.,1.77018771687692));
#42568=CARTESIAN_POINT('Ctrl Pts',(-0.16803277280837,-1.,1.78690649988931));
#42569=CARTESIAN_POINT('Ctrl Pts',(-0.16803277280837,1.,1.78690649988931));
#42570=CARTESIAN_POINT('Ctrl Pts',(-0.169936923908078,-1.,1.80561530633924));
#42571=CARTESIAN_POINT('Ctrl Pts',(-0.169936923908078,1.,1.80561530633924));
#42572=CARTESIAN_POINT('Ctrl Pts',(-0.171554770207306,-1.,1.82215766815414));
#42573=CARTESIAN_POINT('Ctrl Pts',(-0.171554770207306,1.,1.82215766815414));
#42574=CARTESIAN_POINT('Ctrl Pts',(-0.17288944289442,-1.,1.83658380530747));
#42575=CARTESIAN_POINT('Ctrl Pts',(-0.17288944289442,1.,1.83658380530747));
#42576=CARTESIAN_POINT('Ctrl Pts',(-0.173946627589401,-1.,1.84898113200543));
#42577=CARTESIAN_POINT('Ctrl Pts',(-0.173946627589401,1.,1.84898113200543));
#42578=CARTESIAN_POINT('Ctrl Pts',(-0.174735259276856,-1.,1.85948367089838));
#42579=CARTESIAN_POINT('Ctrl Pts',(-0.174735259276856,1.,1.85948367089838));
#42580=CARTESIAN_POINT('Ctrl Pts',(-0.175268337590901,-1.,1.86828349694972));
#42581=CARTESIAN_POINT('Ctrl Pts',(-0.175268337590901,1.,1.86828349694972));
#42582=CARTESIAN_POINT('Ctrl Pts',(-0.175563480746206,-1.,1.87563767773249));
#42583=CARTESIAN_POINT('Ctrl Pts',(-0.175563480746206,1.,1.87563767773249));
#42584=CARTESIAN_POINT('Ctrl Pts',(-0.175644148889271,-1.,1.88188663144846));
#42585=CARTESIAN_POINT('Ctrl Pts',(-0.175644148889271,1.,1.88188663144846));
#42586=CARTESIAN_POINT('Ctrl Pts',(-0.175538155840286,-1.,1.88742606272818));
#42587=CARTESIAN_POINT('Ctrl Pts',(-0.175538155840286,1.,1.88742606272818));
#42588=CARTESIAN_POINT('Ctrl Pts',(-0.175274276190664,-1.,1.89264630198279));
#42589=CARTESIAN_POINT('Ctrl Pts',(-0.175274276190664,1.,1.89264630198279));
#42590=CARTESIAN_POINT('Ctrl Pts',(-0.174879405091277,-1.,1.89788101117148));
#42591=CARTESIAN_POINT('Ctrl Pts',(-0.174879405091277,1.,1.89788101117148));
#42592=CARTESIAN_POINT('Ctrl Pts',(-0.174375518661222,-1.,1.90335253863003));
#42593=CARTESIAN_POINT('Ctrl Pts',(-0.174375518661222,1.,1.90335253863003));
#42594=CARTESIAN_POINT('Ctrl Pts',(-0.173776635257984,-1.,1.90911693975475));
#42595=CARTESIAN_POINT('Ctrl Pts',(-0.173776635257984,1.,1.90911693975475));
#42596=CARTESIAN_POINT('Ctrl Pts',(-0.173090695383619,-1.,1.91511429159681));
#42597=CARTESIAN_POINT('Ctrl Pts',(-0.173090695383619,1.,1.91511429159681));
#42598=CARTESIAN_POINT('Ctrl Pts',(-0.172321621259557,-1.,1.92122334398034));
#42599=CARTESIAN_POINT('Ctrl Pts',(-0.172321621259557,1.,1.92122334398034));
#42600=CARTESIAN_POINT('Ctrl Pts',(-0.17147119153296,-1.,1.92731093582));
#42601=CARTESIAN_POINT('Ctrl Pts',(-0.17147119153296,1.,1.92731093582));
#42602=CARTESIAN_POINT('Ctrl Pts',(-0.170541253116136,-1.,1.93329183155455));
#42603=CARTESIAN_POINT('Ctrl Pts',(-0.170541253116136,1.,1.93329183155455));
#42604=CARTESIAN_POINT('Ctrl Pts',(-0.169534904817425,-1.,1.93915639211497));
#42605=CARTESIAN_POINT('Ctrl Pts',(-0.169534904817425,1.,1.93915639211497));
#42606=CARTESIAN_POINT('Ctrl Pts',(-0.168455741607516,-1.,1.94493757756879));
#42607=CARTESIAN_POINT('Ctrl Pts',(-0.168455741607516,1.,1.94493757756879));
#42608=CARTESIAN_POINT('Ctrl Pts',(-0.167307501784469,-1.,1.95069027794286));
#42609=CARTESIAN_POINT('Ctrl Pts',(-0.167307501784469,1.,1.95069027794286));
#42610=CARTESIAN_POINT('Ctrl Pts',(-0.166093592002833,-1.,1.95646759718755));
#42611=CARTESIAN_POINT('Ctrl Pts',(-0.166093592002833,1.,1.95646759718755));
#42612=CARTESIAN_POINT('Ctrl Pts',(-0.1648165689203,-1.,1.96229379940174));
#42613=CARTESIAN_POINT('Ctrl Pts',(-0.1648165689203,1.,1.96229379940174));
#42614=CARTESIAN_POINT('Ctrl Pts',(-0.16347818545776,-1.,1.96816512678));
#42615=CARTESIAN_POINT('Ctrl Pts',(-0.16347818545776,1.,1.96816512678));
#42616=CARTESIAN_POINT('Ctrl Pts',(-0.162079693556302,-1.,1.97406280235204));
#42617=CARTESIAN_POINT('Ctrl Pts',(-0.162079693556302,1.,1.97406280235204));
#42618=CARTESIAN_POINT('Ctrl Pts',(-0.16062206078461,-1.,1.97996195437557));
#42619=CARTESIAN_POINT('Ctrl Pts',(-0.16062206078461,1.,1.97996195437557));
#42620=CARTESIAN_POINT('Ctrl Pts',(-0.159106226437289,-1.,1.98584238283279));
#42621=CARTESIAN_POINT('Ctrl Pts',(-0.159106226437289,1.,1.98584238283279));
#42622=CARTESIAN_POINT('Ctrl Pts',(-0.157533331459215,-1.,1.99169810931893));
#42623=CARTESIAN_POINT('Ctrl Pts',(-0.157533331459215,1.,1.99169810931893));
#42624=CARTESIAN_POINT('Ctrl Pts',(-0.155904629548775,-1.,1.99753284771487));
#42625=CARTESIAN_POINT('Ctrl Pts',(-0.155904629548775,1.,1.99753284771487));
#42626=CARTESIAN_POINT('Ctrl Pts',(-0.154221403049719,-1.,2.00335565310539));
#42627=CARTESIAN_POINT('Ctrl Pts',(-0.154221403049719,1.,2.00335565310539));
#42628=CARTESIAN_POINT('Ctrl Pts',(-0.152484883621452,-1.,2.00917680318426));
#42629=CARTESIAN_POINT('Ctrl Pts',(-0.152484883621452,1.,2.00917680318426));
#42630=CARTESIAN_POINT('Ctrl Pts',(-0.150696157673084,-1.,2.01500291940243));
#42631=CARTESIAN_POINT('Ctrl Pts',(-0.150696157673084,1.,2.01500291940243));
#42632=CARTESIAN_POINT('Ctrl Pts',(-0.148856124775343,-1.,2.02083464969897));
#42633=CARTESIAN_POINT('Ctrl Pts',(-0.148856124775343,1.,2.02083464969897));
#42634=CARTESIAN_POINT('Ctrl Pts',(-0.146965557332586,-1.,2.02666926182017));
#42635=CARTESIAN_POINT('Ctrl Pts',(-0.146965557332586,1.,2.02666926182017));
#42636=CARTESIAN_POINT('Ctrl Pts',(-0.145025140186058,-1.,2.03250223739941));
#42637=CARTESIAN_POINT('Ctrl Pts',(-0.145025140186058,1.,2.03250223739941));
#42638=CARTESIAN_POINT('Ctrl Pts',(-0.143035515058208,-1.,2.03832911025913));
#42639=CARTESIAN_POINT('Ctrl Pts',(-0.143035515058208,1.,2.03832911025913));
#42640=CARTESIAN_POINT('Ctrl Pts',(-0.140997332152546,-1.,2.04414757947919));
#42641=CARTESIAN_POINT('Ctrl Pts',(-0.140997332152546,1.,2.04414757947919));
#42642=CARTESIAN_POINT('Ctrl Pts',(-0.138911255368966,-1.,2.04995762001333));
#42643=CARTESIAN_POINT('Ctrl Pts',(-0.138911255368966,1.,2.04995762001333));
#42644=CARTESIAN_POINT('Ctrl Pts',(-0.136777941218044,-1.,2.0557604441427));
#42645=CARTESIAN_POINT('Ctrl Pts',(-0.136777941218044,1.,2.0557604441427));
#42646=CARTESIAN_POINT('Ctrl Pts',(-0.134598026192107,-1.,2.06155781517844));
#42647=CARTESIAN_POINT('Ctrl Pts',(-0.134598026192107,1.,2.06155781517844));
#42648=CARTESIAN_POINT('Ctrl Pts',(-0.13237211154771,-1.,2.06735123910319));
#42649=CARTESIAN_POINT('Ctrl Pts',(-0.13237211154771,1.,2.06735123910319));
#42650=CARTESIAN_POINT('Ctrl Pts',(-0.130100748328401,-1.,2.07314114713047));
#42651=CARTESIAN_POINT('Ctrl Pts',(-0.130100748328401,1.,2.07314114713047));
#42652=CARTESIAN_POINT('Ctrl Pts',(-0.127784445276116,-1.,2.07892715110967));
#42653=CARTESIAN_POINT('Ctrl Pts',(-0.127784445276116,1.,2.07892715110967));
#42654=CARTESIAN_POINT('Ctrl Pts',(-0.125423679412058,-1.,2.08470840653628));
#42655=CARTESIAN_POINT('Ctrl Pts',(-0.125423679412058,1.,2.08470840653628));
#42656=CARTESIAN_POINT('Ctrl Pts',(-0.123018905621083,-1.,2.09048392424826));
#42657=CARTESIAN_POINT('Ctrl Pts',(-0.123018905621083,1.,2.09048392424826));
#42658=CARTESIAN_POINT('Ctrl Pts',(-0.120570567965129,-1.,2.09625292867756));
#42659=CARTESIAN_POINT('Ctrl Pts',(-0.120570567965129,1.,2.09625292867756));
#42660=CARTESIAN_POINT('Ctrl Pts',(-0.118079107988368,-1.,2.10201512132945));
#42661=CARTESIAN_POINT('Ctrl Pts',(-0.118079107988368,1.,2.10201512132945));
#42662=CARTESIAN_POINT('Ctrl Pts',(-0.115544957687941,-1.,2.10777050261359));
#42663=CARTESIAN_POINT('Ctrl Pts',(-0.115544957687941,1.,2.10777050261359));
#42664=CARTESIAN_POINT('Ctrl Pts',(-0.112968534419746,-1.,2.11351924490335));
#42665=CARTESIAN_POINT('Ctrl Pts',(-0.112968534419746,1.,2.11351924490335));
#42666=CARTESIAN_POINT('Ctrl Pts',(-0.11035023613502,-1.,2.11926155590849));
#42667=CARTESIAN_POINT('Ctrl Pts',(-0.11035023613502,1.,2.11926155590849));
#42668=CARTESIAN_POINT('Ctrl Pts',(-0.107690435231068,-1.,2.12499752306927));
#42669=CARTESIAN_POINT('Ctrl Pts',(-0.107690435231068,1.,2.12499752306927));
#42670=CARTESIAN_POINT('Ctrl Pts',(-0.104989479152703,-1.,2.1307270488718));
#42671=CARTESIAN_POINT('Ctrl Pts',(-0.104989479152703,1.,2.1307270488718));
#42672=CARTESIAN_POINT('Ctrl Pts',(-0.102247700556064,-1.,2.13644992667052));
#42673=CARTESIAN_POINT('Ctrl Pts',(-0.102247700556064,1.,2.13644992667052));
#42674=CARTESIAN_POINT('Ctrl Pts',(-0.0994654261990745,-1.,2.14216588395974));
#42675=CARTESIAN_POINT('Ctrl Pts',(-0.0994654261990745,1.,2.14216588395974));
#42676=CARTESIAN_POINT('Ctrl Pts',(-0.0966429852305691,-1.,2.14787463531864));
#42677=CARTESIAN_POINT('Ctrl Pts',(-0.0966429852305691,1.,2.14787463531864));
#42678=CARTESIAN_POINT('Ctrl Pts',(-0.0937807218868348,-1.,2.15357593978377));
#42679=CARTESIAN_POINT('Ctrl Pts',(-0.0937807218868348,1.,2.15357593978377));
#42680=CARTESIAN_POINT('Ctrl Pts',(-0.0908789888108269,-1.,2.15926961544808));
#42681=CARTESIAN_POINT('Ctrl Pts',(-0.0908789888108269,1.,2.15926961544808));
#42682=CARTESIAN_POINT('Ctrl Pts',(-0.0879381291387825,-1.,2.16495552645275));
#42683=CARTESIAN_POINT('Ctrl Pts',(-0.0879381291387825,1.,2.16495552645275));
#42684=CARTESIAN_POINT('Ctrl Pts',(-0.0849584620835646,-1.,2.17063357871031));
#42685=CARTESIAN_POINT('Ctrl Pts',(-0.0849584620835646,1.,2.17063357871031));
#42686=CARTESIAN_POINT('Ctrl Pts',(-0.0819402680871942,-1.,2.1763037121106));
#42687=CARTESIAN_POINT('Ctrl Pts',(-0.0819402680871942,1.,2.1763037121106));
#42688=CARTESIAN_POINT('Ctrl Pts',(-0.078883772768323,-1.,2.18196589448304));
#42689=CARTESIAN_POINT('Ctrl Pts',(-0.078883772768323,1.,2.18196589448304));
#42690=CARTESIAN_POINT('Ctrl Pts',(-0.0757891465833414,-1.,2.1876201139874));
#42691=CARTESIAN_POINT('Ctrl Pts',(-0.0757891465833414,1.,2.1876201139874));
#42692=CARTESIAN_POINT('Ctrl Pts',(-0.0732830357304279,-1.,2.19213712012956));
#42693=CARTESIAN_POINT('Ctrl Pts',(-0.0732830357304279,1.,2.19213712012956));
#42694=CARTESIAN_POINT('Ctrl Pts',(-0.071386377952463,-1.,2.19552129483562));
#42695=CARTESIAN_POINT('Ctrl Pts',(-0.071386377952463,1.,2.19552129483562));
#42696=CARTESIAN_POINT('Ctrl Pts',(-0.0701143536324929,-1.,2.19777582085261));
#42697=CARTESIAN_POINT('Ctrl Pts',(-0.0701143536324929,1.,2.19777582085261));
#42698=CARTESIAN_POINT('Ctrl Pts',(-0.0694764450219586,-1.,2.19890268624765));
#42699=CARTESIAN_POINT('Ctrl Pts',(-0.0694764450219586,1.,2.19890268624765));
#42700=CARTESIAN_POINT('',(-0.163289472382896,1.,1.74236521665491));
#42701=CARTESIAN_POINT('Ctrl Pts',(-0.163289472382896,1.,1.74236521665491));
#42702=CARTESIAN_POINT('Ctrl Pts',(-0.163814161002474,1.,1.74720349503904));
#42703=CARTESIAN_POINT('Ctrl Pts',(-0.164834765708484,1.,1.75666056640041));
#42704=CARTESIAN_POINT('Ctrl Pts',(-0.166279355148738,1.,1.77018771687692));
#42705=CARTESIAN_POINT('Ctrl Pts',(-0.16803277280837,1.,1.78690649988931));
#42706=CARTESIAN_POINT('Ctrl Pts',(-0.169936923908078,1.,1.80561530633924));
#42707=CARTESIAN_POINT('Ctrl Pts',(-0.171554770207306,1.,1.82215766815414));
#42708=CARTESIAN_POINT('Ctrl Pts',(-0.17288944289442,1.,1.83658380530747));
#42709=CARTESIAN_POINT('Ctrl Pts',(-0.173946627589401,1.,1.84898113200543));
#42710=CARTESIAN_POINT('Ctrl Pts',(-0.174735259276856,1.,1.85948367089838));
#42711=CARTESIAN_POINT('Ctrl Pts',(-0.175268337590901,1.,1.86828349694972));
#42712=CARTESIAN_POINT('Ctrl Pts',(-0.175563480746206,1.,1.87563767773249));
#42713=CARTESIAN_POINT('Ctrl Pts',(-0.175644148889271,1.,1.88188663144846));
#42714=CARTESIAN_POINT('Ctrl Pts',(-0.175538155840286,1.,1.88742606272818));
#42715=CARTESIAN_POINT('Ctrl Pts',(-0.175274276190664,1.,1.89264630198279));
#42716=CARTESIAN_POINT('Ctrl Pts',(-0.174879405091277,1.,1.89788101117148));
#42717=CARTESIAN_POINT('Ctrl Pts',(-0.174375518661222,1.,1.90335253863003));
#42718=CARTESIAN_POINT('Ctrl Pts',(-0.173776635257984,1.,1.90911693975475));
#42719=CARTESIAN_POINT('Ctrl Pts',(-0.173090695383619,1.,1.91511429159681));
#42720=CARTESIAN_POINT('Ctrl Pts',(-0.172321621259557,1.,1.92122334398034));
#42721=CARTESIAN_POINT('Ctrl Pts',(-0.17147119153296,1.,1.92731093582));
#42722=CARTESIAN_POINT('Ctrl Pts',(-0.170541253116136,1.,1.93329183155455));
#42723=CARTESIAN_POINT('Ctrl Pts',(-0.169534904817425,1.,1.93915639211497));
#42724=CARTESIAN_POINT('Ctrl Pts',(-0.168455741607516,1.,1.94493757756879));
#42725=CARTESIAN_POINT('Ctrl Pts',(-0.167307501784469,1.,1.95069027794286));
#42726=CARTESIAN_POINT('Ctrl Pts',(-0.166093592002833,1.,1.95646759718755));
#42727=CARTESIAN_POINT('Ctrl Pts',(-0.1648165689203,1.,1.96229379940174));
#42728=CARTESIAN_POINT('Ctrl Pts',(-0.16347818545776,1.,1.96816512678));
#42729=CARTESIAN_POINT('Ctrl Pts',(-0.162079693556302,1.,1.97406280235204));
#42730=CARTESIAN_POINT('Ctrl Pts',(-0.16062206078461,1.,1.97996195437557));
#42731=CARTESIAN_POINT('Ctrl Pts',(-0.159106226437289,1.,1.98584238283279));
#42732=CARTESIAN_POINT('Ctrl Pts',(-0.157533331459215,1.,1.99169810931893));
#42733=CARTESIAN_POINT('Ctrl Pts',(-0.155904629548775,1.,1.99753284771487));
#42734=CARTESIAN_POINT('Ctrl Pts',(-0.154221403049719,1.,2.00335565310539));
#42735=CARTESIAN_POINT('Ctrl Pts',(-0.152484883621452,1.,2.00917680318426));
#42736=CARTESIAN_POINT('Ctrl Pts',(-0.150696157673084,1.,2.01500291940243));
#42737=CARTESIAN_POINT('Ctrl Pts',(-0.148856124775343,1.,2.02083464969897));
#42738=CARTESIAN_POINT('Ctrl Pts',(-0.146965557332586,1.,2.02666926182017));
#42739=CARTESIAN_POINT('Ctrl Pts',(-0.145025140186058,1.,2.03250223739941));
#42740=CARTESIAN_POINT('Ctrl Pts',(-0.143035515058208,1.,2.03832911025913));
#42741=CARTESIAN_POINT('Ctrl Pts',(-0.140997332152546,1.,2.04414757947919));
#42742=CARTESIAN_POINT('Ctrl Pts',(-0.138911255368966,1.,2.04995762001333));
#42743=CARTESIAN_POINT('Ctrl Pts',(-0.136777941218044,1.,2.0557604441427));
#42744=CARTESIAN_POINT('Ctrl Pts',(-0.134598026192107,1.,2.06155781517844));
#42745=CARTESIAN_POINT('Ctrl Pts',(-0.13237211154771,1.,2.06735123910319));
#42746=CARTESIAN_POINT('Ctrl Pts',(-0.130100748328401,1.,2.07314114713047));
#42747=CARTESIAN_POINT('Ctrl Pts',(-0.127784445276116,1.,2.07892715110967));
#42748=CARTESIAN_POINT('Ctrl Pts',(-0.125423679412058,1.,2.08470840653628));
#42749=CARTESIAN_POINT('Ctrl Pts',(-0.123018905621083,1.,2.09048392424826));
#42750=CARTESIAN_POINT('Ctrl Pts',(-0.120570567965129,1.,2.09625292867756));
#42751=CARTESIAN_POINT('Ctrl Pts',(-0.118079107988368,1.,2.10201512132945));
#42752=CARTESIAN_POINT('Ctrl Pts',(-0.115544957687941,1.,2.10777050261359));
#42753=CARTESIAN_POINT('Ctrl Pts',(-0.112968534419746,1.,2.11351924490335));
#42754=CARTESIAN_POINT('Ctrl Pts',(-0.11035023613502,1.,2.11926155590849));
#42755=CARTESIAN_POINT('Ctrl Pts',(-0.107690435231068,1.,2.12499752306927));
#42756=CARTESIAN_POINT('Ctrl Pts',(-0.104989479152703,1.,2.1307270488718));
#42757=CARTESIAN_POINT('Ctrl Pts',(-0.102247700556064,1.,2.13644992667052));
#42758=CARTESIAN_POINT('Ctrl Pts',(-0.0994654261990745,1.,2.14216588395974));
#42759=CARTESIAN_POINT('Ctrl Pts',(-0.0966429852305691,1.,2.14787463531864));
#42760=CARTESIAN_POINT('Ctrl Pts',(-0.0937807218868348,1.,2.15357593978377));
#42761=CARTESIAN_POINT('Ctrl Pts',(-0.0908789888108269,1.,2.15926961544808));
#42762=CARTESIAN_POINT('Ctrl Pts',(-0.0879381291387825,1.,2.16495552645275));
#42763=CARTESIAN_POINT('Ctrl Pts',(-0.0849584620835646,1.,2.17063357871031));
#42764=CARTESIAN_POINT('Ctrl Pts',(-0.0819402680871942,1.,2.1763037121106));
#42765=CARTESIAN_POINT('Ctrl Pts',(-0.078883772768323,1.,2.18196589448304));
#42766=CARTESIAN_POINT('Ctrl Pts',(-0.0757891465833414,1.,2.1876201139874));
#42767=CARTESIAN_POINT('Ctrl Pts',(-0.0732830357304279,1.,2.19213712012956));
#42768=CARTESIAN_POINT('Ctrl Pts',(-0.071386377952463,1.,2.19552129483562));
#42769=CARTESIAN_POINT('Ctrl Pts',(-0.0701143536324929,1.,2.19777582085261));
#42770=CARTESIAN_POINT('Ctrl Pts',(-0.0694764450219586,1.,2.19890268624765));
#42771=CARTESIAN_POINT('',(-0.163289472382897,0.,1.74236521665491));
#42772=CARTESIAN_POINT('Origin',(0.,0.,0.));
#42773=CARTESIAN_POINT('',(-0.383122945602004,1.,1.7075470150345));
#42774=CARTESIAN_POINT('Origin',(0.,1.,0.));
#42775=CARTESIAN_POINT('',(-0.383122945602004,0.,1.7075470150345));
#42776=CARTESIAN_POINT('Ctrl Pts',(-0.61342227326009,-1.,2.11275013067528));
#42777=CARTESIAN_POINT('Ctrl Pts',(-0.61342227326009,1.,2.11275013067528));
#42778=CARTESIAN_POINT('Ctrl Pts',(-0.61246736556225,-1.,2.11187554260142));
#42779=CARTESIAN_POINT('Ctrl Pts',(-0.61246736556225,1.,2.11187554260142));
#42780=CARTESIAN_POINT('Ctrl Pts',(-0.610560911691113,-1.,2.11012443807661));
#42781=CARTESIAN_POINT('Ctrl Pts',(-0.610560911691113,1.,2.11012443807661));
#42782=CARTESIAN_POINT('Ctrl Pts',(-0.607711315456826,-1.,2.10749199615859));
#42783=CARTESIAN_POINT('Ctrl Pts',(-0.607711315456826,1.,2.10749199615859));
#42784=CARTESIAN_POINT('Ctrl Pts',(-0.603932030738212,-1.,2.10397049887709));
#42785=CARTESIAN_POINT('Ctrl Pts',(-0.603932030738212,1.,2.10397049887709));
#42786=CARTESIAN_POINT('Ctrl Pts',(-0.599241616422144,-1.,2.09954930865331));
#42787=CARTESIAN_POINT('Ctrl Pts',(-0.599241616422144,1.,2.09954930865331));
#42788=CARTESIAN_POINT('Ctrl Pts',(-0.594585006052824,-1.,2.09510876220501));
#42789=CARTESIAN_POINT('Ctrl Pts',(-0.594585006052824,1.,2.09510876220501));
#42790=CARTESIAN_POINT('Ctrl Pts',(-0.589962365403189,-1.,2.09064881812053));
#42791=CARTESIAN_POINT('Ctrl Pts',(-0.589962365403189,1.,2.09064881812053));
#42792=CARTESIAN_POINT('Ctrl Pts',(-0.585373918990895,-1.,2.086169437277));
#42793=CARTESIAN_POINT('Ctrl Pts',(-0.585373918990895,1.,2.086169437277));
#42794=CARTESIAN_POINT('Ctrl Pts',(-0.580819952107257,-1.,2.08167059018138));
#42795=CARTESIAN_POINT('Ctrl Pts',(-0.580819952107257,1.,2.08167059018138));
#42796=CARTESIAN_POINT('Ctrl Pts',(-0.576300797416275,-1.,2.07715226767361));
#42797=CARTESIAN_POINT('Ctrl Pts',(-0.576300797416275,1.,2.07715226767361));
#42798=CARTESIAN_POINT('Ctrl Pts',(-0.571816823242411,-1.,2.07261449292757));
#42799=CARTESIAN_POINT('Ctrl Pts',(-0.571816823242411,1.,2.07261449292757));
#42800=CARTESIAN_POINT('Ctrl Pts',(-0.567368421181229,-1.,2.06805732997383));
#42801=CARTESIAN_POINT('Ctrl Pts',(-0.567368421181229,1.,2.06805732997383));
#42802=CARTESIAN_POINT('Ctrl Pts',(-0.562955993082574,-1.,2.06348090160697));
#42803=CARTESIAN_POINT('Ctrl Pts',(-0.562955993082574,1.,2.06348090160697));
#42804=CARTESIAN_POINT('Ctrl Pts',(-0.558579940185467,-1.,2.05888537756571));
#42805=CARTESIAN_POINT('Ctrl Pts',(-0.558579940185467,1.,2.05888537756571));
#42806=CARTESIAN_POINT('Ctrl Pts',(-0.55424065746411,-1.,2.05427091604482));
#42807=CARTESIAN_POINT('Ctrl Pts',(-0.55424065746411,1.,2.05427091604482));
#42808=CARTESIAN_POINT('Ctrl Pts',(-0.549938525150342,-1.,2.04963761077974));
#42809=CARTESIAN_POINT('Ctrl Pts',(-0.549938525150342,1.,2.04963761077974));
#42810=CARTESIAN_POINT('Ctrl Pts',(-0.545673903817348,-1.,2.0449854471456));
#42811=CARTESIAN_POINT('Ctrl Pts',(-0.545673903817348,1.,2.0449854471456));
#42812=CARTESIAN_POINT('Ctrl Pts',(-0.54144712061552,-1.,2.0403142269048));
#42813=CARTESIAN_POINT('Ctrl Pts',(-0.54144712061552,1.,2.0403142269048));
#42814=CARTESIAN_POINT('Ctrl Pts',(-0.537258489833134,-1.,2.03562362953993));
#42815=CARTESIAN_POINT('Ctrl Pts',(-0.537258489833134,1.,2.03562362953993));
#42816=CARTESIAN_POINT('Ctrl Pts',(-0.533108355132905,-1.,2.03091336214401));
#42817=CARTESIAN_POINT('Ctrl Pts',(-0.533108355132905,1.,2.03091336214401));
#42818=CARTESIAN_POINT('Ctrl Pts',(-0.528997127241911,-1.,2.02618329083289));
#42819=CARTESIAN_POINT('Ctrl Pts',(-0.528997127241911,1.,2.02618329083289));
#42820=CARTESIAN_POINT('Ctrl Pts',(-0.524925318333518,-1.,2.02143356304712));
#42821=CARTESIAN_POINT('Ctrl Pts',(-0.524925318333518,1.,2.02143356304712));
#42822=CARTESIAN_POINT('Ctrl Pts',(-0.520893590399428,-1.,2.01666477917305));
#42823=CARTESIAN_POINT('Ctrl Pts',(-0.520893590399428,1.,2.01666477917305));
#42824=CARTESIAN_POINT('Ctrl Pts',(-0.516902681728733,-1.,2.01187773939257));
#42825=CARTESIAN_POINT('Ctrl Pts',(-0.516902681728733,1.,2.01187773939257));
#42826=CARTESIAN_POINT('Ctrl Pts',(-0.512953306961814,-1.,2.00707309946955));
#42827=CARTESIAN_POINT('Ctrl Pts',(-0.512953306961814,1.,2.00707309946955));
#42828=CARTESIAN_POINT('Ctrl Pts',(-0.509046069886152,-1.,2.00225107134733));
#42829=CARTESIAN_POINT('Ctrl Pts',(-0.509046069886152,1.,2.00225107134733));
#42830=CARTESIAN_POINT('Ctrl Pts',(-0.505181361323011,-1.,1.99741107463567));
#42831=CARTESIAN_POINT('Ctrl Pts',(-0.505181361323011,1.,1.99741107463567));
#42832=CARTESIAN_POINT('Ctrl Pts',(-0.501359287727129,-1.,1.9925514912615));
#42833=CARTESIAN_POINT('Ctrl Pts',(-0.501359287727129,1.,1.9925514912615));
#42834=CARTESIAN_POINT('Ctrl Pts',(-0.497579909545564,-1.,1.98767044752929));
#42835=CARTESIAN_POINT('Ctrl Pts',(-0.497579909545564,1.,1.98767044752929));
#42836=CARTESIAN_POINT('Ctrl Pts',(-0.493843476541492,-1.,1.9827665876182));
#42837=CARTESIAN_POINT('Ctrl Pts',(-0.493843476541492,1.,1.9827665876182));
#42838=CARTESIAN_POINT('Ctrl Pts',(-0.490150627860955,-1.,1.97783973019229));
#42839=CARTESIAN_POINT('Ctrl Pts',(-0.490150627860955,1.,1.97783973019229));
#42840=CARTESIAN_POINT('Ctrl Pts',(-0.486502692907661,-1.,1.97289186263272));
#42841=CARTESIAN_POINT('Ctrl Pts',(-0.486502692907661,1.,1.97289186263272));
#42842=CARTESIAN_POINT('Ctrl Pts',(-0.482901662120687,-1.,1.96792703422358));
#42843=CARTESIAN_POINT('Ctrl Pts',(-0.482901662120687,1.,1.96792703422358));
#42844=CARTESIAN_POINT('Ctrl Pts',(-0.479349583074846,-1.,1.96294933055938));
#42845=CARTESIAN_POINT('Ctrl Pts',(-0.479349583074846,1.,1.96294933055938));
#42846=CARTESIAN_POINT('Ctrl Pts',(-0.475848034683172,-1.,1.95796111148175));
#42847=CARTESIAN_POINT('Ctrl Pts',(-0.475848034683172,1.,1.95796111148175));
#42848=CARTESIAN_POINT('Ctrl Pts',(-0.47239767226408,-1.,1.95296148278136));
#42849=CARTESIAN_POINT('Ctrl Pts',(-0.47239767226408,1.,1.95296148278136));
#42850=CARTESIAN_POINT('Ctrl Pts',(-0.468997482913158,-1.,1.94794381136524));
#42851=CARTESIAN_POINT('Ctrl Pts',(-0.468997482913158,1.,1.94794381136524));
#42852=CARTESIAN_POINT('Ctrl Pts',(-0.465645462026065,-1.,1.94289794196205));
#42853=CARTESIAN_POINT('Ctrl Pts',(-0.465645462026065,1.,1.94289794196205));
#42854=CARTESIAN_POINT('Ctrl Pts',(-0.462340031009087,-1.,1.93781486640834));
#42855=CARTESIAN_POINT('Ctrl Pts',(-0.462340031009087,1.,1.93781486640834));
#42856=CARTESIAN_POINT('Ctrl Pts',(-0.459081234547931,-1.,1.93269066517936));
#42857=CARTESIAN_POINT('Ctrl Pts',(-0.459081234547931,1.,1.93269066517936));
#42858=CARTESIAN_POINT('Ctrl Pts',(-0.455872005174335,-1.,1.92753067150461));
#42859=CARTESIAN_POINT('Ctrl Pts',(-0.455872005174335,1.,1.92753067150461));
#42860=CARTESIAN_POINT('Ctrl Pts',(-0.452719478359356,-1.,1.9223538064847));
#42861=CARTESIAN_POINT('Ctrl Pts',(-0.452719478359356,1.,1.9223538064847));
#42862=CARTESIAN_POINT('Ctrl Pts',(-0.449632260106572,-1.,1.91718342555717));
#42863=CARTESIAN_POINT('Ctrl Pts',(-0.449632260106572,1.,1.91718342555717));
#42864=CARTESIAN_POINT('Ctrl Pts',(-0.446617343485651,-1.,1.91203699981095));
#42865=CARTESIAN_POINT('Ctrl Pts',(-0.446617343485651,1.,1.91203699981095));
#42866=CARTESIAN_POINT('Ctrl Pts',(-0.44367755684917,-1.,1.90691756144906));
#42867=CARTESIAN_POINT('Ctrl Pts',(-0.44367755684917,1.,1.90691756144906));
#42868=CARTESIAN_POINT('Ctrl Pts',(-0.440807833704161,-1.,1.90180124389137));
#42869=CARTESIAN_POINT('Ctrl Pts',(-0.440807833704161,1.,1.90180124389137));
#42870=CARTESIAN_POINT('Ctrl Pts',(-0.437995003948443,-1.,1.89663648956549));
#42871=CARTESIAN_POINT('Ctrl Pts',(-0.437995003948443,1.,1.89663648956549));
#42872=CARTESIAN_POINT('Ctrl Pts',(-0.43522566096358,-1.,1.89136993975585));
#42873=CARTESIAN_POINT('Ctrl Pts',(-0.43522566096358,1.,1.89136993975585));
#42874=CARTESIAN_POINT('Ctrl Pts',(-0.432493038548833,-1.,1.88596913666828));
#42875=CARTESIAN_POINT('Ctrl Pts',(-0.432493038548833,1.,1.88596913666828));
#42876=CARTESIAN_POINT('Ctrl Pts',(-0.429803062482217,-1.,1.88044229001778));
#42877=CARTESIAN_POINT('Ctrl Pts',(-0.429803062482217,1.,1.88044229001778));
#42878=CARTESIAN_POINT('Ctrl Pts',(-0.427183828518743,-1.,1.87486989291333));
#42879=CARTESIAN_POINT('Ctrl Pts',(-0.427183828518743,1.,1.87486989291333));
#42880=CARTESIAN_POINT('Ctrl Pts',(-0.424678177290876,-1.,1.8693780394412));
#42881=CARTESIAN_POINT('Ctrl Pts',(-0.424678177290876,1.,1.8693780394412));
#42882=CARTESIAN_POINT('Ctrl Pts',(-0.422327307417885,-1.,1.86408083333863));
#42883=CARTESIAN_POINT('Ctrl Pts',(-0.422327307417885,1.,1.86408083333863));
#42884=CARTESIAN_POINT('Ctrl Pts',(-0.420157287975583,-1.,1.8590328109667));
#42885=CARTESIAN_POINT('Ctrl Pts',(-0.420157287975583,1.,1.8590328109667));
#42886=CARTESIAN_POINT('Ctrl Pts',(-0.418164129144045,-1.,1.8541763285645));
#42887=CARTESIAN_POINT('Ctrl Pts',(-0.418164129144045,1.,1.8541763285645));
#42888=CARTESIAN_POINT('Ctrl Pts',(-0.416300022039885,-1.,1.84929312930314));
#42889=CARTESIAN_POINT('Ctrl Pts',(-0.416300022039885,1.,1.84929312930314));
#42890=CARTESIAN_POINT('Ctrl Pts',(-0.414487438255542,-1.,1.84405757074218));
#42891=CARTESIAN_POINT('Ctrl Pts',(-0.414487438255542,1.,1.84405757074218));
#42892=CARTESIAN_POINT('Ctrl Pts',(-0.412633125322945,-1.,1.8380895347617));
#42893=CARTESIAN_POINT('Ctrl Pts',(-0.412633125322945,1.,1.8380895347617));
#42894=CARTESIAN_POINT('Ctrl Pts',(-0.410641256301276,-1.,1.83100408895047));
#42895=CARTESIAN_POINT('Ctrl Pts',(-0.410641256301276,1.,1.83100408895047));
#42896=CARTESIAN_POINT('Ctrl Pts',(-0.408428948106227,-1.,1.82247022677562));
#42897=CARTESIAN_POINT('Ctrl Pts',(-0.408428948106227,1.,1.82247022677562));
#42898=CARTESIAN_POINT('Ctrl Pts',(-0.405933518407175,-1.,1.81223801812013));
#42899=CARTESIAN_POINT('Ctrl Pts',(-0.405933518407175,1.,1.81223801812013));
#42900=CARTESIAN_POINT('Ctrl Pts',(-0.403107976163396,-1.,1.80012077173238));
#42901=CARTESIAN_POINT('Ctrl Pts',(-0.403107976163396,1.,1.80012077173238));
#42902=CARTESIAN_POINT('Ctrl Pts',(-0.399919403774155,-1.,1.78598826343754));
#42903=CARTESIAN_POINT('Ctrl Pts',(-0.399919403774155,1.,1.78598826343754));
#42904=CARTESIAN_POINT('Ctrl Pts',(-0.396346196110688,-1.,1.76975560043442));
#42905=CARTESIAN_POINT('Ctrl Pts',(-0.396346196110688,1.,1.76975560043442));
#42906=CARTESIAN_POINT('Ctrl Pts',(-0.392375812285395,-1.,1.75137405310193));
#42907=CARTESIAN_POINT('Ctrl Pts',(-0.392375812285395,1.,1.75137405310193));
#42908=CARTESIAN_POINT('Ctrl Pts',(-0.388877023502615,-1.,1.73493170972829));
#42909=CARTESIAN_POINT('Ctrl Pts',(-0.388877023502615,1.,1.73493170972829));
#42910=CARTESIAN_POINT('Ctrl Pts',(-0.386070790323281,-1.,1.72162022244582));
#42911=CARTESIAN_POINT('Ctrl Pts',(-0.386070790323281,1.,1.72162022244582));
#42912=CARTESIAN_POINT('Ctrl Pts',(-0.384119047314215,-1.,1.71231062891398));
#42913=CARTESIAN_POINT('Ctrl Pts',(-0.384119047314215,1.,1.71231062891398));
#42914=CARTESIAN_POINT('Ctrl Pts',(-0.383122945602004,-1.,1.7075470150345));
#42915=CARTESIAN_POINT('Ctrl Pts',(-0.383122945602004,1.,1.7075470150345));
#42916=CARTESIAN_POINT('',(-0.61342227326009,1.,2.11275013067528));
#42917=CARTESIAN_POINT('Ctrl Pts',(-0.61342227326009,1.,2.11275013067528));
#42918=CARTESIAN_POINT('Ctrl Pts',(-0.61246736556225,1.,2.11187554260142));
#42919=CARTESIAN_POINT('Ctrl Pts',(-0.610560911691113,1.,2.11012443807661));
#42920=CARTESIAN_POINT('Ctrl Pts',(-0.607711315456826,1.,2.10749199615859));
#42921=CARTESIAN_POINT('Ctrl Pts',(-0.603932030738212,1.,2.10397049887709));
#42922=CARTESIAN_POINT('Ctrl Pts',(-0.599241616422144,1.,2.09954930865331));
#42923=CARTESIAN_POINT('Ctrl Pts',(-0.594585006052824,1.,2.09510876220501));
#42924=CARTESIAN_POINT('Ctrl Pts',(-0.589962365403189,1.,2.09064881812053));
#42925=CARTESIAN_POINT('Ctrl Pts',(-0.585373918990895,1.,2.086169437277));
#42926=CARTESIAN_POINT('Ctrl Pts',(-0.580819952107257,1.,2.08167059018138));
#42927=CARTESIAN_POINT('Ctrl Pts',(-0.576300797416275,1.,2.07715226767361));
#42928=CARTESIAN_POINT('Ctrl Pts',(-0.571816823242411,1.,2.07261449292757));
#42929=CARTESIAN_POINT('Ctrl Pts',(-0.567368421181229,1.,2.06805732997383));
#42930=CARTESIAN_POINT('Ctrl Pts',(-0.562955993082574,1.,2.06348090160697));
#42931=CARTESIAN_POINT('Ctrl Pts',(-0.558579940185467,1.,2.05888537756571));
#42932=CARTESIAN_POINT('Ctrl Pts',(-0.55424065746411,1.,2.05427091604482));
#42933=CARTESIAN_POINT('Ctrl Pts',(-0.549938525150342,1.,2.04963761077974));
#42934=CARTESIAN_POINT('Ctrl Pts',(-0.545673903817348,1.,2.0449854471456));
#42935=CARTESIAN_POINT('Ctrl Pts',(-0.54144712061552,1.,2.0403142269048));
#42936=CARTESIAN_POINT('Ctrl Pts',(-0.537258489833134,1.,2.03562362953993));
#42937=CARTESIAN_POINT('Ctrl Pts',(-0.533108355132905,1.,2.03091336214401));
#42938=CARTESIAN_POINT('Ctrl Pts',(-0.528997127241911,1.,2.02618329083289));
#42939=CARTESIAN_POINT('Ctrl Pts',(-0.524925318333518,1.,2.02143356304712));
#42940=CARTESIAN_POINT('Ctrl Pts',(-0.520893590399428,1.,2.01666477917305));
#42941=CARTESIAN_POINT('Ctrl Pts',(-0.516902681728733,1.,2.01187773939257));
#42942=CARTESIAN_POINT('Ctrl Pts',(-0.512953306961814,1.,2.00707309946955));
#42943=CARTESIAN_POINT('Ctrl Pts',(-0.509046069886152,1.,2.00225107134733));
#42944=CARTESIAN_POINT('Ctrl Pts',(-0.505181361323011,1.,1.99741107463567));
#42945=CARTESIAN_POINT('Ctrl Pts',(-0.501359287727129,1.,1.9925514912615));
#42946=CARTESIAN_POINT('Ctrl Pts',(-0.497579909545564,1.,1.98767044752929));
#42947=CARTESIAN_POINT('Ctrl Pts',(-0.493843476541492,1.,1.9827665876182));
#42948=CARTESIAN_POINT('Ctrl Pts',(-0.490150627860955,1.,1.97783973019229));
#42949=CARTESIAN_POINT('Ctrl Pts',(-0.486502692907661,1.,1.97289186263272));
#42950=CARTESIAN_POINT('Ctrl Pts',(-0.482901662120687,1.,1.96792703422358));
#42951=CARTESIAN_POINT('Ctrl Pts',(-0.479349583074846,1.,1.96294933055938));
#42952=CARTESIAN_POINT('Ctrl Pts',(-0.475848034683172,1.,1.95796111148175));
#42953=CARTESIAN_POINT('Ctrl Pts',(-0.47239767226408,1.,1.95296148278136));
#42954=CARTESIAN_POINT('Ctrl Pts',(-0.468997482913158,1.,1.94794381136524));
#42955=CARTESIAN_POINT('Ctrl Pts',(-0.465645462026065,1.,1.94289794196205));
#42956=CARTESIAN_POINT('Ctrl Pts',(-0.462340031009087,1.,1.93781486640834));
#42957=CARTESIAN_POINT('Ctrl Pts',(-0.459081234547931,1.,1.93269066517936));
#42958=CARTESIAN_POINT('Ctrl Pts',(-0.455872005174335,1.,1.92753067150461));
#42959=CARTESIAN_POINT('Ctrl Pts',(-0.452719478359356,1.,1.9223538064847));
#42960=CARTESIAN_POINT('Ctrl Pts',(-0.449632260106572,1.,1.91718342555717));
#42961=CARTESIAN_POINT('Ctrl Pts',(-0.446617343485651,1.,1.91203699981095));
#42962=CARTESIAN_POINT('Ctrl Pts',(-0.44367755684917,1.,1.90691756144906));
#42963=CARTESIAN_POINT('Ctrl Pts',(-0.440807833704161,1.,1.90180124389137));
#42964=CARTESIAN_POINT('Ctrl Pts',(-0.437995003948443,1.,1.89663648956549));
#42965=CARTESIAN_POINT('Ctrl Pts',(-0.43522566096358,1.,1.89136993975585));
#42966=CARTESIAN_POINT('Ctrl Pts',(-0.432493038548833,1.,1.88596913666828));
#42967=CARTESIAN_POINT('Ctrl Pts',(-0.429803062482217,1.,1.88044229001778));
#42968=CARTESIAN_POINT('Ctrl Pts',(-0.427183828518743,1.,1.87486989291333));
#42969=CARTESIAN_POINT('Ctrl Pts',(-0.424678177290876,1.,1.8693780394412));
#42970=CARTESIAN_POINT('Ctrl Pts',(-0.422327307417885,1.,1.86408083333863));
#42971=CARTESIAN_POINT('Ctrl Pts',(-0.420157287975583,1.,1.8590328109667));
#42972=CARTESIAN_POINT('Ctrl Pts',(-0.418164129144045,1.,1.8541763285645));
#42973=CARTESIAN_POINT('Ctrl Pts',(-0.416300022039885,1.,1.84929312930314));
#42974=CARTESIAN_POINT('Ctrl Pts',(-0.414487438255542,1.,1.84405757074218));
#42975=CARTESIAN_POINT('Ctrl Pts',(-0.412633125322945,1.,1.8380895347617));
#42976=CARTESIAN_POINT('Ctrl Pts',(-0.410641256301276,1.,1.83100408895047));
#42977=CARTESIAN_POINT('Ctrl Pts',(-0.408428948106227,1.,1.82247022677562));
#42978=CARTESIAN_POINT('Ctrl Pts',(-0.405933518407175,1.,1.81223801812013));
#42979=CARTESIAN_POINT('Ctrl Pts',(-0.403107976163396,1.,1.80012077173238));
#42980=CARTESIAN_POINT('Ctrl Pts',(-0.399919403774155,1.,1.78598826343754));
#42981=CARTESIAN_POINT('Ctrl Pts',(-0.396346196110688,1.,1.76975560043442));
#42982=CARTESIAN_POINT('Ctrl Pts',(-0.392375812285395,1.,1.75137405310193));
#42983=CARTESIAN_POINT('Ctrl Pts',(-0.388877023502615,1.,1.73493170972829));
#42984=CARTESIAN_POINT('Ctrl Pts',(-0.386070790323281,1.,1.72162022244582));
#42985=CARTESIAN_POINT('Ctrl Pts',(-0.384119047314215,1.,1.71231062891398));
#42986=CARTESIAN_POINT('Ctrl Pts',(-0.383122945602004,1.,1.7075470150345));
#42987=CARTESIAN_POINT('',(-0.61342227326009,0.,2.11275013067528));
#42988=CARTESIAN_POINT('Origin',(-0.745574324794401,0.,2.0698113262342));
#42989=CARTESIAN_POINT('',(-0.745574324794401,1.,2.0698113262342));
#42990=CARTESIAN_POINT('',(-0.61342227326009,1.,2.11275013067528));
#42991=CARTESIAN_POINT('',(-0.745574324794401,0.,2.0698113262342));
#42992=CARTESIAN_POINT('Ctrl Pts',(-0.693717979106306,-1.,1.60662857109684));
#42993=CARTESIAN_POINT('Ctrl Pts',(-0.693717979106306,1.,1.60662857109684));
#42994=CARTESIAN_POINT('Ctrl Pts',(-0.695712097881194,-1.,1.61106790958151));
#42995=CARTESIAN_POINT('Ctrl Pts',(-0.695712097881194,1.,1.61106790958151));
#42996=CARTESIAN_POINT('Ctrl Pts',(-0.699605146405088,-1.,1.61974673472612));
#42997=CARTESIAN_POINT('Ctrl Pts',(-0.699605146405088,1.,1.61974673472612));
#42998=CARTESIAN_POINT('Ctrl Pts',(-0.705159151988319,-1.,1.63216541664676));
#42999=CARTESIAN_POINT('Ctrl Pts',(-0.705159151988319,1.,1.63216541664676));
#43000=CARTESIAN_POINT('Ctrl Pts',(-0.711993139355394,-1.,1.64752408832016));
#43001=CARTESIAN_POINT('Ctrl Pts',(-0.711993139355394,1.,1.64752408832016));
#43002=CARTESIAN_POINT('Ctrl Pts',(-0.719585433804282,-1.,1.6647288055568));
#43003=CARTESIAN_POINT('Ctrl Pts',(-0.719585433804282,1.,1.6647288055568));
#43004=CARTESIAN_POINT('Ctrl Pts',(-0.726235967997433,-1.,1.67996158455503));
#43005=CARTESIAN_POINT('Ctrl Pts',(-0.726235967997433,1.,1.67996158455503));
#43006=CARTESIAN_POINT('Ctrl Pts',(-0.731963238697195,-1.,1.69326921975743));
#43007=CARTESIAN_POINT('Ctrl Pts',(-0.731963238697195,1.,1.69326921975743));
#43008=CARTESIAN_POINT('Ctrl Pts',(-0.736799665724771,-1.,1.70473309006121));
#43009=CARTESIAN_POINT('Ctrl Pts',(-0.736799665724771,1.,1.70473309006121));
#43010=CARTESIAN_POINT('Ctrl Pts',(-0.740795162032088,-1.,1.71447789751927));
#43011=CARTESIAN_POINT('Ctrl Pts',(-0.740795162032088,1.,1.71447789751927));
#43012=CARTESIAN_POINT('Ctrl Pts',(-0.744021445433764,-1.,1.7226822991693));
#43013=CARTESIAN_POINT('Ctrl Pts',(-0.744021445433764,1.,1.7226822991693));
#43014=CARTESIAN_POINT('Ctrl Pts',(-0.746574710096436,-1.,1.72958533647399));
#43015=CARTESIAN_POINT('Ctrl Pts',(-0.746574710096436,1.,1.72958533647399));
#43016=CARTESIAN_POINT('Ctrl Pts',(-0.748582462954855,-1.,1.73550351679848));
#43017=CARTESIAN_POINT('Ctrl Pts',(-0.748582462954855,1.,1.73550351679848));
#43018=CARTESIAN_POINT('Ctrl Pts',(-0.75019343597954,-1.,1.74080458266705));
#43019=CARTESIAN_POINT('Ctrl Pts',(-0.75019343597954,1.,1.74080458266705));
#43020=CARTESIAN_POINT('Ctrl Pts',(-0.751555614163629,-1.,1.74585086852298));
#43021=CARTESIAN_POINT('Ctrl Pts',(-0.751555614163629,1.,1.74585086852298));
#43022=CARTESIAN_POINT('Ctrl Pts',(-0.752797683531377,-1.,1.75095139468809));
#43023=CARTESIAN_POINT('Ctrl Pts',(-0.752797683531377,1.,1.75095139468809));
#43024=CARTESIAN_POINT('Ctrl Pts',(-0.75400925402848,-1.,1.75631083600175));
#43025=CARTESIAN_POINT('Ctrl Pts',(-0.75400925402848,1.,1.75631083600175));
#43026=CARTESIAN_POINT('Ctrl Pts',(-0.755220979975262,-1.,1.7619781724032));
#43027=CARTESIAN_POINT('Ctrl Pts',(-0.755220979975262,1.,1.7619781724032));
#43028=CARTESIAN_POINT('Ctrl Pts',(-0.756421896028403,-1.,1.76789396003141));
#43029=CARTESIAN_POINT('Ctrl Pts',(-0.756421896028403,1.,1.76789396003141));
#43030=CARTESIAN_POINT('Ctrl Pts',(-0.757578264077238,-1.,1.77394167108342));
#43031=CARTESIAN_POINT('Ctrl Pts',(-0.757578264077238,1.,1.77394167108342));
#43032=CARTESIAN_POINT('Ctrl Pts',(-0.75865062667738,-1.,1.77999411220912));
#43033=CARTESIAN_POINT('Ctrl Pts',(-0.75865062667738,1.,1.77999411220912));
#43034=CARTESIAN_POINT('Ctrl Pts',(-0.759614401109868,-1.,1.78596964884526));
#43035=CARTESIAN_POINT('Ctrl Pts',(-0.759614401109868,1.,1.78596964884526));
#43036=CARTESIAN_POINT('Ctrl Pts',(-0.760469555880425,-1.,1.79185815610802));
#43037=CARTESIAN_POINT('Ctrl Pts',(-0.760469555880425,1.,1.79185815610802));
#43038=CARTESIAN_POINT('Ctrl Pts',(-0.761229695230359,-1.,1.79768986997735));
#43039=CARTESIAN_POINT('Ctrl Pts',(-0.761229695230359,1.,1.79768986997735));
#43040=CARTESIAN_POINT('Ctrl Pts',(-0.761915336443516,-1.,1.80351583877334));
#43041=CARTESIAN_POINT('Ctrl Pts',(-0.761915336443516,1.,1.80351583877334));
#43042=CARTESIAN_POINT('Ctrl Pts',(-0.762546129464036,-1.,1.80938551463989));
#43043=CARTESIAN_POINT('Ctrl Pts',(-0.762546129464036,1.,1.80938551463989));
#43044=CARTESIAN_POINT('Ctrl Pts',(-0.763132003836783,-1.,1.81532118405566));
#43045=CARTESIAN_POINT('Ctrl Pts',(-0.763132003836783,1.,1.81532118405566));
#43046=CARTESIAN_POINT('Ctrl Pts',(-0.763673465462854,-1.,1.82131873145297));
#43047=CARTESIAN_POINT('Ctrl Pts',(-0.763673465462854,1.,1.82131873145297));
#43048=CARTESIAN_POINT('Ctrl Pts',(-0.764165902606055,-1.,1.8273599120008));
#43049=CARTESIAN_POINT('Ctrl Pts',(-0.764165902606055,1.,1.8273599120008));
#43050=CARTESIAN_POINT('Ctrl Pts',(-0.764602549687845,-1.,1.8334207722714));
#43051=CARTESIAN_POINT('Ctrl Pts',(-0.764602549687845,1.,1.8334207722714));
#43052=CARTESIAN_POINT('Ctrl Pts',(-0.764978057881687,-1.,1.83948181064823));
#43053=CARTESIAN_POINT('Ctrl Pts',(-0.764978057881687,1.,1.83948181064823));
#43054=CARTESIAN_POINT('Ctrl Pts',(-0.765291664861971,-1.,1.8455369887591));
#43055=CARTESIAN_POINT('Ctrl Pts',(-0.765291664861971,1.,1.8455369887591));
#43056=CARTESIAN_POINT('Ctrl Pts',(-0.765545710619023,-1.,1.85158945130054));
#43057=CARTESIAN_POINT('Ctrl Pts',(-0.765545710619023,1.,1.85158945130054));
#43058=CARTESIAN_POINT('Ctrl Pts',(-0.765744212909305,-1.,1.85764741390391));
#43059=CARTESIAN_POINT('Ctrl Pts',(-0.765744212909305,1.,1.85764741390391));
#43060=CARTESIAN_POINT('Ctrl Pts',(-0.765891519092557,-1.,1.86372027063314));
#43061=CARTESIAN_POINT('Ctrl Pts',(-0.765891519092557,1.,1.86372027063314));
#43062=CARTESIAN_POINT('Ctrl Pts',(-0.765990708546111,-1.,1.86981398314345));
#43063=CARTESIAN_POINT('Ctrl Pts',(-0.765990708546111,1.,1.86981398314345));
#43064=CARTESIAN_POINT('Ctrl Pts',(-0.766042837036759,-1.,1.87592888967886));
#43065=CARTESIAN_POINT('Ctrl Pts',(-0.766042837036759,1.,1.87592888967886));
#43066=CARTESIAN_POINT('Ctrl Pts',(-0.766047794851869,-1.,1.88206215302561));
#43067=CARTESIAN_POINT('Ctrl Pts',(-0.766047794851869,1.,1.88206215302561));
#43068=CARTESIAN_POINT('Ctrl Pts',(-0.76600483706209,-1.,1.88820926433409));
#43069=CARTESIAN_POINT('Ctrl Pts',(-0.76600483706209,1.,1.88820926433409));
#43070=CARTESIAN_POINT('Ctrl Pts',(-0.765913193856979,-1.,1.89436577771389));
#43071=CARTESIAN_POINT('Ctrl Pts',(-0.765913193856979,1.,1.89436577771389));
#43072=CARTESIAN_POINT('Ctrl Pts',(-0.765772772593395,-1.,1.90052930393599));
#43073=CARTESIAN_POINT('Ctrl Pts',(-0.765772772593395,1.,1.90052930393599));
#43074=CARTESIAN_POINT('Ctrl Pts',(-0.765584196937936,-1.,1.90669961402362));
#43075=CARTESIAN_POINT('Ctrl Pts',(-0.765584196937936,1.,1.90669961402362));
#43076=CARTESIAN_POINT('Ctrl Pts',(-0.765348465884739,-1.,1.91287765805174));
#43077=CARTESIAN_POINT('Ctrl Pts',(-0.765348465884739,1.,1.91287765805174));
#43078=CARTESIAN_POINT('Ctrl Pts',(-0.765066729667095,-1.,1.91906491634197));
#43079=CARTESIAN_POINT('Ctrl Pts',(-0.765066729667095,1.,1.91906491634197));
#43080=CARTESIAN_POINT('Ctrl Pts',(-0.764740025488189,-1.,1.92526263537041));
#43081=CARTESIAN_POINT('Ctrl Pts',(-0.764740025488189,1.,1.92526263537041));
#43082=CARTESIAN_POINT('Ctrl Pts',(-0.764369010673889,-1.,1.93147105496367));
#43083=CARTESIAN_POINT('Ctrl Pts',(-0.764369010673889,1.,1.93147105496367));
#43084=CARTESIAN_POINT('Ctrl Pts',(-0.763954049121393,-1.,1.93768964875867));
#43085=CARTESIAN_POINT('Ctrl Pts',(-0.763954049121393,1.,1.93768964875867));
#43086=CARTESIAN_POINT('Ctrl Pts',(-0.76349533353858,-1.,1.94391746617626));
#43087=CARTESIAN_POINT('Ctrl Pts',(-0.76349533353858,1.,1.94391746617626));
#43088=CARTESIAN_POINT('Ctrl Pts',(-0.762992990878774,-1.,1.95015342590025));
#43089=CARTESIAN_POINT('Ctrl Pts',(-0.762992990878774,1.,1.95015342590025));
#43090=CARTESIAN_POINT('Ctrl Pts',(-0.762447203806263,-1.,1.95639665309893));
#43091=CARTESIAN_POINT('Ctrl Pts',(-0.762447203806263,1.,1.95639665309893));
#43092=CARTESIAN_POINT('Ctrl Pts',(-0.761858300014575,-1.,1.96264672744229));
#43093=CARTESIAN_POINT('Ctrl Pts',(-0.761858300014575,1.,1.96264672744229));
#43094=CARTESIAN_POINT('Ctrl Pts',(-0.761226690483986,-1.,1.96890351582545));
#43095=CARTESIAN_POINT('Ctrl Pts',(-0.761226690483986,1.,1.96890351582545));
#43096=CARTESIAN_POINT('Ctrl Pts',(-0.760552825409855,-1.,1.97516705321521));
#43097=CARTESIAN_POINT('Ctrl Pts',(-0.760552825409855,1.,1.97516705321521));
#43098=CARTESIAN_POINT('Ctrl Pts',(-0.759837147452135,-1.,1.98143741418156));
#43099=CARTESIAN_POINT('Ctrl Pts',(-0.759837147452135,1.,1.98143741418156));
#43100=CARTESIAN_POINT('Ctrl Pts',(-0.759080037802243,-1.,1.98771456680806));
#43101=CARTESIAN_POINT('Ctrl Pts',(-0.759080037802243,1.,1.98771456680806));
#43102=CARTESIAN_POINT('Ctrl Pts',(-0.758281796766377,-1.,1.9939983109871));
#43103=CARTESIAN_POINT('Ctrl Pts',(-0.758281796766377,1.,1.9939983109871));
#43104=CARTESIAN_POINT('Ctrl Pts',(-0.757442676862341,-1.,2.00028834739072));
#43105=CARTESIAN_POINT('Ctrl Pts',(-0.757442676862341,1.,2.00028834739072));
#43106=CARTESIAN_POINT('Ctrl Pts',(-0.756562904646496,-1.,2.00658431587682));
#43107=CARTESIAN_POINT('Ctrl Pts',(-0.756562904646496,1.,2.00658431587682));
#43108=CARTESIAN_POINT('Ctrl Pts',(-0.7556427049581,-1.,2.01288584328149));
#43109=CARTESIAN_POINT('Ctrl Pts',(-0.7556427049581,1.,2.01288584328149));
#43110=CARTESIAN_POINT('Ctrl Pts',(-0.75468233072352,-1.,2.01919259406003));
#43111=CARTESIAN_POINT('Ctrl Pts',(-0.75468233072352,1.,2.01919259406003));
#43112=CARTESIAN_POINT('Ctrl Pts',(-0.753682061113766,-1.,2.02550428623587));
#43113=CARTESIAN_POINT('Ctrl Pts',(-0.753682061113766,1.,2.02550428623587));
#43114=CARTESIAN_POINT('Ctrl Pts',(-0.752642180488104,-1.,2.03182068456467));
#43115=CARTESIAN_POINT('Ctrl Pts',(-0.752642180488104,1.,2.03182068456467));
#43116=CARTESIAN_POINT('Ctrl Pts',(-0.751562963361384,-1.,2.03814160092173));
#43117=CARTESIAN_POINT('Ctrl Pts',(-0.751562963361384,1.,2.03814160092173));
#43118=CARTESIAN_POINT('Ctrl Pts',(-0.750444657874758,-1.,2.04446689147754));
#43119=CARTESIAN_POINT('Ctrl Pts',(-0.750444657874758,1.,2.04446689147754));
#43120=CARTESIAN_POINT('Ctrl Pts',(-0.749287468663053,-1.,2.05079645591606));
#43121=CARTESIAN_POINT('Ctrl Pts',(-0.749287468663053,1.,2.05079645591606));
#43122=CARTESIAN_POINT('Ctrl Pts',(-0.748091554181101,-1.,2.05713023030263));
#43123=CARTESIAN_POINT('Ctrl Pts',(-0.748091554181101,1.,2.05713023030263));
#43124=CARTESIAN_POINT('Ctrl Pts',(-0.747103932785504,-1.,2.06220058927162));
#43125=CARTESIAN_POINT('Ctrl Pts',(-0.747103932785504,1.,2.06220058927162));
#43126=CARTESIAN_POINT('Ctrl Pts',(-0.746345871542696,-1.,2.06600523016401));
#43127=CARTESIAN_POINT('Ctrl Pts',(-0.746345871542696,1.,2.06600523016401));
#43128=CARTESIAN_POINT('Ctrl Pts',(-0.74583279137781,-1.,2.06854248895575));
#43129=CARTESIAN_POINT('Ctrl Pts',(-0.74583279137781,1.,2.06854248895575));
#43130=CARTESIAN_POINT('Ctrl Pts',(-0.745574324794401,-1.,2.0698113262342));
#43131=CARTESIAN_POINT('Ctrl Pts',(-0.745574324794401,1.,2.0698113262342));
#43132=CARTESIAN_POINT('',(-0.693717979106306,1.,1.60662857109684));
#43133=CARTESIAN_POINT('Ctrl Pts',(-0.693717979106306,1.,1.60662857109684));
#43134=CARTESIAN_POINT('Ctrl Pts',(-0.695712097881194,1.,1.61106790958151));
#43135=CARTESIAN_POINT('Ctrl Pts',(-0.699605146405088,1.,1.61974673472612));
#43136=CARTESIAN_POINT('Ctrl Pts',(-0.705159151988319,1.,1.63216541664676));
#43137=CARTESIAN_POINT('Ctrl Pts',(-0.711993139355394,1.,1.64752408832016));
#43138=CARTESIAN_POINT('Ctrl Pts',(-0.719585433804282,1.,1.6647288055568));
#43139=CARTESIAN_POINT('Ctrl Pts',(-0.726235967997433,1.,1.67996158455503));
#43140=CARTESIAN_POINT('Ctrl Pts',(-0.731963238697195,1.,1.69326921975743));
#43141=CARTESIAN_POINT('Ctrl Pts',(-0.736799665724771,1.,1.70473309006121));
#43142=CARTESIAN_POINT('Ctrl Pts',(-0.740795162032088,1.,1.71447789751927));
#43143=CARTESIAN_POINT('Ctrl Pts',(-0.744021445433764,1.,1.7226822991693));
#43144=CARTESIAN_POINT('Ctrl Pts',(-0.746574710096436,1.,1.72958533647399));
#43145=CARTESIAN_POINT('Ctrl Pts',(-0.748582462954855,1.,1.73550351679848));
#43146=CARTESIAN_POINT('Ctrl Pts',(-0.75019343597954,1.,1.74080458266705));
#43147=CARTESIAN_POINT('Ctrl Pts',(-0.751555614163629,1.,1.74585086852298));
#43148=CARTESIAN_POINT('Ctrl Pts',(-0.752797683531377,1.,1.75095139468809));
#43149=CARTESIAN_POINT('Ctrl Pts',(-0.75400925402848,1.,1.75631083600175));
#43150=CARTESIAN_POINT('Ctrl Pts',(-0.755220979975262,1.,1.7619781724032));
#43151=CARTESIAN_POINT('Ctrl Pts',(-0.756421896028403,1.,1.76789396003141));
#43152=CARTESIAN_POINT('Ctrl Pts',(-0.757578264077238,1.,1.77394167108342));
#43153=CARTESIAN_POINT('Ctrl Pts',(-0.75865062667738,1.,1.77999411220912));
#43154=CARTESIAN_POINT('Ctrl Pts',(-0.759614401109868,1.,1.78596964884526));
#43155=CARTESIAN_POINT('Ctrl Pts',(-0.760469555880425,1.,1.79185815610802));
#43156=CARTESIAN_POINT('Ctrl Pts',(-0.761229695230359,1.,1.79768986997735));
#43157=CARTESIAN_POINT('Ctrl Pts',(-0.761915336443516,1.,1.80351583877334));
#43158=CARTESIAN_POINT('Ctrl Pts',(-0.762546129464036,1.,1.80938551463989));
#43159=CARTESIAN_POINT('Ctrl Pts',(-0.763132003836783,1.,1.81532118405566));
#43160=CARTESIAN_POINT('Ctrl Pts',(-0.763673465462854,1.,1.82131873145297));
#43161=CARTESIAN_POINT('Ctrl Pts',(-0.764165902606055,1.,1.8273599120008));
#43162=CARTESIAN_POINT('Ctrl Pts',(-0.764602549687845,1.,1.8334207722714));
#43163=CARTESIAN_POINT('Ctrl Pts',(-0.764978057881687,1.,1.83948181064823));
#43164=CARTESIAN_POINT('Ctrl Pts',(-0.765291664861971,1.,1.8455369887591));
#43165=CARTESIAN_POINT('Ctrl Pts',(-0.765545710619023,1.,1.85158945130054));
#43166=CARTESIAN_POINT('Ctrl Pts',(-0.765744212909305,1.,1.85764741390391));
#43167=CARTESIAN_POINT('Ctrl Pts',(-0.765891519092557,1.,1.86372027063314));
#43168=CARTESIAN_POINT('Ctrl Pts',(-0.765990708546111,1.,1.86981398314345));
#43169=CARTESIAN_POINT('Ctrl Pts',(-0.766042837036759,1.,1.87592888967886));
#43170=CARTESIAN_POINT('Ctrl Pts',(-0.766047794851869,1.,1.88206215302561));
#43171=CARTESIAN_POINT('Ctrl Pts',(-0.76600483706209,1.,1.88820926433409));
#43172=CARTESIAN_POINT('Ctrl Pts',(-0.765913193856979,1.,1.89436577771389));
#43173=CARTESIAN_POINT('Ctrl Pts',(-0.765772772593395,1.,1.90052930393599));
#43174=CARTESIAN_POINT('Ctrl Pts',(-0.765584196937936,1.,1.90669961402362));
#43175=CARTESIAN_POINT('Ctrl Pts',(-0.765348465884739,1.,1.91287765805174));
#43176=CARTESIAN_POINT('Ctrl Pts',(-0.765066729667095,1.,1.91906491634197));
#43177=CARTESIAN_POINT('Ctrl Pts',(-0.764740025488189,1.,1.92526263537041));
#43178=CARTESIAN_POINT('Ctrl Pts',(-0.764369010673889,1.,1.93147105496367));
#43179=CARTESIAN_POINT('Ctrl Pts',(-0.763954049121393,1.,1.93768964875867));
#43180=CARTESIAN_POINT('Ctrl Pts',(-0.76349533353858,1.,1.94391746617626));
#43181=CARTESIAN_POINT('Ctrl Pts',(-0.762992990878774,1.,1.95015342590025));
#43182=CARTESIAN_POINT('Ctrl Pts',(-0.762447203806263,1.,1.95639665309893));
#43183=CARTESIAN_POINT('Ctrl Pts',(-0.761858300014575,1.,1.96264672744229));
#43184=CARTESIAN_POINT('Ctrl Pts',(-0.761226690483986,1.,1.96890351582545));
#43185=CARTESIAN_POINT('Ctrl Pts',(-0.760552825409855,1.,1.97516705321521));
#43186=CARTESIAN_POINT('Ctrl Pts',(-0.759837147452135,1.,1.98143741418156));
#43187=CARTESIAN_POINT('Ctrl Pts',(-0.759080037802243,1.,1.98771456680806));
#43188=CARTESIAN_POINT('Ctrl Pts',(-0.758281796766377,1.,1.9939983109871));
#43189=CARTESIAN_POINT('Ctrl Pts',(-0.757442676862341,1.,2.00028834739072));
#43190=CARTESIAN_POINT('Ctrl Pts',(-0.756562904646496,1.,2.00658431587682));
#43191=CARTESIAN_POINT('Ctrl Pts',(-0.7556427049581,1.,2.01288584328149));
#43192=CARTESIAN_POINT('Ctrl Pts',(-0.75468233072352,1.,2.01919259406003));
#43193=CARTESIAN_POINT('Ctrl Pts',(-0.753682061113766,1.,2.02550428623587));
#43194=CARTESIAN_POINT('Ctrl Pts',(-0.752642180488104,1.,2.03182068456467));
#43195=CARTESIAN_POINT('Ctrl Pts',(-0.751562963361384,1.,2.03814160092173));
#43196=CARTESIAN_POINT('Ctrl Pts',(-0.750444657874758,1.,2.04446689147754));
#43197=CARTESIAN_POINT('Ctrl Pts',(-0.749287468663053,1.,2.05079645591606));
#43198=CARTESIAN_POINT('Ctrl Pts',(-0.748091554181101,1.,2.05713023030263));
#43199=CARTESIAN_POINT('Ctrl Pts',(-0.747103932785504,1.,2.06220058927162));
#43200=CARTESIAN_POINT('Ctrl Pts',(-0.746345871542696,1.,2.06600523016401));
#43201=CARTESIAN_POINT('Ctrl Pts',(-0.74583279137781,1.,2.06854248895575));
#43202=CARTESIAN_POINT('Ctrl Pts',(-0.745574324794401,1.,2.0698113262342));
#43203=CARTESIAN_POINT('',(-0.693717979106306,0.,1.60662857109684));
#43204=CARTESIAN_POINT('Origin',(0.,0.,0.));
#43205=CARTESIAN_POINT('',(-0.892032620296855,1.,1.5055822144029));
#43206=CARTESIAN_POINT('Origin',(0.,1.,0.));
#43207=CARTESIAN_POINT('',(-0.892032620296855,0.,1.5055822144029));
#43208=CARTESIAN_POINT('Ctrl Pts',(-1.23627494547115,-1.,1.81978687191668));
#43209=CARTESIAN_POINT('Ctrl Pts',(-1.23627494547115,1.,1.81978687191668));
#43210=CARTESIAN_POINT('Ctrl Pts',(-1.23509651170476,-1.,1.81925017193666));
#43211=CARTESIAN_POINT('Ctrl Pts',(-1.23509651170476,1.,1.81925017193666));
#43212=CARTESIAN_POINT('Ctrl Pts',(-1.2327422452705,-1.,1.81817389921279));
#43213=CARTESIAN_POINT('Ctrl Pts',(-1.2327422452705,1.,1.81817389921279));
#43214=CARTESIAN_POINT('Ctrl Pts',(-1.2292186489137,-1.,1.8165508718364));
#43215=CARTESIAN_POINT('Ctrl Pts',(-1.2292186489137,1.,1.8165508718364));
#43216=CARTESIAN_POINT('Ctrl Pts',(-1.2245361330495,-1.,1.81436959210434));
#43217=CARTESIAN_POINT('Ctrl Pts',(-1.2245361330495,1.,1.81436959210434));
#43218=CARTESIAN_POINT('Ctrl Pts',(-1.21870906103557,-1.,1.81161420806656));
#43219=CARTESIAN_POINT('Ctrl Pts',(-1.21870906103557,1.,1.81161420806656));
#43220=CARTESIAN_POINT('Ctrl Pts',(-1.21290815708314,-1.,1.80882996917129));
#43221=CARTESIAN_POINT('Ctrl Pts',(-1.21290815708314,1.,1.80882996917129));
#43222=CARTESIAN_POINT('Ctrl Pts',(-1.20713356605475,-1.,1.80601678480707));
#43223=CARTESIAN_POINT('Ctrl Pts',(-1.20713356605475,1.,1.80601678480707));
#43224=CARTESIAN_POINT('Ctrl Pts',(-1.20138548938974,-1.,1.80317454838603));
#43225=CARTESIAN_POINT('Ctrl Pts',(-1.20138548938974,1.,1.80317454838603));
#43226=CARTESIAN_POINT('Ctrl Pts',(-1.19566418930242,-1.,1.80030314369879));
#43227=CARTESIAN_POINT('Ctrl Pts',(-1.19566418930242,1.,1.80030314369879));
#43228=CARTESIAN_POINT('Ctrl Pts',(-1.18996997934445,-1.,1.79740245923478));
#43229=CARTESIAN_POINT('Ctrl Pts',(-1.18996997934445,1.,1.79740245923478));
#43230=CARTESIAN_POINT('Ctrl Pts',(-1.18430321697432,-1.,1.79447240321515));
#43231=CARTESIAN_POINT('Ctrl Pts',(-1.18430321697432,1.,1.79447240321515));
#43232=CARTESIAN_POINT('Ctrl Pts',(-1.17866429440809,-1.,1.79151291552689));
#43233=CARTESIAN_POINT('Ctrl Pts',(-1.17866429440809,1.,1.79151291552689));
#43234=CARTESIAN_POINT('Ctrl Pts',(-1.17305363177328,-1.,1.78852398877616));
#43235=CARTESIAN_POINT('Ctrl Pts',(-1.17305363177328,1.,1.78852398877616));
#43236=CARTESIAN_POINT('Ctrl Pts',(-1.16747166312303,-1.,1.78550566040443));
#43237=CARTESIAN_POINT('Ctrl Pts',(-1.16747166312303,1.,1.78550566040443));
#43238=CARTESIAN_POINT('Ctrl Pts',(-1.16191881298499,-1.,1.78245795881009));
#43239=CARTESIAN_POINT('Ctrl Pts',(-1.16191881298499,1.,1.78245795881009));
#43240=CARTESIAN_POINT('Ctrl Pts',(-1.15639547194698,-1.,1.77938085564275));
#43241=CARTESIAN_POINT('Ctrl Pts',(-1.15639547194698,1.,1.77938085564275));
#43242=CARTESIAN_POINT('Ctrl Pts',(-1.15090197841515,-1.,1.7762742255701));
#43243=CARTESIAN_POINT('Ctrl Pts',(-1.15090197841515,1.,1.7762742255701));
#43244=CARTESIAN_POINT('Ctrl Pts',(-1.1454385822692,-1.,1.77313777896194));
#43245=CARTESIAN_POINT('Ctrl Pts',(-1.1454385822692,1.,1.77313777896194));
#43246=CARTESIAN_POINT('Ctrl Pts',(-1.14000548336975,-1.,1.76997111386769));
#43247=CARTESIAN_POINT('Ctrl Pts',(-1.14000548336975,1.,1.76997111386769));
#43248=CARTESIAN_POINT('Ctrl Pts',(-1.1346029180462,-1.,1.76677384551862));
#43249=CARTESIAN_POINT('Ctrl Pts',(-1.1346029180462,1.,1.76677384551862));
#43250=CARTESIAN_POINT('Ctrl Pts',(-1.12923123555075,-1.,1.7635457196617));
#43251=CARTESIAN_POINT('Ctrl Pts',(-1.12923123555075,1.,1.7635457196617));
#43252=CARTESIAN_POINT('Ctrl Pts',(-1.12389096855086,-1.,1.76028671825096));
#43253=CARTESIAN_POINT('Ctrl Pts',(-1.12389096855086,1.,1.76028671825096));
#43254=CARTESIAN_POINT('Ctrl Pts',(-1.11858293216763,-1.,1.75699720772105));
#43255=CARTESIAN_POINT('Ctrl Pts',(-1.11858293216763,1.,1.75699720772105));
#43256=CARTESIAN_POINT('Ctrl Pts',(-1.11330807582551,-1.,1.7536777209463));
#43257=CARTESIAN_POINT('Ctrl Pts',(-1.11330807582551,1.,1.7536777209463));
#43258=CARTESIAN_POINT('Ctrl Pts',(-1.10806728183007,-1.,1.7503286607592));
#43259=CARTESIAN_POINT('Ctrl Pts',(-1.10806728183007,1.,1.7503286607592));
#43260=CARTESIAN_POINT('Ctrl Pts',(-1.10286118991143,-1.,1.74695004214923));
#43261=CARTESIAN_POINT('Ctrl Pts',(-1.10286118991143,1.,1.74695004214923));
#43262=CARTESIAN_POINT('Ctrl Pts',(-1.09768999241225,-1.,1.74354119236208));
#43263=CARTESIAN_POINT('Ctrl Pts',(-1.09768999241225,1.,1.74354119236208));
#43264=CARTESIAN_POINT('Ctrl Pts',(-1.09255329056493,-1.,1.74010053962247));
#43265=CARTESIAN_POINT('Ctrl Pts',(-1.09255329056493,1.,1.74010053962247));
#43266=CARTESIAN_POINT('Ctrl Pts',(-1.08745056285427,-1.,1.73662628326091));
#43267=CARTESIAN_POINT('Ctrl Pts',(-1.08745056285427,1.,1.73662628326091));
#43268=CARTESIAN_POINT('Ctrl Pts',(-1.08238162784749,-1.,1.73311705663407));
#43269=CARTESIAN_POINT('Ctrl Pts',(-1.08238162784749,1.,1.73311705663407));
#43270=CARTESIAN_POINT('Ctrl Pts',(-1.0773470373727,-1.,1.72957248977424));
#43271=CARTESIAN_POINT('Ctrl Pts',(-1.0773470373727,1.,1.72957248977424));
#43272=CARTESIAN_POINT('Ctrl Pts',(-1.07234866990252,-1.,1.72599406198488));
#43273=CARTESIAN_POINT('Ctrl Pts',(-1.07234866990252,1.,1.72599406198488));
#43274=CARTESIAN_POINT('Ctrl Pts',(-1.06738966975462,-1.,1.72238500928453));
#43275=CARTESIAN_POINT('Ctrl Pts',(-1.06738966975462,1.,1.72238500928453));
#43276=CARTESIAN_POINT('Ctrl Pts',(-1.06247324680647,-1.,1.71874858456904));
#43277=CARTESIAN_POINT('Ctrl Pts',(-1.06247324680647,1.,1.71874858456904));
#43278=CARTESIAN_POINT('Ctrl Pts',(-1.05760163192479,-1.,1.7150865442702));
#43279=CARTESIAN_POINT('Ctrl Pts',(-1.05760163192479,1.,1.7150865442702));
#43280=CARTESIAN_POINT('Ctrl Pts',(-1.05277517202855,-1.,1.71139783543989));
#43281=CARTESIAN_POINT('Ctrl Pts',(-1.05277517202855,1.,1.71139783543989));
#43282=CARTESIAN_POINT('Ctrl Pts',(-1.04799085404995,-1.,1.70767646263649));
#43283=CARTESIAN_POINT('Ctrl Pts',(-1.04799085404995,1.,1.70767646263649));
#43284=CARTESIAN_POINT('Ctrl Pts',(-1.04324363334554,-1.,1.70391338707982));
#43285=CARTESIAN_POINT('Ctrl Pts',(-1.04324363334554,1.,1.70391338707982));
#43286=CARTESIAN_POINT('Ctrl Pts',(-1.03852922490789,-1.,1.70010052930962));
#43287=CARTESIAN_POINT('Ctrl Pts',(-1.03852922490789,1.,1.70010052930962));
#43288=CARTESIAN_POINT('Ctrl Pts',(-1.03384646003588,-1.,1.69623414782771));
#43289=CARTESIAN_POINT('Ctrl Pts',(-1.03384646003588,1.,1.69623414782771));
#43290=CARTESIAN_POINT('Ctrl Pts',(-1.02919977579147,-1.,1.69231840863458));
#43291=CARTESIAN_POINT('Ctrl Pts',(-1.02919977579147,1.,1.69231840863458));
#43292=CARTESIAN_POINT('Ctrl Pts',(-1.02460180535255,-1.,1.68836910178447));
#43293=CARTESIAN_POINT('Ctrl Pts',(-1.02460180535255,1.,1.68836910178447));
#43294=CARTESIAN_POINT('Ctrl Pts',(-1.02006795074201,-1.,1.68440578021706));
#43295=CARTESIAN_POINT('Ctrl Pts',(-1.02006795074201,1.,1.68440578021706));
#43296=CARTESIAN_POINT('Ctrl Pts',(-1.01561026162773,-1.,1.68044289894798));
#43297=CARTESIAN_POINT('Ctrl Pts',(-1.01561026162773,1.,1.68044289894798));
#43298=CARTESIAN_POINT('Ctrl Pts',(-1.01123236493511,-1.,1.67648246776464));
#43299=CARTESIAN_POINT('Ctrl Pts',(-1.01123236493511,1.,1.67648246776464));
#43300=CARTESIAN_POINT('Ctrl Pts',(-1.00692206696414,-1.,1.67250335383293));
#43301=CARTESIAN_POINT('Ctrl Pts',(-1.00692206696414,1.,1.67250335383293));
#43302=CARTESIAN_POINT('Ctrl Pts',(-1.00265091003727,-1.,1.66846059277303));
#43303=CARTESIAN_POINT('Ctrl Pts',(-1.00265091003727,1.,1.66846059277303));
#43304=CARTESIAN_POINT('Ctrl Pts',(-0.998389654952758,-1.,1.66430758030376));
#43305=CARTESIAN_POINT('Ctrl Pts',(-0.998389654952758,1.,1.66430758030376));
#43306=CARTESIAN_POINT('Ctrl Pts',(-0.994121836661306,-1.,1.66001553809947));
#43307=CARTESIAN_POINT('Ctrl Pts',(-0.994121836661306,1.,1.66001553809947));
#43308=CARTESIAN_POINT('Ctrl Pts',(-0.989855627854165,-1.,1.65559044289699));
#43309=CARTESIAN_POINT('Ctrl Pts',(-0.989855627854165,1.,1.65559044289699));
#43310=CARTESIAN_POINT('Ctrl Pts',(-0.985642622920821,-1.,1.65110016612638));
#43311=CARTESIAN_POINT('Ctrl Pts',(-0.985642622920821,1.,1.65110016612638));
#43312=CARTESIAN_POINT('Ctrl Pts',(-0.981562530939489,-1.,1.64665139190656));
#43313=CARTESIAN_POINT('Ctrl Pts',(-0.981562530939489,1.,1.64665139190656));
#43314=CARTESIAN_POINT('Ctrl Pts',(-0.977689794119416,-1.,1.64233990826687));
#43315=CARTESIAN_POINT('Ctrl Pts',(-0.977689794119416,1.,1.64233990826687));
#43316=CARTESIAN_POINT('Ctrl Pts',(-0.974066058287418,-1.,1.63820952658144));
#43317=CARTESIAN_POINT('Ctrl Pts',(-0.974066058287418,1.,1.63820952658144));
#43318=CARTESIAN_POINT('Ctrl Pts',(-0.970669715997509,-1.,1.63420665729798));
#43319=CARTESIAN_POINT('Ctrl Pts',(-0.970669715997509,1.,1.63420665729798));
#43320=CARTESIAN_POINT('Ctrl Pts',(-0.967387853230345,-1.,1.63013849959461));
#43321=CARTESIAN_POINT('Ctrl Pts',(-0.967387853230345,1.,1.63013849959461));
#43322=CARTESIAN_POINT('Ctrl Pts',(-0.964046107040536,-1.,1.62571930670187));
#43323=CARTESIAN_POINT('Ctrl Pts',(-0.964046107040536,1.,1.62571930670187));
#43324=CARTESIAN_POINT('Ctrl Pts',(-0.960438326101729,-1.,1.62061638140221));
#43325=CARTESIAN_POINT('Ctrl Pts',(-0.960438326101729,1.,1.62061638140221));
#43326=CARTESIAN_POINT('Ctrl Pts',(-0.956354422920671,-1.,1.61449324337085));
#43327=CARTESIAN_POINT('Ctrl Pts',(-0.956354422920671,1.,1.61449324337085));
#43328=CARTESIAN_POINT('Ctrl Pts',(-0.951613284356035,-1.,1.60706069896936));
#43329=CARTESIAN_POINT('Ctrl Pts',(-0.951613284356035,1.,1.60706069896936));
#43330=CARTESIAN_POINT('Ctrl Pts',(-0.946078063315257,-1.,1.59810042043673));
#43331=CARTESIAN_POINT('Ctrl Pts',(-0.946078063315257,1.,1.59810042043673));
#43332=CARTESIAN_POINT('Ctrl Pts',(-0.939646377893399,-1.,1.58744937487176));
#43333=CARTESIAN_POINT('Ctrl Pts',(-0.939646377893399,1.,1.58744937487176));
#43334=CARTESIAN_POINT('Ctrl Pts',(-0.932246680108685,-1.,1.57499388382243));
#43335=CARTESIAN_POINT('Ctrl Pts',(-0.932246680108685,1.,1.57499388382243));
#43336=CARTESIAN_POINT('Ctrl Pts',(-0.923832188944341,-1.,1.56065988578893));
#43337=CARTESIAN_POINT('Ctrl Pts',(-0.923832188944341,1.,1.56065988578893));
#43338=CARTESIAN_POINT('Ctrl Pts',(-0.914375919026456,-1.,1.54440491149498));
#43339=CARTESIAN_POINT('Ctrl Pts',(-0.914375919026456,1.,1.54440491149498));
#43340=CARTESIAN_POINT('Ctrl Pts',(-0.905967409625651,-1.,1.52984849887993));
#43341=CARTESIAN_POINT('Ctrl Pts',(-0.905967409625651,1.,1.52984849887993));
#43342=CARTESIAN_POINT('Ctrl Pts',(-0.899185047483511,-1.,1.51805569590094));
#43343=CARTESIAN_POINT('Ctrl Pts',(-0.899185047483511,1.,1.51805569590094));
#43344=CARTESIAN_POINT('Ctrl Pts',(-0.894452006964543,-1.,1.50980486806688));
#43345=CARTESIAN_POINT('Ctrl Pts',(-0.894452006964543,1.,1.50980486806688));
#43346=CARTESIAN_POINT('Ctrl Pts',(-0.892032620296855,-1.,1.5055822144029));
#43347=CARTESIAN_POINT('Ctrl Pts',(-0.892032620296855,1.,1.5055822144029));
#43348=CARTESIAN_POINT('',(-1.23627494547115,1.,1.81978687191668));
#43349=CARTESIAN_POINT('Ctrl Pts',(-1.23627494547115,1.,1.81978687191668));
#43350=CARTESIAN_POINT('Ctrl Pts',(-1.23509651170476,1.,1.81925017193666));
#43351=CARTESIAN_POINT('Ctrl Pts',(-1.2327422452705,1.,1.81817389921279));
#43352=CARTESIAN_POINT('Ctrl Pts',(-1.2292186489137,1.,1.8165508718364));
#43353=CARTESIAN_POINT('Ctrl Pts',(-1.2245361330495,1.,1.81436959210434));
#43354=CARTESIAN_POINT('Ctrl Pts',(-1.21870906103557,1.,1.81161420806656));
#43355=CARTESIAN_POINT('Ctrl Pts',(-1.21290815708314,1.,1.80882996917129));
#43356=CARTESIAN_POINT('Ctrl Pts',(-1.20713356605475,1.,1.80601678480707));
#43357=CARTESIAN_POINT('Ctrl Pts',(-1.20138548938974,1.,1.80317454838603));
#43358=CARTESIAN_POINT('Ctrl Pts',(-1.19566418930242,1.,1.80030314369879));
#43359=CARTESIAN_POINT('Ctrl Pts',(-1.18996997934445,1.,1.79740245923478));
#43360=CARTESIAN_POINT('Ctrl Pts',(-1.18430321697432,1.,1.79447240321515));
#43361=CARTESIAN_POINT('Ctrl Pts',(-1.17866429440809,1.,1.79151291552689));
#43362=CARTESIAN_POINT('Ctrl Pts',(-1.17305363177328,1.,1.78852398877616));
#43363=CARTESIAN_POINT('Ctrl Pts',(-1.16747166312303,1.,1.78550566040443));
#43364=CARTESIAN_POINT('Ctrl Pts',(-1.16191881298499,1.,1.78245795881009));
#43365=CARTESIAN_POINT('Ctrl Pts',(-1.15639547194698,1.,1.77938085564275));
#43366=CARTESIAN_POINT('Ctrl Pts',(-1.15090197841515,1.,1.7762742255701));
#43367=CARTESIAN_POINT('Ctrl Pts',(-1.1454385822692,1.,1.77313777896194));
#43368=CARTESIAN_POINT('Ctrl Pts',(-1.14000548336975,1.,1.76997111386769));
#43369=CARTESIAN_POINT('Ctrl Pts',(-1.1346029180462,1.,1.76677384551862));
#43370=CARTESIAN_POINT('Ctrl Pts',(-1.12923123555075,1.,1.7635457196617));
#43371=CARTESIAN_POINT('Ctrl Pts',(-1.12389096855086,1.,1.76028671825096));
#43372=CARTESIAN_POINT('Ctrl Pts',(-1.11858293216763,1.,1.75699720772105));
#43373=CARTESIAN_POINT('Ctrl Pts',(-1.11330807582551,1.,1.7536777209463));
#43374=CARTESIAN_POINT('Ctrl Pts',(-1.10806728183007,1.,1.7503286607592));
#43375=CARTESIAN_POINT('Ctrl Pts',(-1.10286118991143,1.,1.74695004214923));
#43376=CARTESIAN_POINT('Ctrl Pts',(-1.09768999241225,1.,1.74354119236208));
#43377=CARTESIAN_POINT('Ctrl Pts',(-1.09255329056493,1.,1.74010053962247));
#43378=CARTESIAN_POINT('Ctrl Pts',(-1.08745056285427,1.,1.73662628326091));
#43379=CARTESIAN_POINT('Ctrl Pts',(-1.08238162784749,1.,1.73311705663407));
#43380=CARTESIAN_POINT('Ctrl Pts',(-1.0773470373727,1.,1.72957248977424));
#43381=CARTESIAN_POINT('Ctrl Pts',(-1.07234866990252,1.,1.72599406198488));
#43382=CARTESIAN_POINT('Ctrl Pts',(-1.06738966975462,1.,1.72238500928453));
#43383=CARTESIAN_POINT('Ctrl Pts',(-1.06247324680647,1.,1.71874858456904));
#43384=CARTESIAN_POINT('Ctrl Pts',(-1.05760163192479,1.,1.7150865442702));
#43385=CARTESIAN_POINT('Ctrl Pts',(-1.05277517202855,1.,1.71139783543989));
#43386=CARTESIAN_POINT('Ctrl Pts',(-1.04799085404995,1.,1.70767646263649));
#43387=CARTESIAN_POINT('Ctrl Pts',(-1.04324363334554,1.,1.70391338707982));
#43388=CARTESIAN_POINT('Ctrl Pts',(-1.03852922490789,1.,1.70010052930962));
#43389=CARTESIAN_POINT('Ctrl Pts',(-1.03384646003588,1.,1.69623414782771));
#43390=CARTESIAN_POINT('Ctrl Pts',(-1.02919977579147,1.,1.69231840863458));
#43391=CARTESIAN_POINT('Ctrl Pts',(-1.02460180535255,1.,1.68836910178447));
#43392=CARTESIAN_POINT('Ctrl Pts',(-1.02006795074201,1.,1.68440578021706));
#43393=CARTESIAN_POINT('Ctrl Pts',(-1.01561026162773,1.,1.68044289894798));
#43394=CARTESIAN_POINT('Ctrl Pts',(-1.01123236493511,1.,1.67648246776464));
#43395=CARTESIAN_POINT('Ctrl Pts',(-1.00692206696414,1.,1.67250335383293));
#43396=CARTESIAN_POINT('Ctrl Pts',(-1.00265091003727,1.,1.66846059277303));
#43397=CARTESIAN_POINT('Ctrl Pts',(-0.998389654952758,1.,1.66430758030376));
#43398=CARTESIAN_POINT('Ctrl Pts',(-0.994121836661306,1.,1.66001553809947));
#43399=CARTESIAN_POINT('Ctrl Pts',(-0.989855627854165,1.,1.65559044289699));
#43400=CARTESIAN_POINT('Ctrl Pts',(-0.985642622920821,1.,1.65110016612638));
#43401=CARTESIAN_POINT('Ctrl Pts',(-0.981562530939489,1.,1.64665139190656));
#43402=CARTESIAN_POINT('Ctrl Pts',(-0.977689794119416,1.,1.64233990826687));
#43403=CARTESIAN_POINT('Ctrl Pts',(-0.974066058287418,1.,1.63820952658144));
#43404=CARTESIAN_POINT('Ctrl Pts',(-0.970669715997509,1.,1.63420665729798));
#43405=CARTESIAN_POINT('Ctrl Pts',(-0.967387853230345,1.,1.63013849959461));
#43406=CARTESIAN_POINT('Ctrl Pts',(-0.964046107040536,1.,1.62571930670187));
#43407=CARTESIAN_POINT('Ctrl Pts',(-0.960438326101729,1.,1.62061638140221));
#43408=CARTESIAN_POINT('Ctrl Pts',(-0.956354422920671,1.,1.61449324337085));
#43409=CARTESIAN_POINT('Ctrl Pts',(-0.951613284356035,1.,1.60706069896936));
#43410=CARTESIAN_POINT('Ctrl Pts',(-0.946078063315257,1.,1.59810042043673));
#43411=CARTESIAN_POINT('Ctrl Pts',(-0.939646377893399,1.,1.58744937487176));
#43412=CARTESIAN_POINT('Ctrl Pts',(-0.932246680108685,1.,1.57499388382243));
#43413=CARTESIAN_POINT('Ctrl Pts',(-0.923832188944341,1.,1.56065988578893));
#43414=CARTESIAN_POINT('Ctrl Pts',(-0.914375919026456,1.,1.54440491149498));
#43415=CARTESIAN_POINT('Ctrl Pts',(-0.905967409625651,1.,1.52984849887993));
#43416=CARTESIAN_POINT('Ctrl Pts',(-0.899185047483511,1.,1.51805569590094));
#43417=CARTESIAN_POINT('Ctrl Pts',(-0.894452006964543,1.,1.50980486806688));
#43418=CARTESIAN_POINT('Ctrl Pts',(-0.892032620296855,1.,1.5055822144029));
#43419=CARTESIAN_POINT('',(-1.23627494547115,0.,1.81978687191668));
#43420=CARTESIAN_POINT('Origin',(-1.34869019493419,0.,1.73811241238545));
#43421=CARTESIAN_POINT('',(-1.34869019493419,1.,1.73811241238545));
#43422=CARTESIAN_POINT('',(-1.23627494547115,1.,1.81978687191668));
#43423=CARTESIAN_POINT('',(-1.34869019493419,0.,1.73811241238545));
#43424=CARTESIAN_POINT('Ctrl Pts',(-1.15624053661742,-1.,1.31362392696032));
#43425=CARTESIAN_POINT('Ctrl Pts',(-1.15624053661742,1.,1.31362392696032));
#43426=CARTESIAN_POINT('Ctrl Pts',(-1.15950888730809,-1.,1.31722977216397));
#43427=CARTESIAN_POINT('Ctrl Pts',(-1.15950888730809,1.,1.31722977216397));
#43428=CARTESIAN_POINT('Ctrl Pts',(-1.16589330093588,-1.,1.32428080721772));
#43429=CARTESIAN_POINT('Ctrl Pts',(-1.16589330093588,1.,1.32428080721772));
#43430=CARTESIAN_POINT('Ctrl Pts',(-1.17501305789857,-1.,1.33437539347008));
#43431=CARTESIAN_POINT('Ctrl Pts',(-1.17501305789857,1.,1.33437539347008));
#43432=CARTESIAN_POINT('Ctrl Pts',(-1.18625865667441,-1.,1.34687054001093));
#43433=CARTESIAN_POINT('Ctrl Pts',(-1.18625865667441,1.,1.34687054001093));
#43434=CARTESIAN_POINT('Ctrl Pts',(-1.1987959077932,-1.,1.36088705043885));
#43435=CARTESIAN_POINT('Ctrl Pts',(-1.1987959077932,1.,1.36088705043885));
#43436=CARTESIAN_POINT('Ctrl Pts',(-1.20982812925645,-1.,1.37331915607905));
#43437=CARTESIAN_POINT('Ctrl Pts',(-1.20982812925645,1.,1.37331915607905));
#43438=CARTESIAN_POINT('Ctrl Pts',(-1.21938737280852,-1.,1.38420564527715));
#43439=CARTESIAN_POINT('Ctrl Pts',(-1.21938737280852,1.,1.38420564527715));
#43440=CARTESIAN_POINT('Ctrl Pts',(-1.22752961899387,-1.,1.39361389568796));
#43441=CARTESIAN_POINT('Ctrl Pts',(-1.22752961899387,1.,1.39361389568796));
#43442=CARTESIAN_POINT('Ctrl Pts',(-1.23434087290423,-1.,1.40164708206106));
#43443=CARTESIAN_POINT('Ctrl Pts',(-1.23434087290423,1.,1.40164708206106));
#43444=CARTESIAN_POINT('Ctrl Pts',(-1.23994455029534,-1.,1.40845295531283));
#43445=CARTESIAN_POINT('Ctrl Pts',(-1.23994455029534,1.,1.40845295531283));
#43446=CARTESIAN_POINT('Ctrl Pts',(-1.24450600513056,-1.,1.41422913175179));
#43447=CARTESIAN_POINT('Ctrl Pts',(-1.24450600513056,1.,1.41422913175179));
#43448=CARTESIAN_POINT('Ctrl Pts',(-1.24824430986571,-1.,1.41923722596025));
#43449=CARTESIAN_POINT('Ctrl Pts',(-1.24824430986571,1.,1.41923722596025));
#43450=CARTESIAN_POINT('Ctrl Pts',(-1.2514145557001,-1.,1.42378102115575));
#43451=CARTESIAN_POINT('Ctrl Pts',(-1.2514145557001,1.,1.42378102115575));
#43452=CARTESIAN_POINT('Ctrl Pts',(-1.25426945222639,-1.,1.42815938799387));
#43453=CARTESIAN_POINT('Ctrl Pts',(-1.25426945222639,1.,1.42815938799387));
#43454=CARTESIAN_POINT('Ctrl Pts',(-1.25702687965755,-1.,1.43262645609691));
#43455=CARTESIAN_POINT('Ctrl Pts',(-1.25702687965755,1.,1.43262645609691));
#43456=CARTESIAN_POINT('Ctrl Pts',(-1.25983531012005,-1.,1.43734919180848));
#43457=CARTESIAN_POINT('Ctrl Pts',(-1.25983531012005,1.,1.43734919180848));
#43458=CARTESIAN_POINT('Ctrl Pts',(-1.26273903323859,-1.,1.44236470511303));
#43459=CARTESIAN_POINT('Ctrl Pts',(-1.26273903323859,1.,1.44236470511303));
#43460=CARTESIAN_POINT('Ctrl Pts',(-1.26570925118868,-1.,1.44761985001662));
#43461=CARTESIAN_POINT('Ctrl Pts',(-1.26570925118868,1.,1.44761985001662));
#43462=CARTESIAN_POINT('Ctrl Pts',(-1.2686778680489,-1.,1.45301422764247));
#43463=CARTESIAN_POINT('Ctrl Pts',(-1.2686778680489,1.,1.45301422764247));
#43464=CARTESIAN_POINT('Ctrl Pts',(-1.27156805265289,-1.,1.45843906294697));
#43465=CARTESIAN_POINT('Ctrl Pts',(-1.27156805265289,1.,1.45843906294697));
#43466=CARTESIAN_POINT('Ctrl Pts',(-1.27433119897822,-1.,1.46382431332476));
#43467=CARTESIAN_POINT('Ctrl Pts',(-1.27433119897822,1.,1.46382431332476));
#43468=CARTESIAN_POINT('Ctrl Pts',(-1.27696414831089,-1.,1.46916035917133));
#43469=CARTESIAN_POINT('Ctrl Pts',(-1.27696414831089,1.,1.46916035917133));
#43470=CARTESIAN_POINT('Ctrl Pts',(-1.2794891824849,-1.,1.4744717526707));
#43471=CARTESIAN_POINT('Ctrl Pts',(-1.2794891824849,1.,1.4744717526707));
#43472=CARTESIAN_POINT('Ctrl Pts',(-1.28194158939517,-1.,1.47980070347095));
#43473=CARTESIAN_POINT('Ctrl Pts',(-1.28194158939517,1.,1.47980070347095));
#43474=CARTESIAN_POINT('Ctrl Pts',(-1.28435533880201,-1.,1.4851881711891));
#43475=CARTESIAN_POINT('Ctrl Pts',(-1.28435533880201,1.,1.4851881711891));
#43476=CARTESIAN_POINT('Ctrl Pts',(-1.2867467611644,-1.,1.4906522831278));
#43477=CARTESIAN_POINT('Ctrl Pts',(-1.2867467611644,1.,1.4906522831278));
#43478=CARTESIAN_POINT('Ctrl Pts',(-1.28911506584254,-1.,1.49618896881754));
#43479=CARTESIAN_POINT('Ctrl Pts',(-1.28911506584254,1.,1.49618896881754));
#43480=CARTESIAN_POINT('Ctrl Pts',(-1.29145022885181,-1.,1.50178230149776));
#43481=CARTESIAN_POINT('Ctrl Pts',(-1.29145022885181,1.,1.50178230149776));
#43482=CARTESIAN_POINT('Ctrl Pts',(-1.29373841372842,-1.,1.50741159078365));
#43483=CARTESIAN_POINT('Ctrl Pts',(-1.29373841372842,1.,1.50741159078365));
#43484=CARTESIAN_POINT('Ctrl Pts',(-1.29596850710509,-1.,1.51305994241402));
#43485=CARTESIAN_POINT('Ctrl Pts',(-1.29596850710509,1.,1.51305994241402));
#43486=CARTESIAN_POINT('Ctrl Pts',(-1.29813791800747,-1.,1.51872184912724));
#43487=CARTESIAN_POINT('Ctrl Pts',(-1.29813791800747,1.,1.51872184912724));
#43488=CARTESIAN_POINT('Ctrl Pts',(-1.30024984366328,-1.,1.52439957861062));
#43489=CARTESIAN_POINT('Ctrl Pts',(-1.30024984366328,1.,1.52439957861062));
#43490=CARTESIAN_POINT('Ctrl Pts',(-1.30231064395568,-1.,1.53009970283891));
#43491=CARTESIAN_POINT('Ctrl Pts',(-1.30231064395568,1.,1.53009970283891));
#43492=CARTESIAN_POINT('Ctrl Pts',(-1.30432735639489,-1.,1.53582981268977));
#43493=CARTESIAN_POINT('Ctrl Pts',(-1.30432735639489,1.,1.53582981268977));
#43494=CARTESIAN_POINT('Ctrl Pts',(-1.30630475189556,-1.,1.54159462645432));
#43495=CARTESIAN_POINT('Ctrl Pts',(-1.30630475189556,1.,1.54159462645432));
#43496=CARTESIAN_POINT('Ctrl Pts',(-1.30824393907473,-1.,1.54739413957185));
#43497=CARTESIAN_POINT('Ctrl Pts',(-1.30824393907473,1.,1.54739413957185));
#43498=CARTESIAN_POINT('Ctrl Pts',(-1.31014393684222,-1.,1.55322568759481));
#43499=CARTESIAN_POINT('Ctrl Pts',(-1.31014393684222,1.,1.55322568759481));
#43500=CARTESIAN_POINT('Ctrl Pts',(-1.31200264341696,-1.,1.55908521254821));
#43501=CARTESIAN_POINT('Ctrl Pts',(-1.31200264341696,1.,1.55908521254821));
#43502=CARTESIAN_POINT('Ctrl Pts',(-1.31381795281002,-1.,1.56496872402353));
#43503=CARTESIAN_POINT('Ctrl Pts',(-1.31381795281002,1.,1.56496872402353));
#43504=CARTESIAN_POINT('Ctrl Pts',(-1.31558903860016,-1.,1.57087397835723));
#43505=CARTESIAN_POINT('Ctrl Pts',(-1.31558903860016,1.,1.57087397835723));
#43506=CARTESIAN_POINT('Ctrl Pts',(-1.31731642317187,-1.,1.5768005650559));
#43507=CARTESIAN_POINT('Ctrl Pts',(-1.31731642317187,1.,1.5768005650559));
#43508=CARTESIAN_POINT('Ctrl Pts',(-1.31900135021432,-1.,1.58274907898834));
#43509=CARTESIAN_POINT('Ctrl Pts',(-1.31900135021432,1.,1.58274907898834));
#43510=CARTESIAN_POINT('Ctrl Pts',(-1.32064537110892,-1.,1.58872057258245));
#43511=CARTESIAN_POINT('Ctrl Pts',(-1.32064537110892,1.,1.58872057258245));
#43512=CARTESIAN_POINT('Ctrl Pts',(-1.32224985747682,-1.,1.59471591079403));
#43513=CARTESIAN_POINT('Ctrl Pts',(-1.32224985747682,1.,1.59471591079403));
#43514=CARTESIAN_POINT('Ctrl Pts',(-1.32381550858256,-1.,1.60073511858687));
#43515=CARTESIAN_POINT('Ctrl Pts',(-1.32381550858256,1.,1.60073511858687));
#43516=CARTESIAN_POINT('Ctrl Pts',(-1.32534250785782,-1.,1.60677758290954));
#43517=CARTESIAN_POINT('Ctrl Pts',(-1.32534250785782,1.,1.60677758290954));
#43518=CARTESIAN_POINT('Ctrl Pts',(-1.32683074483356,-1.,1.6128423401575));
#43519=CARTESIAN_POINT('Ctrl Pts',(-1.32683074483356,1.,1.6128423401575));
#43520=CARTESIAN_POINT('Ctrl Pts',(-1.32828000610449,-1.,1.61892832270724));
#43521=CARTESIAN_POINT('Ctrl Pts',(-1.32828000610449,1.,1.61892832270724));
#43522=CARTESIAN_POINT('Ctrl Pts',(-1.3296901950568,-1.,1.62503464209797));
#43523=CARTESIAN_POINT('Ctrl Pts',(-1.3296901950568,1.,1.62503464209797));
#43524=CARTESIAN_POINT('Ctrl Pts',(-1.33106149345645,-1.,1.63116079730923));
#43525=CARTESIAN_POINT('Ctrl Pts',(-1.33106149345645,1.,1.63116079730923));
#43526=CARTESIAN_POINT('Ctrl Pts',(-1.33239425103724,-1.,1.63730653475089));
#43527=CARTESIAN_POINT('Ctrl Pts',(-1.33239425103724,1.,1.63730653475089));
#43528=CARTESIAN_POINT('Ctrl Pts',(-1.33368890676572,-1.,1.6434717485603));
#43529=CARTESIAN_POINT('Ctrl Pts',(-1.33368890676572,1.,1.6434717485603));
#43530=CARTESIAN_POINT('Ctrl Pts',(-1.33494590467993,-1.,1.6496563728683));
#43531=CARTESIAN_POINT('Ctrl Pts',(-1.33494590467993,1.,1.6496563728683));
#43532=CARTESIAN_POINT('Ctrl Pts',(-1.33616559745172,-1.,1.65586025952593));
#43533=CARTESIAN_POINT('Ctrl Pts',(-1.33616559745172,1.,1.65586025952593));
#43534=CARTESIAN_POINT('Ctrl Pts',(-1.33734820885262,-1.,1.66208312541983));
#43535=CARTESIAN_POINT('Ctrl Pts',(-1.33734820885262,1.,1.66208312541983));
#43536=CARTESIAN_POINT('Ctrl Pts',(-1.33849388654388,-1.,1.66832460783989));
#43537=CARTESIAN_POINT('Ctrl Pts',(-1.33849388654388,1.,1.66832460783989));
#43538=CARTESIAN_POINT('Ctrl Pts',(-1.3396027347034,-1.,1.67458429426086));
#43539=CARTESIAN_POINT('Ctrl Pts',(-1.3396027347034,1.,1.67458429426086));
#43540=CARTESIAN_POINT('Ctrl Pts',(-1.34067485185203,-1.,1.68086176030362));
#43541=CARTESIAN_POINT('Ctrl Pts',(-1.34067485185203,1.,1.68086176030362));
#43542=CARTESIAN_POINT('Ctrl Pts',(-1.341710374848,-1.,1.68715660868764));
#43543=CARTESIAN_POINT('Ctrl Pts',(-1.341710374848,1.,1.68715660868764));
#43544=CARTESIAN_POINT('Ctrl Pts',(-1.34270948206319,-1.,1.6934684849687));
#43545=CARTESIAN_POINT('Ctrl Pts',(-1.34270948206319,1.,1.6934684849687));
#43546=CARTESIAN_POINT('Ctrl Pts',(-1.34367237124483,-1.,1.69979707754427));
#43547=CARTESIAN_POINT('Ctrl Pts',(-1.34367237124483,1.,1.69979707754427));
#43548=CARTESIAN_POINT('Ctrl Pts',(-1.34459924533831,-1.,1.70614212266738));
#43549=CARTESIAN_POINT('Ctrl Pts',(-1.34459924533831,1.,1.70614212266738));
#43550=CARTESIAN_POINT('Ctrl Pts',(-1.34549029589416,-1.,1.71250340686822));
#43551=CARTESIAN_POINT('Ctrl Pts',(-1.34549029589416,1.,1.71250340686822));
#43552=CARTESIAN_POINT('Ctrl Pts',(-1.34634568653227,-1.,1.7188807715049));
#43553=CARTESIAN_POINT('Ctrl Pts',(-1.34634568653227,1.,1.7188807715049));
#43554=CARTESIAN_POINT('Ctrl Pts',(-1.34716554819527,-1.,1.72527410680674));
#43555=CARTESIAN_POINT('Ctrl Pts',(-1.34716554819527,1.,1.72527410680674));
#43556=CARTESIAN_POINT('Ctrl Pts',(-1.34779309152035,-1.,1.7304014965394));
#43557=CARTESIAN_POINT('Ctrl Pts',(-1.34779309152035,1.,1.7304014965394));
#43558=CARTESIAN_POINT('Ctrl Pts',(-1.34824783112887,-1.,1.73425417885907));
#43559=CARTESIAN_POINT('Ctrl Pts',(-1.34824783112887,1.,1.73425417885907));
#43560=CARTESIAN_POINT('Ctrl Pts',(-1.34854391898045,-1.,1.73682580585691));
#43561=CARTESIAN_POINT('Ctrl Pts',(-1.34854391898045,1.,1.73682580585691));
#43562=CARTESIAN_POINT('Ctrl Pts',(-1.34869019493419,-1.,1.73811241238545));
#43563=CARTESIAN_POINT('Ctrl Pts',(-1.34869019493419,1.,1.73811241238545));
#43564=CARTESIAN_POINT('',(-1.15624053661742,1.,1.31362392696032));
#43565=CARTESIAN_POINT('Ctrl Pts',(-1.15624053661742,1.,1.31362392696032));
#43566=CARTESIAN_POINT('Ctrl Pts',(-1.15950888730809,1.,1.31722977216397));
#43567=CARTESIAN_POINT('Ctrl Pts',(-1.16589330093588,1.,1.32428080721772));
#43568=CARTESIAN_POINT('Ctrl Pts',(-1.17501305789857,1.,1.33437539347008));
#43569=CARTESIAN_POINT('Ctrl Pts',(-1.18625865667441,1.,1.34687054001093));
#43570=CARTESIAN_POINT('Ctrl Pts',(-1.1987959077932,1.,1.36088705043885));
#43571=CARTESIAN_POINT('Ctrl Pts',(-1.20982812925645,1.,1.37331915607905));
#43572=CARTESIAN_POINT('Ctrl Pts',(-1.21938737280852,1.,1.38420564527715));
#43573=CARTESIAN_POINT('Ctrl Pts',(-1.22752961899387,1.,1.39361389568796));
#43574=CARTESIAN_POINT('Ctrl Pts',(-1.23434087290423,1.,1.40164708206106));
#43575=CARTESIAN_POINT('Ctrl Pts',(-1.23994455029534,1.,1.40845295531283));
#43576=CARTESIAN_POINT('Ctrl Pts',(-1.24450600513056,1.,1.41422913175179));
#43577=CARTESIAN_POINT('Ctrl Pts',(-1.24824430986571,1.,1.41923722596025));
#43578=CARTESIAN_POINT('Ctrl Pts',(-1.2514145557001,1.,1.42378102115575));
#43579=CARTESIAN_POINT('Ctrl Pts',(-1.25426945222639,1.,1.42815938799387));
#43580=CARTESIAN_POINT('Ctrl Pts',(-1.25702687965755,1.,1.43262645609691));
#43581=CARTESIAN_POINT('Ctrl Pts',(-1.25983531012005,1.,1.43734919180848));
#43582=CARTESIAN_POINT('Ctrl Pts',(-1.26273903323859,1.,1.44236470511303));
#43583=CARTESIAN_POINT('Ctrl Pts',(-1.26570925118868,1.,1.44761985001662));
#43584=CARTESIAN_POINT('Ctrl Pts',(-1.2686778680489,1.,1.45301422764247));
#43585=CARTESIAN_POINT('Ctrl Pts',(-1.27156805265289,1.,1.45843906294697));
#43586=CARTESIAN_POINT('Ctrl Pts',(-1.27433119897822,1.,1.46382431332476));
#43587=CARTESIAN_POINT('Ctrl Pts',(-1.27696414831089,1.,1.46916035917133));
#43588=CARTESIAN_POINT('Ctrl Pts',(-1.2794891824849,1.,1.4744717526707));
#43589=CARTESIAN_POINT('Ctrl Pts',(-1.28194158939517,1.,1.47980070347095));
#43590=CARTESIAN_POINT('Ctrl Pts',(-1.28435533880201,1.,1.4851881711891));
#43591=CARTESIAN_POINT('Ctrl Pts',(-1.2867467611644,1.,1.4906522831278));
#43592=CARTESIAN_POINT('Ctrl Pts',(-1.28911506584254,1.,1.49618896881754));
#43593=CARTESIAN_POINT('Ctrl Pts',(-1.29145022885181,1.,1.50178230149776));
#43594=CARTESIAN_POINT('Ctrl Pts',(-1.29373841372842,1.,1.50741159078365));
#43595=CARTESIAN_POINT('Ctrl Pts',(-1.29596850710509,1.,1.51305994241402));
#43596=CARTESIAN_POINT('Ctrl Pts',(-1.29813791800747,1.,1.51872184912724));
#43597=CARTESIAN_POINT('Ctrl Pts',(-1.30024984366328,1.,1.52439957861062));
#43598=CARTESIAN_POINT('Ctrl Pts',(-1.30231064395568,1.,1.53009970283891));
#43599=CARTESIAN_POINT('Ctrl Pts',(-1.30432735639489,1.,1.53582981268977));
#43600=CARTESIAN_POINT('Ctrl Pts',(-1.30630475189556,1.,1.54159462645432));
#43601=CARTESIAN_POINT('Ctrl Pts',(-1.30824393907473,1.,1.54739413957185));
#43602=CARTESIAN_POINT('Ctrl Pts',(-1.31014393684222,1.,1.55322568759481));
#43603=CARTESIAN_POINT('Ctrl Pts',(-1.31200264341696,1.,1.55908521254821));
#43604=CARTESIAN_POINT('Ctrl Pts',(-1.31381795281002,1.,1.56496872402353));
#43605=CARTESIAN_POINT('Ctrl Pts',(-1.31558903860016,1.,1.57087397835723));
#43606=CARTESIAN_POINT('Ctrl Pts',(-1.31731642317187,1.,1.5768005650559));
#43607=CARTESIAN_POINT('Ctrl Pts',(-1.31900135021432,1.,1.58274907898834));
#43608=CARTESIAN_POINT('Ctrl Pts',(-1.32064537110892,1.,1.58872057258245));
#43609=CARTESIAN_POINT('Ctrl Pts',(-1.32224985747682,1.,1.59471591079403));
#43610=CARTESIAN_POINT('Ctrl Pts',(-1.32381550858256,1.,1.60073511858687));
#43611=CARTESIAN_POINT('Ctrl Pts',(-1.32534250785782,1.,1.60677758290954));
#43612=CARTESIAN_POINT('Ctrl Pts',(-1.32683074483356,1.,1.6128423401575));
#43613=CARTESIAN_POINT('Ctrl Pts',(-1.32828000610449,1.,1.61892832270724));
#43614=CARTESIAN_POINT('Ctrl Pts',(-1.3296901950568,1.,1.62503464209797));
#43615=CARTESIAN_POINT('Ctrl Pts',(-1.33106149345645,1.,1.63116079730923));
#43616=CARTESIAN_POINT('Ctrl Pts',(-1.33239425103724,1.,1.63730653475089));
#43617=CARTESIAN_POINT('Ctrl Pts',(-1.33368890676572,1.,1.6434717485603));
#43618=CARTESIAN_POINT('Ctrl Pts',(-1.33494590467993,1.,1.6496563728683));
#43619=CARTESIAN_POINT('Ctrl Pts',(-1.33616559745172,1.,1.65586025952593));
#43620=CARTESIAN_POINT('Ctrl Pts',(-1.33734820885262,1.,1.66208312541983));
#43621=CARTESIAN_POINT('Ctrl Pts',(-1.33849388654388,1.,1.66832460783989));
#43622=CARTESIAN_POINT('Ctrl Pts',(-1.3396027347034,1.,1.67458429426086));
#43623=CARTESIAN_POINT('Ctrl Pts',(-1.34067485185203,1.,1.68086176030362));
#43624=CARTESIAN_POINT('Ctrl Pts',(-1.341710374848,1.,1.68715660868764));
#43625=CARTESIAN_POINT('Ctrl Pts',(-1.34270948206319,1.,1.6934684849687));
#43626=CARTESIAN_POINT('Ctrl Pts',(-1.34367237124483,1.,1.69979707754427));
#43627=CARTESIAN_POINT('Ctrl Pts',(-1.34459924533831,1.,1.70614212266738));
#43628=CARTESIAN_POINT('Ctrl Pts',(-1.34549029589416,1.,1.71250340686822));
#43629=CARTESIAN_POINT('Ctrl Pts',(-1.34634568653227,1.,1.7188807715049));
#43630=CARTESIAN_POINT('Ctrl Pts',(-1.34716554819527,1.,1.72527410680674));
#43631=CARTESIAN_POINT('Ctrl Pts',(-1.34779309152035,1.,1.7304014965394));
#43632=CARTESIAN_POINT('Ctrl Pts',(-1.34824783112887,1.,1.73425417885907));
#43633=CARTESIAN_POINT('Ctrl Pts',(-1.34854391898045,1.,1.73682580585691));
#43634=CARTESIAN_POINT('Ctrl Pts',(-1.34869019493419,1.,1.73811241238545));
#43635=CARTESIAN_POINT('',(-1.15624053661742,0.,1.31362392696032));
#43636=CARTESIAN_POINT('Origin',(0.,0.,0.));
#43637=CARTESIAN_POINT('',(-1.31362392696033,1.,1.15624053661742));
#43638=CARTESIAN_POINT('Origin',(0.,1.,0.));
#43639=CARTESIAN_POINT('',(-1.31362392696033,0.,1.15624053661742));
#43640=CARTESIAN_POINT('Ctrl Pts',(-1.73811241238545,-1.,1.34869019493419));
#43641=CARTESIAN_POINT('Ctrl Pts',(-1.73811241238545,1.,1.34869019493419));
#43642=CARTESIAN_POINT('Ctrl Pts',(-1.73682580585819,-1.,1.34854391898145));
#43643=CARTESIAN_POINT('Ctrl Pts',(-1.73682580585819,1.,1.34854391898145));
#43644=CARTESIAN_POINT('Ctrl Pts',(-1.73425417886255,-1.,1.34824783113158));
#43645=CARTESIAN_POINT('Ctrl Pts',(-1.73425417886255,1.,1.34824783113158));
#43646=CARTESIAN_POINT('Ctrl Pts',(-1.73040149654497,-1.,1.3477930915247));
#43647=CARTESIAN_POINT('Ctrl Pts',(-1.73040149654497,1.,1.3477930915247));
#43648=CARTESIAN_POINT('Ctrl Pts',(-1.72527410681298,-1.,1.34716554820013));
#43649=CARTESIAN_POINT('Ctrl Pts',(-1.72527410681298,1.,1.34716554820013));
#43650=CARTESIAN_POINT('Ctrl Pts',(-1.7188807715095,-1.,1.34634568653586));
#43651=CARTESIAN_POINT('Ctrl Pts',(-1.7188807715095,1.,1.34634568653586));
#43652=CARTESIAN_POINT('Ctrl Pts',(-1.71250340687011,-1.,1.34549029589563));
#43653=CARTESIAN_POINT('Ctrl Pts',(-1.71250340687011,1.,1.34549029589563));
#43654=CARTESIAN_POINT('Ctrl Pts',(-1.70614212266676,-1.,1.34459924533783));
#43655=CARTESIAN_POINT('Ctrl Pts',(-1.70614212266676,1.,1.34459924533783));
#43656=CARTESIAN_POINT('Ctrl Pts',(-1.69979707754221,-1.,1.34367237124322));
#43657=CARTESIAN_POINT('Ctrl Pts',(-1.69979707754221,1.,1.34367237124322));
#43658=CARTESIAN_POINT('Ctrl Pts',(-1.6934684849664,-1.,1.34270948206139));
#43659=CARTESIAN_POINT('Ctrl Pts',(-1.6934684849664,1.,1.34270948206139));
#43660=CARTESIAN_POINT('Ctrl Pts',(-1.68715660868602,-1.,1.34171037484673));
#43661=CARTESIAN_POINT('Ctrl Pts',(-1.68715660868602,1.,1.34171037484673));
#43662=CARTESIAN_POINT('Ctrl Pts',(-1.68086176030308,-1.,1.3406748518516));
#43663=CARTESIAN_POINT('Ctrl Pts',(-1.68086176030308,1.,1.3406748518516));
#43664=CARTESIAN_POINT('Ctrl Pts',(-1.67458429426126,-1.,1.33960273470372));
#43665=CARTESIAN_POINT('Ctrl Pts',(-1.67458429426126,1.,1.33960273470372));
#43666=CARTESIAN_POINT('Ctrl Pts',(-1.66832460784078,-1.,1.33849388654458));
#43667=CARTESIAN_POINT('Ctrl Pts',(-1.66832460784078,1.,1.33849388654458));
#43668=CARTESIAN_POINT('Ctrl Pts',(-1.66208312542073,-1.,1.33734820885331));
#43669=CARTESIAN_POINT('Ctrl Pts',(-1.66208312542073,1.,1.33734820885331));
#43670=CARTESIAN_POINT('Ctrl Pts',(-1.65586025952651,-1.,1.33616559745217));
#43671=CARTESIAN_POINT('Ctrl Pts',(-1.65586025952651,1.,1.33616559745217));
#43672=CARTESIAN_POINT('Ctrl Pts',(-1.64965637286843,-1.,1.33494590468003));
#43673=CARTESIAN_POINT('Ctrl Pts',(-1.64965637286843,1.,1.33494590468003));
#43674=CARTESIAN_POINT('Ctrl Pts',(-1.64347174856007,-1.,1.33368890676554));
#43675=CARTESIAN_POINT('Ctrl Pts',(-1.64347174856007,1.,1.33368890676554));
#43676=CARTESIAN_POINT('Ctrl Pts',(-1.6373065347505,-1.,1.33239425103694));
#43677=CARTESIAN_POINT('Ctrl Pts',(-1.6373065347505,1.,1.33239425103694));
#43678=CARTESIAN_POINT('Ctrl Pts',(-1.63116079730887,-1.,1.33106149345618));
#43679=CARTESIAN_POINT('Ctrl Pts',(-1.63116079730887,1.,1.33106149345618));
#43680=CARTESIAN_POINT('Ctrl Pts',(-1.62503464209777,-1.,1.32969019505665));
#43681=CARTESIAN_POINT('Ctrl Pts',(-1.62503464209777,1.,1.32969019505665));
#43682=CARTESIAN_POINT('Ctrl Pts',(-1.61892832270723,-1.,1.32828000610448));
#43683=CARTESIAN_POINT('Ctrl Pts',(-1.61892832270723,1.,1.32828000610448));
#43684=CARTESIAN_POINT('Ctrl Pts',(-1.61284234015762,-1.,1.32683074483365));
#43685=CARTESIAN_POINT('Ctrl Pts',(-1.61284234015762,1.,1.32683074483365));
#43686=CARTESIAN_POINT('Ctrl Pts',(-1.6067775829097,-1.,1.32534250785794));
#43687=CARTESIAN_POINT('Ctrl Pts',(-1.6067775829097,1.,1.32534250785794));
#43688=CARTESIAN_POINT('Ctrl Pts',(-1.600735118587,-1.,1.32381550858266));
#43689=CARTESIAN_POINT('Ctrl Pts',(-1.600735118587,1.,1.32381550858266));
#43690=CARTESIAN_POINT('Ctrl Pts',(-1.59471591079408,-1.,1.32224985747686));
#43691=CARTESIAN_POINT('Ctrl Pts',(-1.59471591079408,1.,1.32224985747686));
#43692=CARTESIAN_POINT('Ctrl Pts',(-1.58872057258244,-1.,1.32064537110891));
#43693=CARTESIAN_POINT('Ctrl Pts',(-1.58872057258244,1.,1.32064537110891));
#43694=CARTESIAN_POINT('Ctrl Pts',(-1.58274907898829,-1.,1.31900135021428));
#43695=CARTESIAN_POINT('Ctrl Pts',(-1.58274907898829,1.,1.31900135021428));
#43696=CARTESIAN_POINT('Ctrl Pts',(-1.57680056505585,-1.,1.31731642317183));
#43697=CARTESIAN_POINT('Ctrl Pts',(-1.57680056505585,1.,1.31731642317183));
#43698=CARTESIAN_POINT('Ctrl Pts',(-1.57087397835721,-1.,1.31558903860015));
#43699=CARTESIAN_POINT('Ctrl Pts',(-1.57087397835721,1.,1.31558903860015));
#43700=CARTESIAN_POINT('Ctrl Pts',(-1.56496872402352,-1.,1.31381795281002));
#43701=CARTESIAN_POINT('Ctrl Pts',(-1.56496872402352,1.,1.31381795281002));
#43702=CARTESIAN_POINT('Ctrl Pts',(-1.55908521254822,-1.,1.31200264341696));
#43703=CARTESIAN_POINT('Ctrl Pts',(-1.55908521254822,1.,1.31200264341696));
#43704=CARTESIAN_POINT('Ctrl Pts',(-1.55322568759481,-1.,1.31014393684221));
#43705=CARTESIAN_POINT('Ctrl Pts',(-1.55322568759481,1.,1.31014393684221));
#43706=CARTESIAN_POINT('Ctrl Pts',(-1.54739413957183,-1.,1.30824393907471));
#43707=CARTESIAN_POINT('Ctrl Pts',(-1.54739413957183,1.,1.30824393907471));
#43708=CARTESIAN_POINT('Ctrl Pts',(-1.54159462645428,-1.,1.30630475189553));
#43709=CARTESIAN_POINT('Ctrl Pts',(-1.54159462645428,1.,1.30630475189553));
#43710=CARTESIAN_POINT('Ctrl Pts',(-1.53582981268976,-1.,1.30432735639487));
#43711=CARTESIAN_POINT('Ctrl Pts',(-1.53582981268976,1.,1.30432735639487));
#43712=CARTESIAN_POINT('Ctrl Pts',(-1.53009970283893,-1.,1.3023106439557));
#43713=CARTESIAN_POINT('Ctrl Pts',(-1.53009970283893,1.,1.3023106439557));
#43714=CARTESIAN_POINT('Ctrl Pts',(-1.5243995786107,-1.,1.30024984366334));
#43715=CARTESIAN_POINT('Ctrl Pts',(-1.5243995786107,1.,1.30024984366334));
#43716=CARTESIAN_POINT('Ctrl Pts',(-1.51872184912735,-1.,1.29813791800757));
#43717=CARTESIAN_POINT('Ctrl Pts',(-1.51872184912735,1.,1.29813791800757));
#43718=CARTESIAN_POINT('Ctrl Pts',(-1.51305994241412,-1.,1.29596850710518));
#43719=CARTESIAN_POINT('Ctrl Pts',(-1.51305994241412,1.,1.29596850710518));
#43720=CARTESIAN_POINT('Ctrl Pts',(-1.50741159078367,-1.,1.29373841372843));
#43721=CARTESIAN_POINT('Ctrl Pts',(-1.50741159078367,1.,1.29373841372843));
#43722=CARTESIAN_POINT('Ctrl Pts',(-1.50178230149764,-1.,1.29145022885171));
#43723=CARTESIAN_POINT('Ctrl Pts',(-1.50178230149764,1.,1.29145022885171));
#43724=CARTESIAN_POINT('Ctrl Pts',(-1.49618896881729,-1.,1.28911506584232));
#43725=CARTESIAN_POINT('Ctrl Pts',(-1.49618896881729,1.,1.28911506584232));
#43726=CARTESIAN_POINT('Ctrl Pts',(-1.4906522831275,-1.,1.28674676116415));
#43727=CARTESIAN_POINT('Ctrl Pts',(-1.4906522831275,1.,1.28674676116415));
#43728=CARTESIAN_POINT('Ctrl Pts',(-1.48518817118891,-1.,1.28435533880184));
#43729=CARTESIAN_POINT('Ctrl Pts',(-1.48518817118891,1.,1.28435533880184));
#43730=CARTESIAN_POINT('Ctrl Pts',(-1.47980070347102,-1.,1.28194158939522));
#43731=CARTESIAN_POINT('Ctrl Pts',(-1.47980070347102,1.,1.28194158939522));
#43732=CARTESIAN_POINT('Ctrl Pts',(-1.4744717526711,-1.,1.27948918248524));
#43733=CARTESIAN_POINT('Ctrl Pts',(-1.4744717526711,1.,1.27948918248524));
#43734=CARTESIAN_POINT('Ctrl Pts',(-1.46916035917197,-1.,1.27696414831144));
#43735=CARTESIAN_POINT('Ctrl Pts',(-1.46916035917197,1.,1.27696414831144));
#43736=CARTESIAN_POINT('Ctrl Pts',(-1.4638243133254,-1.,1.27433119897877));
#43737=CARTESIAN_POINT('Ctrl Pts',(-1.4638243133254,1.,1.27433119897877));
#43738=CARTESIAN_POINT('Ctrl Pts',(-1.45843906294725,-1.,1.27156805265312));
#43739=CARTESIAN_POINT('Ctrl Pts',(-1.45843906294725,1.,1.27156805265312));
#43740=CARTESIAN_POINT('Ctrl Pts',(-1.45301422764205,-1.,1.26867786804854));
#43741=CARTESIAN_POINT('Ctrl Pts',(-1.45301422764205,1.,1.26867786804854));
#43742=CARTESIAN_POINT('Ctrl Pts',(-1.44761985001544,-1.,1.26570925118767));
#43743=CARTESIAN_POINT('Ctrl Pts',(-1.44761985001544,1.,1.26570925118767));
#43744=CARTESIAN_POINT('Ctrl Pts',(-1.44236470511145,-1.,1.26273903323723));
#43745=CARTESIAN_POINT('Ctrl Pts',(-1.44236470511145,1.,1.26273903323723));
#43746=CARTESIAN_POINT('Ctrl Pts',(-1.43734919180719,-1.,1.25983531011894));
#43747=CARTESIAN_POINT('Ctrl Pts',(-1.43734919180719,1.,1.25983531011894));
#43748=CARTESIAN_POINT('Ctrl Pts',(-1.43262645609679,-1.,1.25702687965744));
#43749=CARTESIAN_POINT('Ctrl Pts',(-1.43262645609679,1.,1.25702687965744));
#43750=CARTESIAN_POINT('Ctrl Pts',(-1.42815938799555,-1.,1.25426945222783));
#43751=CARTESIAN_POINT('Ctrl Pts',(-1.42815938799555,1.,1.25426945222783));
#43752=CARTESIAN_POINT('Ctrl Pts',(-1.42378102115911,-1.,1.25141455570299));
#43753=CARTESIAN_POINT('Ctrl Pts',(-1.42378102115911,1.,1.25141455570299));
#43754=CARTESIAN_POINT('Ctrl Pts',(-1.41923722596421,-1.,1.24824430986911));
#43755=CARTESIAN_POINT('Ctrl Pts',(-1.41923722596421,1.,1.24824430986911));
#43756=CARTESIAN_POINT('Ctrl Pts',(-1.41422913175437,-1.,1.24450600513278));
#43757=CARTESIAN_POINT('Ctrl Pts',(-1.41422913175437,1.,1.24450600513278));
#43758=CARTESIAN_POINT('Ctrl Pts',(-1.40845295531151,-1.,1.23994455029421));
#43759=CARTESIAN_POINT('Ctrl Pts',(-1.40845295531151,1.,1.23994455029421));
#43760=CARTESIAN_POINT('Ctrl Pts',(-1.40164708205345,-1.,1.23434087289768));
#43761=CARTESIAN_POINT('Ctrl Pts',(-1.40164708205345,1.,1.23434087289768));
#43762=CARTESIAN_POINT('Ctrl Pts',(-1.39361389567257,-1.,1.22752961898063));
#43763=CARTESIAN_POINT('Ctrl Pts',(-1.39361389567257,1.,1.22752961898063));
#43764=CARTESIAN_POINT('Ctrl Pts',(-1.38420564525391,-1.,1.21938737278853));
#43765=CARTESIAN_POINT('Ctrl Pts',(-1.38420564525391,1.,1.21938737278853));
#43766=CARTESIAN_POINT('Ctrl Pts',(-1.37331915604962,-1.,1.20982812923113));
#43767=CARTESIAN_POINT('Ctrl Pts',(-1.37331915604962,1.,1.20982812923113));
#43768=CARTESIAN_POINT('Ctrl Pts',(-1.36088705040677,-1.,1.1987959077656));
#43769=CARTESIAN_POINT('Ctrl Pts',(-1.36088705040677,1.,1.1987959077656));
#43770=CARTESIAN_POINT('Ctrl Pts',(-1.34687053998157,-1.,1.18625865664915));
#43771=CARTESIAN_POINT('Ctrl Pts',(-1.34687053998157,1.,1.18625865664915));
#43772=CARTESIAN_POINT('Ctrl Pts',(-1.33437539344842,-1.,1.17501305787994));
#43773=CARTESIAN_POINT('Ctrl Pts',(-1.33437539344842,1.,1.17501305787994));
#43774=CARTESIAN_POINT('Ctrl Pts',(-1.32428080720544,-1.,1.16589330092532));
#43775=CARTESIAN_POINT('Ctrl Pts',(-1.32428080720544,1.,1.16589330092532));
#43776=CARTESIAN_POINT('Ctrl Pts',(-1.3172297721596,-1.,1.15950888730433));
#43777=CARTESIAN_POINT('Ctrl Pts',(-1.3172297721596,1.,1.15950888730433));
#43778=CARTESIAN_POINT('Ctrl Pts',(-1.31362392696033,-1.,1.15624053661742));
#43779=CARTESIAN_POINT('Ctrl Pts',(-1.31362392696033,1.,1.15624053661742));
#43780=CARTESIAN_POINT('',(-1.73811241238545,1.,1.34869019493419));
#43781=CARTESIAN_POINT('Ctrl Pts',(-1.73811241238545,1.,1.34869019493419));
#43782=CARTESIAN_POINT('Ctrl Pts',(-1.73682580585819,1.,1.34854391898145));
#43783=CARTESIAN_POINT('Ctrl Pts',(-1.73425417886255,1.,1.34824783113158));
#43784=CARTESIAN_POINT('Ctrl Pts',(-1.73040149654497,1.,1.3477930915247));
#43785=CARTESIAN_POINT('Ctrl Pts',(-1.72527410681298,1.,1.34716554820013));
#43786=CARTESIAN_POINT('Ctrl Pts',(-1.7188807715095,1.,1.34634568653586));
#43787=CARTESIAN_POINT('Ctrl Pts',(-1.71250340687011,1.,1.34549029589563));
#43788=CARTESIAN_POINT('Ctrl Pts',(-1.70614212266676,1.,1.34459924533783));
#43789=CARTESIAN_POINT('Ctrl Pts',(-1.69979707754221,1.,1.34367237124322));
#43790=CARTESIAN_POINT('Ctrl Pts',(-1.6934684849664,1.,1.34270948206139));
#43791=CARTESIAN_POINT('Ctrl Pts',(-1.68715660868602,1.,1.34171037484673));
#43792=CARTESIAN_POINT('Ctrl Pts',(-1.68086176030308,1.,1.3406748518516));
#43793=CARTESIAN_POINT('Ctrl Pts',(-1.67458429426126,1.,1.33960273470372));
#43794=CARTESIAN_POINT('Ctrl Pts',(-1.66832460784078,1.,1.33849388654458));
#43795=CARTESIAN_POINT('Ctrl Pts',(-1.66208312542073,1.,1.33734820885331));
#43796=CARTESIAN_POINT('Ctrl Pts',(-1.65586025952651,1.,1.33616559745217));
#43797=CARTESIAN_POINT('Ctrl Pts',(-1.64965637286843,1.,1.33494590468003));
#43798=CARTESIAN_POINT('Ctrl Pts',(-1.64347174856007,1.,1.33368890676554));
#43799=CARTESIAN_POINT('Ctrl Pts',(-1.6373065347505,1.,1.33239425103694));
#43800=CARTESIAN_POINT('Ctrl Pts',(-1.63116079730887,1.,1.33106149345618));
#43801=CARTESIAN_POINT('Ctrl Pts',(-1.62503464209777,1.,1.32969019505665));
#43802=CARTESIAN_POINT('Ctrl Pts',(-1.61892832270723,1.,1.32828000610448));
#43803=CARTESIAN_POINT('Ctrl Pts',(-1.61284234015762,1.,1.32683074483365));
#43804=CARTESIAN_POINT('Ctrl Pts',(-1.6067775829097,1.,1.32534250785794));
#43805=CARTESIAN_POINT('Ctrl Pts',(-1.600735118587,1.,1.32381550858266));
#43806=CARTESIAN_POINT('Ctrl Pts',(-1.59471591079408,1.,1.32224985747686));
#43807=CARTESIAN_POINT('Ctrl Pts',(-1.58872057258244,1.,1.32064537110891));
#43808=CARTESIAN_POINT('Ctrl Pts',(-1.58274907898829,1.,1.31900135021428));
#43809=CARTESIAN_POINT('Ctrl Pts',(-1.57680056505585,1.,1.31731642317183));
#43810=CARTESIAN_POINT('Ctrl Pts',(-1.57087397835721,1.,1.31558903860015));
#43811=CARTESIAN_POINT('Ctrl Pts',(-1.56496872402352,1.,1.31381795281002));
#43812=CARTESIAN_POINT('Ctrl Pts',(-1.55908521254822,1.,1.31200264341696));
#43813=CARTESIAN_POINT('Ctrl Pts',(-1.55322568759481,1.,1.31014393684221));
#43814=CARTESIAN_POINT('Ctrl Pts',(-1.54739413957183,1.,1.30824393907471));
#43815=CARTESIAN_POINT('Ctrl Pts',(-1.54159462645428,1.,1.30630475189553));
#43816=CARTESIAN_POINT('Ctrl Pts',(-1.53582981268976,1.,1.30432735639487));
#43817=CARTESIAN_POINT('Ctrl Pts',(-1.53009970283893,1.,1.3023106439557));
#43818=CARTESIAN_POINT('Ctrl Pts',(-1.5243995786107,1.,1.30024984366334));
#43819=CARTESIAN_POINT('Ctrl Pts',(-1.51872184912735,1.,1.29813791800757));
#43820=CARTESIAN_POINT('Ctrl Pts',(-1.51305994241412,1.,1.29596850710518));
#43821=CARTESIAN_POINT('Ctrl Pts',(-1.50741159078367,1.,1.29373841372843));
#43822=CARTESIAN_POINT('Ctrl Pts',(-1.50178230149764,1.,1.29145022885171));
#43823=CARTESIAN_POINT('Ctrl Pts',(-1.49618896881729,1.,1.28911506584232));
#43824=CARTESIAN_POINT('Ctrl Pts',(-1.4906522831275,1.,1.28674676116415));
#43825=CARTESIAN_POINT('Ctrl Pts',(-1.48518817118891,1.,1.28435533880184));
#43826=CARTESIAN_POINT('Ctrl Pts',(-1.47980070347102,1.,1.28194158939522));
#43827=CARTESIAN_POINT('Ctrl Pts',(-1.4744717526711,1.,1.27948918248524));
#43828=CARTESIAN_POINT('Ctrl Pts',(-1.46916035917197,1.,1.27696414831144));
#43829=CARTESIAN_POINT('Ctrl Pts',(-1.4638243133254,1.,1.27433119897877));
#43830=CARTESIAN_POINT('Ctrl Pts',(-1.45843906294725,1.,1.27156805265312));
#43831=CARTESIAN_POINT('Ctrl Pts',(-1.45301422764205,1.,1.26867786804854));
#43832=CARTESIAN_POINT('Ctrl Pts',(-1.44761985001544,1.,1.26570925118767));
#43833=CARTESIAN_POINT('Ctrl Pts',(-1.44236470511145,1.,1.26273903323723));
#43834=CARTESIAN_POINT('Ctrl Pts',(-1.43734919180719,1.,1.25983531011894));
#43835=CARTESIAN_POINT('Ctrl Pts',(-1.43262645609679,1.,1.25702687965744));
#43836=CARTESIAN_POINT('Ctrl Pts',(-1.42815938799555,1.,1.25426945222783));
#43837=CARTESIAN_POINT('Ctrl Pts',(-1.42378102115911,1.,1.25141455570299));
#43838=CARTESIAN_POINT('Ctrl Pts',(-1.41923722596421,1.,1.24824430986911));
#43839=CARTESIAN_POINT('Ctrl Pts',(-1.41422913175437,1.,1.24450600513278));
#43840=CARTESIAN_POINT('Ctrl Pts',(-1.40845295531151,1.,1.23994455029421));
#43841=CARTESIAN_POINT('Ctrl Pts',(-1.40164708205345,1.,1.23434087289768));
#43842=CARTESIAN_POINT('Ctrl Pts',(-1.39361389567257,1.,1.22752961898063));
#43843=CARTESIAN_POINT('Ctrl Pts',(-1.38420564525391,1.,1.21938737278853));
#43844=CARTESIAN_POINT('Ctrl Pts',(-1.37331915604962,1.,1.20982812923113));
#43845=CARTESIAN_POINT('Ctrl Pts',(-1.36088705040677,1.,1.1987959077656));
#43846=CARTESIAN_POINT('Ctrl Pts',(-1.34687053998157,1.,1.18625865664915));
#43847=CARTESIAN_POINT('Ctrl Pts',(-1.33437539344842,1.,1.17501305787994));
#43848=CARTESIAN_POINT('Ctrl Pts',(-1.32428080720544,1.,1.16589330092532));
#43849=CARTESIAN_POINT('Ctrl Pts',(-1.3172297721596,1.,1.15950888730433));
#43850=CARTESIAN_POINT('Ctrl Pts',(-1.31362392696033,1.,1.15624053661742));
#43851=CARTESIAN_POINT('',(-1.73811241238545,0.,1.34869019493419));
#43852=CARTESIAN_POINT('Origin',(-1.81978687191668,0.,1.23627494547115));
#43853=CARTESIAN_POINT('',(-1.81978687191668,1.,1.23627494547115));
#43854=CARTESIAN_POINT('',(-1.73811241238545,1.,1.34869019493419));
#43855=CARTESIAN_POINT('',(-1.81978687191668,0.,1.23627494547115));
#43856=CARTESIAN_POINT('Ctrl Pts',(-1.5055822144029,-1.,0.892032620296855));
#43857=CARTESIAN_POINT('Ctrl Pts',(-1.5055822144029,1.,0.892032620296855));
#43858=CARTESIAN_POINT('Ctrl Pts',(-1.50980486807181,-1.,0.894452006967538));
#43859=CARTESIAN_POINT('Ctrl Pts',(-1.50980486807181,1.,0.894452006967538));
#43860=CARTESIAN_POINT('Ctrl Pts',(-1.51805569591479,-1.,0.89918504749193));
#43861=CARTESIAN_POINT('Ctrl Pts',(-1.51805569591479,1.,0.89918504749193));
#43862=CARTESIAN_POINT('Ctrl Pts',(-1.52984849890434,-1.,0.905967409640499));
#43863=CARTESIAN_POINT('Ctrl Pts',(-1.52984849890434,1.,0.905967409640499));
#43864=CARTESIAN_POINT('Ctrl Pts',(-1.54440491152808,-1.,0.91437591904658));
#43865=CARTESIAN_POINT('Ctrl Pts',(-1.54440491152808,1.,0.91437591904658));
#43866=CARTESIAN_POINT('Ctrl Pts',(-1.56065988582509,-1.,0.923832188966322));
#43867=CARTESIAN_POINT('Ctrl Pts',(-1.56065988582509,1.,0.923832188966322));
#43868=CARTESIAN_POINT('Ctrl Pts',(-1.57499388385561,-1.,0.932246680128849));
#43869=CARTESIAN_POINT('Ctrl Pts',(-1.57499388385561,1.,0.932246680128849));
#43870=CARTESIAN_POINT('Ctrl Pts',(-1.58744937489796,-1.,0.939646377909319));
#43871=CARTESIAN_POINT('Ctrl Pts',(-1.58744937489796,1.,0.939646377909319));
#43872=CARTESIAN_POINT('Ctrl Pts',(-1.59810042045408,-1.,0.946078063325796));
#43873=CARTESIAN_POINT('Ctrl Pts',(-1.59810042045408,1.,0.946078063325796));
#43874=CARTESIAN_POINT('Ctrl Pts',(-1.60706069897794,-1.,0.951613284361248));
#43875=CARTESIAN_POINT('Ctrl Pts',(-1.60706069897794,1.,0.951613284361248));
#43876=CARTESIAN_POINT('Ctrl Pts',(-1.61449324337233,-1.,0.956354422921573));
#43877=CARTESIAN_POINT('Ctrl Pts',(-1.61449324337233,1.,0.956354422921573));
#43878=CARTESIAN_POINT('Ctrl Pts',(-1.62061638139929,-1.,0.960438326099958));
#43879=CARTESIAN_POINT('Ctrl Pts',(-1.62061638139929,1.,0.960438326099958));
#43880=CARTESIAN_POINT('Ctrl Pts',(-1.6257193066974,-1.,0.964046107037821));
#43881=CARTESIAN_POINT('Ctrl Pts',(-1.6257193066974,1.,0.964046107037821));
#43882=CARTESIAN_POINT('Ctrl Pts',(-1.63013849959083,-1.,0.967387853228041));
#43883=CARTESIAN_POINT('Ctrl Pts',(-1.63013849959083,1.,0.967387853228041));
#43884=CARTESIAN_POINT('Ctrl Pts',(-1.63420665729609,-1.,0.970669715996356));
#43885=CARTESIAN_POINT('Ctrl Pts',(-1.63420665729609,1.,0.970669715996356));
#43886=CARTESIAN_POINT('Ctrl Pts',(-1.63820952658157,-1.,0.974066058287501));
#43887=CARTESIAN_POINT('Ctrl Pts',(-1.63820952658157,1.,0.974066058287501));
#43888=CARTESIAN_POINT('Ctrl Pts',(-1.64233990826831,-1.,0.977689794120297));
#43889=CARTESIAN_POINT('Ctrl Pts',(-1.64233990826831,1.,0.977689794120297));
#43890=CARTESIAN_POINT('Ctrl Pts',(-1.64665139190834,-1.,0.981562530940574));
#43891=CARTESIAN_POINT('Ctrl Pts',(-1.64665139190834,1.,0.981562530940574));
#43892=CARTESIAN_POINT('Ctrl Pts',(-1.6511001661277,-1.,0.985642622921626));
#43893=CARTESIAN_POINT('Ctrl Pts',(-1.6511001661277,1.,0.985642622921626));
#43894=CARTESIAN_POINT('Ctrl Pts',(-1.65559044289746,-1.,0.98985562785445));
#43895=CARTESIAN_POINT('Ctrl Pts',(-1.65559044289746,1.,0.98985562785445));
#43896=CARTESIAN_POINT('Ctrl Pts',(-1.66001553809916,-1.,0.994121836661116));
#43897=CARTESIAN_POINT('Ctrl Pts',(-1.66001553809916,1.,0.994121836661116));
#43898=CARTESIAN_POINT('Ctrl Pts',(-1.66430758030304,-1.,0.998389654952317));
#43899=CARTESIAN_POINT('Ctrl Pts',(-1.66430758030304,1.,0.998389654952317));
#43900=CARTESIAN_POINT('Ctrl Pts',(-1.66846059277231,-1.,1.00265091003682));
#43901=CARTESIAN_POINT('Ctrl Pts',(-1.66846059277231,1.,1.00265091003682));
#43902=CARTESIAN_POINT('Ctrl Pts',(-1.67250335383248,-1.,1.00692206696387));
#43903=CARTESIAN_POINT('Ctrl Pts',(-1.67250335383248,1.,1.00692206696387));
#43904=CARTESIAN_POINT('Ctrl Pts',(-1.67648246776457,-1.,1.01123236493507));
#43905=CARTESIAN_POINT('Ctrl Pts',(-1.67648246776457,1.,1.01123236493507));
#43906=CARTESIAN_POINT('Ctrl Pts',(-1.6804428989482,-1.,1.01561026162787));
#43907=CARTESIAN_POINT('Ctrl Pts',(-1.6804428989482,1.,1.01561026162787));
#43908=CARTESIAN_POINT('Ctrl Pts',(-1.68440578021739,-1.,1.02006795074222));
#43909=CARTESIAN_POINT('Ctrl Pts',(-1.68440578021739,1.,1.02006795074222));
#43910=CARTESIAN_POINT('Ctrl Pts',(-1.68836910178475,-1.,1.02460180535272));
#43911=CARTESIAN_POINT('Ctrl Pts',(-1.68836910178475,1.,1.02460180535272));
#43912=CARTESIAN_POINT('Ctrl Pts',(-1.69231840863471,-1.,1.02919977579155));
#43913=CARTESIAN_POINT('Ctrl Pts',(-1.69231840863471,1.,1.02919977579155));
#43914=CARTESIAN_POINT('Ctrl Pts',(-1.69623414782769,-1.,1.03384646003587));
#43915=CARTESIAN_POINT('Ctrl Pts',(-1.69623414782769,1.,1.03384646003587));
#43916=CARTESIAN_POINT('Ctrl Pts',(-1.70010052930951,-1.,1.03852922490782));
#43917=CARTESIAN_POINT('Ctrl Pts',(-1.70010052930951,1.,1.03852922490782));
#43918=CARTESIAN_POINT('Ctrl Pts',(-1.70391338707969,-1.,1.04324363334546));
#43919=CARTESIAN_POINT('Ctrl Pts',(-1.70391338707969,1.,1.04324363334546));
#43920=CARTESIAN_POINT('Ctrl Pts',(-1.70767646263641,-1.,1.0479908540499));
#43921=CARTESIAN_POINT('Ctrl Pts',(-1.70767646263641,1.,1.0479908540499));
#43922=CARTESIAN_POINT('Ctrl Pts',(-1.71139783543986,-1.,1.05277517202854));
#43923=CARTESIAN_POINT('Ctrl Pts',(-1.71139783543986,1.,1.05277517202854));
#43924=CARTESIAN_POINT('Ctrl Pts',(-1.71508654427022,-1.,1.05760163192481));
#43925=CARTESIAN_POINT('Ctrl Pts',(-1.71508654427022,1.,1.05760163192481));
#43926=CARTESIAN_POINT('Ctrl Pts',(-1.71874858456908,-1.,1.0624732468065));
#43927=CARTESIAN_POINT('Ctrl Pts',(-1.71874858456908,1.,1.0624732468065));
#43928=CARTESIAN_POINT('Ctrl Pts',(-1.72238500928456,-1.,1.06738966975463));
#43929=CARTESIAN_POINT('Ctrl Pts',(-1.72238500928456,1.,1.06738966975463));
#43930=CARTESIAN_POINT('Ctrl Pts',(-1.72599406198489,-1.,1.07234866990252));
#43931=CARTESIAN_POINT('Ctrl Pts',(-1.72599406198489,1.,1.07234866990252));
#43932=CARTESIAN_POINT('Ctrl Pts',(-1.72957248977424,-1.,1.0773470373727));
#43933=CARTESIAN_POINT('Ctrl Pts',(-1.72957248977424,1.,1.0773470373727));
#43934=CARTESIAN_POINT('Ctrl Pts',(-1.73311705663407,-1.,1.08238162784749));
#43935=CARTESIAN_POINT('Ctrl Pts',(-1.73311705663407,1.,1.08238162784749));
#43936=CARTESIAN_POINT('Ctrl Pts',(-1.73662628326093,-1.,1.08745056285429));
#43937=CARTESIAN_POINT('Ctrl Pts',(-1.73662628326093,1.,1.08745056285429));
#43938=CARTESIAN_POINT('Ctrl Pts',(-1.74010053962252,-1.,1.09255329056496));
#43939=CARTESIAN_POINT('Ctrl Pts',(-1.74010053962252,1.,1.09255329056496));
#43940=CARTESIAN_POINT('Ctrl Pts',(-1.74354119236212,-1.,1.09768999241229));
#43941=CARTESIAN_POINT('Ctrl Pts',(-1.74354119236212,1.,1.09768999241229));
#43942=CARTESIAN_POINT('Ctrl Pts',(-1.74695004214924,-1.,1.10286118991144));
#43943=CARTESIAN_POINT('Ctrl Pts',(-1.74695004214924,1.,1.10286118991144));
#43944=CARTESIAN_POINT('Ctrl Pts',(-1.75032866075914,-1.,1.10806728183003));
#43945=CARTESIAN_POINT('Ctrl Pts',(-1.75032866075914,1.,1.10806728183003));
#43946=CARTESIAN_POINT('Ctrl Pts',(-1.75367772094617,-1.,1.11330807582542));
#43947=CARTESIAN_POINT('Ctrl Pts',(-1.75367772094617,1.,1.11330807582542));
#43948=CARTESIAN_POINT('Ctrl Pts',(-1.75699720772089,-1.,1.11858293216752));
#43949=CARTESIAN_POINT('Ctrl Pts',(-1.75699720772089,1.,1.11858293216752));
#43950=CARTESIAN_POINT('Ctrl Pts',(-1.76028671825084,-1.,1.12389096855078));
#43951=CARTESIAN_POINT('Ctrl Pts',(-1.76028671825084,1.,1.12389096855078));
#43952=CARTESIAN_POINT('Ctrl Pts',(-1.76354571966171,-1.,1.12923123555076));
#43953=CARTESIAN_POINT('Ctrl Pts',(-1.76354571966171,1.,1.12923123555076));
#43954=CARTESIAN_POINT('Ctrl Pts',(-1.76677384551883,-1.,1.13460291804635));
#43955=CARTESIAN_POINT('Ctrl Pts',(-1.76677384551883,1.,1.13460291804635));
#43956=CARTESIAN_POINT('Ctrl Pts',(-1.76997111386806,-1.,1.14000548337));
#43957=CARTESIAN_POINT('Ctrl Pts',(-1.76997111386806,1.,1.14000548337));
#43958=CARTESIAN_POINT('Ctrl Pts',(-1.77313777896234,-1.,1.14543858226948));
#43959=CARTESIAN_POINT('Ctrl Pts',(-1.77313777896234,1.,1.14543858226948));
#43960=CARTESIAN_POINT('Ctrl Pts',(-1.77627422557034,-1.,1.15090197841531));
#43961=CARTESIAN_POINT('Ctrl Pts',(-1.77627422557034,1.,1.15090197841531));
#43962=CARTESIAN_POINT('Ctrl Pts',(-1.77938085564261,-1.,1.15639547194689));
#43963=CARTESIAN_POINT('Ctrl Pts',(-1.77938085564261,1.,1.15639547194689));
#43964=CARTESIAN_POINT('Ctrl Pts',(-1.78245795880949,-1.,1.16191881298458));
#43965=CARTESIAN_POINT('Ctrl Pts',(-1.78245795880949,1.,1.16191881298458));
#43966=CARTESIAN_POINT('Ctrl Pts',(-1.78550566040349,-1.,1.16747166312239));
#43967=CARTESIAN_POINT('Ctrl Pts',(-1.78550566040349,1.,1.16747166312239));
#43968=CARTESIAN_POINT('Ctrl Pts',(-1.78852398877523,-1.,1.17305363177265));
#43969=CARTESIAN_POINT('Ctrl Pts',(-1.78852398877523,1.,1.17305363177265));
#43970=CARTESIAN_POINT('Ctrl Pts',(-1.79151291552646,-1.,1.17866429440781));
#43971=CARTESIAN_POINT('Ctrl Pts',(-1.79151291552646,1.,1.17866429440781));
#43972=CARTESIAN_POINT('Ctrl Pts',(-1.79447240321572,-1.,1.18430321697471));
#43973=CARTESIAN_POINT('Ctrl Pts',(-1.79447240321572,1.,1.18430321697471));
#43974=CARTESIAN_POINT('Ctrl Pts',(-1.79740245923649,-1.,1.1899699793456));
#43975=CARTESIAN_POINT('Ctrl Pts',(-1.79740245923649,1.,1.1899699793456));
#43976=CARTESIAN_POINT('Ctrl Pts',(-1.80030314370121,-1.,1.19566418930405));
#43977=CARTESIAN_POINT('Ctrl Pts',(-1.80030314370121,1.,1.19566418930405));
#43978=CARTESIAN_POINT('Ctrl Pts',(-1.8031745483882,-1.,1.2013854893912));
#43979=CARTESIAN_POINT('Ctrl Pts',(-1.8031745483882,1.,1.2013854893912));
#43980=CARTESIAN_POINT('Ctrl Pts',(-1.80601678480772,-1.,1.20713356605519));
#43981=CARTESIAN_POINT('Ctrl Pts',(-1.80601678480772,1.,1.20713356605519));
#43982=CARTESIAN_POINT('Ctrl Pts',(-1.80882996916931,-1.,1.2129081570818));
#43983=CARTESIAN_POINT('Ctrl Pts',(-1.80882996916931,1.,1.2129081570818));
#43984=CARTESIAN_POINT('Ctrl Pts',(-1.81161420806172,-1.,1.2187090610323));
#43985=CARTESIAN_POINT('Ctrl Pts',(-1.81161420806172,1.,1.2187090610323));
#43986=CARTESIAN_POINT('Ctrl Pts',(-1.81436959209778,-1.,1.22453613304507));
#43987=CARTESIAN_POINT('Ctrl Pts',(-1.81436959209778,1.,1.22453613304507));
#43988=CARTESIAN_POINT('Ctrl Pts',(-1.81655087183054,-1.,1.22921864890975));
#43989=CARTESIAN_POINT('Ctrl Pts',(-1.81655087183054,1.,1.22921864890975));
#43990=CARTESIAN_POINT('Ctrl Pts',(-1.81817389920914,-1.,1.23274224526804));
#43991=CARTESIAN_POINT('Ctrl Pts',(-1.81817389920914,1.,1.23274224526804));
#43992=CARTESIAN_POINT('Ctrl Pts',(-1.81925017193531,-1.,1.23509651170384));
#43993=CARTESIAN_POINT('Ctrl Pts',(-1.81925017193531,1.,1.23509651170384));
#43994=CARTESIAN_POINT('Ctrl Pts',(-1.81978687191668,-1.,1.23627494547115));
#43995=CARTESIAN_POINT('Ctrl Pts',(-1.81978687191668,1.,1.23627494547115));
#43996=CARTESIAN_POINT('',(-1.5055822144029,1.,0.892032620296855));
#43997=CARTESIAN_POINT('Ctrl Pts',(-1.5055822144029,1.,0.892032620296855));
#43998=CARTESIAN_POINT('Ctrl Pts',(-1.50980486807181,1.,0.894452006967538));
#43999=CARTESIAN_POINT('Ctrl Pts',(-1.51805569591479,1.,0.89918504749193));
#44000=CARTESIAN_POINT('Ctrl Pts',(-1.52984849890434,1.,0.905967409640499));
#44001=CARTESIAN_POINT('Ctrl Pts',(-1.54440491152808,1.,0.91437591904658));
#44002=CARTESIAN_POINT('Ctrl Pts',(-1.56065988582509,1.,0.923832188966322));
#44003=CARTESIAN_POINT('Ctrl Pts',(-1.57499388385561,1.,0.932246680128849));
#44004=CARTESIAN_POINT('Ctrl Pts',(-1.58744937489796,1.,0.939646377909319));
#44005=CARTESIAN_POINT('Ctrl Pts',(-1.59810042045408,1.,0.946078063325796));
#44006=CARTESIAN_POINT('Ctrl Pts',(-1.60706069897794,1.,0.951613284361248));
#44007=CARTESIAN_POINT('Ctrl Pts',(-1.61449324337233,1.,0.956354422921573));
#44008=CARTESIAN_POINT('Ctrl Pts',(-1.62061638139929,1.,0.960438326099958));
#44009=CARTESIAN_POINT('Ctrl Pts',(-1.6257193066974,1.,0.964046107037821));
#44010=CARTESIAN_POINT('Ctrl Pts',(-1.63013849959083,1.,0.967387853228041));
#44011=CARTESIAN_POINT('Ctrl Pts',(-1.63420665729609,1.,0.970669715996356));
#44012=CARTESIAN_POINT('Ctrl Pts',(-1.63820952658157,1.,0.974066058287501));
#44013=CARTESIAN_POINT('Ctrl Pts',(-1.64233990826831,1.,0.977689794120297));
#44014=CARTESIAN_POINT('Ctrl Pts',(-1.64665139190834,1.,0.981562530940574));
#44015=CARTESIAN_POINT('Ctrl Pts',(-1.6511001661277,1.,0.985642622921626));
#44016=CARTESIAN_POINT('Ctrl Pts',(-1.65559044289746,1.,0.98985562785445));
#44017=CARTESIAN_POINT('Ctrl Pts',(-1.66001553809916,1.,0.994121836661116));
#44018=CARTESIAN_POINT('Ctrl Pts',(-1.66430758030304,1.,0.998389654952317));
#44019=CARTESIAN_POINT('Ctrl Pts',(-1.66846059277231,1.,1.00265091003682));
#44020=CARTESIAN_POINT('Ctrl Pts',(-1.67250335383248,1.,1.00692206696387));
#44021=CARTESIAN_POINT('Ctrl Pts',(-1.67648246776457,1.,1.01123236493507));
#44022=CARTESIAN_POINT('Ctrl Pts',(-1.6804428989482,1.,1.01561026162787));
#44023=CARTESIAN_POINT('Ctrl Pts',(-1.68440578021739,1.,1.02006795074222));
#44024=CARTESIAN_POINT('Ctrl Pts',(-1.68836910178475,1.,1.02460180535272));
#44025=CARTESIAN_POINT('Ctrl Pts',(-1.69231840863471,1.,1.02919977579155));
#44026=CARTESIAN_POINT('Ctrl Pts',(-1.69623414782769,1.,1.03384646003587));
#44027=CARTESIAN_POINT('Ctrl Pts',(-1.70010052930951,1.,1.03852922490782));
#44028=CARTESIAN_POINT('Ctrl Pts',(-1.70391338707969,1.,1.04324363334546));
#44029=CARTESIAN_POINT('Ctrl Pts',(-1.70767646263641,1.,1.0479908540499));
#44030=CARTESIAN_POINT('Ctrl Pts',(-1.71139783543986,1.,1.05277517202854));
#44031=CARTESIAN_POINT('Ctrl Pts',(-1.71508654427022,1.,1.05760163192481));
#44032=CARTESIAN_POINT('Ctrl Pts',(-1.71874858456908,1.,1.0624732468065));
#44033=CARTESIAN_POINT('Ctrl Pts',(-1.72238500928456,1.,1.06738966975463));
#44034=CARTESIAN_POINT('Ctrl Pts',(-1.72599406198489,1.,1.07234866990252));
#44035=CARTESIAN_POINT('Ctrl Pts',(-1.72957248977424,1.,1.0773470373727));
#44036=CARTESIAN_POINT('Ctrl Pts',(-1.73311705663407,1.,1.08238162784749));
#44037=CARTESIAN_POINT('Ctrl Pts',(-1.73662628326093,1.,1.08745056285429));
#44038=CARTESIAN_POINT('Ctrl Pts',(-1.74010053962252,1.,1.09255329056496));
#44039=CARTESIAN_POINT('Ctrl Pts',(-1.74354119236212,1.,1.09768999241229));
#44040=CARTESIAN_POINT('Ctrl Pts',(-1.74695004214924,1.,1.10286118991144));
#44041=CARTESIAN_POINT('Ctrl Pts',(-1.75032866075914,1.,1.10806728183003));
#44042=CARTESIAN_POINT('Ctrl Pts',(-1.75367772094617,1.,1.11330807582542));
#44043=CARTESIAN_POINT('Ctrl Pts',(-1.75699720772089,1.,1.11858293216752));
#44044=CARTESIAN_POINT('Ctrl Pts',(-1.76028671825084,1.,1.12389096855078));
#44045=CARTESIAN_POINT('Ctrl Pts',(-1.76354571966171,1.,1.12923123555076));
#44046=CARTESIAN_POINT('Ctrl Pts',(-1.76677384551883,1.,1.13460291804635));
#44047=CARTESIAN_POINT('Ctrl Pts',(-1.76997111386806,1.,1.14000548337));
#44048=CARTESIAN_POINT('Ctrl Pts',(-1.77313777896234,1.,1.14543858226948));
#44049=CARTESIAN_POINT('Ctrl Pts',(-1.77627422557034,1.,1.15090197841531));
#44050=CARTESIAN_POINT('Ctrl Pts',(-1.77938085564261,1.,1.15639547194689));
#44051=CARTESIAN_POINT('Ctrl Pts',(-1.78245795880949,1.,1.16191881298458));
#44052=CARTESIAN_POINT('Ctrl Pts',(-1.78550566040349,1.,1.16747166312239));
#44053=CARTESIAN_POINT('Ctrl Pts',(-1.78852398877523,1.,1.17305363177265));
#44054=CARTESIAN_POINT('Ctrl Pts',(-1.79151291552646,1.,1.17866429440781));
#44055=CARTESIAN_POINT('Ctrl Pts',(-1.79447240321572,1.,1.18430321697471));
#44056=CARTESIAN_POINT('Ctrl Pts',(-1.79740245923649,1.,1.1899699793456));
#44057=CARTESIAN_POINT('Ctrl Pts',(-1.80030314370121,1.,1.19566418930405));
#44058=CARTESIAN_POINT('Ctrl Pts',(-1.8031745483882,1.,1.2013854893912));
#44059=CARTESIAN_POINT('Ctrl Pts',(-1.80601678480772,1.,1.20713356605519));
#44060=CARTESIAN_POINT('Ctrl Pts',(-1.80882996916931,1.,1.2129081570818));
#44061=CARTESIAN_POINT('Ctrl Pts',(-1.81161420806172,1.,1.2187090610323));
#44062=CARTESIAN_POINT('Ctrl Pts',(-1.81436959209778,1.,1.22453613304507));
#44063=CARTESIAN_POINT('Ctrl Pts',(-1.81655087183054,1.,1.22921864890975));
#44064=CARTESIAN_POINT('Ctrl Pts',(-1.81817389920914,1.,1.23274224526804));
#44065=CARTESIAN_POINT('Ctrl Pts',(-1.81925017193531,1.,1.23509651170384));
#44066=CARTESIAN_POINT('Ctrl Pts',(-1.81978687191668,1.,1.23627494547115));
#44067=CARTESIAN_POINT('',(-1.5055822144029,0.,0.892032620296856));
#44068=CARTESIAN_POINT('Origin',(0.,0.,0.));
#44069=CARTESIAN_POINT('',(-1.60662857109684,1.,0.693717979106305));
#44070=CARTESIAN_POINT('Origin',(0.,1.,0.));
#44071=CARTESIAN_POINT('',(-1.60662857109684,0.,0.693717979106306));
#44072=CARTESIAN_POINT('Ctrl Pts',(-2.0698113262342,-1.,0.7455743247944));
#44073=CARTESIAN_POINT('Ctrl Pts',(-2.0698113262342,1.,0.7455743247944));
#44074=CARTESIAN_POINT('Ctrl Pts',(-2.06854248895728,-1.,0.745832791378367));
#44075=CARTESIAN_POINT('Ctrl Pts',(-2.06854248895728,1.,0.745832791378367));
#44076=CARTESIAN_POINT('Ctrl Pts',(-2.06600523016815,-1.,0.7463458715442));
#44077=CARTESIAN_POINT('Ctrl Pts',(-2.06600523016815,1.,0.7463458715442));
#44078=CARTESIAN_POINT('Ctrl Pts',(-2.06220058927826,-1.,0.747103932787919));
#44079=CARTESIAN_POINT('Ctrl Pts',(-2.06220058927826,1.,0.747103932787919));
#44080=CARTESIAN_POINT('Ctrl Pts',(-2.05713023031006,-1.,0.748091554183802));
#44081=CARTESIAN_POINT('Ctrl Pts',(-2.05713023031006,1.,0.748091554183802));
#44082=CARTESIAN_POINT('Ctrl Pts',(-2.05079645592154,-1.,0.749287468665046));
#44083=CARTESIAN_POINT('Ctrl Pts',(-2.05079645592154,1.,0.749287468665046));
#44084=CARTESIAN_POINT('Ctrl Pts',(-2.04446689147979,-1.,0.750444657875576));
#44085=CARTESIAN_POINT('Ctrl Pts',(-2.04446689147979,1.,0.750444657875576));
#44086=CARTESIAN_POINT('Ctrl Pts',(-2.03814160092099,-1.,0.751562963361115));
#44087=CARTESIAN_POINT('Ctrl Pts',(-2.03814160092099,1.,0.751562963361115));
#44088=CARTESIAN_POINT('Ctrl Pts',(-2.03182068456221,-1.,0.752642180487211));
#44089=CARTESIAN_POINT('Ctrl Pts',(-2.03182068456221,1.,0.752642180487211));
#44090=CARTESIAN_POINT('Ctrl Pts',(-2.02550428623313,-1.,0.753682061112768));
#44091=CARTESIAN_POINT('Ctrl Pts',(-2.02550428623313,1.,0.753682061112768));
#44092=CARTESIAN_POINT('Ctrl Pts',(-2.01919259405809,-1.,0.754682330722816));
#44093=CARTESIAN_POINT('Ctrl Pts',(-2.01919259405809,1.,0.754682330722816));
#44094=CARTESIAN_POINT('Ctrl Pts',(-2.01288584328084,-1.,0.755642704957865));
#44095=CARTESIAN_POINT('Ctrl Pts',(-2.01288584328084,1.,0.755642704957865));
#44096=CARTESIAN_POINT('Ctrl Pts',(-2.0065843158773,-1.,0.75656290464667));
#44097=CARTESIAN_POINT('Ctrl Pts',(-2.0065843158773,1.,0.75656290464667));
#44098=CARTESIAN_POINT('Ctrl Pts',(-2.00028834739178,-1.,0.757442676862724));
#44099=CARTESIAN_POINT('Ctrl Pts',(-2.00028834739178,1.,0.757442676862724));
#44100=CARTESIAN_POINT('Ctrl Pts',(-1.99399831098817,-1.,0.758281796766761));
#44101=CARTESIAN_POINT('Ctrl Pts',(-1.99399831098817,1.,0.758281796766761));
#44102=CARTESIAN_POINT('Ctrl Pts',(-1.98771456680874,-1.,0.759080037802488));
#44103=CARTESIAN_POINT('Ctrl Pts',(-1.98771456680874,1.,0.759080037802488));
#44104=CARTESIAN_POINT('Ctrl Pts',(-1.98143741418172,-1.,0.75983714745219));
#44105=CARTESIAN_POINT('Ctrl Pts',(-1.98143741418172,1.,0.75983714745219));
#44106=CARTESIAN_POINT('Ctrl Pts',(-1.97516705321494,-1.,0.760552825409757));
#44107=CARTESIAN_POINT('Ctrl Pts',(-1.97516705321494,1.,0.760552825409757));
#44108=CARTESIAN_POINT('Ctrl Pts',(-1.96890351582499,-1.,0.76122669048382));
#44109=CARTESIAN_POINT('Ctrl Pts',(-1.96890351582499,1.,0.76122669048382));
#44110=CARTESIAN_POINT('Ctrl Pts',(-1.96264672744186,-1.,0.761858300014423));
#44111=CARTESIAN_POINT('Ctrl Pts',(-1.96264672744186,1.,0.761858300014423));
#44112=CARTESIAN_POINT('Ctrl Pts',(-1.95639665309869,-1.,0.762447203806179));
#44113=CARTESIAN_POINT('Ctrl Pts',(-1.95639665309869,1.,0.762447203806179));
#44114=CARTESIAN_POINT('Ctrl Pts',(-1.95015342590024,-1.,0.762992990878769));
#44115=CARTESIAN_POINT('Ctrl Pts',(-1.95015342590024,1.,0.762992990878769));
#44116=CARTESIAN_POINT('Ctrl Pts',(-1.9439174661764,-1.,0.763495333538629));
#44117=CARTESIAN_POINT('Ctrl Pts',(-1.9439174661764,1.,0.763495333538629));
#44118=CARTESIAN_POINT('Ctrl Pts',(-1.93768964875886,-1.,0.763954049121458));
#44119=CARTESIAN_POINT('Ctrl Pts',(-1.93768964875886,1.,0.763954049121458));
#44120=CARTESIAN_POINT('Ctrl Pts',(-1.93147105496382,-1.,0.76436901067394));
#44121=CARTESIAN_POINT('Ctrl Pts',(-1.93147105496382,1.,0.76436901067394));
#44122=CARTESIAN_POINT('Ctrl Pts',(-1.92526263537048,-1.,0.764740025488211));
#44123=CARTESIAN_POINT('Ctrl Pts',(-1.92526263537048,1.,0.764740025488211));
#44124=CARTESIAN_POINT('Ctrl Pts',(-1.91906491634196,-1.,0.765066729667088));
#44125=CARTESIAN_POINT('Ctrl Pts',(-1.91906491634196,1.,0.765066729667088));
#44126=CARTESIAN_POINT('Ctrl Pts',(-1.91287765805169,-1.,0.765348465884722));
#44127=CARTESIAN_POINT('Ctrl Pts',(-1.91287765805169,1.,0.765348465884722));
#44128=CARTESIAN_POINT('Ctrl Pts',(-1.90669961402356,-1.,0.765584196937919));
#44129=CARTESIAN_POINT('Ctrl Pts',(-1.90669961402356,1.,0.765584196937919));
#44130=CARTESIAN_POINT('Ctrl Pts',(-1.90052930393596,-1.,0.765772772593386));
#44131=CARTESIAN_POINT('Ctrl Pts',(-1.90052930393596,1.,0.765772772593386));
#44132=CARTESIAN_POINT('Ctrl Pts',(-1.89436577771388,-1.,0.765913193856978));
#44133=CARTESIAN_POINT('Ctrl Pts',(-1.89436577771388,1.,0.765913193856978));
#44134=CARTESIAN_POINT('Ctrl Pts',(-1.88820926433409,-1.,0.766004837062091));
#44135=CARTESIAN_POINT('Ctrl Pts',(-1.88820926433409,1.,0.766004837062091));
#44136=CARTESIAN_POINT('Ctrl Pts',(-1.88206215302561,-1.,0.766047794851864));
#44137=CARTESIAN_POINT('Ctrl Pts',(-1.88206215302561,1.,0.766047794851864));
#44138=CARTESIAN_POINT('Ctrl Pts',(-1.87592888967883,-1.,0.766042837036744));
#44139=CARTESIAN_POINT('Ctrl Pts',(-1.87592888967883,1.,0.766042837036744));
#44140=CARTESIAN_POINT('Ctrl Pts',(-1.86981398314341,-1.,0.765990708546091));
#44141=CARTESIAN_POINT('Ctrl Pts',(-1.86981398314341,1.,0.765990708546091));
#44142=CARTESIAN_POINT('Ctrl Pts',(-1.86372027063312,-1.,0.765891519092547));
#44143=CARTESIAN_POINT('Ctrl Pts',(-1.86372027063312,1.,0.765891519092547));
#44144=CARTESIAN_POINT('Ctrl Pts',(-1.85764741390394,-1.,0.765744212909318));
#44145=CARTESIAN_POINT('Ctrl Pts',(-1.85764741390394,1.,0.765744212909318));
#44146=CARTESIAN_POINT('Ctrl Pts',(-1.85158945130063,-1.,0.765545710619062));
#44147=CARTESIAN_POINT('Ctrl Pts',(-1.85158945130063,1.,0.765545710619062));
#44148=CARTESIAN_POINT('Ctrl Pts',(-1.84553698875924,-1.,0.765291664862029));
#44149=CARTESIAN_POINT('Ctrl Pts',(-1.84553698875924,1.,0.765291664862029));
#44150=CARTESIAN_POINT('Ctrl Pts',(-1.83948181064835,-1.,0.764978057881737));
#44151=CARTESIAN_POINT('Ctrl Pts',(-1.83948181064835,1.,0.764978057881737));
#44152=CARTESIAN_POINT('Ctrl Pts',(-1.83342077227142,-1.,0.764602549687853));
#44153=CARTESIAN_POINT('Ctrl Pts',(-1.83342077227142,1.,0.764602549687853));
#44154=CARTESIAN_POINT('Ctrl Pts',(-1.82735991200065,-1.,0.764165902605995));
#44155=CARTESIAN_POINT('Ctrl Pts',(-1.82735991200065,1.,0.764165902605995));
#44156=CARTESIAN_POINT('Ctrl Pts',(-1.82131873145266,-1.,0.763673465462726));
#44157=CARTESIAN_POINT('Ctrl Pts',(-1.82131873145266,1.,0.763673465462726));
#44158=CARTESIAN_POINT('Ctrl Pts',(-1.8153211840553,-1.,0.763132003836634));
#44159=CARTESIAN_POINT('Ctrl Pts',(-1.8153211840553,1.,0.763132003836634));
#44160=CARTESIAN_POINT('Ctrl Pts',(-1.80938551463965,-1.,0.762546129463938));
#44161=CARTESIAN_POINT('Ctrl Pts',(-1.80938551463965,1.,0.762546129463938));
#44162=CARTESIAN_POINT('Ctrl Pts',(-1.80351583877342,-1.,0.761915336443547));
#44163=CARTESIAN_POINT('Ctrl Pts',(-1.80351583877342,1.,0.761915336443547));
#44164=CARTESIAN_POINT('Ctrl Pts',(-1.79768986997783,-1.,0.761229695230558));
#44165=CARTESIAN_POINT('Ctrl Pts',(-1.79768986997783,1.,0.761229695230558));
#44166=CARTESIAN_POINT('Ctrl Pts',(-1.7918581561088,-1.,0.760469555880749));
#44167=CARTESIAN_POINT('Ctrl Pts',(-1.7918581561088,1.,0.760469555880749));
#44168=CARTESIAN_POINT('Ctrl Pts',(-1.78596964884604,-1.,0.759614401110189));
#44169=CARTESIAN_POINT('Ctrl Pts',(-1.78596964884604,1.,0.759614401110189));
#44170=CARTESIAN_POINT('Ctrl Pts',(-1.77999411220945,-1.,0.758650626677518));
#44171=CARTESIAN_POINT('Ctrl Pts',(-1.77999411220945,1.,0.758650626677518));
#44172=CARTESIAN_POINT('Ctrl Pts',(-1.77394167108292,-1.,0.757578264077029));
#44173=CARTESIAN_POINT('Ctrl Pts',(-1.77394167108292,1.,0.757578264077029));
#44174=CARTESIAN_POINT('Ctrl Pts',(-1.76789396002998,-1.,0.75642189602781));
#44175=CARTESIAN_POINT('Ctrl Pts',(-1.76789396002998,1.,0.75642189602781));
#44176=CARTESIAN_POINT('Ctrl Pts',(-1.76197817240128,-1.,0.755220979974461));
#44177=CARTESIAN_POINT('Ctrl Pts',(-1.76197817240128,1.,0.755220979974461));
#44178=CARTESIAN_POINT('Ctrl Pts',(-1.75631083600019,-1.,0.754009254027829));
#44179=CARTESIAN_POINT('Ctrl Pts',(-1.75631083600019,1.,0.754009254027829));
#44180=CARTESIAN_POINT('Ctrl Pts',(-1.75095139468794,-1.,0.752797683531314));
#44181=CARTESIAN_POINT('Ctrl Pts',(-1.75095139468794,1.,0.752797683531314));
#44182=CARTESIAN_POINT('Ctrl Pts',(-1.74585086852502,-1.,0.751555614164482));
#44183=CARTESIAN_POINT('Ctrl Pts',(-1.74585086852502,1.,0.751555614164482));
#44184=CARTESIAN_POINT('Ctrl Pts',(-1.74080458267114,-1.,0.750193435981249));
#44185=CARTESIAN_POINT('Ctrl Pts',(-1.74080458267114,1.,0.750193435981249));
#44186=CARTESIAN_POINT('Ctrl Pts',(-1.7355035168033,-1.,0.74858246295687));
#44187=CARTESIAN_POINT('Ctrl Pts',(-1.7355035168033,1.,0.74858246295687));
#44188=CARTESIAN_POINT('Ctrl Pts',(-1.72958533647714,-1.,0.746574710097752));
#44189=CARTESIAN_POINT('Ctrl Pts',(-1.72958533647714,1.,0.746574710097752));
#44190=CARTESIAN_POINT('Ctrl Pts',(-1.72268229916769,-1.,0.744021445433093));
#44191=CARTESIAN_POINT('Ctrl Pts',(-1.72268229916769,1.,0.744021445433093));
#44192=CARTESIAN_POINT('Ctrl Pts',(-1.71447789751001,-1.,0.74079516202821));
#44193=CARTESIAN_POINT('Ctrl Pts',(-1.71447789751001,1.,0.74079516202821));
#44194=CARTESIAN_POINT('Ctrl Pts',(-1.70473309004249,-1.,0.736799665716932));
#44195=CARTESIAN_POINT('Ctrl Pts',(-1.70473309004249,1.,0.736799665716932));
#44196=CARTESIAN_POINT('Ctrl Pts',(-1.69326921972915,-1.,0.731963238685357));
#44197=CARTESIAN_POINT('Ctrl Pts',(-1.69326921972915,1.,0.731963238685357));
#44198=CARTESIAN_POINT('Ctrl Pts',(-1.67996158451922,-1.,0.726235967982445));
#44199=CARTESIAN_POINT('Ctrl Pts',(-1.67996158451922,1.,0.726235967982445));
#44200=CARTESIAN_POINT('Ctrl Pts',(-1.66472880551777,-1.,0.71958543378795));
#44201=CARTESIAN_POINT('Ctrl Pts',(-1.66472880551777,1.,0.71958543378795));
#44202=CARTESIAN_POINT('Ctrl Pts',(-1.64752408828442,-1.,0.711993139340447));
#44203=CARTESIAN_POINT('Ctrl Pts',(-1.64752408828442,1.,0.711993139340447));
#44204=CARTESIAN_POINT('Ctrl Pts',(-1.6321654166204,-1.,0.705159151977294));
#44205=CARTESIAN_POINT('Ctrl Pts',(-1.6321654166204,1.,0.705159151977294));
#44206=CARTESIAN_POINT('Ctrl Pts',(-1.61974673471117,-1.,0.699605146398837));
#44207=CARTESIAN_POINT('Ctrl Pts',(-1.61974673471117,1.,0.699605146398837));
#44208=CARTESIAN_POINT('Ctrl Pts',(-1.61106790957619,-1.,0.69571209787897));
#44209=CARTESIAN_POINT('Ctrl Pts',(-1.61106790957619,1.,0.69571209787897));
#44210=CARTESIAN_POINT('Ctrl Pts',(-1.60662857109684,-1.,0.693717979106305));
#44211=CARTESIAN_POINT('Ctrl Pts',(-1.60662857109684,1.,0.693717979106305));
#44212=CARTESIAN_POINT('',(-2.0698113262342,1.,0.7455743247944));
#44213=CARTESIAN_POINT('Ctrl Pts',(-2.0698113262342,1.,0.7455743247944));
#44214=CARTESIAN_POINT('Ctrl Pts',(-2.06854248895728,1.,0.745832791378367));
#44215=CARTESIAN_POINT('Ctrl Pts',(-2.06600523016815,1.,0.7463458715442));
#44216=CARTESIAN_POINT('Ctrl Pts',(-2.06220058927826,1.,0.747103932787919));
#44217=CARTESIAN_POINT('Ctrl Pts',(-2.05713023031006,1.,0.748091554183802));
#44218=CARTESIAN_POINT('Ctrl Pts',(-2.05079645592154,1.,0.749287468665046));
#44219=CARTESIAN_POINT('Ctrl Pts',(-2.04446689147979,1.,0.750444657875576));
#44220=CARTESIAN_POINT('Ctrl Pts',(-2.03814160092099,1.,0.751562963361115));
#44221=CARTESIAN_POINT('Ctrl Pts',(-2.03182068456221,1.,0.752642180487211));
#44222=CARTESIAN_POINT('Ctrl Pts',(-2.02550428623313,1.,0.753682061112768));
#44223=CARTESIAN_POINT('Ctrl Pts',(-2.01919259405809,1.,0.754682330722816));
#44224=CARTESIAN_POINT('Ctrl Pts',(-2.01288584328084,1.,0.755642704957865));
#44225=CARTESIAN_POINT('Ctrl Pts',(-2.0065843158773,1.,0.75656290464667));
#44226=CARTESIAN_POINT('Ctrl Pts',(-2.00028834739178,1.,0.757442676862724));
#44227=CARTESIAN_POINT('Ctrl Pts',(-1.99399831098817,1.,0.758281796766761));
#44228=CARTESIAN_POINT('Ctrl Pts',(-1.98771456680874,1.,0.759080037802488));
#44229=CARTESIAN_POINT('Ctrl Pts',(-1.98143741418172,1.,0.75983714745219));
#44230=CARTESIAN_POINT('Ctrl Pts',(-1.97516705321494,1.,0.760552825409757));
#44231=CARTESIAN_POINT('Ctrl Pts',(-1.96890351582499,1.,0.76122669048382));
#44232=CARTESIAN_POINT('Ctrl Pts',(-1.96264672744186,1.,0.761858300014423));
#44233=CARTESIAN_POINT('Ctrl Pts',(-1.95639665309869,1.,0.762447203806179));
#44234=CARTESIAN_POINT('Ctrl Pts',(-1.95015342590024,1.,0.762992990878769));
#44235=CARTESIAN_POINT('Ctrl Pts',(-1.9439174661764,1.,0.763495333538629));
#44236=CARTESIAN_POINT('Ctrl Pts',(-1.93768964875886,1.,0.763954049121458));
#44237=CARTESIAN_POINT('Ctrl Pts',(-1.93147105496382,1.,0.76436901067394));
#44238=CARTESIAN_POINT('Ctrl Pts',(-1.92526263537048,1.,0.764740025488211));
#44239=CARTESIAN_POINT('Ctrl Pts',(-1.91906491634196,1.,0.765066729667088));
#44240=CARTESIAN_POINT('Ctrl Pts',(-1.91287765805169,1.,0.765348465884722));
#44241=CARTESIAN_POINT('Ctrl Pts',(-1.90669961402356,1.,0.765584196937919));
#44242=CARTESIAN_POINT('Ctrl Pts',(-1.90052930393596,1.,0.765772772593386));
#44243=CARTESIAN_POINT('Ctrl Pts',(-1.89436577771388,1.,0.765913193856978));
#44244=CARTESIAN_POINT('Ctrl Pts',(-1.88820926433409,1.,0.766004837062091));
#44245=CARTESIAN_POINT('Ctrl Pts',(-1.88206215302561,1.,0.766047794851864));
#44246=CARTESIAN_POINT('Ctrl Pts',(-1.87592888967883,1.,0.766042837036744));
#44247=CARTESIAN_POINT('Ctrl Pts',(-1.86981398314341,1.,0.765990708546091));
#44248=CARTESIAN_POINT('Ctrl Pts',(-1.86372027063312,1.,0.765891519092547));
#44249=CARTESIAN_POINT('Ctrl Pts',(-1.85764741390394,1.,0.765744212909318));
#44250=CARTESIAN_POINT('Ctrl Pts',(-1.85158945130063,1.,0.765545710619062));
#44251=CARTESIAN_POINT('Ctrl Pts',(-1.84553698875924,1.,0.765291664862029));
#44252=CARTESIAN_POINT('Ctrl Pts',(-1.83948181064835,1.,0.764978057881737));
#44253=CARTESIAN_POINT('Ctrl Pts',(-1.83342077227142,1.,0.764602549687853));
#44254=CARTESIAN_POINT('Ctrl Pts',(-1.82735991200065,1.,0.764165902605995));
#44255=CARTESIAN_POINT('Ctrl Pts',(-1.82131873145266,1.,0.763673465462726));
#44256=CARTESIAN_POINT('Ctrl Pts',(-1.8153211840553,1.,0.763132003836634));
#44257=CARTESIAN_POINT('Ctrl Pts',(-1.80938551463965,1.,0.762546129463938));
#44258=CARTESIAN_POINT('Ctrl Pts',(-1.80351583877342,1.,0.761915336443547));
#44259=CARTESIAN_POINT('Ctrl Pts',(-1.79768986997783,1.,0.761229695230558));
#44260=CARTESIAN_POINT('Ctrl Pts',(-1.7918581561088,1.,0.760469555880749));
#44261=CARTESIAN_POINT('Ctrl Pts',(-1.78596964884604,1.,0.759614401110189));
#44262=CARTESIAN_POINT('Ctrl Pts',(-1.77999411220945,1.,0.758650626677518));
#44263=CARTESIAN_POINT('Ctrl Pts',(-1.77394167108292,1.,0.757578264077029));
#44264=CARTESIAN_POINT('Ctrl Pts',(-1.76789396002998,1.,0.75642189602781));
#44265=CARTESIAN_POINT('Ctrl Pts',(-1.76197817240128,1.,0.755220979974461));
#44266=CARTESIAN_POINT('Ctrl Pts',(-1.75631083600019,1.,0.754009254027829));
#44267=CARTESIAN_POINT('Ctrl Pts',(-1.75095139468794,1.,0.752797683531314));
#44268=CARTESIAN_POINT('Ctrl Pts',(-1.74585086852502,1.,0.751555614164482));
#44269=CARTESIAN_POINT('Ctrl Pts',(-1.74080458267114,1.,0.750193435981249));
#44270=CARTESIAN_POINT('Ctrl Pts',(-1.7355035168033,1.,0.74858246295687));
#44271=CARTESIAN_POINT('Ctrl Pts',(-1.72958533647714,1.,0.746574710097752));
#44272=CARTESIAN_POINT('Ctrl Pts',(-1.72268229916769,1.,0.744021445433093));
#44273=CARTESIAN_POINT('Ctrl Pts',(-1.71447789751001,1.,0.74079516202821));
#44274=CARTESIAN_POINT('Ctrl Pts',(-1.70473309004249,1.,0.736799665716932));
#44275=CARTESIAN_POINT('Ctrl Pts',(-1.69326921972915,1.,0.731963238685357));
#44276=CARTESIAN_POINT('Ctrl Pts',(-1.67996158451922,1.,0.726235967982445));
#44277=CARTESIAN_POINT('Ctrl Pts',(-1.66472880551777,1.,0.71958543378795));
#44278=CARTESIAN_POINT('Ctrl Pts',(-1.64752408828442,1.,0.711993139340447));
#44279=CARTESIAN_POINT('Ctrl Pts',(-1.6321654166204,1.,0.705159151977294));
#44280=CARTESIAN_POINT('Ctrl Pts',(-1.61974673471117,1.,0.699605146398837));
#44281=CARTESIAN_POINT('Ctrl Pts',(-1.61106790957619,1.,0.69571209787897));
#44282=CARTESIAN_POINT('Ctrl Pts',(-1.60662857109684,1.,0.693717979106305));
#44283=CARTESIAN_POINT('',(-2.0698113262342,0.,0.7455743247944));
#44284=CARTESIAN_POINT('Origin',(-2.11275013067528,0.,0.61342227326009));
#44285=CARTESIAN_POINT('',(-2.11275013067528,1.,0.61342227326009));
#44286=CARTESIAN_POINT('',(-2.0698113262342,1.,0.7455743247944));
#44287=CARTESIAN_POINT('',(-2.11275013067528,0.,0.61342227326009));
#44288=CARTESIAN_POINT('Ctrl Pts',(-1.7075470150345,-1.,0.383122945602004));
#44289=CARTESIAN_POINT('Ctrl Pts',(-1.7075470150345,1.,0.383122945602004));
#44290=CARTESIAN_POINT('Ctrl Pts',(-1.71231062891958,-1.,0.384119047315542));
#44291=CARTESIAN_POINT('Ctrl Pts',(-1.71231062891958,1.,0.384119047315542));
#44292=CARTESIAN_POINT('Ctrl Pts',(-1.72162022246158,-1.,0.38607079032701));
#44293=CARTESIAN_POINT('Ctrl Pts',(-1.72162022246158,1.,0.38607079032701));
#44294=CARTESIAN_POINT('Ctrl Pts',(-1.7349317097561,-1.,0.388877023509191));
#44295=CARTESIAN_POINT('Ctrl Pts',(-1.7349317097561,1.,0.388877023509191));
#44296=CARTESIAN_POINT('Ctrl Pts',(-1.75137405313962,-1.,0.392375812294307));
#44297=CARTESIAN_POINT('Ctrl Pts',(-1.75137405313962,1.,0.392375812294307));
#44298=CARTESIAN_POINT('Ctrl Pts',(-1.7697556004756,-1.,0.39634619612042));
#44299=CARTESIAN_POINT('Ctrl Pts',(-1.7697556004756,1.,0.39634619612042));
#44300=CARTESIAN_POINT('Ctrl Pts',(-1.78598826347533,-1.,0.39991940378308));
#44301=CARTESIAN_POINT('Ctrl Pts',(-1.78598826347533,1.,0.39991940378308));
#44302=CARTESIAN_POINT('Ctrl Pts',(-1.80012077176221,-1.,0.403107976170441));
#44303=CARTESIAN_POINT('Ctrl Pts',(-1.80012077176221,1.,0.403107976170441));
#44304=CARTESIAN_POINT('Ctrl Pts',(-1.81223801813988,-1.,0.405933518411838));
#44305=CARTESIAN_POINT('Ctrl Pts',(-1.81223801813988,1.,0.405933518411838));
#44306=CARTESIAN_POINT('Ctrl Pts',(-1.8224702267854,-1.,0.408428948108533));
#44307=CARTESIAN_POINT('Ctrl Pts',(-1.8224702267854,1.,0.408428948108533));
#44308=CARTESIAN_POINT('Ctrl Pts',(-1.83100408895216,-1.,0.410641256301675));
#44309=CARTESIAN_POINT('Ctrl Pts',(-1.83100408895216,1.,0.410641256301675));
#44310=CARTESIAN_POINT('Ctrl Pts',(-1.83808953475839,-1.,0.412633125322161));
#44311=CARTESIAN_POINT('Ctrl Pts',(-1.83808953475839,1.,0.412633125322161));
#44312=CARTESIAN_POINT('Ctrl Pts',(-1.8440575707371,-1.,0.41448743825434));
#44313=CARTESIAN_POINT('Ctrl Pts',(-1.8440575707371,1.,0.41448743825434));
#44314=CARTESIAN_POINT('Ctrl Pts',(-1.84929312929882,-1.,0.416300022038864));
#44315=CARTESIAN_POINT('Ctrl Pts',(-1.84929312929882,1.,0.416300022038864));
#44316=CARTESIAN_POINT('Ctrl Pts',(-1.85417632856234,-1.,0.418164129143534));
#44317=CARTESIAN_POINT('Ctrl Pts',(-1.85417632856234,1.,0.418164129143534));
#44318=CARTESIAN_POINT('Ctrl Pts',(-1.85903281096686,-1.,0.420157287975619));
#44319=CARTESIAN_POINT('Ctrl Pts',(-1.85903281096686,1.,0.420157287975619));
#44320=CARTESIAN_POINT('Ctrl Pts',(-1.86408083334028,-1.,0.422327307418275));
#44321=CARTESIAN_POINT('Ctrl Pts',(-1.86408083334028,1.,0.422327307418275));
#44322=CARTESIAN_POINT('Ctrl Pts',(-1.86937803944323,-1.,0.424678177291359));
#44323=CARTESIAN_POINT('Ctrl Pts',(-1.86937803944323,1.,0.424678177291359));
#44324=CARTESIAN_POINT('Ctrl Pts',(-1.87486989291484,-1.,0.427183828519102));
#44325=CARTESIAN_POINT('Ctrl Pts',(-1.87486989291484,1.,0.427183828519102));
#44326=CARTESIAN_POINT('Ctrl Pts',(-1.88044229001832,-1.,0.429803062482344));
#44327=CARTESIAN_POINT('Ctrl Pts',(-1.88044229001832,1.,0.429803062482344));
#44328=CARTESIAN_POINT('Ctrl Pts',(-1.88596913666793,-1.,0.432493038548748));
#44329=CARTESIAN_POINT('Ctrl Pts',(-1.88596913666793,1.,0.432493038548748));
#44330=CARTESIAN_POINT('Ctrl Pts',(-1.89136993975504,-1.,0.435225660963383));
#44331=CARTESIAN_POINT('Ctrl Pts',(-1.89136993975504,1.,0.435225660963383));
#44332=CARTESIAN_POINT('Ctrl Pts',(-1.89663648956466,-1.,0.437995003948244));
#44333=CARTESIAN_POINT('Ctrl Pts',(-1.89663648956466,1.,0.437995003948244));
#44334=CARTESIAN_POINT('Ctrl Pts',(-1.90180124389086,-1.,0.440807833704038));
#44335=CARTESIAN_POINT('Ctrl Pts',(-1.90180124389086,1.,0.440807833704038));
#44336=CARTESIAN_POINT('Ctrl Pts',(-1.90691756144898,-1.,0.44367755684915));
#44337=CARTESIAN_POINT('Ctrl Pts',(-1.90691756144898,1.,0.44367755684915));
#44338=CARTESIAN_POINT('Ctrl Pts',(-1.9120369998112,-1.,0.446617343485711));
#44339=CARTESIAN_POINT('Ctrl Pts',(-1.9120369998112,1.,0.446617343485711));
#44340=CARTESIAN_POINT('Ctrl Pts',(-1.91718342555755,-1.,0.449632260106662));
#44341=CARTESIAN_POINT('Ctrl Pts',(-1.91718342555755,1.,0.449632260106662));
#44342=CARTESIAN_POINT('Ctrl Pts',(-1.92235380648502,-1.,0.452719478359432));
#44343=CARTESIAN_POINT('Ctrl Pts',(-1.92235380648502,1.,0.452719478359432));
#44344=CARTESIAN_POINT('Ctrl Pts',(-1.92753067150476,-1.,0.455872005174371));
#44345=CARTESIAN_POINT('Ctrl Pts',(-1.92753067150476,1.,0.455872005174371));
#44346=CARTESIAN_POINT('Ctrl Pts',(-1.93269066517934,-1.,0.459081234547926));
#44347=CARTESIAN_POINT('Ctrl Pts',(-1.93269066517934,1.,0.459081234547926));
#44348=CARTESIAN_POINT('Ctrl Pts',(-1.93781486640821,-1.,0.462340031009056));
#44349=CARTESIAN_POINT('Ctrl Pts',(-1.93781486640821,1.,0.462340031009056));
#44350=CARTESIAN_POINT('Ctrl Pts',(-1.9428979419619,-1.,0.46564546202603));
#44351=CARTESIAN_POINT('Ctrl Pts',(-1.9428979419619,1.,0.46564546202603));
#44352=CARTESIAN_POINT('Ctrl Pts',(-1.94794381136514,-1.,0.468997482913135));
#44353=CARTESIAN_POINT('Ctrl Pts',(-1.94794381136514,1.,0.468997482913135));
#44354=CARTESIAN_POINT('Ctrl Pts',(-1.95296148278133,-1.,0.472397672264072));
#44355=CARTESIAN_POINT('Ctrl Pts',(-1.95296148278133,1.,0.472397672264072));
#44356=CARTESIAN_POINT('Ctrl Pts',(-1.95796111148177,-1.,0.475848034683176));
#44357=CARTESIAN_POINT('Ctrl Pts',(-1.95796111148177,1.,0.475848034683176));
#44358=CARTESIAN_POINT('Ctrl Pts',(-1.96294933055943,-1.,0.479349583074855));
#44359=CARTESIAN_POINT('Ctrl Pts',(-1.96294933055943,1.,0.479349583074855));
#44360=CARTESIAN_POINT('Ctrl Pts',(-1.96792703422362,-1.,0.48290166212069));
#44361=CARTESIAN_POINT('Ctrl Pts',(-1.96792703422362,1.,0.48290166212069));
#44362=CARTESIAN_POINT('Ctrl Pts',(-1.97289186263272,-1.,0.486502692907659));
#44363=CARTESIAN_POINT('Ctrl Pts',(-1.97289186263272,1.,0.486502692907659));
#44364=CARTESIAN_POINT('Ctrl Pts',(-1.97783973019229,-1.,0.490150627860952));
#44365=CARTESIAN_POINT('Ctrl Pts',(-1.97783973019229,1.,0.490150627860952));
#44366=CARTESIAN_POINT('Ctrl Pts',(-1.98276658761821,-1.,0.493843476541494));
#44367=CARTESIAN_POINT('Ctrl Pts',(-1.98276658761821,1.,0.493843476541494));
#44368=CARTESIAN_POINT('Ctrl Pts',(-1.98767044752932,-1.,0.497579909545574));
#44369=CARTESIAN_POINT('Ctrl Pts',(-1.98767044752932,1.,0.497579909545574));
#44370=CARTESIAN_POINT('Ctrl Pts',(-1.99255149126155,-1.,0.501359287727146));
#44371=CARTESIAN_POINT('Ctrl Pts',(-1.99255149126155,1.,0.501359287727146));
#44372=CARTESIAN_POINT('Ctrl Pts',(-1.99741107463572,-1.,0.505181361323026));
#44373=CARTESIAN_POINT('Ctrl Pts',(-1.99741107463572,1.,0.505181361323026));
#44374=CARTESIAN_POINT('Ctrl Pts',(-2.00225107134734,-1.,0.509046069886157));
#44375=CARTESIAN_POINT('Ctrl Pts',(-2.00225107134734,1.,0.509046069886157));
#44376=CARTESIAN_POINT('Ctrl Pts',(-2.00707309946949,-1.,0.512953306961792));
#44377=CARTESIAN_POINT('Ctrl Pts',(-2.00707309946949,1.,0.512953306961792));
#44378=CARTESIAN_POINT('Ctrl Pts',(-2.01187773939242,-1.,0.516902681728687));
#44379=CARTESIAN_POINT('Ctrl Pts',(-2.01187773939242,1.,0.516902681728687));
#44380=CARTESIAN_POINT('Ctrl Pts',(-2.01666477917286,-1.,0.52089359039937));
#44381=CARTESIAN_POINT('Ctrl Pts',(-2.01666477917286,1.,0.52089359039937));
#44382=CARTESIAN_POINT('Ctrl Pts',(-2.02143356304698,-1.,0.524925318333476));
#44383=CARTESIAN_POINT('Ctrl Pts',(-2.02143356304698,1.,0.524925318333476));
#44384=CARTESIAN_POINT('Ctrl Pts',(-2.0261832908329,-1.,0.528997127241914));
#44385=CARTESIAN_POINT('Ctrl Pts',(-2.0261832908329,1.,0.528997127241914));
#44386=CARTESIAN_POINT('Ctrl Pts',(-2.03091336214426,-1.,0.533108355132976));
#44387=CARTESIAN_POINT('Ctrl Pts',(-2.03091336214426,1.,0.533108355132976));
#44388=CARTESIAN_POINT('Ctrl Pts',(-2.03562362954037,-1.,0.537258489833262));
#44389=CARTESIAN_POINT('Ctrl Pts',(-2.03562362954037,1.,0.537258489833262));
#44390=CARTESIAN_POINT('Ctrl Pts',(-2.04031422690527,-1.,0.541447120615659));
#44391=CARTESIAN_POINT('Ctrl Pts',(-2.04031422690527,1.,0.541447120615659));
#44392=CARTESIAN_POINT('Ctrl Pts',(-2.04498544714588,-1.,0.54567390381743));
#44393=CARTESIAN_POINT('Ctrl Pts',(-2.04498544714588,1.,0.54567390381743));
#44394=CARTESIAN_POINT('Ctrl Pts',(-2.04963761077958,-1.,0.549938525150295));
#44395=CARTESIAN_POINT('Ctrl Pts',(-2.04963761077958,1.,0.549938525150295));
#44396=CARTESIAN_POINT('Ctrl Pts',(-2.05427091604413,-1.,0.554240657463906));
#44397=CARTESIAN_POINT('Ctrl Pts',(-2.05427091604413,1.,0.554240657463906));
#44398=CARTESIAN_POINT('Ctrl Pts',(-2.05888537756462,-1.,0.558579940185151));
#44399=CARTESIAN_POINT('Ctrl Pts',(-2.05888537756462,1.,0.558579940185151));
#44400=CARTESIAN_POINT('Ctrl Pts',(-2.06348090160589,-1.,0.562955993082261));
#44401=CARTESIAN_POINT('Ctrl Pts',(-2.06348090160589,1.,0.562955993082261));
#44402=CARTESIAN_POINT('Ctrl Pts',(-2.06805732997334,-1.,0.567368421181087));
#44403=CARTESIAN_POINT('Ctrl Pts',(-2.06805732997334,1.,0.567368421181087));
#44404=CARTESIAN_POINT('Ctrl Pts',(-2.07261449292824,-1.,0.571816823242603));
#44405=CARTESIAN_POINT('Ctrl Pts',(-2.07261449292824,1.,0.571816823242603));
#44406=CARTESIAN_POINT('Ctrl Pts',(-2.07715226767559,-1.,0.576300797416844));
#44407=CARTESIAN_POINT('Ctrl Pts',(-2.07715226767559,1.,0.576300797416844));
#44408=CARTESIAN_POINT('Ctrl Pts',(-2.08167059018418,-1.,0.580819952108063));
#44409=CARTESIAN_POINT('Ctrl Pts',(-2.08167059018418,1.,0.580819952108063));
#44410=CARTESIAN_POINT('Ctrl Pts',(-2.08616943727951,-1.,0.585373918991617));
#44411=CARTESIAN_POINT('Ctrl Pts',(-2.08616943727951,1.,0.585373918991617));
#44412=CARTESIAN_POINT('Ctrl Pts',(-2.09064881812129,-1.,0.589962365403406));
#44413=CARTESIAN_POINT('Ctrl Pts',(-2.09064881812129,1.,0.589962365403406));
#44414=CARTESIAN_POINT('Ctrl Pts',(-2.0951087622027,-1.,0.594585006052162));
#44415=CARTESIAN_POINT('Ctrl Pts',(-2.0951087622027,1.,0.594585006052162));
#44416=CARTESIAN_POINT('Ctrl Pts',(-2.0995493086477,-1.,0.599241616420533));
#44417=CARTESIAN_POINT('Ctrl Pts',(-2.0995493086477,1.,0.599241616420533));
#44418=CARTESIAN_POINT('Ctrl Pts',(-2.10397049886949,-1.,0.60393203073603));
#44419=CARTESIAN_POINT('Ctrl Pts',(-2.10397049886949,1.,0.60393203073603));
#44420=CARTESIAN_POINT('Ctrl Pts',(-2.1074919961518,-1.,0.607711315454876));
#44421=CARTESIAN_POINT('Ctrl Pts',(-2.1074919961518,1.,0.607711315454876));
#44422=CARTESIAN_POINT('Ctrl Pts',(-2.11012443807238,-1.,0.610560911689899));
#44423=CARTESIAN_POINT('Ctrl Pts',(-2.11012443807238,1.,0.610560911689899));
#44424=CARTESIAN_POINT('Ctrl Pts',(-2.11187554259986,-1.,0.6124673655618));
#44425=CARTESIAN_POINT('Ctrl Pts',(-2.11187554259986,1.,0.6124673655618));
#44426=CARTESIAN_POINT('Ctrl Pts',(-2.11275013067528,-1.,0.61342227326009));
#44427=CARTESIAN_POINT('Ctrl Pts',(-2.11275013067528,1.,0.61342227326009));
#44428=CARTESIAN_POINT('',(-1.7075470150345,1.,0.383122945602004));
#44429=CARTESIAN_POINT('Ctrl Pts',(-1.7075470150345,1.,0.383122945602004));
#44430=CARTESIAN_POINT('Ctrl Pts',(-1.71231062891958,1.,0.384119047315542));
#44431=CARTESIAN_POINT('Ctrl Pts',(-1.72162022246158,1.,0.38607079032701));
#44432=CARTESIAN_POINT('Ctrl Pts',(-1.7349317097561,1.,0.388877023509191));
#44433=CARTESIAN_POINT('Ctrl Pts',(-1.75137405313962,1.,0.392375812294307));
#44434=CARTESIAN_POINT('Ctrl Pts',(-1.7697556004756,1.,0.39634619612042));
#44435=CARTESIAN_POINT('Ctrl Pts',(-1.78598826347533,1.,0.39991940378308));
#44436=CARTESIAN_POINT('Ctrl Pts',(-1.80012077176221,1.,0.403107976170441));
#44437=CARTESIAN_POINT('Ctrl Pts',(-1.81223801813988,1.,0.405933518411838));
#44438=CARTESIAN_POINT('Ctrl Pts',(-1.8224702267854,1.,0.408428948108533));
#44439=CARTESIAN_POINT('Ctrl Pts',(-1.83100408895216,1.,0.410641256301675));
#44440=CARTESIAN_POINT('Ctrl Pts',(-1.83808953475839,1.,0.412633125322161));
#44441=CARTESIAN_POINT('Ctrl Pts',(-1.8440575707371,1.,0.41448743825434));
#44442=CARTESIAN_POINT('Ctrl Pts',(-1.84929312929882,1.,0.416300022038864));
#44443=CARTESIAN_POINT('Ctrl Pts',(-1.85417632856234,1.,0.418164129143534));
#44444=CARTESIAN_POINT('Ctrl Pts',(-1.85903281096686,1.,0.420157287975619));
#44445=CARTESIAN_POINT('Ctrl Pts',(-1.86408083334028,1.,0.422327307418275));
#44446=CARTESIAN_POINT('Ctrl Pts',(-1.86937803944323,1.,0.424678177291359));
#44447=CARTESIAN_POINT('Ctrl Pts',(-1.87486989291484,1.,0.427183828519102));
#44448=CARTESIAN_POINT('Ctrl Pts',(-1.88044229001832,1.,0.429803062482344));
#44449=CARTESIAN_POINT('Ctrl Pts',(-1.88596913666793,1.,0.432493038548748));
#44450=CARTESIAN_POINT('Ctrl Pts',(-1.89136993975504,1.,0.435225660963383));
#44451=CARTESIAN_POINT('Ctrl Pts',(-1.89663648956466,1.,0.437995003948244));
#44452=CARTESIAN_POINT('Ctrl Pts',(-1.90180124389086,1.,0.440807833704038));
#44453=CARTESIAN_POINT('Ctrl Pts',(-1.90691756144898,1.,0.44367755684915));
#44454=CARTESIAN_POINT('Ctrl Pts',(-1.9120369998112,1.,0.446617343485711));
#44455=CARTESIAN_POINT('Ctrl Pts',(-1.91718342555755,1.,0.449632260106662));
#44456=CARTESIAN_POINT('Ctrl Pts',(-1.92235380648502,1.,0.452719478359432));
#44457=CARTESIAN_POINT('Ctrl Pts',(-1.92753067150476,1.,0.455872005174371));
#44458=CARTESIAN_POINT('Ctrl Pts',(-1.93269066517934,1.,0.459081234547926));
#44459=CARTESIAN_POINT('Ctrl Pts',(-1.93781486640821,1.,0.462340031009056));
#44460=CARTESIAN_POINT('Ctrl Pts',(-1.9428979419619,1.,0.46564546202603));
#44461=CARTESIAN_POINT('Ctrl Pts',(-1.94794381136514,1.,0.468997482913135));
#44462=CARTESIAN_POINT('Ctrl Pts',(-1.95296148278133,1.,0.472397672264072));
#44463=CARTESIAN_POINT('Ctrl Pts',(-1.95796111148177,1.,0.475848034683176));
#44464=CARTESIAN_POINT('Ctrl Pts',(-1.96294933055943,1.,0.479349583074855));
#44465=CARTESIAN_POINT('Ctrl Pts',(-1.96792703422362,1.,0.48290166212069));
#44466=CARTESIAN_POINT('Ctrl Pts',(-1.97289186263272,1.,0.486502692907659));
#44467=CARTESIAN_POINT('Ctrl Pts',(-1.97783973019229,1.,0.490150627860952));
#44468=CARTESIAN_POINT('Ctrl Pts',(-1.98276658761821,1.,0.493843476541494));
#44469=CARTESIAN_POINT('Ctrl Pts',(-1.98767044752932,1.,0.497579909545574));
#44470=CARTESIAN_POINT('Ctrl Pts',(-1.99255149126155,1.,0.501359287727146));
#44471=CARTESIAN_POINT('Ctrl Pts',(-1.99741107463572,1.,0.505181361323026));
#44472=CARTESIAN_POINT('Ctrl Pts',(-2.00225107134734,1.,0.509046069886157));
#44473=CARTESIAN_POINT('Ctrl Pts',(-2.00707309946949,1.,0.512953306961792));
#44474=CARTESIAN_POINT('Ctrl Pts',(-2.01187773939242,1.,0.516902681728687));
#44475=CARTESIAN_POINT('Ctrl Pts',(-2.01666477917286,1.,0.52089359039937));
#44476=CARTESIAN_POINT('Ctrl Pts',(-2.02143356304698,1.,0.524925318333476));
#44477=CARTESIAN_POINT('Ctrl Pts',(-2.0261832908329,1.,0.528997127241914));
#44478=CARTESIAN_POINT('Ctrl Pts',(-2.03091336214426,1.,0.533108355132976));
#44479=CARTESIAN_POINT('Ctrl Pts',(-2.03562362954037,1.,0.537258489833262));
#44480=CARTESIAN_POINT('Ctrl Pts',(-2.04031422690527,1.,0.541447120615659));
#44481=CARTESIAN_POINT('Ctrl Pts',(-2.04498544714588,1.,0.54567390381743));
#44482=CARTESIAN_POINT('Ctrl Pts',(-2.04963761077958,1.,0.549938525150295));
#44483=CARTESIAN_POINT('Ctrl Pts',(-2.05427091604413,1.,0.554240657463906));
#44484=CARTESIAN_POINT('Ctrl Pts',(-2.05888537756462,1.,0.558579940185151));
#44485=CARTESIAN_POINT('Ctrl Pts',(-2.06348090160589,1.,0.562955993082261));
#44486=CARTESIAN_POINT('Ctrl Pts',(-2.06805732997334,1.,0.567368421181087));
#44487=CARTESIAN_POINT('Ctrl Pts',(-2.07261449292824,1.,0.571816823242603));
#44488=CARTESIAN_POINT('Ctrl Pts',(-2.07715226767559,1.,0.576300797416844));
#44489=CARTESIAN_POINT('Ctrl Pts',(-2.08167059018418,1.,0.580819952108063));
#44490=CARTESIAN_POINT('Ctrl Pts',(-2.08616943727951,1.,0.585373918991617));
#44491=CARTESIAN_POINT('Ctrl Pts',(-2.09064881812129,1.,0.589962365403406));
#44492=CARTESIAN_POINT('Ctrl Pts',(-2.0951087622027,1.,0.594585006052162));
#44493=CARTESIAN_POINT('Ctrl Pts',(-2.0995493086477,1.,0.599241616420533));
#44494=CARTESIAN_POINT('Ctrl Pts',(-2.10397049886949,1.,0.60393203073603));
#44495=CARTESIAN_POINT('Ctrl Pts',(-2.1074919961518,1.,0.607711315454876));
#44496=CARTESIAN_POINT('Ctrl Pts',(-2.11012443807238,1.,0.610560911689899));
#44497=CARTESIAN_POINT('Ctrl Pts',(-2.11187554259986,1.,0.6124673655618));
#44498=CARTESIAN_POINT('Ctrl Pts',(-2.11275013067528,1.,0.61342227326009));
#44499=CARTESIAN_POINT('',(-1.7075470150345,0.,0.383122945602003));
#44500=CARTESIAN_POINT('Origin',(0.,0.,0.));
#44501=CARTESIAN_POINT('',(-1.74236521665491,1.,0.163289472382896));
#44502=CARTESIAN_POINT('Origin',(0.,1.,0.));
#44503=CARTESIAN_POINT('',(-1.74236521665491,0.,0.163289472382896));
#44504=CARTESIAN_POINT('Ctrl Pts',(-2.19890268624765,-1.,0.069476445021958));
#44505=CARTESIAN_POINT('Ctrl Pts',(-2.19890268624765,1.,0.069476445021958));
#44506=CARTESIAN_POINT('Ctrl Pts',(-2.19777582085423,-1.,0.0701143536325489));
#44507=CARTESIAN_POINT('Ctrl Pts',(-2.19777582085423,1.,0.0701143536325489));
#44508=CARTESIAN_POINT('Ctrl Pts',(-2.19552129484002,-1.,0.0713863779526153));
#44509=CARTESIAN_POINT('Ctrl Pts',(-2.19552129484002,1.,0.0713863779526153));
#44510=CARTESIAN_POINT('Ctrl Pts',(-2.19213712013662,-1.,0.0732830357306724));
#44511=CARTESIAN_POINT('Ctrl Pts',(-2.19213712013662,1.,0.0732830357306724));
#44512=CARTESIAN_POINT('Ctrl Pts',(-2.1876201139953,-1.,0.0757891465836146));
#44513=CARTESIAN_POINT('Ctrl Pts',(-2.1876201139953,1.,0.0757891465836146));
#44514=CARTESIAN_POINT('Ctrl Pts',(-2.18196589448887,-1.,0.0788837727685241));
#44515=CARTESIAN_POINT('Ctrl Pts',(-2.18196589448887,1.,0.0788837727685241));
#44516=CARTESIAN_POINT('Ctrl Pts',(-2.176303712113,-1.,0.0819402680872764));
#44517=CARTESIAN_POINT('Ctrl Pts',(-2.176303712113,1.,0.0819402680872764));
#44518=CARTESIAN_POINT('Ctrl Pts',(-2.17063357870952,-1.,0.0849584620835371));
#44519=CARTESIAN_POINT('Ctrl Pts',(-2.17063357870952,1.,0.0849584620835371));
#44520=CARTESIAN_POINT('Ctrl Pts',(-2.16495552645014,-1.,0.0879381291386921));
#44521=CARTESIAN_POINT('Ctrl Pts',(-2.16495552645014,1.,0.0879381291386921));
#44522=CARTESIAN_POINT('Ctrl Pts',(-2.15926961544516,-1.,0.0908789888107264));
#44523=CARTESIAN_POINT('Ctrl Pts',(-2.15926961544516,1.,0.0908789888107264));
#44524=CARTESIAN_POINT('Ctrl Pts',(-2.1535759397817,-1.,0.0937807218867642));
#44525=CARTESIAN_POINT('Ctrl Pts',(-2.1535759397817,1.,0.0937807218867642));
#44526=CARTESIAN_POINT('Ctrl Pts',(-2.14787463531795,-1.,0.0966429852305457));
#44527=CARTESIAN_POINT('Ctrl Pts',(-2.14787463531795,1.,0.0966429852305457));
#44528=CARTESIAN_POINT('Ctrl Pts',(-2.14216588396025,-1.,0.0994654261990914));
#44529=CARTESIAN_POINT('Ctrl Pts',(-2.14216588396025,1.,0.0994654261990914));
#44530=CARTESIAN_POINT('Ctrl Pts',(-2.13644992667165,-1.,0.1022477005561));
#44531=CARTESIAN_POINT('Ctrl Pts',(-2.13644992667165,1.,0.1022477005561));
#44532=CARTESIAN_POINT('Ctrl Pts',(-2.13072704887293,-1.,0.104989479152739));
#44533=CARTESIAN_POINT('Ctrl Pts',(-2.13072704887293,1.,0.104989479152739));
#44534=CARTESIAN_POINT('Ctrl Pts',(-2.12499752307,-1.,0.10769043523109));
#44535=CARTESIAN_POINT('Ctrl Pts',(-2.12499752307,1.,0.10769043523109));
#44536=CARTESIAN_POINT('Ctrl Pts',(-2.11926155590865,-1.,0.110350236135025));
#44537=CARTESIAN_POINT('Ctrl Pts',(-2.11926155590865,1.,0.110350236135025));
#44538=CARTESIAN_POINT('Ctrl Pts',(-2.11351924490306,-1.,0.112968534419737));
#44539=CARTESIAN_POINT('Ctrl Pts',(-2.11351924490306,1.,0.112968534419737));
#44540=CARTESIAN_POINT('Ctrl Pts',(-2.10777050261309,-1.,0.115544957687926));
#44541=CARTESIAN_POINT('Ctrl Pts',(-2.10777050261309,1.,0.115544957687926));
#44542=CARTESIAN_POINT('Ctrl Pts',(-2.102015121329,-1.,0.118079107988355));
#44543=CARTESIAN_POINT('Ctrl Pts',(-2.102015121329,1.,0.118079107988355));
#44544=CARTESIAN_POINT('Ctrl Pts',(-2.0962529286773,-1.,0.120570567965122));
#44545=CARTESIAN_POINT('Ctrl Pts',(-2.0962529286773,1.,0.120570567965122));
#44546=CARTESIAN_POINT('Ctrl Pts',(-2.09048392424825,-1.,0.123018905621083));
#44547=CARTESIAN_POINT('Ctrl Pts',(-2.09048392424825,1.,0.123018905621083));
#44548=CARTESIAN_POINT('Ctrl Pts',(-2.08470840653643,-1.,0.125423679412061));
#44549=CARTESIAN_POINT('Ctrl Pts',(-2.08470840653643,1.,0.125423679412061));
#44550=CARTESIAN_POINT('Ctrl Pts',(-2.07892715110987,-1.,0.12778444527612));
#44551=CARTESIAN_POINT('Ctrl Pts',(-2.07892715110987,1.,0.12778444527612));
#44552=CARTESIAN_POINT('Ctrl Pts',(-2.07314114713063,-1.,0.130100748328403));
#44553=CARTESIAN_POINT('Ctrl Pts',(-2.07314114713063,1.,0.130100748328403));
#44554=CARTESIAN_POINT('Ctrl Pts',(-2.06735123910326,-1.,0.13237211154771));
#44555=CARTESIAN_POINT('Ctrl Pts',(-2.06735123910326,1.,0.13237211154771));
#44556=CARTESIAN_POINT('Ctrl Pts',(-2.06155781517842,-1.,0.134598026192106));
#44557=CARTESIAN_POINT('Ctrl Pts',(-2.06155781517842,1.,0.134598026192106));
#44558=CARTESIAN_POINT('Ctrl Pts',(-2.05576044414264,-1.,0.136777941218043));
#44559=CARTESIAN_POINT('Ctrl Pts',(-2.05576044414264,1.,0.136777941218043));
#44560=CARTESIAN_POINT('Ctrl Pts',(-2.04995762001328,-1.,0.138911255368966));
#44561=CARTESIAN_POINT('Ctrl Pts',(-2.04995762001328,1.,0.138911255368966));
#44562=CARTESIAN_POINT('Ctrl Pts',(-2.04414757947916,-1.,0.140997332152546));
#44563=CARTESIAN_POINT('Ctrl Pts',(-2.04414757947916,1.,0.140997332152546));
#44564=CARTESIAN_POINT('Ctrl Pts',(-2.03832911025912,-1.,0.143035515058209));
#44565=CARTESIAN_POINT('Ctrl Pts',(-2.03832911025912,1.,0.143035515058209));
#44566=CARTESIAN_POINT('Ctrl Pts',(-2.03250223739942,-1.,0.145025140186057));
#44567=CARTESIAN_POINT('Ctrl Pts',(-2.03250223739942,1.,0.145025140186057));
#44568=CARTESIAN_POINT('Ctrl Pts',(-2.02666926182017,-1.,0.146965557332583));
#44569=CARTESIAN_POINT('Ctrl Pts',(-2.02666926182017,1.,0.146965557332583));
#44570=CARTESIAN_POINT('Ctrl Pts',(-2.02083464969894,-1.,0.148856124775337));
#44571=CARTESIAN_POINT('Ctrl Pts',(-2.02083464969894,1.,0.148856124775337));
#44572=CARTESIAN_POINT('Ctrl Pts',(-2.01500291940238,-1.,0.150696157673078));
#44573=CARTESIAN_POINT('Ctrl Pts',(-2.01500291940238,1.,0.150696157673078));
#44574=CARTESIAN_POINT('Ctrl Pts',(-2.00917680318424,-1.,0.15248488362145));
#44575=CARTESIAN_POINT('Ctrl Pts',(-2.00917680318424,1.,0.15248488362145));
#44576=CARTESIAN_POINT('Ctrl Pts',(-2.00335565310543,-1.,0.154221403049722));
#44577=CARTESIAN_POINT('Ctrl Pts',(-2.00335565310543,1.,0.154221403049722));
#44578=CARTESIAN_POINT('Ctrl Pts',(-1.99753284771497,-1.,0.155904629548783));
#44579=CARTESIAN_POINT('Ctrl Pts',(-1.99753284771497,1.,0.155904629548783));
#44580=CARTESIAN_POINT('Ctrl Pts',(-1.99169810931908,-1.,0.157533331459227));
#44581=CARTESIAN_POINT('Ctrl Pts',(-1.99169810931908,1.,0.157533331459227));
#44582=CARTESIAN_POINT('Ctrl Pts',(-1.98584238283292,-1.,0.159106226437299));
#44583=CARTESIAN_POINT('Ctrl Pts',(-1.98584238283292,1.,0.159106226437299));
#44584=CARTESIAN_POINT('Ctrl Pts',(-1.97996195437559,-1.,0.160622060784611));
#44585=CARTESIAN_POINT('Ctrl Pts',(-1.97996195437559,1.,0.160622060784611));
#44586=CARTESIAN_POINT('Ctrl Pts',(-1.97406280235188,-1.,0.162079693556288));
#44587=CARTESIAN_POINT('Ctrl Pts',(-1.97406280235188,1.,0.162079693556288));
#44588=CARTESIAN_POINT('Ctrl Pts',(-1.96816512677967,-1.,0.163478185457734));
#44589=CARTESIAN_POINT('Ctrl Pts',(-1.96816512677967,1.,0.163478185457734));
#44590=CARTESIAN_POINT('Ctrl Pts',(-1.96229379940136,-1.,0.164816568920269));
#44591=CARTESIAN_POINT('Ctrl Pts',(-1.96229379940136,1.,0.164816568920269));
#44592=CARTESIAN_POINT('Ctrl Pts',(-1.9564675971873,-1.,0.166093592002812));
#44593=CARTESIAN_POINT('Ctrl Pts',(-1.9564675971873,1.,0.166093592002812));
#44594=CARTESIAN_POINT('Ctrl Pts',(-1.95069027794294,-1.,0.167307501784475));
#44595=CARTESIAN_POINT('Ctrl Pts',(-1.95069027794294,1.,0.167307501784475));
#44596=CARTESIAN_POINT('Ctrl Pts',(-1.94493757756931,-1.,0.168455741607556));
#44597=CARTESIAN_POINT('Ctrl Pts',(-1.94493757756931,1.,0.168455741607556));
#44598=CARTESIAN_POINT('Ctrl Pts',(-1.93915639211581,-1.,0.169534904817491));
#44599=CARTESIAN_POINT('Ctrl Pts',(-1.93915639211581,1.,0.169534904817491));
#44600=CARTESIAN_POINT('Ctrl Pts',(-1.93329183155539,-1.,0.170541253116201));
#44601=CARTESIAN_POINT('Ctrl Pts',(-1.93329183155539,1.,0.170541253116201));
#44602=CARTESIAN_POINT('Ctrl Pts',(-1.92731093582036,-1.,0.171471191532988));
#44603=CARTESIAN_POINT('Ctrl Pts',(-1.92731093582036,1.,0.171471191532988));
#44604=CARTESIAN_POINT('Ctrl Pts',(-1.9212233439798,-1.,0.172321621259514));
#44605=CARTESIAN_POINT('Ctrl Pts',(-1.9212233439798,1.,0.172321621259514));
#44606=CARTESIAN_POINT('Ctrl Pts',(-1.91511429159527,-1.,0.173090695383496));
#44607=CARTESIAN_POINT('Ctrl Pts',(-1.91511429159527,1.,0.173090695383496));
#44608=CARTESIAN_POINT('Ctrl Pts',(-1.90911693975267,-1.,0.173776635257817));
#44609=CARTESIAN_POINT('Ctrl Pts',(-1.90911693975267,1.,0.173776635257817));
#44610=CARTESIAN_POINT('Ctrl Pts',(-1.90335253862834,-1.,0.174375518661085));
#44611=CARTESIAN_POINT('Ctrl Pts',(-1.90335253862834,1.,0.174375518661085));
#44612=CARTESIAN_POINT('Ctrl Pts',(-1.89788101117132,-1.,0.174879405091263));
#44613=CARTESIAN_POINT('Ctrl Pts',(-1.89788101117132,1.,0.174879405091263));
#44614=CARTESIAN_POINT('Ctrl Pts',(-1.892646301985,-1.,0.175274276190844));
#44615=CARTESIAN_POINT('Ctrl Pts',(-1.892646301985,1.,0.175274276190844));
#44616=CARTESIAN_POINT('Ctrl Pts',(-1.88742606273259,-1.,0.175538155840648));
#44617=CARTESIAN_POINT('Ctrl Pts',(-1.88742606273259,1.,0.175538155840648));
#44618=CARTESIAN_POINT('Ctrl Pts',(-1.88188663145367,-1.,0.175644148889698));
#44619=CARTESIAN_POINT('Ctrl Pts',(-1.88188663145367,1.,0.175644148889698));
#44620=CARTESIAN_POINT('Ctrl Pts',(-1.87563767773588,-1.,0.175563480746485));
#44621=CARTESIAN_POINT('Ctrl Pts',(-1.87563767773588,1.,0.175563480746485));
#44622=CARTESIAN_POINT('Ctrl Pts',(-1.86828349694799,-1.,0.175268337590758));
#44623=CARTESIAN_POINT('Ctrl Pts',(-1.86828349694799,1.,0.175268337590758));
#44624=CARTESIAN_POINT('Ctrl Pts',(-1.85948367088837,-1.,0.17473525927603));
#44625=CARTESIAN_POINT('Ctrl Pts',(-1.85948367088837,1.,0.17473525927603));
#44626=CARTESIAN_POINT('Ctrl Pts',(-1.8489811319852,-1.,0.173946627587731));
#44627=CARTESIAN_POINT('Ctrl Pts',(-1.8489811319852,1.,0.173946627587731));
#44628=CARTESIAN_POINT('Ctrl Pts',(-1.83658380527692,-1.,0.1728894428919));
#44629=CARTESIAN_POINT('Ctrl Pts',(-1.83658380527692,1.,0.1728894428919));
#44630=CARTESIAN_POINT('Ctrl Pts',(-1.82215766811545,-1.,0.171554770204119));
#44631=CARTESIAN_POINT('Ctrl Pts',(-1.82215766811545,1.,0.171554770204119));
#44632=CARTESIAN_POINT('Ctrl Pts',(-1.80561530629706,-1.,0.169936923904608));
#44633=CARTESIAN_POINT('Ctrl Pts',(-1.80561530629706,1.,0.169936923904608));
#44634=CARTESIAN_POINT('Ctrl Pts',(-1.7869064998507,-1.,0.168032772805197));
#44635=CARTESIAN_POINT('Ctrl Pts',(-1.7869064998507,1.,0.168032772805197));
#44636=CARTESIAN_POINT('Ctrl Pts',(-1.77018771684844,-1.,0.1662793551464));
#44637=CARTESIAN_POINT('Ctrl Pts',(-1.77018771684844,1.,0.1662793551464));
#44638=CARTESIAN_POINT('Ctrl Pts',(-1.75666056638427,-1.,0.164834765707158));
#44639=CARTESIAN_POINT('Ctrl Pts',(-1.75666056638427,1.,0.164834765707158));
#44640=CARTESIAN_POINT('Ctrl Pts',(-1.7472034950333,-1.,0.163814161002002));
#44641=CARTESIAN_POINT('Ctrl Pts',(-1.7472034950333,1.,0.163814161002002));
#44642=CARTESIAN_POINT('Ctrl Pts',(-1.74236521665491,-1.,0.163289472382896));
#44643=CARTESIAN_POINT('Ctrl Pts',(-1.74236521665491,1.,0.163289472382896));
#44644=CARTESIAN_POINT('',(-2.19890268624765,1.,0.069476445021958));
#44645=CARTESIAN_POINT('Ctrl Pts',(-2.19890268624765,1.,0.069476445021958));
#44646=CARTESIAN_POINT('Ctrl Pts',(-2.19777582085423,1.,0.0701143536325489));
#44647=CARTESIAN_POINT('Ctrl Pts',(-2.19552129484002,1.,0.0713863779526153));
#44648=CARTESIAN_POINT('Ctrl Pts',(-2.19213712013662,1.,0.0732830357306724));
#44649=CARTESIAN_POINT('Ctrl Pts',(-2.1876201139953,1.,0.0757891465836146));
#44650=CARTESIAN_POINT('Ctrl Pts',(-2.18196589448887,1.,0.0788837727685241));
#44651=CARTESIAN_POINT('Ctrl Pts',(-2.176303712113,1.,0.0819402680872764));
#44652=CARTESIAN_POINT('Ctrl Pts',(-2.17063357870952,1.,0.0849584620835371));
#44653=CARTESIAN_POINT('Ctrl Pts',(-2.16495552645014,1.,0.0879381291386921));
#44654=CARTESIAN_POINT('Ctrl Pts',(-2.15926961544516,1.,0.0908789888107264));
#44655=CARTESIAN_POINT('Ctrl Pts',(-2.1535759397817,1.,0.0937807218867642));
#44656=CARTESIAN_POINT('Ctrl Pts',(-2.14787463531795,1.,0.0966429852305457));
#44657=CARTESIAN_POINT('Ctrl Pts',(-2.14216588396025,1.,0.0994654261990914));
#44658=CARTESIAN_POINT('Ctrl Pts',(-2.13644992667165,1.,0.1022477005561));
#44659=CARTESIAN_POINT('Ctrl Pts',(-2.13072704887293,1.,0.104989479152739));
#44660=CARTESIAN_POINT('Ctrl Pts',(-2.12499752307,1.,0.10769043523109));
#44661=CARTESIAN_POINT('Ctrl Pts',(-2.11926155590865,1.,0.110350236135025));
#44662=CARTESIAN_POINT('Ctrl Pts',(-2.11351924490306,1.,0.112968534419737));
#44663=CARTESIAN_POINT('Ctrl Pts',(-2.10777050261309,1.,0.115544957687926));
#44664=CARTESIAN_POINT('Ctrl Pts',(-2.102015121329,1.,0.118079107988355));
#44665=CARTESIAN_POINT('Ctrl Pts',(-2.0962529286773,1.,0.120570567965122));
#44666=CARTESIAN_POINT('Ctrl Pts',(-2.09048392424825,1.,0.123018905621083));
#44667=CARTESIAN_POINT('Ctrl Pts',(-2.08470840653643,1.,0.125423679412061));
#44668=CARTESIAN_POINT('Ctrl Pts',(-2.07892715110987,1.,0.12778444527612));
#44669=CARTESIAN_POINT('Ctrl Pts',(-2.07314114713063,1.,0.130100748328403));
#44670=CARTESIAN_POINT('Ctrl Pts',(-2.06735123910326,1.,0.13237211154771));
#44671=CARTESIAN_POINT('Ctrl Pts',(-2.06155781517842,1.,0.134598026192106));
#44672=CARTESIAN_POINT('Ctrl Pts',(-2.05576044414264,1.,0.136777941218043));
#44673=CARTESIAN_POINT('Ctrl Pts',(-2.04995762001328,1.,0.138911255368966));
#44674=CARTESIAN_POINT('Ctrl Pts',(-2.04414757947916,1.,0.140997332152546));
#44675=CARTESIAN_POINT('Ctrl Pts',(-2.03832911025912,1.,0.143035515058209));
#44676=CARTESIAN_POINT('Ctrl Pts',(-2.03250223739942,1.,0.145025140186057));
#44677=CARTESIAN_POINT('Ctrl Pts',(-2.02666926182017,1.,0.146965557332583));
#44678=CARTESIAN_POINT('Ctrl Pts',(-2.02083464969894,1.,0.148856124775337));
#44679=CARTESIAN_POINT('Ctrl Pts',(-2.01500291940238,1.,0.150696157673078));
#44680=CARTESIAN_POINT('Ctrl Pts',(-2.00917680318424,1.,0.15248488362145));
#44681=CARTESIAN_POINT('Ctrl Pts',(-2.00335565310543,1.,0.154221403049722));
#44682=CARTESIAN_POINT('Ctrl Pts',(-1.99753284771497,1.,0.155904629548783));
#44683=CARTESIAN_POINT('Ctrl Pts',(-1.99169810931908,1.,0.157533331459227));
#44684=CARTESIAN_POINT('Ctrl Pts',(-1.98584238283292,1.,0.159106226437299));
#44685=CARTESIAN_POINT('Ctrl Pts',(-1.97996195437559,1.,0.160622060784611));
#44686=CARTESIAN_POINT('Ctrl Pts',(-1.97406280235188,1.,0.162079693556288));
#44687=CARTESIAN_POINT('Ctrl Pts',(-1.96816512677967,1.,0.163478185457734));
#44688=CARTESIAN_POINT('Ctrl Pts',(-1.96229379940136,1.,0.164816568920269));
#44689=CARTESIAN_POINT('Ctrl Pts',(-1.9564675971873,1.,0.166093592002812));
#44690=CARTESIAN_POINT('Ctrl Pts',(-1.95069027794294,1.,0.167307501784475));
#44691=CARTESIAN_POINT('Ctrl Pts',(-1.94493757756931,1.,0.168455741607556));
#44692=CARTESIAN_POINT('Ctrl Pts',(-1.93915639211581,1.,0.169534904817491));
#44693=CARTESIAN_POINT('Ctrl Pts',(-1.93329183155539,1.,0.170541253116201));
#44694=CARTESIAN_POINT('Ctrl Pts',(-1.92731093582036,1.,0.171471191532988));
#44695=CARTESIAN_POINT('Ctrl Pts',(-1.9212233439798,1.,0.172321621259514));
#44696=CARTESIAN_POINT('Ctrl Pts',(-1.91511429159527,1.,0.173090695383496));
#44697=CARTESIAN_POINT('Ctrl Pts',(-1.90911693975267,1.,0.173776635257817));
#44698=CARTESIAN_POINT('Ctrl Pts',(-1.90335253862834,1.,0.174375518661085));
#44699=CARTESIAN_POINT('Ctrl Pts',(-1.89788101117132,1.,0.174879405091263));
#44700=CARTESIAN_POINT('Ctrl Pts',(-1.892646301985,1.,0.175274276190844));
#44701=CARTESIAN_POINT('Ctrl Pts',(-1.88742606273259,1.,0.175538155840648));
#44702=CARTESIAN_POINT('Ctrl Pts',(-1.88188663145367,1.,0.175644148889698));
#44703=CARTESIAN_POINT('Ctrl Pts',(-1.87563767773588,1.,0.175563480746485));
#44704=CARTESIAN_POINT('Ctrl Pts',(-1.86828349694799,1.,0.175268337590758));
#44705=CARTESIAN_POINT('Ctrl Pts',(-1.85948367088837,1.,0.17473525927603));
#44706=CARTESIAN_POINT('Ctrl Pts',(-1.8489811319852,1.,0.173946627587731));
#44707=CARTESIAN_POINT('Ctrl Pts',(-1.83658380527692,1.,0.1728894428919));
#44708=CARTESIAN_POINT('Ctrl Pts',(-1.82215766811545,1.,0.171554770204119));
#44709=CARTESIAN_POINT('Ctrl Pts',(-1.80561530629706,1.,0.169936923904608));
#44710=CARTESIAN_POINT('Ctrl Pts',(-1.7869064998507,1.,0.168032772805197));
#44711=CARTESIAN_POINT('Ctrl Pts',(-1.77018771684844,1.,0.1662793551464));
#44712=CARTESIAN_POINT('Ctrl Pts',(-1.75666056638427,1.,0.164834765707158));
#44713=CARTESIAN_POINT('Ctrl Pts',(-1.7472034950333,1.,0.163814161002002));
#44714=CARTESIAN_POINT('Ctrl Pts',(-1.74236521665491,1.,0.163289472382896));
#44715=CARTESIAN_POINT('',(-2.19890268624765,0.,0.069476445021958));
#44716=CARTESIAN_POINT('Origin',(-2.19890268624765,0.,-0.0694764450219585));
#44717=CARTESIAN_POINT('',(-2.19890268624765,1.,-0.0694764450219585));
#44718=CARTESIAN_POINT('',(-2.19890268624765,1.,0.069476445021958));
#44719=CARTESIAN_POINT('',(-2.19890268624765,0.,-0.0694764450219585));
#44720=CARTESIAN_POINT('Ctrl Pts',(-1.74236521665491,-1.,-0.163289472382896));
#44721=CARTESIAN_POINT('Ctrl Pts',(-1.74236521665491,1.,-0.163289472382896));
#44722=CARTESIAN_POINT('Ctrl Pts',(-1.74720349503904,-1.,-0.163814161002474));
#44723=CARTESIAN_POINT('Ctrl Pts',(-1.74720349503904,1.,-0.163814161002474));
#44724=CARTESIAN_POINT('Ctrl Pts',(-1.75666056640041,-1.,-0.164834765708484));
#44725=CARTESIAN_POINT('Ctrl Pts',(-1.75666056640041,1.,-0.164834765708484));
#44726=CARTESIAN_POINT('Ctrl Pts',(-1.77018771687692,-1.,-0.166279355148738));
#44727=CARTESIAN_POINT('Ctrl Pts',(-1.77018771687692,1.,-0.166279355148738));
#44728=CARTESIAN_POINT('Ctrl Pts',(-1.78690649988931,-1.,-0.16803277280837));
#44729=CARTESIAN_POINT('Ctrl Pts',(-1.78690649988931,1.,-0.16803277280837));
#44730=CARTESIAN_POINT('Ctrl Pts',(-1.80561530633924,-1.,-0.169936923908078));
#44731=CARTESIAN_POINT('Ctrl Pts',(-1.80561530633924,1.,-0.169936923908078));
#44732=CARTESIAN_POINT('Ctrl Pts',(-1.82215766815414,-1.,-0.171554770207306));
#44733=CARTESIAN_POINT('Ctrl Pts',(-1.82215766815414,1.,-0.171554770207306));
#44734=CARTESIAN_POINT('Ctrl Pts',(-1.83658380530747,-1.,-0.17288944289442));
#44735=CARTESIAN_POINT('Ctrl Pts',(-1.83658380530747,1.,-0.17288944289442));
#44736=CARTESIAN_POINT('Ctrl Pts',(-1.84898113200543,-1.,-0.173946627589401));
#44737=CARTESIAN_POINT('Ctrl Pts',(-1.84898113200543,1.,-0.173946627589401));
#44738=CARTESIAN_POINT('Ctrl Pts',(-1.85948367089838,-1.,-0.174735259276856));
#44739=CARTESIAN_POINT('Ctrl Pts',(-1.85948367089838,1.,-0.174735259276856));
#44740=CARTESIAN_POINT('Ctrl Pts',(-1.86828349694972,-1.,-0.175268337590901));
#44741=CARTESIAN_POINT('Ctrl Pts',(-1.86828349694972,1.,-0.175268337590901));
#44742=CARTESIAN_POINT('Ctrl Pts',(-1.87563767773249,-1.,-0.175563480746205));
#44743=CARTESIAN_POINT('Ctrl Pts',(-1.87563767773249,1.,-0.175563480746205));
#44744=CARTESIAN_POINT('Ctrl Pts',(-1.88188663144846,-1.,-0.175644148889271));
#44745=CARTESIAN_POINT('Ctrl Pts',(-1.88188663144846,1.,-0.175644148889271));
#44746=CARTESIAN_POINT('Ctrl Pts',(-1.88742606272818,-1.,-0.175538155840286));
#44747=CARTESIAN_POINT('Ctrl Pts',(-1.88742606272818,1.,-0.175538155840286));
#44748=CARTESIAN_POINT('Ctrl Pts',(-1.89264630198279,-1.,-0.175274276190664));
#44749=CARTESIAN_POINT('Ctrl Pts',(-1.89264630198279,1.,-0.175274276190664));
#44750=CARTESIAN_POINT('Ctrl Pts',(-1.89788101117148,-1.,-0.174879405091277));
#44751=CARTESIAN_POINT('Ctrl Pts',(-1.89788101117148,1.,-0.174879405091277));
#44752=CARTESIAN_POINT('Ctrl Pts',(-1.90335253863003,-1.,-0.174375518661222));
#44753=CARTESIAN_POINT('Ctrl Pts',(-1.90335253863003,1.,-0.174375518661222));
#44754=CARTESIAN_POINT('Ctrl Pts',(-1.90911693975475,-1.,-0.173776635257984));
#44755=CARTESIAN_POINT('Ctrl Pts',(-1.90911693975475,1.,-0.173776635257984));
#44756=CARTESIAN_POINT('Ctrl Pts',(-1.91511429159681,-1.,-0.173090695383619));
#44757=CARTESIAN_POINT('Ctrl Pts',(-1.91511429159681,1.,-0.173090695383619));
#44758=CARTESIAN_POINT('Ctrl Pts',(-1.92122334398034,-1.,-0.172321621259557));
#44759=CARTESIAN_POINT('Ctrl Pts',(-1.92122334398034,1.,-0.172321621259557));
#44760=CARTESIAN_POINT('Ctrl Pts',(-1.92731093582,-1.,-0.17147119153296));
#44761=CARTESIAN_POINT('Ctrl Pts',(-1.92731093582,1.,-0.17147119153296));
#44762=CARTESIAN_POINT('Ctrl Pts',(-1.93329183155455,-1.,-0.170541253116136));
#44763=CARTESIAN_POINT('Ctrl Pts',(-1.93329183155455,1.,-0.170541253116136));
#44764=CARTESIAN_POINT('Ctrl Pts',(-1.93915639211497,-1.,-0.169534904817425));
#44765=CARTESIAN_POINT('Ctrl Pts',(-1.93915639211497,1.,-0.169534904817425));
#44766=CARTESIAN_POINT('Ctrl Pts',(-1.94493757756879,-1.,-0.168455741607516));
#44767=CARTESIAN_POINT('Ctrl Pts',(-1.94493757756879,1.,-0.168455741607516));
#44768=CARTESIAN_POINT('Ctrl Pts',(-1.95069027794286,-1.,-0.167307501784469));
#44769=CARTESIAN_POINT('Ctrl Pts',(-1.95069027794286,1.,-0.167307501784469));
#44770=CARTESIAN_POINT('Ctrl Pts',(-1.95646759718755,-1.,-0.166093592002833));
#44771=CARTESIAN_POINT('Ctrl Pts',(-1.95646759718755,1.,-0.166093592002833));
#44772=CARTESIAN_POINT('Ctrl Pts',(-1.96229379940174,-1.,-0.1648165689203));
#44773=CARTESIAN_POINT('Ctrl Pts',(-1.96229379940174,1.,-0.1648165689203));
#44774=CARTESIAN_POINT('Ctrl Pts',(-1.96816512678,-1.,-0.16347818545776));
#44775=CARTESIAN_POINT('Ctrl Pts',(-1.96816512678,1.,-0.16347818545776));
#44776=CARTESIAN_POINT('Ctrl Pts',(-1.97406280235204,-1.,-0.162079693556302));
#44777=CARTESIAN_POINT('Ctrl Pts',(-1.97406280235204,1.,-0.162079693556302));
#44778=CARTESIAN_POINT('Ctrl Pts',(-1.97996195437557,-1.,-0.16062206078461));
#44779=CARTESIAN_POINT('Ctrl Pts',(-1.97996195437557,1.,-0.16062206078461));
#44780=CARTESIAN_POINT('Ctrl Pts',(-1.98584238283279,-1.,-0.159106226437289));
#44781=CARTESIAN_POINT('Ctrl Pts',(-1.98584238283279,1.,-0.159106226437289));
#44782=CARTESIAN_POINT('Ctrl Pts',(-1.99169810931893,-1.,-0.157533331459215));
#44783=CARTESIAN_POINT('Ctrl Pts',(-1.99169810931893,1.,-0.157533331459215));
#44784=CARTESIAN_POINT('Ctrl Pts',(-1.99753284771487,-1.,-0.155904629548775));
#44785=CARTESIAN_POINT('Ctrl Pts',(-1.99753284771487,1.,-0.155904629548775));
#44786=CARTESIAN_POINT('Ctrl Pts',(-2.00335565310539,-1.,-0.154221403049719));
#44787=CARTESIAN_POINT('Ctrl Pts',(-2.00335565310539,1.,-0.154221403049719));
#44788=CARTESIAN_POINT('Ctrl Pts',(-2.00917680318426,-1.,-0.152484883621452));
#44789=CARTESIAN_POINT('Ctrl Pts',(-2.00917680318426,1.,-0.152484883621452));
#44790=CARTESIAN_POINT('Ctrl Pts',(-2.01500291940243,-1.,-0.150696157673084));
#44791=CARTESIAN_POINT('Ctrl Pts',(-2.01500291940243,1.,-0.150696157673084));
#44792=CARTESIAN_POINT('Ctrl Pts',(-2.02083464969897,-1.,-0.148856124775343));
#44793=CARTESIAN_POINT('Ctrl Pts',(-2.02083464969897,1.,-0.148856124775343));
#44794=CARTESIAN_POINT('Ctrl Pts',(-2.02666926182017,-1.,-0.146965557332586));
#44795=CARTESIAN_POINT('Ctrl Pts',(-2.02666926182017,1.,-0.146965557332586));
#44796=CARTESIAN_POINT('Ctrl Pts',(-2.03250223739941,-1.,-0.145025140186058));
#44797=CARTESIAN_POINT('Ctrl Pts',(-2.03250223739941,1.,-0.145025140186058));
#44798=CARTESIAN_POINT('Ctrl Pts',(-2.03832911025913,-1.,-0.143035515058208));
#44799=CARTESIAN_POINT('Ctrl Pts',(-2.03832911025913,1.,-0.143035515058208));
#44800=CARTESIAN_POINT('Ctrl Pts',(-2.04414757947919,-1.,-0.140997332152545));
#44801=CARTESIAN_POINT('Ctrl Pts',(-2.04414757947919,1.,-0.140997332152545));
#44802=CARTESIAN_POINT('Ctrl Pts',(-2.04995762001333,-1.,-0.138911255368966));
#44803=CARTESIAN_POINT('Ctrl Pts',(-2.04995762001333,1.,-0.138911255368966));
#44804=CARTESIAN_POINT('Ctrl Pts',(-2.0557604441427,-1.,-0.136777941218044));
#44805=CARTESIAN_POINT('Ctrl Pts',(-2.0557604441427,1.,-0.136777941218044));
#44806=CARTESIAN_POINT('Ctrl Pts',(-2.06155781517844,-1.,-0.134598026192107));
#44807=CARTESIAN_POINT('Ctrl Pts',(-2.06155781517844,1.,-0.134598026192107));
#44808=CARTESIAN_POINT('Ctrl Pts',(-2.06735123910319,-1.,-0.13237211154771));
#44809=CARTESIAN_POINT('Ctrl Pts',(-2.06735123910319,1.,-0.13237211154771));
#44810=CARTESIAN_POINT('Ctrl Pts',(-2.07314114713047,-1.,-0.130100748328401));
#44811=CARTESIAN_POINT('Ctrl Pts',(-2.07314114713047,1.,-0.130100748328401));
#44812=CARTESIAN_POINT('Ctrl Pts',(-2.07892715110967,-1.,-0.127784445276116));
#44813=CARTESIAN_POINT('Ctrl Pts',(-2.07892715110967,1.,-0.127784445276116));
#44814=CARTESIAN_POINT('Ctrl Pts',(-2.08470840653628,-1.,-0.125423679412058));
#44815=CARTESIAN_POINT('Ctrl Pts',(-2.08470840653628,1.,-0.125423679412058));
#44816=CARTESIAN_POINT('Ctrl Pts',(-2.09048392424826,-1.,-0.123018905621083));
#44817=CARTESIAN_POINT('Ctrl Pts',(-2.09048392424826,1.,-0.123018905621083));
#44818=CARTESIAN_POINT('Ctrl Pts',(-2.09625292867756,-1.,-0.120570567965129));
#44819=CARTESIAN_POINT('Ctrl Pts',(-2.09625292867756,1.,-0.120570567965129));
#44820=CARTESIAN_POINT('Ctrl Pts',(-2.10201512132945,-1.,-0.118079107988368));
#44821=CARTESIAN_POINT('Ctrl Pts',(-2.10201512132945,1.,-0.118079107988368));
#44822=CARTESIAN_POINT('Ctrl Pts',(-2.10777050261359,-1.,-0.11554495768794));
#44823=CARTESIAN_POINT('Ctrl Pts',(-2.10777050261359,1.,-0.11554495768794));
#44824=CARTESIAN_POINT('Ctrl Pts',(-2.11351924490335,-1.,-0.112968534419746));
#44825=CARTESIAN_POINT('Ctrl Pts',(-2.11351924490335,1.,-0.112968534419746));
#44826=CARTESIAN_POINT('Ctrl Pts',(-2.11926155590849,-1.,-0.11035023613502));
#44827=CARTESIAN_POINT('Ctrl Pts',(-2.11926155590849,1.,-0.11035023613502));
#44828=CARTESIAN_POINT('Ctrl Pts',(-2.12499752306927,-1.,-0.107690435231068));
#44829=CARTESIAN_POINT('Ctrl Pts',(-2.12499752306927,1.,-0.107690435231068));
#44830=CARTESIAN_POINT('Ctrl Pts',(-2.1307270488718,-1.,-0.104989479152703));
#44831=CARTESIAN_POINT('Ctrl Pts',(-2.1307270488718,1.,-0.104989479152703));
#44832=CARTESIAN_POINT('Ctrl Pts',(-2.13644992667052,-1.,-0.102247700556064));
#44833=CARTESIAN_POINT('Ctrl Pts',(-2.13644992667052,1.,-0.102247700556064));
#44834=CARTESIAN_POINT('Ctrl Pts',(-2.14216588395974,-1.,-0.0994654261990744));
#44835=CARTESIAN_POINT('Ctrl Pts',(-2.14216588395974,1.,-0.0994654261990744));
#44836=CARTESIAN_POINT('Ctrl Pts',(-2.14787463531864,-1.,-0.096642985230569));
#44837=CARTESIAN_POINT('Ctrl Pts',(-2.14787463531864,1.,-0.096642985230569));
#44838=CARTESIAN_POINT('Ctrl Pts',(-2.15357593978377,-1.,-0.0937807218868346));
#44839=CARTESIAN_POINT('Ctrl Pts',(-2.15357593978377,1.,-0.0937807218868346));
#44840=CARTESIAN_POINT('Ctrl Pts',(-2.15926961544808,-1.,-0.0908789888108267));
#44841=CARTESIAN_POINT('Ctrl Pts',(-2.15926961544808,1.,-0.0908789888108267));
#44842=CARTESIAN_POINT('Ctrl Pts',(-2.16495552645275,-1.,-0.0879381291387824));
#44843=CARTESIAN_POINT('Ctrl Pts',(-2.16495552645275,1.,-0.0879381291387824));
#44844=CARTESIAN_POINT('Ctrl Pts',(-2.17063357871031,-1.,-0.0849584620835644));
#44845=CARTESIAN_POINT('Ctrl Pts',(-2.17063357871031,1.,-0.0849584620835644));
#44846=CARTESIAN_POINT('Ctrl Pts',(-2.1763037121106,-1.,-0.0819402680871941));
#44847=CARTESIAN_POINT('Ctrl Pts',(-2.1763037121106,1.,-0.0819402680871941));
#44848=CARTESIAN_POINT('Ctrl Pts',(-2.18196589448304,-1.,-0.0788837727683229));
#44849=CARTESIAN_POINT('Ctrl Pts',(-2.18196589448304,1.,-0.0788837727683229));
#44850=CARTESIAN_POINT('Ctrl Pts',(-2.1876201139874,-1.,-0.0757891465833413));
#44851=CARTESIAN_POINT('Ctrl Pts',(-2.1876201139874,1.,-0.0757891465833413));
#44852=CARTESIAN_POINT('Ctrl Pts',(-2.19213712012956,-1.,-0.0732830357304277));
#44853=CARTESIAN_POINT('Ctrl Pts',(-2.19213712012956,1.,-0.0732830357304277));
#44854=CARTESIAN_POINT('Ctrl Pts',(-2.19552129483562,-1.,-0.0713863779524629));
#44855=CARTESIAN_POINT('Ctrl Pts',(-2.19552129483562,1.,-0.0713863779524629));
#44856=CARTESIAN_POINT('Ctrl Pts',(-2.19777582085261,-1.,-0.0701143536324927));
#44857=CARTESIAN_POINT('Ctrl Pts',(-2.19777582085261,1.,-0.0701143536324927));
#44858=CARTESIAN_POINT('Ctrl Pts',(-2.19890268624765,-1.,-0.0694764450219585));
#44859=CARTESIAN_POINT('Ctrl Pts',(-2.19890268624765,1.,-0.0694764450219585));
#44860=CARTESIAN_POINT('',(-1.74236521665491,1.,-0.163289472382896));
#44861=CARTESIAN_POINT('Ctrl Pts',(-1.74236521665491,1.,-0.163289472382896));
#44862=CARTESIAN_POINT('Ctrl Pts',(-1.74720349503904,1.,-0.163814161002474));
#44863=CARTESIAN_POINT('Ctrl Pts',(-1.75666056640041,1.,-0.164834765708484));
#44864=CARTESIAN_POINT('Ctrl Pts',(-1.77018771687692,1.,-0.166279355148738));
#44865=CARTESIAN_POINT('Ctrl Pts',(-1.78690649988931,1.,-0.16803277280837));
#44866=CARTESIAN_POINT('Ctrl Pts',(-1.80561530633924,1.,-0.169936923908078));
#44867=CARTESIAN_POINT('Ctrl Pts',(-1.82215766815414,1.,-0.171554770207306));
#44868=CARTESIAN_POINT('Ctrl Pts',(-1.83658380530747,1.,-0.17288944289442));
#44869=CARTESIAN_POINT('Ctrl Pts',(-1.84898113200543,1.,-0.173946627589401));
#44870=CARTESIAN_POINT('Ctrl Pts',(-1.85948367089838,1.,-0.174735259276856));
#44871=CARTESIAN_POINT('Ctrl Pts',(-1.86828349694972,1.,-0.175268337590901));
#44872=CARTESIAN_POINT('Ctrl Pts',(-1.87563767773249,1.,-0.175563480746205));
#44873=CARTESIAN_POINT('Ctrl Pts',(-1.88188663144846,1.,-0.175644148889271));
#44874=CARTESIAN_POINT('Ctrl Pts',(-1.88742606272818,1.,-0.175538155840286));
#44875=CARTESIAN_POINT('Ctrl Pts',(-1.89264630198279,1.,-0.175274276190664));
#44876=CARTESIAN_POINT('Ctrl Pts',(-1.89788101117148,1.,-0.174879405091277));
#44877=CARTESIAN_POINT('Ctrl Pts',(-1.90335253863003,1.,-0.174375518661222));
#44878=CARTESIAN_POINT('Ctrl Pts',(-1.90911693975475,1.,-0.173776635257984));
#44879=CARTESIAN_POINT('Ctrl Pts',(-1.91511429159681,1.,-0.173090695383619));
#44880=CARTESIAN_POINT('Ctrl Pts',(-1.92122334398034,1.,-0.172321621259557));
#44881=CARTESIAN_POINT('Ctrl Pts',(-1.92731093582,1.,-0.17147119153296));
#44882=CARTESIAN_POINT('Ctrl Pts',(-1.93329183155455,1.,-0.170541253116136));
#44883=CARTESIAN_POINT('Ctrl Pts',(-1.93915639211497,1.,-0.169534904817425));
#44884=CARTESIAN_POINT('Ctrl Pts',(-1.94493757756879,1.,-0.168455741607516));
#44885=CARTESIAN_POINT('Ctrl Pts',(-1.95069027794286,1.,-0.167307501784469));
#44886=CARTESIAN_POINT('Ctrl Pts',(-1.95646759718755,1.,-0.166093592002833));
#44887=CARTESIAN_POINT('Ctrl Pts',(-1.96229379940174,1.,-0.1648165689203));
#44888=CARTESIAN_POINT('Ctrl Pts',(-1.96816512678,1.,-0.16347818545776));
#44889=CARTESIAN_POINT('Ctrl Pts',(-1.97406280235204,1.,-0.162079693556302));
#44890=CARTESIAN_POINT('Ctrl Pts',(-1.97996195437557,1.,-0.16062206078461));
#44891=CARTESIAN_POINT('Ctrl Pts',(-1.98584238283279,1.,-0.159106226437289));
#44892=CARTESIAN_POINT('Ctrl Pts',(-1.99169810931893,1.,-0.157533331459215));
#44893=CARTESIAN_POINT('Ctrl Pts',(-1.99753284771487,1.,-0.155904629548775));
#44894=CARTESIAN_POINT('Ctrl Pts',(-2.00335565310539,1.,-0.154221403049719));
#44895=CARTESIAN_POINT('Ctrl Pts',(-2.00917680318426,1.,-0.152484883621452));
#44896=CARTESIAN_POINT('Ctrl Pts',(-2.01500291940243,1.,-0.150696157673084));
#44897=CARTESIAN_POINT('Ctrl Pts',(-2.02083464969897,1.,-0.148856124775343));
#44898=CARTESIAN_POINT('Ctrl Pts',(-2.02666926182017,1.,-0.146965557332586));
#44899=CARTESIAN_POINT('Ctrl Pts',(-2.03250223739941,1.,-0.145025140186058));
#44900=CARTESIAN_POINT('Ctrl Pts',(-2.03832911025913,1.,-0.143035515058208));
#44901=CARTESIAN_POINT('Ctrl Pts',(-2.04414757947919,1.,-0.140997332152545));
#44902=CARTESIAN_POINT('Ctrl Pts',(-2.04995762001333,1.,-0.138911255368966));
#44903=CARTESIAN_POINT('Ctrl Pts',(-2.0557604441427,1.,-0.136777941218044));
#44904=CARTESIAN_POINT('Ctrl Pts',(-2.06155781517844,1.,-0.134598026192107));
#44905=CARTESIAN_POINT('Ctrl Pts',(-2.06735123910319,1.,-0.13237211154771));
#44906=CARTESIAN_POINT('Ctrl Pts',(-2.07314114713047,1.,-0.130100748328401));
#44907=CARTESIAN_POINT('Ctrl Pts',(-2.07892715110967,1.,-0.127784445276116));
#44908=CARTESIAN_POINT('Ctrl Pts',(-2.08470840653628,1.,-0.125423679412058));
#44909=CARTESIAN_POINT('Ctrl Pts',(-2.09048392424826,1.,-0.123018905621083));
#44910=CARTESIAN_POINT('Ctrl Pts',(-2.09625292867756,1.,-0.120570567965129));
#44911=CARTESIAN_POINT('Ctrl Pts',(-2.10201512132945,1.,-0.118079107988368));
#44912=CARTESIAN_POINT('Ctrl Pts',(-2.10777050261359,1.,-0.11554495768794));
#44913=CARTESIAN_POINT('Ctrl Pts',(-2.11351924490335,1.,-0.112968534419746));
#44914=CARTESIAN_POINT('Ctrl Pts',(-2.11926155590849,1.,-0.11035023613502));
#44915=CARTESIAN_POINT('Ctrl Pts',(-2.12499752306927,1.,-0.107690435231068));
#44916=CARTESIAN_POINT('Ctrl Pts',(-2.1307270488718,1.,-0.104989479152703));
#44917=CARTESIAN_POINT('Ctrl Pts',(-2.13644992667052,1.,-0.102247700556064));
#44918=CARTESIAN_POINT('Ctrl Pts',(-2.14216588395974,1.,-0.0994654261990744));
#44919=CARTESIAN_POINT('Ctrl Pts',(-2.14787463531864,1.,-0.096642985230569));
#44920=CARTESIAN_POINT('Ctrl Pts',(-2.15357593978377,1.,-0.0937807218868346));
#44921=CARTESIAN_POINT('Ctrl Pts',(-2.15926961544808,1.,-0.0908789888108267));
#44922=CARTESIAN_POINT('Ctrl Pts',(-2.16495552645275,1.,-0.0879381291387824));
#44923=CARTESIAN_POINT('Ctrl Pts',(-2.17063357871031,1.,-0.0849584620835644));
#44924=CARTESIAN_POINT('Ctrl Pts',(-2.1763037121106,1.,-0.0819402680871941));
#44925=CARTESIAN_POINT('Ctrl Pts',(-2.18196589448304,1.,-0.0788837727683229));
#44926=CARTESIAN_POINT('Ctrl Pts',(-2.1876201139874,1.,-0.0757891465833413));
#44927=CARTESIAN_POINT('Ctrl Pts',(-2.19213712012956,1.,-0.0732830357304277));
#44928=CARTESIAN_POINT('Ctrl Pts',(-2.19552129483562,1.,-0.0713863779524629));
#44929=CARTESIAN_POINT('Ctrl Pts',(-2.19777582085261,1.,-0.0701143536324927));
#44930=CARTESIAN_POINT('Ctrl Pts',(-2.19890268624765,1.,-0.0694764450219585));
#44931=CARTESIAN_POINT('',(-1.74236521665491,0.,-0.163289472382896));
#44932=CARTESIAN_POINT('Origin',(0.,0.,0.));
#44933=CARTESIAN_POINT('',(-1.7075470150345,1.,-0.383122945602004));
#44934=CARTESIAN_POINT('Origin',(0.,1.,0.));
#44935=CARTESIAN_POINT('',(-1.7075470150345,0.,-0.383122945602004));
#44936=CARTESIAN_POINT('Ctrl Pts',(-2.11275013067528,-1.,-0.61342227326009));
#44937=CARTESIAN_POINT('Ctrl Pts',(-2.11275013067528,1.,-0.61342227326009));
#44938=CARTESIAN_POINT('Ctrl Pts',(-2.11187554260142,-1.,-0.61246736556225));
#44939=CARTESIAN_POINT('Ctrl Pts',(-2.11187554260142,1.,-0.61246736556225));
#44940=CARTESIAN_POINT('Ctrl Pts',(-2.11012443807661,-1.,-0.610560911691113));
#44941=CARTESIAN_POINT('Ctrl Pts',(-2.11012443807661,1.,-0.610560911691113));
#44942=CARTESIAN_POINT('Ctrl Pts',(-2.10749199615859,-1.,-0.607711315456826));
#44943=CARTESIAN_POINT('Ctrl Pts',(-2.10749199615859,1.,-0.607711315456826));
#44944=CARTESIAN_POINT('Ctrl Pts',(-2.10397049887709,-1.,-0.603932030738212));
#44945=CARTESIAN_POINT('Ctrl Pts',(-2.10397049887709,1.,-0.603932030738212));
#44946=CARTESIAN_POINT('Ctrl Pts',(-2.09954930865331,-1.,-0.599241616422144));
#44947=CARTESIAN_POINT('Ctrl Pts',(-2.09954930865331,1.,-0.599241616422144));
#44948=CARTESIAN_POINT('Ctrl Pts',(-2.09510876220501,-1.,-0.594585006052823));
#44949=CARTESIAN_POINT('Ctrl Pts',(-2.09510876220501,1.,-0.594585006052823));
#44950=CARTESIAN_POINT('Ctrl Pts',(-2.09064881812053,-1.,-0.589962365403189));
#44951=CARTESIAN_POINT('Ctrl Pts',(-2.09064881812053,1.,-0.589962365403189));
#44952=CARTESIAN_POINT('Ctrl Pts',(-2.086169437277,-1.,-0.585373918990895));
#44953=CARTESIAN_POINT('Ctrl Pts',(-2.086169437277,1.,-0.585373918990895));
#44954=CARTESIAN_POINT('Ctrl Pts',(-2.08167059018138,-1.,-0.580819952107257));
#44955=CARTESIAN_POINT('Ctrl Pts',(-2.08167059018138,1.,-0.580819952107257));
#44956=CARTESIAN_POINT('Ctrl Pts',(-2.07715226767361,-1.,-0.576300797416274));
#44957=CARTESIAN_POINT('Ctrl Pts',(-2.07715226767361,1.,-0.576300797416274));
#44958=CARTESIAN_POINT('Ctrl Pts',(-2.07261449292757,-1.,-0.571816823242411));
#44959=CARTESIAN_POINT('Ctrl Pts',(-2.07261449292757,1.,-0.571816823242411));
#44960=CARTESIAN_POINT('Ctrl Pts',(-2.06805732997383,-1.,-0.567368421181229));
#44961=CARTESIAN_POINT('Ctrl Pts',(-2.06805732997383,1.,-0.567368421181229));
#44962=CARTESIAN_POINT('Ctrl Pts',(-2.06348090160697,-1.,-0.562955993082574));
#44963=CARTESIAN_POINT('Ctrl Pts',(-2.06348090160697,1.,-0.562955993082574));
#44964=CARTESIAN_POINT('Ctrl Pts',(-2.05888537756571,-1.,-0.558579940185467));
#44965=CARTESIAN_POINT('Ctrl Pts',(-2.05888537756571,1.,-0.558579940185467));
#44966=CARTESIAN_POINT('Ctrl Pts',(-2.05427091604482,-1.,-0.554240657464109));
#44967=CARTESIAN_POINT('Ctrl Pts',(-2.05427091604482,1.,-0.554240657464109));
#44968=CARTESIAN_POINT('Ctrl Pts',(-2.04963761077974,-1.,-0.549938525150342));
#44969=CARTESIAN_POINT('Ctrl Pts',(-2.04963761077974,1.,-0.549938525150342));
#44970=CARTESIAN_POINT('Ctrl Pts',(-2.0449854471456,-1.,-0.545673903817348));
#44971=CARTESIAN_POINT('Ctrl Pts',(-2.0449854471456,1.,-0.545673903817348));
#44972=CARTESIAN_POINT('Ctrl Pts',(-2.0403142269048,-1.,-0.54144712061552));
#44973=CARTESIAN_POINT('Ctrl Pts',(-2.0403142269048,1.,-0.54144712061552));
#44974=CARTESIAN_POINT('Ctrl Pts',(-2.03562362953993,-1.,-0.537258489833134));
#44975=CARTESIAN_POINT('Ctrl Pts',(-2.03562362953993,1.,-0.537258489833134));
#44976=CARTESIAN_POINT('Ctrl Pts',(-2.03091336214401,-1.,-0.533108355132905));
#44977=CARTESIAN_POINT('Ctrl Pts',(-2.03091336214401,1.,-0.533108355132905));
#44978=CARTESIAN_POINT('Ctrl Pts',(-2.02618329083289,-1.,-0.52899712724191));
#44979=CARTESIAN_POINT('Ctrl Pts',(-2.02618329083289,1.,-0.52899712724191));
#44980=CARTESIAN_POINT('Ctrl Pts',(-2.02143356304712,-1.,-0.524925318333518));
#44981=CARTESIAN_POINT('Ctrl Pts',(-2.02143356304712,1.,-0.524925318333518));
#44982=CARTESIAN_POINT('Ctrl Pts',(-2.01666477917305,-1.,-0.520893590399428));
#44983=CARTESIAN_POINT('Ctrl Pts',(-2.01666477917305,1.,-0.520893590399428));
#44984=CARTESIAN_POINT('Ctrl Pts',(-2.01187773939257,-1.,-0.516902681728733));
#44985=CARTESIAN_POINT('Ctrl Pts',(-2.01187773939257,1.,-0.516902681728733));
#44986=CARTESIAN_POINT('Ctrl Pts',(-2.00707309946955,-1.,-0.512953306961813));
#44987=CARTESIAN_POINT('Ctrl Pts',(-2.00707309946955,1.,-0.512953306961813));
#44988=CARTESIAN_POINT('Ctrl Pts',(-2.00225107134733,-1.,-0.509046069886152));
#44989=CARTESIAN_POINT('Ctrl Pts',(-2.00225107134733,1.,-0.509046069886152));
#44990=CARTESIAN_POINT('Ctrl Pts',(-1.99741107463567,-1.,-0.505181361323011));
#44991=CARTESIAN_POINT('Ctrl Pts',(-1.99741107463567,1.,-0.505181361323011));
#44992=CARTESIAN_POINT('Ctrl Pts',(-1.9925514912615,-1.,-0.501359287727129));
#44993=CARTESIAN_POINT('Ctrl Pts',(-1.9925514912615,1.,-0.501359287727129));
#44994=CARTESIAN_POINT('Ctrl Pts',(-1.98767044752929,-1.,-0.497579909545564));
#44995=CARTESIAN_POINT('Ctrl Pts',(-1.98767044752929,1.,-0.497579909545564));
#44996=CARTESIAN_POINT('Ctrl Pts',(-1.9827665876182,-1.,-0.493843476541492));
#44997=CARTESIAN_POINT('Ctrl Pts',(-1.9827665876182,1.,-0.493843476541492));
#44998=CARTESIAN_POINT('Ctrl Pts',(-1.97783973019229,-1.,-0.490150627860955));
#44999=CARTESIAN_POINT('Ctrl Pts',(-1.97783973019229,1.,-0.490150627860955));
#45000=CARTESIAN_POINT('Ctrl Pts',(-1.97289186263272,-1.,-0.486502692907661));
#45001=CARTESIAN_POINT('Ctrl Pts',(-1.97289186263272,1.,-0.486502692907661));
#45002=CARTESIAN_POINT('Ctrl Pts',(-1.96792703422358,-1.,-0.482901662120686));
#45003=CARTESIAN_POINT('Ctrl Pts',(-1.96792703422358,1.,-0.482901662120686));
#45004=CARTESIAN_POINT('Ctrl Pts',(-1.96294933055938,-1.,-0.479349583074846));
#45005=CARTESIAN_POINT('Ctrl Pts',(-1.96294933055938,1.,-0.479349583074846));
#45006=CARTESIAN_POINT('Ctrl Pts',(-1.95796111148175,-1.,-0.475848034683171));
#45007=CARTESIAN_POINT('Ctrl Pts',(-1.95796111148175,1.,-0.475848034683171));
#45008=CARTESIAN_POINT('Ctrl Pts',(-1.95296148278136,-1.,-0.472397672264079));
#45009=CARTESIAN_POINT('Ctrl Pts',(-1.95296148278136,1.,-0.472397672264079));
#45010=CARTESIAN_POINT('Ctrl Pts',(-1.94794381136524,-1.,-0.468997482913158));
#45011=CARTESIAN_POINT('Ctrl Pts',(-1.94794381136524,1.,-0.468997482913158));
#45012=CARTESIAN_POINT('Ctrl Pts',(-1.94289794196205,-1.,-0.465645462026064));
#45013=CARTESIAN_POINT('Ctrl Pts',(-1.94289794196205,1.,-0.465645462026064));
#45014=CARTESIAN_POINT('Ctrl Pts',(-1.93781486640834,-1.,-0.462340031009087));
#45015=CARTESIAN_POINT('Ctrl Pts',(-1.93781486640834,1.,-0.462340031009087));
#45016=CARTESIAN_POINT('Ctrl Pts',(-1.93269066517936,-1.,-0.459081234547931));
#45017=CARTESIAN_POINT('Ctrl Pts',(-1.93269066517936,1.,-0.459081234547931));
#45018=CARTESIAN_POINT('Ctrl Pts',(-1.92753067150461,-1.,-0.455872005174335));
#45019=CARTESIAN_POINT('Ctrl Pts',(-1.92753067150461,1.,-0.455872005174335));
#45020=CARTESIAN_POINT('Ctrl Pts',(-1.9223538064847,-1.,-0.452719478359356));
#45021=CARTESIAN_POINT('Ctrl Pts',(-1.9223538064847,1.,-0.452719478359356));
#45022=CARTESIAN_POINT('Ctrl Pts',(-1.91718342555717,-1.,-0.449632260106572));
#45023=CARTESIAN_POINT('Ctrl Pts',(-1.91718342555717,1.,-0.449632260106572));
#45024=CARTESIAN_POINT('Ctrl Pts',(-1.91203699981095,-1.,-0.446617343485651));
#45025=CARTESIAN_POINT('Ctrl Pts',(-1.91203699981095,1.,-0.446617343485651));
#45026=CARTESIAN_POINT('Ctrl Pts',(-1.90691756144906,-1.,-0.44367755684917));
#45027=CARTESIAN_POINT('Ctrl Pts',(-1.90691756144906,1.,-0.44367755684917));
#45028=CARTESIAN_POINT('Ctrl Pts',(-1.90180124389137,-1.,-0.44080783370416));
#45029=CARTESIAN_POINT('Ctrl Pts',(-1.90180124389137,1.,-0.44080783370416));
#45030=CARTESIAN_POINT('Ctrl Pts',(-1.89663648956549,-1.,-0.437995003948443));
#45031=CARTESIAN_POINT('Ctrl Pts',(-1.89663648956549,1.,-0.437995003948443));
#45032=CARTESIAN_POINT('Ctrl Pts',(-1.89136993975585,-1.,-0.43522566096358));
#45033=CARTESIAN_POINT('Ctrl Pts',(-1.89136993975585,1.,-0.43522566096358));
#45034=CARTESIAN_POINT('Ctrl Pts',(-1.88596913666828,-1.,-0.432493038548833));
#45035=CARTESIAN_POINT('Ctrl Pts',(-1.88596913666828,1.,-0.432493038548833));
#45036=CARTESIAN_POINT('Ctrl Pts',(-1.88044229001778,-1.,-0.429803062482217));
#45037=CARTESIAN_POINT('Ctrl Pts',(-1.88044229001778,1.,-0.429803062482217));
#45038=CARTESIAN_POINT('Ctrl Pts',(-1.87486989291333,-1.,-0.427183828518743));
#45039=CARTESIAN_POINT('Ctrl Pts',(-1.87486989291333,1.,-0.427183828518743));
#45040=CARTESIAN_POINT('Ctrl Pts',(-1.8693780394412,-1.,-0.424678177290876));
#45041=CARTESIAN_POINT('Ctrl Pts',(-1.8693780394412,1.,-0.424678177290876));
#45042=CARTESIAN_POINT('Ctrl Pts',(-1.86408083333863,-1.,-0.422327307417884));
#45043=CARTESIAN_POINT('Ctrl Pts',(-1.86408083333863,1.,-0.422327307417884));
#45044=CARTESIAN_POINT('Ctrl Pts',(-1.8590328109667,-1.,-0.420157287975583));
#45045=CARTESIAN_POINT('Ctrl Pts',(-1.8590328109667,1.,-0.420157287975583));
#45046=CARTESIAN_POINT('Ctrl Pts',(-1.8541763285645,-1.,-0.418164129144045));
#45047=CARTESIAN_POINT('Ctrl Pts',(-1.8541763285645,1.,-0.418164129144045));
#45048=CARTESIAN_POINT('Ctrl Pts',(-1.84929312930314,-1.,-0.416300022039885));
#45049=CARTESIAN_POINT('Ctrl Pts',(-1.84929312930314,1.,-0.416300022039885));
#45050=CARTESIAN_POINT('Ctrl Pts',(-1.84405757074218,-1.,-0.414487438255542));
#45051=CARTESIAN_POINT('Ctrl Pts',(-1.84405757074218,1.,-0.414487438255542));
#45052=CARTESIAN_POINT('Ctrl Pts',(-1.8380895347617,-1.,-0.412633125322945));
#45053=CARTESIAN_POINT('Ctrl Pts',(-1.8380895347617,1.,-0.412633125322945));
#45054=CARTESIAN_POINT('Ctrl Pts',(-1.83100408895047,-1.,-0.410641256301276));
#45055=CARTESIAN_POINT('Ctrl Pts',(-1.83100408895047,1.,-0.410641256301276));
#45056=CARTESIAN_POINT('Ctrl Pts',(-1.82247022677562,-1.,-0.408428948106227));
#45057=CARTESIAN_POINT('Ctrl Pts',(-1.82247022677562,1.,-0.408428948106227));
#45058=CARTESIAN_POINT('Ctrl Pts',(-1.81223801812013,-1.,-0.405933518407175));
#45059=CARTESIAN_POINT('Ctrl Pts',(-1.81223801812013,1.,-0.405933518407175));
#45060=CARTESIAN_POINT('Ctrl Pts',(-1.80012077173238,-1.,-0.403107976163396));
#45061=CARTESIAN_POINT('Ctrl Pts',(-1.80012077173238,1.,-0.403107976163396));
#45062=CARTESIAN_POINT('Ctrl Pts',(-1.78598826343754,-1.,-0.399919403774155));
#45063=CARTESIAN_POINT('Ctrl Pts',(-1.78598826343754,1.,-0.399919403774155));
#45064=CARTESIAN_POINT('Ctrl Pts',(-1.76975560043442,-1.,-0.396346196110688));
#45065=CARTESIAN_POINT('Ctrl Pts',(-1.76975560043442,1.,-0.396346196110688));
#45066=CARTESIAN_POINT('Ctrl Pts',(-1.75137405310193,-1.,-0.392375812285395));
#45067=CARTESIAN_POINT('Ctrl Pts',(-1.75137405310193,1.,-0.392375812285395));
#45068=CARTESIAN_POINT('Ctrl Pts',(-1.73493170972829,-1.,-0.388877023502615));
#45069=CARTESIAN_POINT('Ctrl Pts',(-1.73493170972829,1.,-0.388877023502615));
#45070=CARTESIAN_POINT('Ctrl Pts',(-1.72162022244582,-1.,-0.386070790323281));
#45071=CARTESIAN_POINT('Ctrl Pts',(-1.72162022244582,1.,-0.386070790323281));
#45072=CARTESIAN_POINT('Ctrl Pts',(-1.71231062891398,-1.,-0.384119047314215));
#45073=CARTESIAN_POINT('Ctrl Pts',(-1.71231062891398,1.,-0.384119047314215));
#45074=CARTESIAN_POINT('Ctrl Pts',(-1.7075470150345,-1.,-0.383122945602004));
#45075=CARTESIAN_POINT('Ctrl Pts',(-1.7075470150345,1.,-0.383122945602004));
#45076=CARTESIAN_POINT('',(-2.11275013067528,1.,-0.61342227326009));
#45077=CARTESIAN_POINT('Ctrl Pts',(-2.11275013067528,1.,-0.61342227326009));
#45078=CARTESIAN_POINT('Ctrl Pts',(-2.11187554260142,1.,-0.61246736556225));
#45079=CARTESIAN_POINT('Ctrl Pts',(-2.11012443807661,1.,-0.610560911691113));
#45080=CARTESIAN_POINT('Ctrl Pts',(-2.10749199615859,1.,-0.607711315456826));
#45081=CARTESIAN_POINT('Ctrl Pts',(-2.10397049887709,1.,-0.603932030738212));
#45082=CARTESIAN_POINT('Ctrl Pts',(-2.09954930865331,1.,-0.599241616422144));
#45083=CARTESIAN_POINT('Ctrl Pts',(-2.09510876220501,1.,-0.594585006052823));
#45084=CARTESIAN_POINT('Ctrl Pts',(-2.09064881812053,1.,-0.589962365403189));
#45085=CARTESIAN_POINT('Ctrl Pts',(-2.086169437277,1.,-0.585373918990895));
#45086=CARTESIAN_POINT('Ctrl Pts',(-2.08167059018138,1.,-0.580819952107257));
#45087=CARTESIAN_POINT('Ctrl Pts',(-2.07715226767361,1.,-0.576300797416274));
#45088=CARTESIAN_POINT('Ctrl Pts',(-2.07261449292757,1.,-0.571816823242411));
#45089=CARTESIAN_POINT('Ctrl Pts',(-2.06805732997383,1.,-0.567368421181229));
#45090=CARTESIAN_POINT('Ctrl Pts',(-2.06348090160697,1.,-0.562955993082574));
#45091=CARTESIAN_POINT('Ctrl Pts',(-2.05888537756571,1.,-0.558579940185467));
#45092=CARTESIAN_POINT('Ctrl Pts',(-2.05427091604482,1.,-0.554240657464109));
#45093=CARTESIAN_POINT('Ctrl Pts',(-2.04963761077974,1.,-0.549938525150342));
#45094=CARTESIAN_POINT('Ctrl Pts',(-2.0449854471456,1.,-0.545673903817348));
#45095=CARTESIAN_POINT('Ctrl Pts',(-2.0403142269048,1.,-0.54144712061552));
#45096=CARTESIAN_POINT('Ctrl Pts',(-2.03562362953993,1.,-0.537258489833134));
#45097=CARTESIAN_POINT('Ctrl Pts',(-2.03091336214401,1.,-0.533108355132905));
#45098=CARTESIAN_POINT('Ctrl Pts',(-2.02618329083289,1.,-0.52899712724191));
#45099=CARTESIAN_POINT('Ctrl Pts',(-2.02143356304712,1.,-0.524925318333518));
#45100=CARTESIAN_POINT('Ctrl Pts',(-2.01666477917305,1.,-0.520893590399428));
#45101=CARTESIAN_POINT('Ctrl Pts',(-2.01187773939257,1.,-0.516902681728733));
#45102=CARTESIAN_POINT('Ctrl Pts',(-2.00707309946955,1.,-0.512953306961813));
#45103=CARTESIAN_POINT('Ctrl Pts',(-2.00225107134733,1.,-0.509046069886152));
#45104=CARTESIAN_POINT('Ctrl Pts',(-1.99741107463567,1.,-0.505181361323011));
#45105=CARTESIAN_POINT('Ctrl Pts',(-1.9925514912615,1.,-0.501359287727129));
#45106=CARTESIAN_POINT('Ctrl Pts',(-1.98767044752929,1.,-0.497579909545564));
#45107=CARTESIAN_POINT('Ctrl Pts',(-1.9827665876182,1.,-0.493843476541492));
#45108=CARTESIAN_POINT('Ctrl Pts',(-1.97783973019229,1.,-0.490150627860955));
#45109=CARTESIAN_POINT('Ctrl Pts',(-1.97289186263272,1.,-0.486502692907661));
#45110=CARTESIAN_POINT('Ctrl Pts',(-1.96792703422358,1.,-0.482901662120686));
#45111=CARTESIAN_POINT('Ctrl Pts',(-1.96294933055938,1.,-0.479349583074846));
#45112=CARTESIAN_POINT('Ctrl Pts',(-1.95796111148175,1.,-0.475848034683171));
#45113=CARTESIAN_POINT('Ctrl Pts',(-1.95296148278136,1.,-0.472397672264079));
#45114=CARTESIAN_POINT('Ctrl Pts',(-1.94794381136524,1.,-0.468997482913158));
#45115=CARTESIAN_POINT('Ctrl Pts',(-1.94289794196205,1.,-0.465645462026064));
#45116=CARTESIAN_POINT('Ctrl Pts',(-1.93781486640834,1.,-0.462340031009087));
#45117=CARTESIAN_POINT('Ctrl Pts',(-1.93269066517936,1.,-0.459081234547931));
#45118=CARTESIAN_POINT('Ctrl Pts',(-1.92753067150461,1.,-0.455872005174335));
#45119=CARTESIAN_POINT('Ctrl Pts',(-1.9223538064847,1.,-0.452719478359356));
#45120=CARTESIAN_POINT('Ctrl Pts',(-1.91718342555717,1.,-0.449632260106572));
#45121=CARTESIAN_POINT('Ctrl Pts',(-1.91203699981095,1.,-0.446617343485651));
#45122=CARTESIAN_POINT('Ctrl Pts',(-1.90691756144906,1.,-0.44367755684917));
#45123=CARTESIAN_POINT('Ctrl Pts',(-1.90180124389137,1.,-0.44080783370416));
#45124=CARTESIAN_POINT('Ctrl Pts',(-1.89663648956549,1.,-0.437995003948443));
#45125=CARTESIAN_POINT('Ctrl Pts',(-1.89136993975585,1.,-0.43522566096358));
#45126=CARTESIAN_POINT('Ctrl Pts',(-1.88596913666828,1.,-0.432493038548833));
#45127=CARTESIAN_POINT('Ctrl Pts',(-1.88044229001778,1.,-0.429803062482217));
#45128=CARTESIAN_POINT('Ctrl Pts',(-1.87486989291333,1.,-0.427183828518743));
#45129=CARTESIAN_POINT('Ctrl Pts',(-1.8693780394412,1.,-0.424678177290876));
#45130=CARTESIAN_POINT('Ctrl Pts',(-1.86408083333863,1.,-0.422327307417884));
#45131=CARTESIAN_POINT('Ctrl Pts',(-1.8590328109667,1.,-0.420157287975583));
#45132=CARTESIAN_POINT('Ctrl Pts',(-1.8541763285645,1.,-0.418164129144045));
#45133=CARTESIAN_POINT('Ctrl Pts',(-1.84929312930314,1.,-0.416300022039885));
#45134=CARTESIAN_POINT('Ctrl Pts',(-1.84405757074218,1.,-0.414487438255542));
#45135=CARTESIAN_POINT('Ctrl Pts',(-1.8380895347617,1.,-0.412633125322945));
#45136=CARTESIAN_POINT('Ctrl Pts',(-1.83100408895047,1.,-0.410641256301276));
#45137=CARTESIAN_POINT('Ctrl Pts',(-1.82247022677562,1.,-0.408428948106227));
#45138=CARTESIAN_POINT('Ctrl Pts',(-1.81223801812013,1.,-0.405933518407175));
#45139=CARTESIAN_POINT('Ctrl Pts',(-1.80012077173238,1.,-0.403107976163396));
#45140=CARTESIAN_POINT('Ctrl Pts',(-1.78598826343754,1.,-0.399919403774155));
#45141=CARTESIAN_POINT('Ctrl Pts',(-1.76975560043442,1.,-0.396346196110688));
#45142=CARTESIAN_POINT('Ctrl Pts',(-1.75137405310193,1.,-0.392375812285395));
#45143=CARTESIAN_POINT('Ctrl Pts',(-1.73493170972829,1.,-0.388877023502615));
#45144=CARTESIAN_POINT('Ctrl Pts',(-1.72162022244582,1.,-0.386070790323281));
#45145=CARTESIAN_POINT('Ctrl Pts',(-1.71231062891398,1.,-0.384119047314215));
#45146=CARTESIAN_POINT('Ctrl Pts',(-1.7075470150345,1.,-0.383122945602004));
#45147=CARTESIAN_POINT('',(-2.11275013067528,0.,-0.61342227326009));
#45148=CARTESIAN_POINT('Origin',(-2.0698113262342,0.,-0.745574324794401));
#45149=CARTESIAN_POINT('',(-2.0698113262342,1.,-0.745574324794401));
#45150=CARTESIAN_POINT('',(-2.11275013067528,1.,-0.61342227326009));
#45151=CARTESIAN_POINT('',(-2.0698113262342,0.,-0.745574324794401));
#45152=CARTESIAN_POINT('Ctrl Pts',(-1.60662857109684,-1.,-0.693717979106306));
#45153=CARTESIAN_POINT('Ctrl Pts',(-1.60662857109684,1.,-0.693717979106306));
#45154=CARTESIAN_POINT('Ctrl Pts',(-1.61106790958151,-1.,-0.695712097881194));
#45155=CARTESIAN_POINT('Ctrl Pts',(-1.61106790958151,1.,-0.695712097881194));
#45156=CARTESIAN_POINT('Ctrl Pts',(-1.61974673472612,-1.,-0.699605146405088));
#45157=CARTESIAN_POINT('Ctrl Pts',(-1.61974673472612,1.,-0.699605146405088));
#45158=CARTESIAN_POINT('Ctrl Pts',(-1.63216541664676,-1.,-0.705159151988319));
#45159=CARTESIAN_POINT('Ctrl Pts',(-1.63216541664676,1.,-0.705159151988319));
#45160=CARTESIAN_POINT('Ctrl Pts',(-1.64752408832016,-1.,-0.711993139355394));
#45161=CARTESIAN_POINT('Ctrl Pts',(-1.64752408832016,1.,-0.711993139355394));
#45162=CARTESIAN_POINT('Ctrl Pts',(-1.6647288055568,-1.,-0.719585433804282));
#45163=CARTESIAN_POINT('Ctrl Pts',(-1.6647288055568,1.,-0.719585433804282));
#45164=CARTESIAN_POINT('Ctrl Pts',(-1.67996158455503,-1.,-0.726235967997433));
#45165=CARTESIAN_POINT('Ctrl Pts',(-1.67996158455503,1.,-0.726235967997433));
#45166=CARTESIAN_POINT('Ctrl Pts',(-1.69326921975743,-1.,-0.731963238697195));
#45167=CARTESIAN_POINT('Ctrl Pts',(-1.69326921975743,1.,-0.731963238697195));
#45168=CARTESIAN_POINT('Ctrl Pts',(-1.70473309006121,-1.,-0.736799665724771));
#45169=CARTESIAN_POINT('Ctrl Pts',(-1.70473309006121,1.,-0.736799665724771));
#45170=CARTESIAN_POINT('Ctrl Pts',(-1.71447789751927,-1.,-0.740795162032087));
#45171=CARTESIAN_POINT('Ctrl Pts',(-1.71447789751927,1.,-0.740795162032087));
#45172=CARTESIAN_POINT('Ctrl Pts',(-1.7226822991693,-1.,-0.744021445433764));
#45173=CARTESIAN_POINT('Ctrl Pts',(-1.7226822991693,1.,-0.744021445433764));
#45174=CARTESIAN_POINT('Ctrl Pts',(-1.72958533647399,-1.,-0.746574710096436));
#45175=CARTESIAN_POINT('Ctrl Pts',(-1.72958533647399,1.,-0.746574710096436));
#45176=CARTESIAN_POINT('Ctrl Pts',(-1.73550351679848,-1.,-0.748582462954854));
#45177=CARTESIAN_POINT('Ctrl Pts',(-1.73550351679848,1.,-0.748582462954854));
#45178=CARTESIAN_POINT('Ctrl Pts',(-1.74080458266705,-1.,-0.75019343597954));
#45179=CARTESIAN_POINT('Ctrl Pts',(-1.74080458266705,1.,-0.75019343597954));
#45180=CARTESIAN_POINT('Ctrl Pts',(-1.74585086852298,-1.,-0.751555614163629));
#45181=CARTESIAN_POINT('Ctrl Pts',(-1.74585086852298,1.,-0.751555614163629));
#45182=CARTESIAN_POINT('Ctrl Pts',(-1.75095139468809,-1.,-0.752797683531377));
#45183=CARTESIAN_POINT('Ctrl Pts',(-1.75095139468809,1.,-0.752797683531377));
#45184=CARTESIAN_POINT('Ctrl Pts',(-1.75631083600175,-1.,-0.75400925402848));
#45185=CARTESIAN_POINT('Ctrl Pts',(-1.75631083600175,1.,-0.75400925402848));
#45186=CARTESIAN_POINT('Ctrl Pts',(-1.7619781724032,-1.,-0.755220979975262));
#45187=CARTESIAN_POINT('Ctrl Pts',(-1.7619781724032,1.,-0.755220979975262));
#45188=CARTESIAN_POINT('Ctrl Pts',(-1.76789396003141,-1.,-0.756421896028403));
#45189=CARTESIAN_POINT('Ctrl Pts',(-1.76789396003141,1.,-0.756421896028403));
#45190=CARTESIAN_POINT('Ctrl Pts',(-1.77394167108342,-1.,-0.757578264077238));
#45191=CARTESIAN_POINT('Ctrl Pts',(-1.77394167108342,1.,-0.757578264077238));
#45192=CARTESIAN_POINT('Ctrl Pts',(-1.77999411220912,-1.,-0.75865062667738));
#45193=CARTESIAN_POINT('Ctrl Pts',(-1.77999411220912,1.,-0.75865062667738));
#45194=CARTESIAN_POINT('Ctrl Pts',(-1.78596964884526,-1.,-0.759614401109868));
#45195=CARTESIAN_POINT('Ctrl Pts',(-1.78596964884526,1.,-0.759614401109868));
#45196=CARTESIAN_POINT('Ctrl Pts',(-1.79185815610802,-1.,-0.760469555880425));
#45197=CARTESIAN_POINT('Ctrl Pts',(-1.79185815610802,1.,-0.760469555880425));
#45198=CARTESIAN_POINT('Ctrl Pts',(-1.79768986997735,-1.,-0.761229695230359));
#45199=CARTESIAN_POINT('Ctrl Pts',(-1.79768986997735,1.,-0.761229695230359));
#45200=CARTESIAN_POINT('Ctrl Pts',(-1.80351583877334,-1.,-0.761915336443515));
#45201=CARTESIAN_POINT('Ctrl Pts',(-1.80351583877334,1.,-0.761915336443515));
#45202=CARTESIAN_POINT('Ctrl Pts',(-1.80938551463989,-1.,-0.762546129464036));
#45203=CARTESIAN_POINT('Ctrl Pts',(-1.80938551463989,1.,-0.762546129464036));
#45204=CARTESIAN_POINT('Ctrl Pts',(-1.81532118405566,-1.,-0.763132003836783));
#45205=CARTESIAN_POINT('Ctrl Pts',(-1.81532118405566,1.,-0.763132003836783));
#45206=CARTESIAN_POINT('Ctrl Pts',(-1.82131873145297,-1.,-0.763673465462854));
#45207=CARTESIAN_POINT('Ctrl Pts',(-1.82131873145297,1.,-0.763673465462854));
#45208=CARTESIAN_POINT('Ctrl Pts',(-1.8273599120008,-1.,-0.764165902606055));
#45209=CARTESIAN_POINT('Ctrl Pts',(-1.8273599120008,1.,-0.764165902606055));
#45210=CARTESIAN_POINT('Ctrl Pts',(-1.8334207722714,-1.,-0.764602549687845));
#45211=CARTESIAN_POINT('Ctrl Pts',(-1.8334207722714,1.,-0.764602549687845));
#45212=CARTESIAN_POINT('Ctrl Pts',(-1.83948181064823,-1.,-0.764978057881687));
#45213=CARTESIAN_POINT('Ctrl Pts',(-1.83948181064823,1.,-0.764978057881687));
#45214=CARTESIAN_POINT('Ctrl Pts',(-1.8455369887591,-1.,-0.765291664861971));
#45215=CARTESIAN_POINT('Ctrl Pts',(-1.8455369887591,1.,-0.765291664861971));
#45216=CARTESIAN_POINT('Ctrl Pts',(-1.85158945130054,-1.,-0.765545710619023));
#45217=CARTESIAN_POINT('Ctrl Pts',(-1.85158945130054,1.,-0.765545710619023));
#45218=CARTESIAN_POINT('Ctrl Pts',(-1.85764741390391,-1.,-0.765744212909305));
#45219=CARTESIAN_POINT('Ctrl Pts',(-1.85764741390391,1.,-0.765744212909305));
#45220=CARTESIAN_POINT('Ctrl Pts',(-1.86372027063314,-1.,-0.765891519092557));
#45221=CARTESIAN_POINT('Ctrl Pts',(-1.86372027063314,1.,-0.765891519092557));
#45222=CARTESIAN_POINT('Ctrl Pts',(-1.86981398314345,-1.,-0.765990708546111));
#45223=CARTESIAN_POINT('Ctrl Pts',(-1.86981398314345,1.,-0.765990708546111));
#45224=CARTESIAN_POINT('Ctrl Pts',(-1.87592888967886,-1.,-0.766042837036759));
#45225=CARTESIAN_POINT('Ctrl Pts',(-1.87592888967886,1.,-0.766042837036759));
#45226=CARTESIAN_POINT('Ctrl Pts',(-1.88206215302561,-1.,-0.766047794851868));
#45227=CARTESIAN_POINT('Ctrl Pts',(-1.88206215302561,1.,-0.766047794851868));
#45228=CARTESIAN_POINT('Ctrl Pts',(-1.88820926433409,-1.,-0.76600483706209));
#45229=CARTESIAN_POINT('Ctrl Pts',(-1.88820926433409,1.,-0.76600483706209));
#45230=CARTESIAN_POINT('Ctrl Pts',(-1.89436577771389,-1.,-0.765913193856979));
#45231=CARTESIAN_POINT('Ctrl Pts',(-1.89436577771389,1.,-0.765913193856979));
#45232=CARTESIAN_POINT('Ctrl Pts',(-1.90052930393599,-1.,-0.765772772593395));
#45233=CARTESIAN_POINT('Ctrl Pts',(-1.90052930393599,1.,-0.765772772593395));
#45234=CARTESIAN_POINT('Ctrl Pts',(-1.90669961402362,-1.,-0.765584196937936));
#45235=CARTESIAN_POINT('Ctrl Pts',(-1.90669961402362,1.,-0.765584196937936));
#45236=CARTESIAN_POINT('Ctrl Pts',(-1.91287765805174,-1.,-0.765348465884739));
#45237=CARTESIAN_POINT('Ctrl Pts',(-1.91287765805174,1.,-0.765348465884739));
#45238=CARTESIAN_POINT('Ctrl Pts',(-1.91906491634197,-1.,-0.765066729667095));
#45239=CARTESIAN_POINT('Ctrl Pts',(-1.91906491634197,1.,-0.765066729667095));
#45240=CARTESIAN_POINT('Ctrl Pts',(-1.92526263537041,-1.,-0.764740025488189));
#45241=CARTESIAN_POINT('Ctrl Pts',(-1.92526263537041,1.,-0.764740025488189));
#45242=CARTESIAN_POINT('Ctrl Pts',(-1.93147105496367,-1.,-0.764369010673889));
#45243=CARTESIAN_POINT('Ctrl Pts',(-1.93147105496367,1.,-0.764369010673889));
#45244=CARTESIAN_POINT('Ctrl Pts',(-1.93768964875867,-1.,-0.763954049121393));
#45245=CARTESIAN_POINT('Ctrl Pts',(-1.93768964875867,1.,-0.763954049121393));
#45246=CARTESIAN_POINT('Ctrl Pts',(-1.94391746617626,-1.,-0.76349533353858));
#45247=CARTESIAN_POINT('Ctrl Pts',(-1.94391746617626,1.,-0.76349533353858));
#45248=CARTESIAN_POINT('Ctrl Pts',(-1.95015342590025,-1.,-0.762992990878774));
#45249=CARTESIAN_POINT('Ctrl Pts',(-1.95015342590025,1.,-0.762992990878774));
#45250=CARTESIAN_POINT('Ctrl Pts',(-1.95639665309893,-1.,-0.762447203806263));
#45251=CARTESIAN_POINT('Ctrl Pts',(-1.95639665309893,1.,-0.762447203806263));
#45252=CARTESIAN_POINT('Ctrl Pts',(-1.96264672744229,-1.,-0.761858300014575));
#45253=CARTESIAN_POINT('Ctrl Pts',(-1.96264672744229,1.,-0.761858300014575));
#45254=CARTESIAN_POINT('Ctrl Pts',(-1.96890351582545,-1.,-0.761226690483986));
#45255=CARTESIAN_POINT('Ctrl Pts',(-1.96890351582545,1.,-0.761226690483986));
#45256=CARTESIAN_POINT('Ctrl Pts',(-1.97516705321521,-1.,-0.760552825409855));
#45257=CARTESIAN_POINT('Ctrl Pts',(-1.97516705321521,1.,-0.760552825409855));
#45258=CARTESIAN_POINT('Ctrl Pts',(-1.98143741418156,-1.,-0.759837147452135));
#45259=CARTESIAN_POINT('Ctrl Pts',(-1.98143741418156,1.,-0.759837147452135));
#45260=CARTESIAN_POINT('Ctrl Pts',(-1.98771456680806,-1.,-0.759080037802242));
#45261=CARTESIAN_POINT('Ctrl Pts',(-1.98771456680806,1.,-0.759080037802242));
#45262=CARTESIAN_POINT('Ctrl Pts',(-1.9939983109871,-1.,-0.758281796766377));
#45263=CARTESIAN_POINT('Ctrl Pts',(-1.9939983109871,1.,-0.758281796766377));
#45264=CARTESIAN_POINT('Ctrl Pts',(-2.00028834739072,-1.,-0.757442676862341));
#45265=CARTESIAN_POINT('Ctrl Pts',(-2.00028834739072,1.,-0.757442676862341));
#45266=CARTESIAN_POINT('Ctrl Pts',(-2.00658431587682,-1.,-0.756562904646496));
#45267=CARTESIAN_POINT('Ctrl Pts',(-2.00658431587682,1.,-0.756562904646496));
#45268=CARTESIAN_POINT('Ctrl Pts',(-2.01288584328149,-1.,-0.7556427049581));
#45269=CARTESIAN_POINT('Ctrl Pts',(-2.01288584328149,1.,-0.7556427049581));
#45270=CARTESIAN_POINT('Ctrl Pts',(-2.01919259406003,-1.,-0.75468233072352));
#45271=CARTESIAN_POINT('Ctrl Pts',(-2.01919259406003,1.,-0.75468233072352));
#45272=CARTESIAN_POINT('Ctrl Pts',(-2.02550428623587,-1.,-0.753682061113765));
#45273=CARTESIAN_POINT('Ctrl Pts',(-2.02550428623587,1.,-0.753682061113765));
#45274=CARTESIAN_POINT('Ctrl Pts',(-2.03182068456467,-1.,-0.752642180488104));
#45275=CARTESIAN_POINT('Ctrl Pts',(-2.03182068456467,1.,-0.752642180488104));
#45276=CARTESIAN_POINT('Ctrl Pts',(-2.03814160092173,-1.,-0.751562963361383));
#45277=CARTESIAN_POINT('Ctrl Pts',(-2.03814160092173,1.,-0.751562963361383));
#45278=CARTESIAN_POINT('Ctrl Pts',(-2.04446689147754,-1.,-0.750444657874758));
#45279=CARTESIAN_POINT('Ctrl Pts',(-2.04446689147754,1.,-0.750444657874758));
#45280=CARTESIAN_POINT('Ctrl Pts',(-2.05079645591606,-1.,-0.749287468663053));
#45281=CARTESIAN_POINT('Ctrl Pts',(-2.05079645591606,1.,-0.749287468663053));
#45282=CARTESIAN_POINT('Ctrl Pts',(-2.05713023030263,-1.,-0.748091554181101));
#45283=CARTESIAN_POINT('Ctrl Pts',(-2.05713023030263,1.,-0.748091554181101));
#45284=CARTESIAN_POINT('Ctrl Pts',(-2.06220058927162,-1.,-0.747103932785504));
#45285=CARTESIAN_POINT('Ctrl Pts',(-2.06220058927162,1.,-0.747103932785504));
#45286=CARTESIAN_POINT('Ctrl Pts',(-2.06600523016401,-1.,-0.746345871542695));
#45287=CARTESIAN_POINT('Ctrl Pts',(-2.06600523016401,1.,-0.746345871542695));
#45288=CARTESIAN_POINT('Ctrl Pts',(-2.06854248895575,-1.,-0.74583279137781));
#45289=CARTESIAN_POINT('Ctrl Pts',(-2.06854248895575,1.,-0.74583279137781));
#45290=CARTESIAN_POINT('Ctrl Pts',(-2.0698113262342,-1.,-0.745574324794401));
#45291=CARTESIAN_POINT('Ctrl Pts',(-2.0698113262342,1.,-0.745574324794401));
#45292=CARTESIAN_POINT('',(-1.60662857109684,1.,-0.693717979106306));
#45293=CARTESIAN_POINT('Ctrl Pts',(-1.60662857109684,1.,-0.693717979106306));
#45294=CARTESIAN_POINT('Ctrl Pts',(-1.61106790958151,1.,-0.695712097881194));
#45295=CARTESIAN_POINT('Ctrl Pts',(-1.61974673472612,1.,-0.699605146405088));
#45296=CARTESIAN_POINT('Ctrl Pts',(-1.63216541664676,1.,-0.705159151988319));
#45297=CARTESIAN_POINT('Ctrl Pts',(-1.64752408832016,1.,-0.711993139355394));
#45298=CARTESIAN_POINT('Ctrl Pts',(-1.6647288055568,1.,-0.719585433804282));
#45299=CARTESIAN_POINT('Ctrl Pts',(-1.67996158455503,1.,-0.726235967997433));
#45300=CARTESIAN_POINT('Ctrl Pts',(-1.69326921975743,1.,-0.731963238697195));
#45301=CARTESIAN_POINT('Ctrl Pts',(-1.70473309006121,1.,-0.736799665724771));
#45302=CARTESIAN_POINT('Ctrl Pts',(-1.71447789751927,1.,-0.740795162032087));
#45303=CARTESIAN_POINT('Ctrl Pts',(-1.7226822991693,1.,-0.744021445433764));
#45304=CARTESIAN_POINT('Ctrl Pts',(-1.72958533647399,1.,-0.746574710096436));
#45305=CARTESIAN_POINT('Ctrl Pts',(-1.73550351679848,1.,-0.748582462954854));
#45306=CARTESIAN_POINT('Ctrl Pts',(-1.74080458266705,1.,-0.75019343597954));
#45307=CARTESIAN_POINT('Ctrl Pts',(-1.74585086852298,1.,-0.751555614163629));
#45308=CARTESIAN_POINT('Ctrl Pts',(-1.75095139468809,1.,-0.752797683531377));
#45309=CARTESIAN_POINT('Ctrl Pts',(-1.75631083600175,1.,-0.75400925402848));
#45310=CARTESIAN_POINT('Ctrl Pts',(-1.7619781724032,1.,-0.755220979975262));
#45311=CARTESIAN_POINT('Ctrl Pts',(-1.76789396003141,1.,-0.756421896028403));
#45312=CARTESIAN_POINT('Ctrl Pts',(-1.77394167108342,1.,-0.757578264077238));
#45313=CARTESIAN_POINT('Ctrl Pts',(-1.77999411220912,1.,-0.75865062667738));
#45314=CARTESIAN_POINT('Ctrl Pts',(-1.78596964884526,1.,-0.759614401109868));
#45315=CARTESIAN_POINT('Ctrl Pts',(-1.79185815610802,1.,-0.760469555880425));
#45316=CARTESIAN_POINT('Ctrl Pts',(-1.79768986997735,1.,-0.761229695230359));
#45317=CARTESIAN_POINT('Ctrl Pts',(-1.80351583877334,1.,-0.761915336443515));
#45318=CARTESIAN_POINT('Ctrl Pts',(-1.80938551463989,1.,-0.762546129464036));
#45319=CARTESIAN_POINT('Ctrl Pts',(-1.81532118405566,1.,-0.763132003836783));
#45320=CARTESIAN_POINT('Ctrl Pts',(-1.82131873145297,1.,-0.763673465462854));
#45321=CARTESIAN_POINT('Ctrl Pts',(-1.8273599120008,1.,-0.764165902606055));
#45322=CARTESIAN_POINT('Ctrl Pts',(-1.8334207722714,1.,-0.764602549687845));
#45323=CARTESIAN_POINT('Ctrl Pts',(-1.83948181064823,1.,-0.764978057881687));
#45324=CARTESIAN_POINT('Ctrl Pts',(-1.8455369887591,1.,-0.765291664861971));
#45325=CARTESIAN_POINT('Ctrl Pts',(-1.85158945130054,1.,-0.765545710619023));
#45326=CARTESIAN_POINT('Ctrl Pts',(-1.85764741390391,1.,-0.765744212909305));
#45327=CARTESIAN_POINT('Ctrl Pts',(-1.86372027063314,1.,-0.765891519092557));
#45328=CARTESIAN_POINT('Ctrl Pts',(-1.86981398314345,1.,-0.765990708546111));
#45329=CARTESIAN_POINT('Ctrl Pts',(-1.87592888967886,1.,-0.766042837036759));
#45330=CARTESIAN_POINT('Ctrl Pts',(-1.88206215302561,1.,-0.766047794851868));
#45331=CARTESIAN_POINT('Ctrl Pts',(-1.88820926433409,1.,-0.76600483706209));
#45332=CARTESIAN_POINT('Ctrl Pts',(-1.89436577771389,1.,-0.765913193856979));
#45333=CARTESIAN_POINT('Ctrl Pts',(-1.90052930393599,1.,-0.765772772593395));
#45334=CARTESIAN_POINT('Ctrl Pts',(-1.90669961402362,1.,-0.765584196937936));
#45335=CARTESIAN_POINT('Ctrl Pts',(-1.91287765805174,1.,-0.765348465884739));
#45336=CARTESIAN_POINT('Ctrl Pts',(-1.91906491634197,1.,-0.765066729667095));
#45337=CARTESIAN_POINT('Ctrl Pts',(-1.92526263537041,1.,-0.764740025488189));
#45338=CARTESIAN_POINT('Ctrl Pts',(-1.93147105496367,1.,-0.764369010673889));
#45339=CARTESIAN_POINT('Ctrl Pts',(-1.93768964875867,1.,-0.763954049121393));
#45340=CARTESIAN_POINT('Ctrl Pts',(-1.94391746617626,1.,-0.76349533353858));
#45341=CARTESIAN_POINT('Ctrl Pts',(-1.95015342590025,1.,-0.762992990878774));
#45342=CARTESIAN_POINT('Ctrl Pts',(-1.95639665309893,1.,-0.762447203806263));
#45343=CARTESIAN_POINT('Ctrl Pts',(-1.96264672744229,1.,-0.761858300014575));
#45344=CARTESIAN_POINT('Ctrl Pts',(-1.96890351582545,1.,-0.761226690483986));
#45345=CARTESIAN_POINT('Ctrl Pts',(-1.97516705321521,1.,-0.760552825409855));
#45346=CARTESIAN_POINT('Ctrl Pts',(-1.98143741418156,1.,-0.759837147452135));
#45347=CARTESIAN_POINT('Ctrl Pts',(-1.98771456680806,1.,-0.759080037802242));
#45348=CARTESIAN_POINT('Ctrl Pts',(-1.9939983109871,1.,-0.758281796766377));
#45349=CARTESIAN_POINT('Ctrl Pts',(-2.00028834739072,1.,-0.757442676862341));
#45350=CARTESIAN_POINT('Ctrl Pts',(-2.00658431587682,1.,-0.756562904646496));
#45351=CARTESIAN_POINT('Ctrl Pts',(-2.01288584328149,1.,-0.7556427049581));
#45352=CARTESIAN_POINT('Ctrl Pts',(-2.01919259406003,1.,-0.75468233072352));
#45353=CARTESIAN_POINT('Ctrl Pts',(-2.02550428623587,1.,-0.753682061113765));
#45354=CARTESIAN_POINT('Ctrl Pts',(-2.03182068456467,1.,-0.752642180488104));
#45355=CARTESIAN_POINT('Ctrl Pts',(-2.03814160092173,1.,-0.751562963361383));
#45356=CARTESIAN_POINT('Ctrl Pts',(-2.04446689147754,1.,-0.750444657874758));
#45357=CARTESIAN_POINT('Ctrl Pts',(-2.05079645591606,1.,-0.749287468663053));
#45358=CARTESIAN_POINT('Ctrl Pts',(-2.05713023030263,1.,-0.748091554181101));
#45359=CARTESIAN_POINT('Ctrl Pts',(-2.06220058927162,1.,-0.747103932785504));
#45360=CARTESIAN_POINT('Ctrl Pts',(-2.06600523016401,1.,-0.746345871542695));
#45361=CARTESIAN_POINT('Ctrl Pts',(-2.06854248895575,1.,-0.74583279137781));
#45362=CARTESIAN_POINT('Ctrl Pts',(-2.0698113262342,1.,-0.745574324794401));
#45363=CARTESIAN_POINT('',(-1.60662857109684,0.,-0.693717979106306));
#45364=CARTESIAN_POINT('Origin',(0.,0.,0.));
#45365=CARTESIAN_POINT('',(-1.5055822144029,1.,-0.892032620296855));
#45366=CARTESIAN_POINT('Origin',(0.,1.,0.));
#45367=CARTESIAN_POINT('',(-1.5055822144029,0.,-0.892032620296855));
#45368=CARTESIAN_POINT('Ctrl Pts',(-1.81978687191668,-1.,-1.23627494547115));
#45369=CARTESIAN_POINT('Ctrl Pts',(-1.81978687191668,1.,-1.23627494547115));
#45370=CARTESIAN_POINT('Ctrl Pts',(-1.81925017193666,-1.,-1.23509651170476));
#45371=CARTESIAN_POINT('Ctrl Pts',(-1.81925017193666,1.,-1.23509651170476));
#45372=CARTESIAN_POINT('Ctrl Pts',(-1.81817389921279,-1.,-1.2327422452705));
#45373=CARTESIAN_POINT('Ctrl Pts',(-1.81817389921279,1.,-1.2327422452705));
#45374=CARTESIAN_POINT('Ctrl Pts',(-1.8165508718364,-1.,-1.2292186489137));
#45375=CARTESIAN_POINT('Ctrl Pts',(-1.8165508718364,1.,-1.2292186489137));
#45376=CARTESIAN_POINT('Ctrl Pts',(-1.81436959210434,-1.,-1.2245361330495));
#45377=CARTESIAN_POINT('Ctrl Pts',(-1.81436959210434,1.,-1.2245361330495));
#45378=CARTESIAN_POINT('Ctrl Pts',(-1.81161420806656,-1.,-1.21870906103557));
#45379=CARTESIAN_POINT('Ctrl Pts',(-1.81161420806656,1.,-1.21870906103557));
#45380=CARTESIAN_POINT('Ctrl Pts',(-1.80882996917129,-1.,-1.21290815708314));
#45381=CARTESIAN_POINT('Ctrl Pts',(-1.80882996917129,1.,-1.21290815708314));
#45382=CARTESIAN_POINT('Ctrl Pts',(-1.80601678480707,-1.,-1.20713356605475));
#45383=CARTESIAN_POINT('Ctrl Pts',(-1.80601678480707,1.,-1.20713356605475));
#45384=CARTESIAN_POINT('Ctrl Pts',(-1.80317454838603,-1.,-1.20138548938974));
#45385=CARTESIAN_POINT('Ctrl Pts',(-1.80317454838603,1.,-1.20138548938974));
#45386=CARTESIAN_POINT('Ctrl Pts',(-1.80030314369879,-1.,-1.19566418930242));
#45387=CARTESIAN_POINT('Ctrl Pts',(-1.80030314369879,1.,-1.19566418930242));
#45388=CARTESIAN_POINT('Ctrl Pts',(-1.79740245923478,-1.,-1.18996997934445));
#45389=CARTESIAN_POINT('Ctrl Pts',(-1.79740245923478,1.,-1.18996997934445));
#45390=CARTESIAN_POINT('Ctrl Pts',(-1.79447240321515,-1.,-1.18430321697432));
#45391=CARTESIAN_POINT('Ctrl Pts',(-1.79447240321515,1.,-1.18430321697432));
#45392=CARTESIAN_POINT('Ctrl Pts',(-1.79151291552689,-1.,-1.17866429440809));
#45393=CARTESIAN_POINT('Ctrl Pts',(-1.79151291552689,1.,-1.17866429440809));
#45394=CARTESIAN_POINT('Ctrl Pts',(-1.78852398877616,-1.,-1.17305363177328));
#45395=CARTESIAN_POINT('Ctrl Pts',(-1.78852398877616,1.,-1.17305363177328));
#45396=CARTESIAN_POINT('Ctrl Pts',(-1.78550566040443,-1.,-1.16747166312303));
#45397=CARTESIAN_POINT('Ctrl Pts',(-1.78550566040443,1.,-1.16747166312303));
#45398=CARTESIAN_POINT('Ctrl Pts',(-1.78245795881009,-1.,-1.16191881298499));
#45399=CARTESIAN_POINT('Ctrl Pts',(-1.78245795881009,1.,-1.16191881298499));
#45400=CARTESIAN_POINT('Ctrl Pts',(-1.77938085564275,-1.,-1.15639547194698));
#45401=CARTESIAN_POINT('Ctrl Pts',(-1.77938085564275,1.,-1.15639547194698));
#45402=CARTESIAN_POINT('Ctrl Pts',(-1.7762742255701,-1.,-1.15090197841515));
#45403=CARTESIAN_POINT('Ctrl Pts',(-1.7762742255701,1.,-1.15090197841515));
#45404=CARTESIAN_POINT('Ctrl Pts',(-1.77313777896194,-1.,-1.1454385822692));
#45405=CARTESIAN_POINT('Ctrl Pts',(-1.77313777896194,1.,-1.1454385822692));
#45406=CARTESIAN_POINT('Ctrl Pts',(-1.76997111386769,-1.,-1.14000548336975));
#45407=CARTESIAN_POINT('Ctrl Pts',(-1.76997111386769,1.,-1.14000548336975));
#45408=CARTESIAN_POINT('Ctrl Pts',(-1.76677384551862,-1.,-1.1346029180462));
#45409=CARTESIAN_POINT('Ctrl Pts',(-1.76677384551862,1.,-1.1346029180462));
#45410=CARTESIAN_POINT('Ctrl Pts',(-1.7635457196617,-1.,-1.12923123555075));
#45411=CARTESIAN_POINT('Ctrl Pts',(-1.7635457196617,1.,-1.12923123555075));
#45412=CARTESIAN_POINT('Ctrl Pts',(-1.76028671825096,-1.,-1.12389096855086));
#45413=CARTESIAN_POINT('Ctrl Pts',(-1.76028671825096,1.,-1.12389096855086));
#45414=CARTESIAN_POINT('Ctrl Pts',(-1.75699720772105,-1.,-1.11858293216763));
#45415=CARTESIAN_POINT('Ctrl Pts',(-1.75699720772105,1.,-1.11858293216763));
#45416=CARTESIAN_POINT('Ctrl Pts',(-1.7536777209463,-1.,-1.11330807582551));
#45417=CARTESIAN_POINT('Ctrl Pts',(-1.7536777209463,1.,-1.11330807582551));
#45418=CARTESIAN_POINT('Ctrl Pts',(-1.7503286607592,-1.,-1.10806728183007));
#45419=CARTESIAN_POINT('Ctrl Pts',(-1.7503286607592,1.,-1.10806728183007));
#45420=CARTESIAN_POINT('Ctrl Pts',(-1.74695004214923,-1.,-1.10286118991143));
#45421=CARTESIAN_POINT('Ctrl Pts',(-1.74695004214923,1.,-1.10286118991143));
#45422=CARTESIAN_POINT('Ctrl Pts',(-1.74354119236208,-1.,-1.09768999241225));
#45423=CARTESIAN_POINT('Ctrl Pts',(-1.74354119236208,1.,-1.09768999241225));
#45424=CARTESIAN_POINT('Ctrl Pts',(-1.74010053962247,-1.,-1.09255329056493));
#45425=CARTESIAN_POINT('Ctrl Pts',(-1.74010053962247,1.,-1.09255329056493));
#45426=CARTESIAN_POINT('Ctrl Pts',(-1.73662628326091,-1.,-1.08745056285427));
#45427=CARTESIAN_POINT('Ctrl Pts',(-1.73662628326091,1.,-1.08745056285427));
#45428=CARTESIAN_POINT('Ctrl Pts',(-1.73311705663407,-1.,-1.08238162784749));
#45429=CARTESIAN_POINT('Ctrl Pts',(-1.73311705663407,1.,-1.08238162784749));
#45430=CARTESIAN_POINT('Ctrl Pts',(-1.72957248977424,-1.,-1.0773470373727));
#45431=CARTESIAN_POINT('Ctrl Pts',(-1.72957248977424,1.,-1.0773470373727));
#45432=CARTESIAN_POINT('Ctrl Pts',(-1.72599406198488,-1.,-1.07234866990252));
#45433=CARTESIAN_POINT('Ctrl Pts',(-1.72599406198488,1.,-1.07234866990252));
#45434=CARTESIAN_POINT('Ctrl Pts',(-1.72238500928453,-1.,-1.06738966975462));
#45435=CARTESIAN_POINT('Ctrl Pts',(-1.72238500928453,1.,-1.06738966975462));
#45436=CARTESIAN_POINT('Ctrl Pts',(-1.71874858456904,-1.,-1.06247324680647));
#45437=CARTESIAN_POINT('Ctrl Pts',(-1.71874858456904,1.,-1.06247324680647));
#45438=CARTESIAN_POINT('Ctrl Pts',(-1.7150865442702,-1.,-1.05760163192479));
#45439=CARTESIAN_POINT('Ctrl Pts',(-1.7150865442702,1.,-1.05760163192479));
#45440=CARTESIAN_POINT('Ctrl Pts',(-1.71139783543989,-1.,-1.05277517202855));
#45441=CARTESIAN_POINT('Ctrl Pts',(-1.71139783543989,1.,-1.05277517202855));
#45442=CARTESIAN_POINT('Ctrl Pts',(-1.70767646263649,-1.,-1.04799085404995));
#45443=CARTESIAN_POINT('Ctrl Pts',(-1.70767646263649,1.,-1.04799085404995));
#45444=CARTESIAN_POINT('Ctrl Pts',(-1.70391338707982,-1.,-1.04324363334554));
#45445=CARTESIAN_POINT('Ctrl Pts',(-1.70391338707982,1.,-1.04324363334554));
#45446=CARTESIAN_POINT('Ctrl Pts',(-1.70010052930962,-1.,-1.03852922490789));
#45447=CARTESIAN_POINT('Ctrl Pts',(-1.70010052930962,1.,-1.03852922490789));
#45448=CARTESIAN_POINT('Ctrl Pts',(-1.69623414782771,-1.,-1.03384646003588));
#45449=CARTESIAN_POINT('Ctrl Pts',(-1.69623414782771,1.,-1.03384646003588));
#45450=CARTESIAN_POINT('Ctrl Pts',(-1.69231840863458,-1.,-1.02919977579147));
#45451=CARTESIAN_POINT('Ctrl Pts',(-1.69231840863458,1.,-1.02919977579147));
#45452=CARTESIAN_POINT('Ctrl Pts',(-1.68836910178447,-1.,-1.02460180535255));
#45453=CARTESIAN_POINT('Ctrl Pts',(-1.68836910178447,1.,-1.02460180535255));
#45454=CARTESIAN_POINT('Ctrl Pts',(-1.68440578021706,-1.,-1.02006795074201));
#45455=CARTESIAN_POINT('Ctrl Pts',(-1.68440578021706,1.,-1.02006795074201));
#45456=CARTESIAN_POINT('Ctrl Pts',(-1.68044289894798,-1.,-1.01561026162773));
#45457=CARTESIAN_POINT('Ctrl Pts',(-1.68044289894798,1.,-1.01561026162773));
#45458=CARTESIAN_POINT('Ctrl Pts',(-1.67648246776464,-1.,-1.01123236493511));
#45459=CARTESIAN_POINT('Ctrl Pts',(-1.67648246776464,1.,-1.01123236493511));
#45460=CARTESIAN_POINT('Ctrl Pts',(-1.67250335383293,-1.,-1.00692206696414));
#45461=CARTESIAN_POINT('Ctrl Pts',(-1.67250335383293,1.,-1.00692206696414));
#45462=CARTESIAN_POINT('Ctrl Pts',(-1.66846059277303,-1.,-1.00265091003727));
#45463=CARTESIAN_POINT('Ctrl Pts',(-1.66846059277303,1.,-1.00265091003727));
#45464=CARTESIAN_POINT('Ctrl Pts',(-1.66430758030376,-1.,-0.998389654952758));
#45465=CARTESIAN_POINT('Ctrl Pts',(-1.66430758030376,1.,-0.998389654952758));
#45466=CARTESIAN_POINT('Ctrl Pts',(-1.66001553809947,-1.,-0.994121836661306));
#45467=CARTESIAN_POINT('Ctrl Pts',(-1.66001553809947,1.,-0.994121836661306));
#45468=CARTESIAN_POINT('Ctrl Pts',(-1.65559044289699,-1.,-0.989855627854165));
#45469=CARTESIAN_POINT('Ctrl Pts',(-1.65559044289699,1.,-0.989855627854165));
#45470=CARTESIAN_POINT('Ctrl Pts',(-1.65110016612638,-1.,-0.985642622920821));
#45471=CARTESIAN_POINT('Ctrl Pts',(-1.65110016612638,1.,-0.985642622920821));
#45472=CARTESIAN_POINT('Ctrl Pts',(-1.64665139190656,-1.,-0.981562530939489));
#45473=CARTESIAN_POINT('Ctrl Pts',(-1.64665139190656,1.,-0.981562530939489));
#45474=CARTESIAN_POINT('Ctrl Pts',(-1.64233990826687,-1.,-0.977689794119416));
#45475=CARTESIAN_POINT('Ctrl Pts',(-1.64233990826687,1.,-0.977689794119416));
#45476=CARTESIAN_POINT('Ctrl Pts',(-1.63820952658144,-1.,-0.974066058287418));
#45477=CARTESIAN_POINT('Ctrl Pts',(-1.63820952658144,1.,-0.974066058287418));
#45478=CARTESIAN_POINT('Ctrl Pts',(-1.63420665729798,-1.,-0.970669715997509));
#45479=CARTESIAN_POINT('Ctrl Pts',(-1.63420665729798,1.,-0.970669715997509));
#45480=CARTESIAN_POINT('Ctrl Pts',(-1.63013849959461,-1.,-0.967387853230345));
#45481=CARTESIAN_POINT('Ctrl Pts',(-1.63013849959461,1.,-0.967387853230345));
#45482=CARTESIAN_POINT('Ctrl Pts',(-1.62571930670187,-1.,-0.964046107040536));
#45483=CARTESIAN_POINT('Ctrl Pts',(-1.62571930670187,1.,-0.964046107040536));
#45484=CARTESIAN_POINT('Ctrl Pts',(-1.62061638140221,-1.,-0.960438326101729));
#45485=CARTESIAN_POINT('Ctrl Pts',(-1.62061638140221,1.,-0.960438326101729));
#45486=CARTESIAN_POINT('Ctrl Pts',(-1.61449324337085,-1.,-0.956354422920671));
#45487=CARTESIAN_POINT('Ctrl Pts',(-1.61449324337085,1.,-0.956354422920671));
#45488=CARTESIAN_POINT('Ctrl Pts',(-1.60706069896936,-1.,-0.951613284356035));
#45489=CARTESIAN_POINT('Ctrl Pts',(-1.60706069896936,1.,-0.951613284356035));
#45490=CARTESIAN_POINT('Ctrl Pts',(-1.59810042043673,-1.,-0.946078063315257));
#45491=CARTESIAN_POINT('Ctrl Pts',(-1.59810042043673,1.,-0.946078063315257));
#45492=CARTESIAN_POINT('Ctrl Pts',(-1.58744937487176,-1.,-0.939646377893399));
#45493=CARTESIAN_POINT('Ctrl Pts',(-1.58744937487176,1.,-0.939646377893399));
#45494=CARTESIAN_POINT('Ctrl Pts',(-1.57499388382243,-1.,-0.932246680108685));
#45495=CARTESIAN_POINT('Ctrl Pts',(-1.57499388382243,1.,-0.932246680108685));
#45496=CARTESIAN_POINT('Ctrl Pts',(-1.56065988578893,-1.,-0.923832188944341));
#45497=CARTESIAN_POINT('Ctrl Pts',(-1.56065988578893,1.,-0.923832188944341));
#45498=CARTESIAN_POINT('Ctrl Pts',(-1.54440491149498,-1.,-0.914375919026456));
#45499=CARTESIAN_POINT('Ctrl Pts',(-1.54440491149498,1.,-0.914375919026456));
#45500=CARTESIAN_POINT('Ctrl Pts',(-1.52984849887993,-1.,-0.905967409625651));
#45501=CARTESIAN_POINT('Ctrl Pts',(-1.52984849887993,1.,-0.905967409625651));
#45502=CARTESIAN_POINT('Ctrl Pts',(-1.51805569590094,-1.,-0.899185047483511));
#45503=CARTESIAN_POINT('Ctrl Pts',(-1.51805569590094,1.,-0.899185047483511));
#45504=CARTESIAN_POINT('Ctrl Pts',(-1.50980486806688,-1.,-0.894452006964543));
#45505=CARTESIAN_POINT('Ctrl Pts',(-1.50980486806688,1.,-0.894452006964543));
#45506=CARTESIAN_POINT('Ctrl Pts',(-1.5055822144029,-1.,-0.892032620296855));
#45507=CARTESIAN_POINT('Ctrl Pts',(-1.5055822144029,1.,-0.892032620296855));
#45508=CARTESIAN_POINT('',(-1.81978687191668,1.,-1.23627494547115));
#45509=CARTESIAN_POINT('Ctrl Pts',(-1.81978687191668,1.,-1.23627494547115));
#45510=CARTESIAN_POINT('Ctrl Pts',(-1.81925017193666,1.,-1.23509651170476));
#45511=CARTESIAN_POINT('Ctrl Pts',(-1.81817389921279,1.,-1.2327422452705));
#45512=CARTESIAN_POINT('Ctrl Pts',(-1.8165508718364,1.,-1.2292186489137));
#45513=CARTESIAN_POINT('Ctrl Pts',(-1.81436959210434,1.,-1.2245361330495));
#45514=CARTESIAN_POINT('Ctrl Pts',(-1.81161420806656,1.,-1.21870906103557));
#45515=CARTESIAN_POINT('Ctrl Pts',(-1.80882996917129,1.,-1.21290815708314));
#45516=CARTESIAN_POINT('Ctrl Pts',(-1.80601678480707,1.,-1.20713356605475));
#45517=CARTESIAN_POINT('Ctrl Pts',(-1.80317454838603,1.,-1.20138548938974));
#45518=CARTESIAN_POINT('Ctrl Pts',(-1.80030314369879,1.,-1.19566418930242));
#45519=CARTESIAN_POINT('Ctrl Pts',(-1.79740245923478,1.,-1.18996997934445));
#45520=CARTESIAN_POINT('Ctrl Pts',(-1.79447240321515,1.,-1.18430321697432));
#45521=CARTESIAN_POINT('Ctrl Pts',(-1.79151291552689,1.,-1.17866429440809));
#45522=CARTESIAN_POINT('Ctrl Pts',(-1.78852398877616,1.,-1.17305363177328));
#45523=CARTESIAN_POINT('Ctrl Pts',(-1.78550566040443,1.,-1.16747166312303));
#45524=CARTESIAN_POINT('Ctrl Pts',(-1.78245795881009,1.,-1.16191881298499));
#45525=CARTESIAN_POINT('Ctrl Pts',(-1.77938085564275,1.,-1.15639547194698));
#45526=CARTESIAN_POINT('Ctrl Pts',(-1.7762742255701,1.,-1.15090197841515));
#45527=CARTESIAN_POINT('Ctrl Pts',(-1.77313777896194,1.,-1.1454385822692));
#45528=CARTESIAN_POINT('Ctrl Pts',(-1.76997111386769,1.,-1.14000548336975));
#45529=CARTESIAN_POINT('Ctrl Pts',(-1.76677384551862,1.,-1.1346029180462));
#45530=CARTESIAN_POINT('Ctrl Pts',(-1.7635457196617,1.,-1.12923123555075));
#45531=CARTESIAN_POINT('Ctrl Pts',(-1.76028671825096,1.,-1.12389096855086));
#45532=CARTESIAN_POINT('Ctrl Pts',(-1.75699720772105,1.,-1.11858293216763));
#45533=CARTESIAN_POINT('Ctrl Pts',(-1.7536777209463,1.,-1.11330807582551));
#45534=CARTESIAN_POINT('Ctrl Pts',(-1.7503286607592,1.,-1.10806728183007));
#45535=CARTESIAN_POINT('Ctrl Pts',(-1.74695004214923,1.,-1.10286118991143));
#45536=CARTESIAN_POINT('Ctrl Pts',(-1.74354119236208,1.,-1.09768999241225));
#45537=CARTESIAN_POINT('Ctrl Pts',(-1.74010053962247,1.,-1.09255329056493));
#45538=CARTESIAN_POINT('Ctrl Pts',(-1.73662628326091,1.,-1.08745056285427));
#45539=CARTESIAN_POINT('Ctrl Pts',(-1.73311705663407,1.,-1.08238162784749));
#45540=CARTESIAN_POINT('Ctrl Pts',(-1.72957248977424,1.,-1.0773470373727));
#45541=CARTESIAN_POINT('Ctrl Pts',(-1.72599406198488,1.,-1.07234866990252));
#45542=CARTESIAN_POINT('Ctrl Pts',(-1.72238500928453,1.,-1.06738966975462));
#45543=CARTESIAN_POINT('Ctrl Pts',(-1.71874858456904,1.,-1.06247324680647));
#45544=CARTESIAN_POINT('Ctrl Pts',(-1.7150865442702,1.,-1.05760163192479));
#45545=CARTESIAN_POINT('Ctrl Pts',(-1.71139783543989,1.,-1.05277517202855));
#45546=CARTESIAN_POINT('Ctrl Pts',(-1.70767646263649,1.,-1.04799085404995));
#45547=CARTESIAN_POINT('Ctrl Pts',(-1.70391338707982,1.,-1.04324363334554));
#45548=CARTESIAN_POINT('Ctrl Pts',(-1.70010052930962,1.,-1.03852922490789));
#45549=CARTESIAN_POINT('Ctrl Pts',(-1.69623414782771,1.,-1.03384646003588));
#45550=CARTESIAN_POINT('Ctrl Pts',(-1.69231840863458,1.,-1.02919977579147));
#45551=CARTESIAN_POINT('Ctrl Pts',(-1.68836910178447,1.,-1.02460180535255));
#45552=CARTESIAN_POINT('Ctrl Pts',(-1.68440578021706,1.,-1.02006795074201));
#45553=CARTESIAN_POINT('Ctrl Pts',(-1.68044289894798,1.,-1.01561026162773));
#45554=CARTESIAN_POINT('Ctrl Pts',(-1.67648246776464,1.,-1.01123236493511));
#45555=CARTESIAN_POINT('Ctrl Pts',(-1.67250335383293,1.,-1.00692206696414));
#45556=CARTESIAN_POINT('Ctrl Pts',(-1.66846059277303,1.,-1.00265091003727));
#45557=CARTESIAN_POINT('Ctrl Pts',(-1.66430758030376,1.,-0.998389654952758));
#45558=CARTESIAN_POINT('Ctrl Pts',(-1.66001553809947,1.,-0.994121836661306));
#45559=CARTESIAN_POINT('Ctrl Pts',(-1.65559044289699,1.,-0.989855627854165));
#45560=CARTESIAN_POINT('Ctrl Pts',(-1.65110016612638,1.,-0.985642622920821));
#45561=CARTESIAN_POINT('Ctrl Pts',(-1.64665139190656,1.,-0.981562530939489));
#45562=CARTESIAN_POINT('Ctrl Pts',(-1.64233990826687,1.,-0.977689794119416));
#45563=CARTESIAN_POINT('Ctrl Pts',(-1.63820952658144,1.,-0.974066058287418));
#45564=CARTESIAN_POINT('Ctrl Pts',(-1.63420665729798,1.,-0.970669715997509));
#45565=CARTESIAN_POINT('Ctrl Pts',(-1.63013849959461,1.,-0.967387853230345));
#45566=CARTESIAN_POINT('Ctrl Pts',(-1.62571930670187,1.,-0.964046107040536));
#45567=CARTESIAN_POINT('Ctrl Pts',(-1.62061638140221,1.,-0.960438326101729));
#45568=CARTESIAN_POINT('Ctrl Pts',(-1.61449324337085,1.,-0.956354422920671));
#45569=CARTESIAN_POINT('Ctrl Pts',(-1.60706069896936,1.,-0.951613284356035));
#45570=CARTESIAN_POINT('Ctrl Pts',(-1.59810042043673,1.,-0.946078063315257));
#45571=CARTESIAN_POINT('Ctrl Pts',(-1.58744937487176,1.,-0.939646377893399));
#45572=CARTESIAN_POINT('Ctrl Pts',(-1.57499388382243,1.,-0.932246680108685));
#45573=CARTESIAN_POINT('Ctrl Pts',(-1.56065988578893,1.,-0.923832188944341));
#45574=CARTESIAN_POINT('Ctrl Pts',(-1.54440491149498,1.,-0.914375919026456));
#45575=CARTESIAN_POINT('Ctrl Pts',(-1.52984849887993,1.,-0.905967409625651));
#45576=CARTESIAN_POINT('Ctrl Pts',(-1.51805569590094,1.,-0.899185047483511));
#45577=CARTESIAN_POINT('Ctrl Pts',(-1.50980486806688,1.,-0.894452006964543));
#45578=CARTESIAN_POINT('Ctrl Pts',(-1.5055822144029,1.,-0.892032620296855));
#45579=CARTESIAN_POINT('',(-1.81978687191668,0.,-1.23627494547115));
#45580=CARTESIAN_POINT('Origin',(-1.73811241238545,0.,-1.34869019493419));
#45581=CARTESIAN_POINT('',(-1.73811241238545,1.,-1.34869019493419));
#45582=CARTESIAN_POINT('',(-1.81978687191668,1.,-1.23627494547115));
#45583=CARTESIAN_POINT('',(-1.73811241238545,0.,-1.34869019493419));
#45584=CARTESIAN_POINT('Ctrl Pts',(-1.31362392696032,-1.,-1.15624053661742));
#45585=CARTESIAN_POINT('Ctrl Pts',(-1.31362392696032,1.,-1.15624053661742));
#45586=CARTESIAN_POINT('Ctrl Pts',(-1.31722977216397,-1.,-1.15950888730809));
#45587=CARTESIAN_POINT('Ctrl Pts',(-1.31722977216397,1.,-1.15950888730809));
#45588=CARTESIAN_POINT('Ctrl Pts',(-1.32428080721772,-1.,-1.16589330093588));
#45589=CARTESIAN_POINT('Ctrl Pts',(-1.32428080721772,1.,-1.16589330093588));
#45590=CARTESIAN_POINT('Ctrl Pts',(-1.33437539347008,-1.,-1.17501305789857));
#45591=CARTESIAN_POINT('Ctrl Pts',(-1.33437539347008,1.,-1.17501305789857));
#45592=CARTESIAN_POINT('Ctrl Pts',(-1.34687054001093,-1.,-1.18625865667441));
#45593=CARTESIAN_POINT('Ctrl Pts',(-1.34687054001093,1.,-1.18625865667441));
#45594=CARTESIAN_POINT('Ctrl Pts',(-1.36088705043885,-1.,-1.1987959077932));
#45595=CARTESIAN_POINT('Ctrl Pts',(-1.36088705043885,1.,-1.1987959077932));
#45596=CARTESIAN_POINT('Ctrl Pts',(-1.37331915607905,-1.,-1.20982812925645));
#45597=CARTESIAN_POINT('Ctrl Pts',(-1.37331915607905,1.,-1.20982812925645));
#45598=CARTESIAN_POINT('Ctrl Pts',(-1.38420564527715,-1.,-1.21938737280852));
#45599=CARTESIAN_POINT('Ctrl Pts',(-1.38420564527715,1.,-1.21938737280852));
#45600=CARTESIAN_POINT('Ctrl Pts',(-1.39361389568796,-1.,-1.22752961899387));
#45601=CARTESIAN_POINT('Ctrl Pts',(-1.39361389568796,1.,-1.22752961899387));
#45602=CARTESIAN_POINT('Ctrl Pts',(-1.40164708206106,-1.,-1.23434087290423));
#45603=CARTESIAN_POINT('Ctrl Pts',(-1.40164708206106,1.,-1.23434087290423));
#45604=CARTESIAN_POINT('Ctrl Pts',(-1.40845295531283,-1.,-1.23994455029534));
#45605=CARTESIAN_POINT('Ctrl Pts',(-1.40845295531283,1.,-1.23994455029534));
#45606=CARTESIAN_POINT('Ctrl Pts',(-1.41422913175179,-1.,-1.24450600513056));
#45607=CARTESIAN_POINT('Ctrl Pts',(-1.41422913175179,1.,-1.24450600513056));
#45608=CARTESIAN_POINT('Ctrl Pts',(-1.41923722596025,-1.,-1.24824430986571));
#45609=CARTESIAN_POINT('Ctrl Pts',(-1.41923722596025,1.,-1.24824430986571));
#45610=CARTESIAN_POINT('Ctrl Pts',(-1.42378102115575,-1.,-1.2514145557001));
#45611=CARTESIAN_POINT('Ctrl Pts',(-1.42378102115575,1.,-1.2514145557001));
#45612=CARTESIAN_POINT('Ctrl Pts',(-1.42815938799387,-1.,-1.25426945222639));
#45613=CARTESIAN_POINT('Ctrl Pts',(-1.42815938799387,1.,-1.25426945222639));
#45614=CARTESIAN_POINT('Ctrl Pts',(-1.43262645609691,-1.,-1.25702687965755));
#45615=CARTESIAN_POINT('Ctrl Pts',(-1.43262645609691,1.,-1.25702687965755));
#45616=CARTESIAN_POINT('Ctrl Pts',(-1.43734919180848,-1.,-1.25983531012005));
#45617=CARTESIAN_POINT('Ctrl Pts',(-1.43734919180848,1.,-1.25983531012005));
#45618=CARTESIAN_POINT('Ctrl Pts',(-1.44236470511303,-1.,-1.26273903323859));
#45619=CARTESIAN_POINT('Ctrl Pts',(-1.44236470511303,1.,-1.26273903323859));
#45620=CARTESIAN_POINT('Ctrl Pts',(-1.44761985001662,-1.,-1.26570925118868));
#45621=CARTESIAN_POINT('Ctrl Pts',(-1.44761985001662,1.,-1.26570925118868));
#45622=CARTESIAN_POINT('Ctrl Pts',(-1.45301422764247,-1.,-1.2686778680489));
#45623=CARTESIAN_POINT('Ctrl Pts',(-1.45301422764247,1.,-1.2686778680489));
#45624=CARTESIAN_POINT('Ctrl Pts',(-1.45843906294697,-1.,-1.27156805265289));
#45625=CARTESIAN_POINT('Ctrl Pts',(-1.45843906294697,1.,-1.27156805265289));
#45626=CARTESIAN_POINT('Ctrl Pts',(-1.46382431332476,-1.,-1.27433119897822));
#45627=CARTESIAN_POINT('Ctrl Pts',(-1.46382431332476,1.,-1.27433119897822));
#45628=CARTESIAN_POINT('Ctrl Pts',(-1.46916035917133,-1.,-1.27696414831089));
#45629=CARTESIAN_POINT('Ctrl Pts',(-1.46916035917133,1.,-1.27696414831089));
#45630=CARTESIAN_POINT('Ctrl Pts',(-1.4744717526707,-1.,-1.2794891824849));
#45631=CARTESIAN_POINT('Ctrl Pts',(-1.4744717526707,1.,-1.2794891824849));
#45632=CARTESIAN_POINT('Ctrl Pts',(-1.47980070347095,-1.,-1.28194158939517));
#45633=CARTESIAN_POINT('Ctrl Pts',(-1.47980070347095,1.,-1.28194158939517));
#45634=CARTESIAN_POINT('Ctrl Pts',(-1.4851881711891,-1.,-1.28435533880201));
#45635=CARTESIAN_POINT('Ctrl Pts',(-1.4851881711891,1.,-1.28435533880201));
#45636=CARTESIAN_POINT('Ctrl Pts',(-1.4906522831278,-1.,-1.2867467611644));
#45637=CARTESIAN_POINT('Ctrl Pts',(-1.4906522831278,1.,-1.2867467611644));
#45638=CARTESIAN_POINT('Ctrl Pts',(-1.49618896881754,-1.,-1.28911506584254));
#45639=CARTESIAN_POINT('Ctrl Pts',(-1.49618896881754,1.,-1.28911506584254));
#45640=CARTESIAN_POINT('Ctrl Pts',(-1.50178230149776,-1.,-1.29145022885181));
#45641=CARTESIAN_POINT('Ctrl Pts',(-1.50178230149776,1.,-1.29145022885181));
#45642=CARTESIAN_POINT('Ctrl Pts',(-1.50741159078365,-1.,-1.29373841372842));
#45643=CARTESIAN_POINT('Ctrl Pts',(-1.50741159078365,1.,-1.29373841372842));
#45644=CARTESIAN_POINT('Ctrl Pts',(-1.51305994241402,-1.,-1.29596850710509));
#45645=CARTESIAN_POINT('Ctrl Pts',(-1.51305994241402,1.,-1.29596850710509));
#45646=CARTESIAN_POINT('Ctrl Pts',(-1.51872184912724,-1.,-1.29813791800747));
#45647=CARTESIAN_POINT('Ctrl Pts',(-1.51872184912724,1.,-1.29813791800747));
#45648=CARTESIAN_POINT('Ctrl Pts',(-1.52439957861062,-1.,-1.30024984366328));
#45649=CARTESIAN_POINT('Ctrl Pts',(-1.52439957861062,1.,-1.30024984366328));
#45650=CARTESIAN_POINT('Ctrl Pts',(-1.53009970283891,-1.,-1.30231064395568));
#45651=CARTESIAN_POINT('Ctrl Pts',(-1.53009970283891,1.,-1.30231064395568));
#45652=CARTESIAN_POINT('Ctrl Pts',(-1.53582981268977,-1.,-1.30432735639489));
#45653=CARTESIAN_POINT('Ctrl Pts',(-1.53582981268977,1.,-1.30432735639489));
#45654=CARTESIAN_POINT('Ctrl Pts',(-1.54159462645432,-1.,-1.30630475189556));
#45655=CARTESIAN_POINT('Ctrl Pts',(-1.54159462645432,1.,-1.30630475189556));
#45656=CARTESIAN_POINT('Ctrl Pts',(-1.54739413957185,-1.,-1.30824393907473));
#45657=CARTESIAN_POINT('Ctrl Pts',(-1.54739413957185,1.,-1.30824393907473));
#45658=CARTESIAN_POINT('Ctrl Pts',(-1.55322568759481,-1.,-1.31014393684222));
#45659=CARTESIAN_POINT('Ctrl Pts',(-1.55322568759481,1.,-1.31014393684222));
#45660=CARTESIAN_POINT('Ctrl Pts',(-1.55908521254821,-1.,-1.31200264341696));
#45661=CARTESIAN_POINT('Ctrl Pts',(-1.55908521254821,1.,-1.31200264341696));
#45662=CARTESIAN_POINT('Ctrl Pts',(-1.56496872402353,-1.,-1.31381795281002));
#45663=CARTESIAN_POINT('Ctrl Pts',(-1.56496872402353,1.,-1.31381795281002));
#45664=CARTESIAN_POINT('Ctrl Pts',(-1.57087397835723,-1.,-1.31558903860016));
#45665=CARTESIAN_POINT('Ctrl Pts',(-1.57087397835723,1.,-1.31558903860016));
#45666=CARTESIAN_POINT('Ctrl Pts',(-1.5768005650559,-1.,-1.31731642317187));
#45667=CARTESIAN_POINT('Ctrl Pts',(-1.5768005650559,1.,-1.31731642317187));
#45668=CARTESIAN_POINT('Ctrl Pts',(-1.58274907898834,-1.,-1.31900135021432));
#45669=CARTESIAN_POINT('Ctrl Pts',(-1.58274907898834,1.,-1.31900135021432));
#45670=CARTESIAN_POINT('Ctrl Pts',(-1.58872057258245,-1.,-1.32064537110892));
#45671=CARTESIAN_POINT('Ctrl Pts',(-1.58872057258245,1.,-1.32064537110892));
#45672=CARTESIAN_POINT('Ctrl Pts',(-1.59471591079403,-1.,-1.32224985747682));
#45673=CARTESIAN_POINT('Ctrl Pts',(-1.59471591079403,1.,-1.32224985747682));
#45674=CARTESIAN_POINT('Ctrl Pts',(-1.60073511858687,-1.,-1.32381550858256));
#45675=CARTESIAN_POINT('Ctrl Pts',(-1.60073511858687,1.,-1.32381550858256));
#45676=CARTESIAN_POINT('Ctrl Pts',(-1.60677758290954,-1.,-1.32534250785782));
#45677=CARTESIAN_POINT('Ctrl Pts',(-1.60677758290954,1.,-1.32534250785782));
#45678=CARTESIAN_POINT('Ctrl Pts',(-1.6128423401575,-1.,-1.32683074483356));
#45679=CARTESIAN_POINT('Ctrl Pts',(-1.6128423401575,1.,-1.32683074483356));
#45680=CARTESIAN_POINT('Ctrl Pts',(-1.61892832270724,-1.,-1.32828000610449));
#45681=CARTESIAN_POINT('Ctrl Pts',(-1.61892832270724,1.,-1.32828000610449));
#45682=CARTESIAN_POINT('Ctrl Pts',(-1.62503464209797,-1.,-1.3296901950568));
#45683=CARTESIAN_POINT('Ctrl Pts',(-1.62503464209797,1.,-1.3296901950568));
#45684=CARTESIAN_POINT('Ctrl Pts',(-1.63116079730923,-1.,-1.33106149345645));
#45685=CARTESIAN_POINT('Ctrl Pts',(-1.63116079730923,1.,-1.33106149345645));
#45686=CARTESIAN_POINT('Ctrl Pts',(-1.63730653475089,-1.,-1.33239425103724));
#45687=CARTESIAN_POINT('Ctrl Pts',(-1.63730653475089,1.,-1.33239425103724));
#45688=CARTESIAN_POINT('Ctrl Pts',(-1.6434717485603,-1.,-1.33368890676572));
#45689=CARTESIAN_POINT('Ctrl Pts',(-1.6434717485603,1.,-1.33368890676572));
#45690=CARTESIAN_POINT('Ctrl Pts',(-1.6496563728683,-1.,-1.33494590467993));
#45691=CARTESIAN_POINT('Ctrl Pts',(-1.6496563728683,1.,-1.33494590467993));
#45692=CARTESIAN_POINT('Ctrl Pts',(-1.65586025952593,-1.,-1.33616559745172));
#45693=CARTESIAN_POINT('Ctrl Pts',(-1.65586025952593,1.,-1.33616559745172));
#45694=CARTESIAN_POINT('Ctrl Pts',(-1.66208312541983,-1.,-1.33734820885262));
#45695=CARTESIAN_POINT('Ctrl Pts',(-1.66208312541983,1.,-1.33734820885262));
#45696=CARTESIAN_POINT('Ctrl Pts',(-1.66832460783989,-1.,-1.33849388654388));
#45697=CARTESIAN_POINT('Ctrl Pts',(-1.66832460783989,1.,-1.33849388654388));
#45698=CARTESIAN_POINT('Ctrl Pts',(-1.67458429426086,-1.,-1.3396027347034));
#45699=CARTESIAN_POINT('Ctrl Pts',(-1.67458429426086,1.,-1.3396027347034));
#45700=CARTESIAN_POINT('Ctrl Pts',(-1.68086176030362,-1.,-1.34067485185203));
#45701=CARTESIAN_POINT('Ctrl Pts',(-1.68086176030362,1.,-1.34067485185203));
#45702=CARTESIAN_POINT('Ctrl Pts',(-1.68715660868764,-1.,-1.341710374848));
#45703=CARTESIAN_POINT('Ctrl Pts',(-1.68715660868764,1.,-1.341710374848));
#45704=CARTESIAN_POINT('Ctrl Pts',(-1.6934684849687,-1.,-1.34270948206319));
#45705=CARTESIAN_POINT('Ctrl Pts',(-1.6934684849687,1.,-1.34270948206319));
#45706=CARTESIAN_POINT('Ctrl Pts',(-1.69979707754427,-1.,-1.34367237124483));
#45707=CARTESIAN_POINT('Ctrl Pts',(-1.69979707754427,1.,-1.34367237124483));
#45708=CARTESIAN_POINT('Ctrl Pts',(-1.70614212266738,-1.,-1.34459924533831));
#45709=CARTESIAN_POINT('Ctrl Pts',(-1.70614212266738,1.,-1.34459924533831));
#45710=CARTESIAN_POINT('Ctrl Pts',(-1.71250340686822,-1.,-1.34549029589416));
#45711=CARTESIAN_POINT('Ctrl Pts',(-1.71250340686822,1.,-1.34549029589416));
#45712=CARTESIAN_POINT('Ctrl Pts',(-1.7188807715049,-1.,-1.34634568653227));
#45713=CARTESIAN_POINT('Ctrl Pts',(-1.7188807715049,1.,-1.34634568653227));
#45714=CARTESIAN_POINT('Ctrl Pts',(-1.72527410680674,-1.,-1.34716554819527));
#45715=CARTESIAN_POINT('Ctrl Pts',(-1.72527410680674,1.,-1.34716554819527));
#45716=CARTESIAN_POINT('Ctrl Pts',(-1.7304014965394,-1.,-1.34779309152035));
#45717=CARTESIAN_POINT('Ctrl Pts',(-1.7304014965394,1.,-1.34779309152035));
#45718=CARTESIAN_POINT('Ctrl Pts',(-1.73425417885907,-1.,-1.34824783112887));
#45719=CARTESIAN_POINT('Ctrl Pts',(-1.73425417885907,1.,-1.34824783112887));
#45720=CARTESIAN_POINT('Ctrl Pts',(-1.73682580585691,-1.,-1.34854391898045));
#45721=CARTESIAN_POINT('Ctrl Pts',(-1.73682580585691,1.,-1.34854391898045));
#45722=CARTESIAN_POINT('Ctrl Pts',(-1.73811241238545,-1.,-1.34869019493419));
#45723=CARTESIAN_POINT('Ctrl Pts',(-1.73811241238545,1.,-1.34869019493419));
#45724=CARTESIAN_POINT('',(-1.31362392696032,1.,-1.15624053661742));
#45725=CARTESIAN_POINT('Ctrl Pts',(-1.31362392696032,1.,-1.15624053661742));
#45726=CARTESIAN_POINT('Ctrl Pts',(-1.31722977216397,1.,-1.15950888730809));
#45727=CARTESIAN_POINT('Ctrl Pts',(-1.32428080721772,1.,-1.16589330093588));
#45728=CARTESIAN_POINT('Ctrl Pts',(-1.33437539347008,1.,-1.17501305789857));
#45729=CARTESIAN_POINT('Ctrl Pts',(-1.34687054001093,1.,-1.18625865667441));
#45730=CARTESIAN_POINT('Ctrl Pts',(-1.36088705043885,1.,-1.1987959077932));
#45731=CARTESIAN_POINT('Ctrl Pts',(-1.37331915607905,1.,-1.20982812925645));
#45732=CARTESIAN_POINT('Ctrl Pts',(-1.38420564527715,1.,-1.21938737280852));
#45733=CARTESIAN_POINT('Ctrl Pts',(-1.39361389568796,1.,-1.22752961899387));
#45734=CARTESIAN_POINT('Ctrl Pts',(-1.40164708206106,1.,-1.23434087290423));
#45735=CARTESIAN_POINT('Ctrl Pts',(-1.40845295531283,1.,-1.23994455029534));
#45736=CARTESIAN_POINT('Ctrl Pts',(-1.41422913175179,1.,-1.24450600513056));
#45737=CARTESIAN_POINT('Ctrl Pts',(-1.41923722596025,1.,-1.24824430986571));
#45738=CARTESIAN_POINT('Ctrl Pts',(-1.42378102115575,1.,-1.2514145557001));
#45739=CARTESIAN_POINT('Ctrl Pts',(-1.42815938799387,1.,-1.25426945222639));
#45740=CARTESIAN_POINT('Ctrl Pts',(-1.43262645609691,1.,-1.25702687965755));
#45741=CARTESIAN_POINT('Ctrl Pts',(-1.43734919180848,1.,-1.25983531012005));
#45742=CARTESIAN_POINT('Ctrl Pts',(-1.44236470511303,1.,-1.26273903323859));
#45743=CARTESIAN_POINT('Ctrl Pts',(-1.44761985001662,1.,-1.26570925118868));
#45744=CARTESIAN_POINT('Ctrl Pts',(-1.45301422764247,1.,-1.2686778680489));
#45745=CARTESIAN_POINT('Ctrl Pts',(-1.45843906294697,1.,-1.27156805265289));
#45746=CARTESIAN_POINT('Ctrl Pts',(-1.46382431332476,1.,-1.27433119897822));
#45747=CARTESIAN_POINT('Ctrl Pts',(-1.46916035917133,1.,-1.27696414831089));
#45748=CARTESIAN_POINT('Ctrl Pts',(-1.4744717526707,1.,-1.2794891824849));
#45749=CARTESIAN_POINT('Ctrl Pts',(-1.47980070347095,1.,-1.28194158939517));
#45750=CARTESIAN_POINT('Ctrl Pts',(-1.4851881711891,1.,-1.28435533880201));
#45751=CARTESIAN_POINT('Ctrl Pts',(-1.4906522831278,1.,-1.2867467611644));
#45752=CARTESIAN_POINT('Ctrl Pts',(-1.49618896881754,1.,-1.28911506584254));
#45753=CARTESIAN_POINT('Ctrl Pts',(-1.50178230149776,1.,-1.29145022885181));
#45754=CARTESIAN_POINT('Ctrl Pts',(-1.50741159078365,1.,-1.29373841372842));
#45755=CARTESIAN_POINT('Ctrl Pts',(-1.51305994241402,1.,-1.29596850710509));
#45756=CARTESIAN_POINT('Ctrl Pts',(-1.51872184912724,1.,-1.29813791800747));
#45757=CARTESIAN_POINT('Ctrl Pts',(-1.52439957861062,1.,-1.30024984366328));
#45758=CARTESIAN_POINT('Ctrl Pts',(-1.53009970283891,1.,-1.30231064395568));
#45759=CARTESIAN_POINT('Ctrl Pts',(-1.53582981268977,1.,-1.30432735639489));
#45760=CARTESIAN_POINT('Ctrl Pts',(-1.54159462645432,1.,-1.30630475189556));
#45761=CARTESIAN_POINT('Ctrl Pts',(-1.54739413957185,1.,-1.30824393907473));
#45762=CARTESIAN_POINT('Ctrl Pts',(-1.55322568759481,1.,-1.31014393684222));
#45763=CARTESIAN_POINT('Ctrl Pts',(-1.55908521254821,1.,-1.31200264341696));
#45764=CARTESIAN_POINT('Ctrl Pts',(-1.56496872402353,1.,-1.31381795281002));
#45765=CARTESIAN_POINT('Ctrl Pts',(-1.57087397835723,1.,-1.31558903860016));
#45766=CARTESIAN_POINT('Ctrl Pts',(-1.5768005650559,1.,-1.31731642317187));
#45767=CARTESIAN_POINT('Ctrl Pts',(-1.58274907898834,1.,-1.31900135021432));
#45768=CARTESIAN_POINT('Ctrl Pts',(-1.58872057258245,1.,-1.32064537110892));
#45769=CARTESIAN_POINT('Ctrl Pts',(-1.59471591079403,1.,-1.32224985747682));
#45770=CARTESIAN_POINT('Ctrl Pts',(-1.60073511858687,1.,-1.32381550858256));
#45771=CARTESIAN_POINT('Ctrl Pts',(-1.60677758290954,1.,-1.32534250785782));
#45772=CARTESIAN_POINT('Ctrl Pts',(-1.6128423401575,1.,-1.32683074483356));
#45773=CARTESIAN_POINT('Ctrl Pts',(-1.61892832270724,1.,-1.32828000610449));
#45774=CARTESIAN_POINT('Ctrl Pts',(-1.62503464209797,1.,-1.3296901950568));
#45775=CARTESIAN_POINT('Ctrl Pts',(-1.63116079730923,1.,-1.33106149345645));
#45776=CARTESIAN_POINT('Ctrl Pts',(-1.63730653475089,1.,-1.33239425103724));
#45777=CARTESIAN_POINT('Ctrl Pts',(-1.6434717485603,1.,-1.33368890676572));
#45778=CARTESIAN_POINT('Ctrl Pts',(-1.6496563728683,1.,-1.33494590467993));
#45779=CARTESIAN_POINT('Ctrl Pts',(-1.65586025952593,1.,-1.33616559745172));
#45780=CARTESIAN_POINT('Ctrl Pts',(-1.66208312541983,1.,-1.33734820885262));
#45781=CARTESIAN_POINT('Ctrl Pts',(-1.66832460783989,1.,-1.33849388654388));
#45782=CARTESIAN_POINT('Ctrl Pts',(-1.67458429426086,1.,-1.3396027347034));
#45783=CARTESIAN_POINT('Ctrl Pts',(-1.68086176030362,1.,-1.34067485185203));
#45784=CARTESIAN_POINT('Ctrl Pts',(-1.68715660868764,1.,-1.341710374848));
#45785=CARTESIAN_POINT('Ctrl Pts',(-1.6934684849687,1.,-1.34270948206319));
#45786=CARTESIAN_POINT('Ctrl Pts',(-1.69979707754427,1.,-1.34367237124483));
#45787=CARTESIAN_POINT('Ctrl Pts',(-1.70614212266738,1.,-1.34459924533831));
#45788=CARTESIAN_POINT('Ctrl Pts',(-1.71250340686822,1.,-1.34549029589416));
#45789=CARTESIAN_POINT('Ctrl Pts',(-1.7188807715049,1.,-1.34634568653227));
#45790=CARTESIAN_POINT('Ctrl Pts',(-1.72527410680674,1.,-1.34716554819527));
#45791=CARTESIAN_POINT('Ctrl Pts',(-1.7304014965394,1.,-1.34779309152035));
#45792=CARTESIAN_POINT('Ctrl Pts',(-1.73425417885907,1.,-1.34824783112887));
#45793=CARTESIAN_POINT('Ctrl Pts',(-1.73682580585691,1.,-1.34854391898045));
#45794=CARTESIAN_POINT('Ctrl Pts',(-1.73811241238545,1.,-1.34869019493419));
#45795=CARTESIAN_POINT('',(-1.31362392696032,0.,-1.15624053661742));
#45796=CARTESIAN_POINT('Origin',(0.,0.,0.));
#45797=CARTESIAN_POINT('',(-1.15624053661742,1.,-1.31362392696033));
#45798=CARTESIAN_POINT('Origin',(0.,1.,0.));
#45799=CARTESIAN_POINT('',(-1.15624053661742,0.,-1.31362392696033));
#45800=CARTESIAN_POINT('Ctrl Pts',(-1.34869019493419,-1.,-1.73811241238545));
#45801=CARTESIAN_POINT('Ctrl Pts',(-1.34869019493419,1.,-1.73811241238545));
#45802=CARTESIAN_POINT('Ctrl Pts',(-1.34854391898145,-1.,-1.73682580585819));
#45803=CARTESIAN_POINT('Ctrl Pts',(-1.34854391898145,1.,-1.73682580585819));
#45804=CARTESIAN_POINT('Ctrl Pts',(-1.34824783113158,-1.,-1.73425417886255));
#45805=CARTESIAN_POINT('Ctrl Pts',(-1.34824783113158,1.,-1.73425417886255));
#45806=CARTESIAN_POINT('Ctrl Pts',(-1.3477930915247,-1.,-1.73040149654497));
#45807=CARTESIAN_POINT('Ctrl Pts',(-1.3477930915247,1.,-1.73040149654497));
#45808=CARTESIAN_POINT('Ctrl Pts',(-1.34716554820013,-1.,-1.72527410681298));
#45809=CARTESIAN_POINT('Ctrl Pts',(-1.34716554820013,1.,-1.72527410681298));
#45810=CARTESIAN_POINT('Ctrl Pts',(-1.34634568653586,-1.,-1.7188807715095));
#45811=CARTESIAN_POINT('Ctrl Pts',(-1.34634568653586,1.,-1.7188807715095));
#45812=CARTESIAN_POINT('Ctrl Pts',(-1.34549029589563,-1.,-1.71250340687011));
#45813=CARTESIAN_POINT('Ctrl Pts',(-1.34549029589563,1.,-1.71250340687011));
#45814=CARTESIAN_POINT('Ctrl Pts',(-1.34459924533783,-1.,-1.70614212266676));
#45815=CARTESIAN_POINT('Ctrl Pts',(-1.34459924533783,1.,-1.70614212266676));
#45816=CARTESIAN_POINT('Ctrl Pts',(-1.34367237124322,-1.,-1.69979707754221));
#45817=CARTESIAN_POINT('Ctrl Pts',(-1.34367237124322,1.,-1.69979707754221));
#45818=CARTESIAN_POINT('Ctrl Pts',(-1.34270948206139,-1.,-1.6934684849664));
#45819=CARTESIAN_POINT('Ctrl Pts',(-1.34270948206139,1.,-1.6934684849664));
#45820=CARTESIAN_POINT('Ctrl Pts',(-1.34171037484673,-1.,-1.68715660868602));
#45821=CARTESIAN_POINT('Ctrl Pts',(-1.34171037484673,1.,-1.68715660868602));
#45822=CARTESIAN_POINT('Ctrl Pts',(-1.3406748518516,-1.,-1.68086176030308));
#45823=CARTESIAN_POINT('Ctrl Pts',(-1.3406748518516,1.,-1.68086176030308));
#45824=CARTESIAN_POINT('Ctrl Pts',(-1.33960273470372,-1.,-1.67458429426126));
#45825=CARTESIAN_POINT('Ctrl Pts',(-1.33960273470372,1.,-1.67458429426126));
#45826=CARTESIAN_POINT('Ctrl Pts',(-1.33849388654458,-1.,-1.66832460784078));
#45827=CARTESIAN_POINT('Ctrl Pts',(-1.33849388654458,1.,-1.66832460784078));
#45828=CARTESIAN_POINT('Ctrl Pts',(-1.33734820885331,-1.,-1.66208312542073));
#45829=CARTESIAN_POINT('Ctrl Pts',(-1.33734820885331,1.,-1.66208312542073));
#45830=CARTESIAN_POINT('Ctrl Pts',(-1.33616559745217,-1.,-1.65586025952651));
#45831=CARTESIAN_POINT('Ctrl Pts',(-1.33616559745217,1.,-1.65586025952651));
#45832=CARTESIAN_POINT('Ctrl Pts',(-1.33494590468003,-1.,-1.64965637286843));
#45833=CARTESIAN_POINT('Ctrl Pts',(-1.33494590468003,1.,-1.64965637286843));
#45834=CARTESIAN_POINT('Ctrl Pts',(-1.33368890676554,-1.,-1.64347174856007));
#45835=CARTESIAN_POINT('Ctrl Pts',(-1.33368890676554,1.,-1.64347174856007));
#45836=CARTESIAN_POINT('Ctrl Pts',(-1.33239425103694,-1.,-1.6373065347505));
#45837=CARTESIAN_POINT('Ctrl Pts',(-1.33239425103694,1.,-1.6373065347505));
#45838=CARTESIAN_POINT('Ctrl Pts',(-1.33106149345618,-1.,-1.63116079730887));
#45839=CARTESIAN_POINT('Ctrl Pts',(-1.33106149345618,1.,-1.63116079730887));
#45840=CARTESIAN_POINT('Ctrl Pts',(-1.32969019505665,-1.,-1.62503464209777));
#45841=CARTESIAN_POINT('Ctrl Pts',(-1.32969019505665,1.,-1.62503464209777));
#45842=CARTESIAN_POINT('Ctrl Pts',(-1.32828000610448,-1.,-1.61892832270723));
#45843=CARTESIAN_POINT('Ctrl Pts',(-1.32828000610448,1.,-1.61892832270723));
#45844=CARTESIAN_POINT('Ctrl Pts',(-1.32683074483365,-1.,-1.61284234015762));
#45845=CARTESIAN_POINT('Ctrl Pts',(-1.32683074483365,1.,-1.61284234015762));
#45846=CARTESIAN_POINT('Ctrl Pts',(-1.32534250785794,-1.,-1.6067775829097));
#45847=CARTESIAN_POINT('Ctrl Pts',(-1.32534250785794,1.,-1.6067775829097));
#45848=CARTESIAN_POINT('Ctrl Pts',(-1.32381550858266,-1.,-1.600735118587));
#45849=CARTESIAN_POINT('Ctrl Pts',(-1.32381550858266,1.,-1.600735118587));
#45850=CARTESIAN_POINT('Ctrl Pts',(-1.32224985747686,-1.,-1.59471591079408));
#45851=CARTESIAN_POINT('Ctrl Pts',(-1.32224985747686,1.,-1.59471591079408));
#45852=CARTESIAN_POINT('Ctrl Pts',(-1.32064537110891,-1.,-1.58872057258244));
#45853=CARTESIAN_POINT('Ctrl Pts',(-1.32064537110891,1.,-1.58872057258244));
#45854=CARTESIAN_POINT('Ctrl Pts',(-1.31900135021428,-1.,-1.58274907898829));
#45855=CARTESIAN_POINT('Ctrl Pts',(-1.31900135021428,1.,-1.58274907898829));
#45856=CARTESIAN_POINT('Ctrl Pts',(-1.31731642317183,-1.,-1.57680056505585));
#45857=CARTESIAN_POINT('Ctrl Pts',(-1.31731642317183,1.,-1.57680056505585));
#45858=CARTESIAN_POINT('Ctrl Pts',(-1.31558903860015,-1.,-1.57087397835721));
#45859=CARTESIAN_POINT('Ctrl Pts',(-1.31558903860015,1.,-1.57087397835721));
#45860=CARTESIAN_POINT('Ctrl Pts',(-1.31381795281002,-1.,-1.56496872402352));
#45861=CARTESIAN_POINT('Ctrl Pts',(-1.31381795281002,1.,-1.56496872402352));
#45862=CARTESIAN_POINT('Ctrl Pts',(-1.31200264341696,-1.,-1.55908521254822));
#45863=CARTESIAN_POINT('Ctrl Pts',(-1.31200264341696,1.,-1.55908521254822));
#45864=CARTESIAN_POINT('Ctrl Pts',(-1.31014393684221,-1.,-1.55322568759481));
#45865=CARTESIAN_POINT('Ctrl Pts',(-1.31014393684221,1.,-1.55322568759481));
#45866=CARTESIAN_POINT('Ctrl Pts',(-1.30824393907471,-1.,-1.54739413957183));
#45867=CARTESIAN_POINT('Ctrl Pts',(-1.30824393907471,1.,-1.54739413957183));
#45868=CARTESIAN_POINT('Ctrl Pts',(-1.30630475189553,-1.,-1.54159462645428));
#45869=CARTESIAN_POINT('Ctrl Pts',(-1.30630475189553,1.,-1.54159462645428));
#45870=CARTESIAN_POINT('Ctrl Pts',(-1.30432735639487,-1.,-1.53582981268976));
#45871=CARTESIAN_POINT('Ctrl Pts',(-1.30432735639487,1.,-1.53582981268976));
#45872=CARTESIAN_POINT('Ctrl Pts',(-1.3023106439557,-1.,-1.53009970283893));
#45873=CARTESIAN_POINT('Ctrl Pts',(-1.3023106439557,1.,-1.53009970283893));
#45874=CARTESIAN_POINT('Ctrl Pts',(-1.30024984366334,-1.,-1.5243995786107));
#45875=CARTESIAN_POINT('Ctrl Pts',(-1.30024984366334,1.,-1.5243995786107));
#45876=CARTESIAN_POINT('Ctrl Pts',(-1.29813791800757,-1.,-1.51872184912735));
#45877=CARTESIAN_POINT('Ctrl Pts',(-1.29813791800757,1.,-1.51872184912735));
#45878=CARTESIAN_POINT('Ctrl Pts',(-1.29596850710518,-1.,-1.51305994241412));
#45879=CARTESIAN_POINT('Ctrl Pts',(-1.29596850710518,1.,-1.51305994241412));
#45880=CARTESIAN_POINT('Ctrl Pts',(-1.29373841372843,-1.,-1.50741159078367));
#45881=CARTESIAN_POINT('Ctrl Pts',(-1.29373841372843,1.,-1.50741159078367));
#45882=CARTESIAN_POINT('Ctrl Pts',(-1.29145022885171,-1.,-1.50178230149764));
#45883=CARTESIAN_POINT('Ctrl Pts',(-1.29145022885171,1.,-1.50178230149764));
#45884=CARTESIAN_POINT('Ctrl Pts',(-1.28911506584232,-1.,-1.49618896881729));
#45885=CARTESIAN_POINT('Ctrl Pts',(-1.28911506584232,1.,-1.49618896881729));
#45886=CARTESIAN_POINT('Ctrl Pts',(-1.28674676116415,-1.,-1.4906522831275));
#45887=CARTESIAN_POINT('Ctrl Pts',(-1.28674676116415,1.,-1.4906522831275));
#45888=CARTESIAN_POINT('Ctrl Pts',(-1.28435533880184,-1.,-1.48518817118891));
#45889=CARTESIAN_POINT('Ctrl Pts',(-1.28435533880184,1.,-1.48518817118891));
#45890=CARTESIAN_POINT('Ctrl Pts',(-1.28194158939522,-1.,-1.47980070347102));
#45891=CARTESIAN_POINT('Ctrl Pts',(-1.28194158939522,1.,-1.47980070347102));
#45892=CARTESIAN_POINT('Ctrl Pts',(-1.27948918248524,-1.,-1.4744717526711));
#45893=CARTESIAN_POINT('Ctrl Pts',(-1.27948918248524,1.,-1.4744717526711));
#45894=CARTESIAN_POINT('Ctrl Pts',(-1.27696414831144,-1.,-1.46916035917197));
#45895=CARTESIAN_POINT('Ctrl Pts',(-1.27696414831144,1.,-1.46916035917197));
#45896=CARTESIAN_POINT('Ctrl Pts',(-1.27433119897877,-1.,-1.4638243133254));
#45897=CARTESIAN_POINT('Ctrl Pts',(-1.27433119897877,1.,-1.4638243133254));
#45898=CARTESIAN_POINT('Ctrl Pts',(-1.27156805265312,-1.,-1.45843906294725));
#45899=CARTESIAN_POINT('Ctrl Pts',(-1.27156805265312,1.,-1.45843906294725));
#45900=CARTESIAN_POINT('Ctrl Pts',(-1.26867786804854,-1.,-1.45301422764205));
#45901=CARTESIAN_POINT('Ctrl Pts',(-1.26867786804854,1.,-1.45301422764205));
#45902=CARTESIAN_POINT('Ctrl Pts',(-1.26570925118767,-1.,-1.44761985001544));
#45903=CARTESIAN_POINT('Ctrl Pts',(-1.26570925118767,1.,-1.44761985001544));
#45904=CARTESIAN_POINT('Ctrl Pts',(-1.26273903323723,-1.,-1.44236470511145));
#45905=CARTESIAN_POINT('Ctrl Pts',(-1.26273903323723,1.,-1.44236470511145));
#45906=CARTESIAN_POINT('Ctrl Pts',(-1.25983531011894,-1.,-1.43734919180719));
#45907=CARTESIAN_POINT('Ctrl Pts',(-1.25983531011894,1.,-1.43734919180719));
#45908=CARTESIAN_POINT('Ctrl Pts',(-1.25702687965744,-1.,-1.43262645609679));
#45909=CARTESIAN_POINT('Ctrl Pts',(-1.25702687965744,1.,-1.43262645609679));
#45910=CARTESIAN_POINT('Ctrl Pts',(-1.25426945222783,-1.,-1.42815938799555));
#45911=CARTESIAN_POINT('Ctrl Pts',(-1.25426945222783,1.,-1.42815938799555));
#45912=CARTESIAN_POINT('Ctrl Pts',(-1.25141455570299,-1.,-1.42378102115911));
#45913=CARTESIAN_POINT('Ctrl Pts',(-1.25141455570299,1.,-1.42378102115911));
#45914=CARTESIAN_POINT('Ctrl Pts',(-1.24824430986911,-1.,-1.41923722596421));
#45915=CARTESIAN_POINT('Ctrl Pts',(-1.24824430986911,1.,-1.41923722596421));
#45916=CARTESIAN_POINT('Ctrl Pts',(-1.24450600513278,-1.,-1.41422913175437));
#45917=CARTESIAN_POINT('Ctrl Pts',(-1.24450600513278,1.,-1.41422913175437));
#45918=CARTESIAN_POINT('Ctrl Pts',(-1.23994455029421,-1.,-1.40845295531151));
#45919=CARTESIAN_POINT('Ctrl Pts',(-1.23994455029421,1.,-1.40845295531151));
#45920=CARTESIAN_POINT('Ctrl Pts',(-1.23434087289768,-1.,-1.40164708205345));
#45921=CARTESIAN_POINT('Ctrl Pts',(-1.23434087289768,1.,-1.40164708205345));
#45922=CARTESIAN_POINT('Ctrl Pts',(-1.22752961898063,-1.,-1.39361389567257));
#45923=CARTESIAN_POINT('Ctrl Pts',(-1.22752961898063,1.,-1.39361389567257));
#45924=CARTESIAN_POINT('Ctrl Pts',(-1.21938737278853,-1.,-1.38420564525391));
#45925=CARTESIAN_POINT('Ctrl Pts',(-1.21938737278853,1.,-1.38420564525391));
#45926=CARTESIAN_POINT('Ctrl Pts',(-1.20982812923113,-1.,-1.37331915604962));
#45927=CARTESIAN_POINT('Ctrl Pts',(-1.20982812923113,1.,-1.37331915604962));
#45928=CARTESIAN_POINT('Ctrl Pts',(-1.1987959077656,-1.,-1.36088705040677));
#45929=CARTESIAN_POINT('Ctrl Pts',(-1.1987959077656,1.,-1.36088705040677));
#45930=CARTESIAN_POINT('Ctrl Pts',(-1.18625865664915,-1.,-1.34687053998157));
#45931=CARTESIAN_POINT('Ctrl Pts',(-1.18625865664915,1.,-1.34687053998157));
#45932=CARTESIAN_POINT('Ctrl Pts',(-1.17501305787994,-1.,-1.33437539344842));
#45933=CARTESIAN_POINT('Ctrl Pts',(-1.17501305787994,1.,-1.33437539344842));
#45934=CARTESIAN_POINT('Ctrl Pts',(-1.16589330092532,-1.,-1.32428080720544));
#45935=CARTESIAN_POINT('Ctrl Pts',(-1.16589330092532,1.,-1.32428080720544));
#45936=CARTESIAN_POINT('Ctrl Pts',(-1.15950888730433,-1.,-1.3172297721596));
#45937=CARTESIAN_POINT('Ctrl Pts',(-1.15950888730433,1.,-1.3172297721596));
#45938=CARTESIAN_POINT('Ctrl Pts',(-1.15624053661742,-1.,-1.31362392696033));
#45939=CARTESIAN_POINT('Ctrl Pts',(-1.15624053661742,1.,-1.31362392696033));
#45940=CARTESIAN_POINT('',(-1.34869019493419,1.,-1.73811241238545));
#45941=CARTESIAN_POINT('Ctrl Pts',(-1.34869019493419,1.,-1.73811241238545));
#45942=CARTESIAN_POINT('Ctrl Pts',(-1.34854391898145,1.,-1.73682580585819));
#45943=CARTESIAN_POINT('Ctrl Pts',(-1.34824783113158,1.,-1.73425417886255));
#45944=CARTESIAN_POINT('Ctrl Pts',(-1.3477930915247,1.,-1.73040149654497));
#45945=CARTESIAN_POINT('Ctrl Pts',(-1.34716554820013,1.,-1.72527410681298));
#45946=CARTESIAN_POINT('Ctrl Pts',(-1.34634568653586,1.,-1.7188807715095));
#45947=CARTESIAN_POINT('Ctrl Pts',(-1.34549029589563,1.,-1.71250340687011));
#45948=CARTESIAN_POINT('Ctrl Pts',(-1.34459924533783,1.,-1.70614212266676));
#45949=CARTESIAN_POINT('Ctrl Pts',(-1.34367237124322,1.,-1.69979707754221));
#45950=CARTESIAN_POINT('Ctrl Pts',(-1.34270948206139,1.,-1.6934684849664));
#45951=CARTESIAN_POINT('Ctrl Pts',(-1.34171037484673,1.,-1.68715660868602));
#45952=CARTESIAN_POINT('Ctrl Pts',(-1.3406748518516,1.,-1.68086176030308));
#45953=CARTESIAN_POINT('Ctrl Pts',(-1.33960273470372,1.,-1.67458429426126));
#45954=CARTESIAN_POINT('Ctrl Pts',(-1.33849388654458,1.,-1.66832460784078));
#45955=CARTESIAN_POINT('Ctrl Pts',(-1.33734820885331,1.,-1.66208312542073));
#45956=CARTESIAN_POINT('Ctrl Pts',(-1.33616559745217,1.,-1.65586025952651));
#45957=CARTESIAN_POINT('Ctrl Pts',(-1.33494590468003,1.,-1.64965637286843));
#45958=CARTESIAN_POINT('Ctrl Pts',(-1.33368890676554,1.,-1.64347174856007));
#45959=CARTESIAN_POINT('Ctrl Pts',(-1.33239425103694,1.,-1.6373065347505));
#45960=CARTESIAN_POINT('Ctrl Pts',(-1.33106149345618,1.,-1.63116079730887));
#45961=CARTESIAN_POINT('Ctrl Pts',(-1.32969019505665,1.,-1.62503464209777));
#45962=CARTESIAN_POINT('Ctrl Pts',(-1.32828000610448,1.,-1.61892832270723));
#45963=CARTESIAN_POINT('Ctrl Pts',(-1.32683074483365,1.,-1.61284234015762));
#45964=CARTESIAN_POINT('Ctrl Pts',(-1.32534250785794,1.,-1.6067775829097));
#45965=CARTESIAN_POINT('Ctrl Pts',(-1.32381550858266,1.,-1.600735118587));
#45966=CARTESIAN_POINT('Ctrl Pts',(-1.32224985747686,1.,-1.59471591079408));
#45967=CARTESIAN_POINT('Ctrl Pts',(-1.32064537110891,1.,-1.58872057258244));
#45968=CARTESIAN_POINT('Ctrl Pts',(-1.31900135021428,1.,-1.58274907898829));
#45969=CARTESIAN_POINT('Ctrl Pts',(-1.31731642317183,1.,-1.57680056505585));
#45970=CARTESIAN_POINT('Ctrl Pts',(-1.31558903860015,1.,-1.57087397835721));
#45971=CARTESIAN_POINT('Ctrl Pts',(-1.31381795281002,1.,-1.56496872402352));
#45972=CARTESIAN_POINT('Ctrl Pts',(-1.31200264341696,1.,-1.55908521254822));
#45973=CARTESIAN_POINT('Ctrl Pts',(-1.31014393684221,1.,-1.55322568759481));
#45974=CARTESIAN_POINT('Ctrl Pts',(-1.30824393907471,1.,-1.54739413957183));
#45975=CARTESIAN_POINT('Ctrl Pts',(-1.30630475189553,1.,-1.54159462645428));
#45976=CARTESIAN_POINT('Ctrl Pts',(-1.30432735639487,1.,-1.53582981268976));
#45977=CARTESIAN_POINT('Ctrl Pts',(-1.3023106439557,1.,-1.53009970283893));
#45978=CARTESIAN_POINT('Ctrl Pts',(-1.30024984366334,1.,-1.5243995786107));
#45979=CARTESIAN_POINT('Ctrl Pts',(-1.29813791800757,1.,-1.51872184912735));
#45980=CARTESIAN_POINT('Ctrl Pts',(-1.29596850710518,1.,-1.51305994241412));
#45981=CARTESIAN_POINT('Ctrl Pts',(-1.29373841372843,1.,-1.50741159078367));
#45982=CARTESIAN_POINT('Ctrl Pts',(-1.29145022885171,1.,-1.50178230149764));
#45983=CARTESIAN_POINT('Ctrl Pts',(-1.28911506584232,1.,-1.49618896881729));
#45984=CARTESIAN_POINT('Ctrl Pts',(-1.28674676116415,1.,-1.4906522831275));
#45985=CARTESIAN_POINT('Ctrl Pts',(-1.28435533880184,1.,-1.48518817118891));
#45986=CARTESIAN_POINT('Ctrl Pts',(-1.28194158939522,1.,-1.47980070347102));
#45987=CARTESIAN_POINT('Ctrl Pts',(-1.27948918248524,1.,-1.4744717526711));
#45988=CARTESIAN_POINT('Ctrl Pts',(-1.27696414831144,1.,-1.46916035917197));
#45989=CARTESIAN_POINT('Ctrl Pts',(-1.27433119897877,1.,-1.4638243133254));
#45990=CARTESIAN_POINT('Ctrl Pts',(-1.27156805265312,1.,-1.45843906294725));
#45991=CARTESIAN_POINT('Ctrl Pts',(-1.26867786804854,1.,-1.45301422764205));
#45992=CARTESIAN_POINT('Ctrl Pts',(-1.26570925118767,1.,-1.44761985001544));
#45993=CARTESIAN_POINT('Ctrl Pts',(-1.26273903323723,1.,-1.44236470511145));
#45994=CARTESIAN_POINT('Ctrl Pts',(-1.25983531011894,1.,-1.43734919180719));
#45995=CARTESIAN_POINT('Ctrl Pts',(-1.25702687965744,1.,-1.43262645609679));
#45996=CARTESIAN_POINT('Ctrl Pts',(-1.25426945222783,1.,-1.42815938799555));
#45997=CARTESIAN_POINT('Ctrl Pts',(-1.25141455570299,1.,-1.42378102115911));
#45998=CARTESIAN_POINT('Ctrl Pts',(-1.24824430986911,1.,-1.41923722596421));
#45999=CARTESIAN_POINT('Ctrl Pts',(-1.24450600513278,1.,-1.41422913175437));
#46000=CARTESIAN_POINT('Ctrl Pts',(-1.23994455029421,1.,-1.40845295531151));
#46001=CARTESIAN_POINT('Ctrl Pts',(-1.23434087289768,1.,-1.40164708205345));
#46002=CARTESIAN_POINT('Ctrl Pts',(-1.22752961898063,1.,-1.39361389567257));
#46003=CARTESIAN_POINT('Ctrl Pts',(-1.21938737278853,1.,-1.38420564525391));
#46004=CARTESIAN_POINT('Ctrl Pts',(-1.20982812923113,1.,-1.37331915604962));
#46005=CARTESIAN_POINT('Ctrl Pts',(-1.1987959077656,1.,-1.36088705040677));
#46006=CARTESIAN_POINT('Ctrl Pts',(-1.18625865664915,1.,-1.34687053998157));
#46007=CARTESIAN_POINT('Ctrl Pts',(-1.17501305787994,1.,-1.33437539344842));
#46008=CARTESIAN_POINT('Ctrl Pts',(-1.16589330092532,1.,-1.32428080720544));
#46009=CARTESIAN_POINT('Ctrl Pts',(-1.15950888730433,1.,-1.3172297721596));
#46010=CARTESIAN_POINT('Ctrl Pts',(-1.15624053661742,1.,-1.31362392696033));
#46011=CARTESIAN_POINT('',(-1.34869019493419,0.,-1.73811241238545));
#46012=CARTESIAN_POINT('Origin',(-1.23627494547115,0.,-1.81978687191668));
#46013=CARTESIAN_POINT('',(-1.23627494547115,1.,-1.81978687191668));
#46014=CARTESIAN_POINT('',(-1.34869019493419,1.,-1.73811241238545));
#46015=CARTESIAN_POINT('',(-1.23627494547115,0.,-1.81978687191668));
#46016=CARTESIAN_POINT('Ctrl Pts',(-0.892032620296855,-1.,-1.5055822144029));
#46017=CARTESIAN_POINT('Ctrl Pts',(-0.892032620296855,1.,-1.5055822144029));
#46018=CARTESIAN_POINT('Ctrl Pts',(-0.894452006967538,-1.,-1.50980486807181));
#46019=CARTESIAN_POINT('Ctrl Pts',(-0.894452006967538,1.,-1.50980486807181));
#46020=CARTESIAN_POINT('Ctrl Pts',(-0.89918504749193,-1.,-1.51805569591479));
#46021=CARTESIAN_POINT('Ctrl Pts',(-0.89918504749193,1.,-1.51805569591479));
#46022=CARTESIAN_POINT('Ctrl Pts',(-0.905967409640499,-1.,-1.52984849890434));
#46023=CARTESIAN_POINT('Ctrl Pts',(-0.905967409640499,1.,-1.52984849890434));
#46024=CARTESIAN_POINT('Ctrl Pts',(-0.91437591904658,-1.,-1.54440491152808));
#46025=CARTESIAN_POINT('Ctrl Pts',(-0.91437591904658,1.,-1.54440491152808));
#46026=CARTESIAN_POINT('Ctrl Pts',(-0.923832188966322,-1.,-1.56065988582509));
#46027=CARTESIAN_POINT('Ctrl Pts',(-0.923832188966322,1.,-1.56065988582509));
#46028=CARTESIAN_POINT('Ctrl Pts',(-0.932246680128849,-1.,-1.57499388385561));
#46029=CARTESIAN_POINT('Ctrl Pts',(-0.932246680128849,1.,-1.57499388385561));
#46030=CARTESIAN_POINT('Ctrl Pts',(-0.939646377909319,-1.,-1.58744937489796));
#46031=CARTESIAN_POINT('Ctrl Pts',(-0.939646377909319,1.,-1.58744937489796));
#46032=CARTESIAN_POINT('Ctrl Pts',(-0.946078063325796,-1.,-1.59810042045408));
#46033=CARTESIAN_POINT('Ctrl Pts',(-0.946078063325796,1.,-1.59810042045408));
#46034=CARTESIAN_POINT('Ctrl Pts',(-0.951613284361248,-1.,-1.60706069897794));
#46035=CARTESIAN_POINT('Ctrl Pts',(-0.951613284361248,1.,-1.60706069897794));
#46036=CARTESIAN_POINT('Ctrl Pts',(-0.956354422921573,-1.,-1.61449324337233));
#46037=CARTESIAN_POINT('Ctrl Pts',(-0.956354422921573,1.,-1.61449324337233));
#46038=CARTESIAN_POINT('Ctrl Pts',(-0.960438326099958,-1.,-1.62061638139929));
#46039=CARTESIAN_POINT('Ctrl Pts',(-0.960438326099958,1.,-1.62061638139929));
#46040=CARTESIAN_POINT('Ctrl Pts',(-0.964046107037821,-1.,-1.6257193066974));
#46041=CARTESIAN_POINT('Ctrl Pts',(-0.964046107037821,1.,-1.6257193066974));
#46042=CARTESIAN_POINT('Ctrl Pts',(-0.967387853228041,-1.,-1.63013849959083));
#46043=CARTESIAN_POINT('Ctrl Pts',(-0.967387853228041,1.,-1.63013849959083));
#46044=CARTESIAN_POINT('Ctrl Pts',(-0.970669715996356,-1.,-1.63420665729609));
#46045=CARTESIAN_POINT('Ctrl Pts',(-0.970669715996356,1.,-1.63420665729609));
#46046=CARTESIAN_POINT('Ctrl Pts',(-0.974066058287501,-1.,-1.63820952658157));
#46047=CARTESIAN_POINT('Ctrl Pts',(-0.974066058287501,1.,-1.63820952658157));
#46048=CARTESIAN_POINT('Ctrl Pts',(-0.977689794120297,-1.,-1.64233990826831));
#46049=CARTESIAN_POINT('Ctrl Pts',(-0.977689794120297,1.,-1.64233990826831));
#46050=CARTESIAN_POINT('Ctrl Pts',(-0.981562530940574,-1.,-1.64665139190834));
#46051=CARTESIAN_POINT('Ctrl Pts',(-0.981562530940574,1.,-1.64665139190834));
#46052=CARTESIAN_POINT('Ctrl Pts',(-0.985642622921626,-1.,-1.6511001661277));
#46053=CARTESIAN_POINT('Ctrl Pts',(-0.985642622921626,1.,-1.6511001661277));
#46054=CARTESIAN_POINT('Ctrl Pts',(-0.98985562785445,-1.,-1.65559044289746));
#46055=CARTESIAN_POINT('Ctrl Pts',(-0.98985562785445,1.,-1.65559044289746));
#46056=CARTESIAN_POINT('Ctrl Pts',(-0.994121836661116,-1.,-1.66001553809916));
#46057=CARTESIAN_POINT('Ctrl Pts',(-0.994121836661116,1.,-1.66001553809916));
#46058=CARTESIAN_POINT('Ctrl Pts',(-0.998389654952317,-1.,-1.66430758030304));
#46059=CARTESIAN_POINT('Ctrl Pts',(-0.998389654952317,1.,-1.66430758030304));
#46060=CARTESIAN_POINT('Ctrl Pts',(-1.00265091003682,-1.,-1.66846059277231));
#46061=CARTESIAN_POINT('Ctrl Pts',(-1.00265091003682,1.,-1.66846059277231));
#46062=CARTESIAN_POINT('Ctrl Pts',(-1.00692206696387,-1.,-1.67250335383248));
#46063=CARTESIAN_POINT('Ctrl Pts',(-1.00692206696387,1.,-1.67250335383248));
#46064=CARTESIAN_POINT('Ctrl Pts',(-1.01123236493507,-1.,-1.67648246776457));
#46065=CARTESIAN_POINT('Ctrl Pts',(-1.01123236493507,1.,-1.67648246776457));
#46066=CARTESIAN_POINT('Ctrl Pts',(-1.01561026162787,-1.,-1.6804428989482));
#46067=CARTESIAN_POINT('Ctrl Pts',(-1.01561026162787,1.,-1.6804428989482));
#46068=CARTESIAN_POINT('Ctrl Pts',(-1.02006795074222,-1.,-1.68440578021739));
#46069=CARTESIAN_POINT('Ctrl Pts',(-1.02006795074222,1.,-1.68440578021739));
#46070=CARTESIAN_POINT('Ctrl Pts',(-1.02460180535272,-1.,-1.68836910178475));
#46071=CARTESIAN_POINT('Ctrl Pts',(-1.02460180535272,1.,-1.68836910178475));
#46072=CARTESIAN_POINT('Ctrl Pts',(-1.02919977579155,-1.,-1.69231840863471));
#46073=CARTESIAN_POINT('Ctrl Pts',(-1.02919977579155,1.,-1.69231840863471));
#46074=CARTESIAN_POINT('Ctrl Pts',(-1.03384646003587,-1.,-1.69623414782769));
#46075=CARTESIAN_POINT('Ctrl Pts',(-1.03384646003587,1.,-1.69623414782769));
#46076=CARTESIAN_POINT('Ctrl Pts',(-1.03852922490782,-1.,-1.70010052930951));
#46077=CARTESIAN_POINT('Ctrl Pts',(-1.03852922490782,1.,-1.70010052930951));
#46078=CARTESIAN_POINT('Ctrl Pts',(-1.04324363334546,-1.,-1.70391338707969));
#46079=CARTESIAN_POINT('Ctrl Pts',(-1.04324363334546,1.,-1.70391338707969));
#46080=CARTESIAN_POINT('Ctrl Pts',(-1.0479908540499,-1.,-1.70767646263641));
#46081=CARTESIAN_POINT('Ctrl Pts',(-1.0479908540499,1.,-1.70767646263641));
#46082=CARTESIAN_POINT('Ctrl Pts',(-1.05277517202854,-1.,-1.71139783543986));
#46083=CARTESIAN_POINT('Ctrl Pts',(-1.05277517202854,1.,-1.71139783543986));
#46084=CARTESIAN_POINT('Ctrl Pts',(-1.05760163192481,-1.,-1.71508654427022));
#46085=CARTESIAN_POINT('Ctrl Pts',(-1.05760163192481,1.,-1.71508654427022));
#46086=CARTESIAN_POINT('Ctrl Pts',(-1.0624732468065,-1.,-1.71874858456908));
#46087=CARTESIAN_POINT('Ctrl Pts',(-1.0624732468065,1.,-1.71874858456908));
#46088=CARTESIAN_POINT('Ctrl Pts',(-1.06738966975463,-1.,-1.72238500928456));
#46089=CARTESIAN_POINT('Ctrl Pts',(-1.06738966975463,1.,-1.72238500928456));
#46090=CARTESIAN_POINT('Ctrl Pts',(-1.07234866990252,-1.,-1.72599406198489));
#46091=CARTESIAN_POINT('Ctrl Pts',(-1.07234866990252,1.,-1.72599406198489));
#46092=CARTESIAN_POINT('Ctrl Pts',(-1.0773470373727,-1.,-1.72957248977424));
#46093=CARTESIAN_POINT('Ctrl Pts',(-1.0773470373727,1.,-1.72957248977424));
#46094=CARTESIAN_POINT('Ctrl Pts',(-1.08238162784749,-1.,-1.73311705663407));
#46095=CARTESIAN_POINT('Ctrl Pts',(-1.08238162784749,1.,-1.73311705663407));
#46096=CARTESIAN_POINT('Ctrl Pts',(-1.08745056285429,-1.,-1.73662628326093));
#46097=CARTESIAN_POINT('Ctrl Pts',(-1.08745056285429,1.,-1.73662628326093));
#46098=CARTESIAN_POINT('Ctrl Pts',(-1.09255329056496,-1.,-1.74010053962252));
#46099=CARTESIAN_POINT('Ctrl Pts',(-1.09255329056496,1.,-1.74010053962252));
#46100=CARTESIAN_POINT('Ctrl Pts',(-1.09768999241229,-1.,-1.74354119236212));
#46101=CARTESIAN_POINT('Ctrl Pts',(-1.09768999241229,1.,-1.74354119236212));
#46102=CARTESIAN_POINT('Ctrl Pts',(-1.10286118991144,-1.,-1.74695004214924));
#46103=CARTESIAN_POINT('Ctrl Pts',(-1.10286118991144,1.,-1.74695004214924));
#46104=CARTESIAN_POINT('Ctrl Pts',(-1.10806728183003,-1.,-1.75032866075914));
#46105=CARTESIAN_POINT('Ctrl Pts',(-1.10806728183003,1.,-1.75032866075914));
#46106=CARTESIAN_POINT('Ctrl Pts',(-1.11330807582542,-1.,-1.75367772094617));
#46107=CARTESIAN_POINT('Ctrl Pts',(-1.11330807582542,1.,-1.75367772094617));
#46108=CARTESIAN_POINT('Ctrl Pts',(-1.11858293216752,-1.,-1.75699720772089));
#46109=CARTESIAN_POINT('Ctrl Pts',(-1.11858293216752,1.,-1.75699720772089));
#46110=CARTESIAN_POINT('Ctrl Pts',(-1.12389096855078,-1.,-1.76028671825084));
#46111=CARTESIAN_POINT('Ctrl Pts',(-1.12389096855078,1.,-1.76028671825084));
#46112=CARTESIAN_POINT('Ctrl Pts',(-1.12923123555076,-1.,-1.76354571966171));
#46113=CARTESIAN_POINT('Ctrl Pts',(-1.12923123555076,1.,-1.76354571966171));
#46114=CARTESIAN_POINT('Ctrl Pts',(-1.13460291804635,-1.,-1.76677384551883));
#46115=CARTESIAN_POINT('Ctrl Pts',(-1.13460291804635,1.,-1.76677384551883));
#46116=CARTESIAN_POINT('Ctrl Pts',(-1.14000548337,-1.,-1.76997111386806));
#46117=CARTESIAN_POINT('Ctrl Pts',(-1.14000548337,1.,-1.76997111386806));
#46118=CARTESIAN_POINT('Ctrl Pts',(-1.14543858226948,-1.,-1.77313777896234));
#46119=CARTESIAN_POINT('Ctrl Pts',(-1.14543858226948,1.,-1.77313777896234));
#46120=CARTESIAN_POINT('Ctrl Pts',(-1.15090197841531,-1.,-1.77627422557034));
#46121=CARTESIAN_POINT('Ctrl Pts',(-1.15090197841531,1.,-1.77627422557034));
#46122=CARTESIAN_POINT('Ctrl Pts',(-1.15639547194689,-1.,-1.77938085564261));
#46123=CARTESIAN_POINT('Ctrl Pts',(-1.15639547194689,1.,-1.77938085564261));
#46124=CARTESIAN_POINT('Ctrl Pts',(-1.16191881298458,-1.,-1.78245795880949));
#46125=CARTESIAN_POINT('Ctrl Pts',(-1.16191881298458,1.,-1.78245795880949));
#46126=CARTESIAN_POINT('Ctrl Pts',(-1.16747166312239,-1.,-1.78550566040349));
#46127=CARTESIAN_POINT('Ctrl Pts',(-1.16747166312239,1.,-1.78550566040349));
#46128=CARTESIAN_POINT('Ctrl Pts',(-1.17305363177265,-1.,-1.78852398877523));
#46129=CARTESIAN_POINT('Ctrl Pts',(-1.17305363177265,1.,-1.78852398877523));
#46130=CARTESIAN_POINT('Ctrl Pts',(-1.17866429440781,-1.,-1.79151291552646));
#46131=CARTESIAN_POINT('Ctrl Pts',(-1.17866429440781,1.,-1.79151291552646));
#46132=CARTESIAN_POINT('Ctrl Pts',(-1.18430321697471,-1.,-1.79447240321572));
#46133=CARTESIAN_POINT('Ctrl Pts',(-1.18430321697471,1.,-1.79447240321572));
#46134=CARTESIAN_POINT('Ctrl Pts',(-1.1899699793456,-1.,-1.79740245923649));
#46135=CARTESIAN_POINT('Ctrl Pts',(-1.1899699793456,1.,-1.79740245923649));
#46136=CARTESIAN_POINT('Ctrl Pts',(-1.19566418930405,-1.,-1.80030314370121));
#46137=CARTESIAN_POINT('Ctrl Pts',(-1.19566418930405,1.,-1.80030314370121));
#46138=CARTESIAN_POINT('Ctrl Pts',(-1.2013854893912,-1.,-1.8031745483882));
#46139=CARTESIAN_POINT('Ctrl Pts',(-1.2013854893912,1.,-1.8031745483882));
#46140=CARTESIAN_POINT('Ctrl Pts',(-1.20713356605519,-1.,-1.80601678480772));
#46141=CARTESIAN_POINT('Ctrl Pts',(-1.20713356605519,1.,-1.80601678480772));
#46142=CARTESIAN_POINT('Ctrl Pts',(-1.2129081570818,-1.,-1.80882996916931));
#46143=CARTESIAN_POINT('Ctrl Pts',(-1.2129081570818,1.,-1.80882996916931));
#46144=CARTESIAN_POINT('Ctrl Pts',(-1.2187090610323,-1.,-1.81161420806172));
#46145=CARTESIAN_POINT('Ctrl Pts',(-1.2187090610323,1.,-1.81161420806172));
#46146=CARTESIAN_POINT('Ctrl Pts',(-1.22453613304507,-1.,-1.81436959209778));
#46147=CARTESIAN_POINT('Ctrl Pts',(-1.22453613304507,1.,-1.81436959209778));
#46148=CARTESIAN_POINT('Ctrl Pts',(-1.22921864890975,-1.,-1.81655087183054));
#46149=CARTESIAN_POINT('Ctrl Pts',(-1.22921864890975,1.,-1.81655087183054));
#46150=CARTESIAN_POINT('Ctrl Pts',(-1.23274224526804,-1.,-1.81817389920914));
#46151=CARTESIAN_POINT('Ctrl Pts',(-1.23274224526804,1.,-1.81817389920914));
#46152=CARTESIAN_POINT('Ctrl Pts',(-1.23509651170384,-1.,-1.81925017193531));
#46153=CARTESIAN_POINT('Ctrl Pts',(-1.23509651170384,1.,-1.81925017193531));
#46154=CARTESIAN_POINT('Ctrl Pts',(-1.23627494547115,-1.,-1.81978687191668));
#46155=CARTESIAN_POINT('Ctrl Pts',(-1.23627494547115,1.,-1.81978687191668));
#46156=CARTESIAN_POINT('',(-0.892032620296855,1.,-1.5055822144029));
#46157=CARTESIAN_POINT('Ctrl Pts',(-0.892032620296855,1.,-1.5055822144029));
#46158=CARTESIAN_POINT('Ctrl Pts',(-0.894452006967538,1.,-1.50980486807181));
#46159=CARTESIAN_POINT('Ctrl Pts',(-0.89918504749193,1.,-1.51805569591479));
#46160=CARTESIAN_POINT('Ctrl Pts',(-0.905967409640499,1.,-1.52984849890434));
#46161=CARTESIAN_POINT('Ctrl Pts',(-0.91437591904658,1.,-1.54440491152808));
#46162=CARTESIAN_POINT('Ctrl Pts',(-0.923832188966322,1.,-1.56065988582509));
#46163=CARTESIAN_POINT('Ctrl Pts',(-0.932246680128849,1.,-1.57499388385561));
#46164=CARTESIAN_POINT('Ctrl Pts',(-0.939646377909319,1.,-1.58744937489796));
#46165=CARTESIAN_POINT('Ctrl Pts',(-0.946078063325796,1.,-1.59810042045408));
#46166=CARTESIAN_POINT('Ctrl Pts',(-0.951613284361248,1.,-1.60706069897794));
#46167=CARTESIAN_POINT('Ctrl Pts',(-0.956354422921573,1.,-1.61449324337233));
#46168=CARTESIAN_POINT('Ctrl Pts',(-0.960438326099958,1.,-1.62061638139929));
#46169=CARTESIAN_POINT('Ctrl Pts',(-0.964046107037821,1.,-1.6257193066974));
#46170=CARTESIAN_POINT('Ctrl Pts',(-0.967387853228041,1.,-1.63013849959083));
#46171=CARTESIAN_POINT('Ctrl Pts',(-0.970669715996356,1.,-1.63420665729609));
#46172=CARTESIAN_POINT('Ctrl Pts',(-0.974066058287501,1.,-1.63820952658157));
#46173=CARTESIAN_POINT('Ctrl Pts',(-0.977689794120297,1.,-1.64233990826831));
#46174=CARTESIAN_POINT('Ctrl Pts',(-0.981562530940574,1.,-1.64665139190834));
#46175=CARTESIAN_POINT('Ctrl Pts',(-0.985642622921626,1.,-1.6511001661277));
#46176=CARTESIAN_POINT('Ctrl Pts',(-0.98985562785445,1.,-1.65559044289746));
#46177=CARTESIAN_POINT('Ctrl Pts',(-0.994121836661116,1.,-1.66001553809916));
#46178=CARTESIAN_POINT('Ctrl Pts',(-0.998389654952317,1.,-1.66430758030304));
#46179=CARTESIAN_POINT('Ctrl Pts',(-1.00265091003682,1.,-1.66846059277231));
#46180=CARTESIAN_POINT('Ctrl Pts',(-1.00692206696387,1.,-1.67250335383248));
#46181=CARTESIAN_POINT('Ctrl Pts',(-1.01123236493507,1.,-1.67648246776457));
#46182=CARTESIAN_POINT('Ctrl Pts',(-1.01561026162787,1.,-1.6804428989482));
#46183=CARTESIAN_POINT('Ctrl Pts',(-1.02006795074222,1.,-1.68440578021739));
#46184=CARTESIAN_POINT('Ctrl Pts',(-1.02460180535272,1.,-1.68836910178475));
#46185=CARTESIAN_POINT('Ctrl Pts',(-1.02919977579155,1.,-1.69231840863471));
#46186=CARTESIAN_POINT('Ctrl Pts',(-1.03384646003587,1.,-1.69623414782769));
#46187=CARTESIAN_POINT('Ctrl Pts',(-1.03852922490782,1.,-1.70010052930951));
#46188=CARTESIAN_POINT('Ctrl Pts',(-1.04324363334546,1.,-1.70391338707969));
#46189=CARTESIAN_POINT('Ctrl Pts',(-1.0479908540499,1.,-1.70767646263641));
#46190=CARTESIAN_POINT('Ctrl Pts',(-1.05277517202854,1.,-1.71139783543986));
#46191=CARTESIAN_POINT('Ctrl Pts',(-1.05760163192481,1.,-1.71508654427022));
#46192=CARTESIAN_POINT('Ctrl Pts',(-1.0624732468065,1.,-1.71874858456908));
#46193=CARTESIAN_POINT('Ctrl Pts',(-1.06738966975463,1.,-1.72238500928456));
#46194=CARTESIAN_POINT('Ctrl Pts',(-1.07234866990252,1.,-1.72599406198489));
#46195=CARTESIAN_POINT('Ctrl Pts',(-1.0773470373727,1.,-1.72957248977424));
#46196=CARTESIAN_POINT('Ctrl Pts',(-1.08238162784749,1.,-1.73311705663407));
#46197=CARTESIAN_POINT('Ctrl Pts',(-1.08745056285429,1.,-1.73662628326093));
#46198=CARTESIAN_POINT('Ctrl Pts',(-1.09255329056496,1.,-1.74010053962252));
#46199=CARTESIAN_POINT('Ctrl Pts',(-1.09768999241229,1.,-1.74354119236212));
#46200=CARTESIAN_POINT('Ctrl Pts',(-1.10286118991144,1.,-1.74695004214924));
#46201=CARTESIAN_POINT('Ctrl Pts',(-1.10806728183003,1.,-1.75032866075914));
#46202=CARTESIAN_POINT('Ctrl Pts',(-1.11330807582542,1.,-1.75367772094617));
#46203=CARTESIAN_POINT('Ctrl Pts',(-1.11858293216752,1.,-1.75699720772089));
#46204=CARTESIAN_POINT('Ctrl Pts',(-1.12389096855078,1.,-1.76028671825084));
#46205=CARTESIAN_POINT('Ctrl Pts',(-1.12923123555076,1.,-1.76354571966171));
#46206=CARTESIAN_POINT('Ctrl Pts',(-1.13460291804635,1.,-1.76677384551883));
#46207=CARTESIAN_POINT('Ctrl Pts',(-1.14000548337,1.,-1.76997111386806));
#46208=CARTESIAN_POINT('Ctrl Pts',(-1.14543858226948,1.,-1.77313777896234));
#46209=CARTESIAN_POINT('Ctrl Pts',(-1.15090197841531,1.,-1.77627422557034));
#46210=CARTESIAN_POINT('Ctrl Pts',(-1.15639547194689,1.,-1.77938085564261));
#46211=CARTESIAN_POINT('Ctrl Pts',(-1.16191881298458,1.,-1.78245795880949));
#46212=CARTESIAN_POINT('Ctrl Pts',(-1.16747166312239,1.,-1.78550566040349));
#46213=CARTESIAN_POINT('Ctrl Pts',(-1.17305363177265,1.,-1.78852398877523));
#46214=CARTESIAN_POINT('Ctrl Pts',(-1.17866429440781,1.,-1.79151291552646));
#46215=CARTESIAN_POINT('Ctrl Pts',(-1.18430321697471,1.,-1.79447240321572));
#46216=CARTESIAN_POINT('Ctrl Pts',(-1.1899699793456,1.,-1.79740245923649));
#46217=CARTESIAN_POINT('Ctrl Pts',(-1.19566418930405,1.,-1.80030314370121));
#46218=CARTESIAN_POINT('Ctrl Pts',(-1.2013854893912,1.,-1.8031745483882));
#46219=CARTESIAN_POINT('Ctrl Pts',(-1.20713356605519,1.,-1.80601678480772));
#46220=CARTESIAN_POINT('Ctrl Pts',(-1.2129081570818,1.,-1.80882996916931));
#46221=CARTESIAN_POINT('Ctrl Pts',(-1.2187090610323,1.,-1.81161420806172));
#46222=CARTESIAN_POINT('Ctrl Pts',(-1.22453613304507,1.,-1.81436959209778));
#46223=CARTESIAN_POINT('Ctrl Pts',(-1.22921864890975,1.,-1.81655087183054));
#46224=CARTESIAN_POINT('Ctrl Pts',(-1.23274224526804,1.,-1.81817389920914));
#46225=CARTESIAN_POINT('Ctrl Pts',(-1.23509651170384,1.,-1.81925017193531));
#46226=CARTESIAN_POINT('Ctrl Pts',(-1.23627494547115,1.,-1.81978687191668));
#46227=CARTESIAN_POINT('',(-0.892032620296856,0.,-1.5055822144029));
#46228=CARTESIAN_POINT('Origin',(0.,0.,0.));
#46229=CARTESIAN_POINT('',(-0.693717979106305,1.,-1.60662857109684));
#46230=CARTESIAN_POINT('Origin',(0.,1.,0.));
#46231=CARTESIAN_POINT('',(-0.693717979106306,0.,-1.60662857109684));
#46232=CARTESIAN_POINT('Ctrl Pts',(-0.745574324794401,-1.,-2.0698113262342));
#46233=CARTESIAN_POINT('Ctrl Pts',(-0.745574324794401,1.,-2.0698113262342));
#46234=CARTESIAN_POINT('Ctrl Pts',(-0.745832791378367,-1.,-2.06854248895728));
#46235=CARTESIAN_POINT('Ctrl Pts',(-0.745832791378367,1.,-2.06854248895728));
#46236=CARTESIAN_POINT('Ctrl Pts',(-0.7463458715442,-1.,-2.06600523016815));
#46237=CARTESIAN_POINT('Ctrl Pts',(-0.7463458715442,1.,-2.06600523016815));
#46238=CARTESIAN_POINT('Ctrl Pts',(-0.747103932787919,-1.,-2.06220058927826));
#46239=CARTESIAN_POINT('Ctrl Pts',(-0.747103932787919,1.,-2.06220058927826));
#46240=CARTESIAN_POINT('Ctrl Pts',(-0.748091554183802,-1.,-2.05713023031006));
#46241=CARTESIAN_POINT('Ctrl Pts',(-0.748091554183802,1.,-2.05713023031006));
#46242=CARTESIAN_POINT('Ctrl Pts',(-0.749287468665046,-1.,-2.05079645592154));
#46243=CARTESIAN_POINT('Ctrl Pts',(-0.749287468665046,1.,-2.05079645592154));
#46244=CARTESIAN_POINT('Ctrl Pts',(-0.750444657875576,-1.,-2.04446689147979));
#46245=CARTESIAN_POINT('Ctrl Pts',(-0.750444657875576,1.,-2.04446689147979));
#46246=CARTESIAN_POINT('Ctrl Pts',(-0.751562963361115,-1.,-2.03814160092099));
#46247=CARTESIAN_POINT('Ctrl Pts',(-0.751562963361115,1.,-2.03814160092099));
#46248=CARTESIAN_POINT('Ctrl Pts',(-0.752642180487211,-1.,-2.03182068456221));
#46249=CARTESIAN_POINT('Ctrl Pts',(-0.752642180487211,1.,-2.03182068456221));
#46250=CARTESIAN_POINT('Ctrl Pts',(-0.753682061112768,-1.,-2.02550428623313));
#46251=CARTESIAN_POINT('Ctrl Pts',(-0.753682061112768,1.,-2.02550428623313));
#46252=CARTESIAN_POINT('Ctrl Pts',(-0.754682330722816,-1.,-2.01919259405809));
#46253=CARTESIAN_POINT('Ctrl Pts',(-0.754682330722816,1.,-2.01919259405809));
#46254=CARTESIAN_POINT('Ctrl Pts',(-0.755642704957865,-1.,-2.01288584328084));
#46255=CARTESIAN_POINT('Ctrl Pts',(-0.755642704957865,1.,-2.01288584328084));
#46256=CARTESIAN_POINT('Ctrl Pts',(-0.75656290464667,-1.,-2.0065843158773));
#46257=CARTESIAN_POINT('Ctrl Pts',(-0.75656290464667,1.,-2.0065843158773));
#46258=CARTESIAN_POINT('Ctrl Pts',(-0.757442676862724,-1.,-2.00028834739178));
#46259=CARTESIAN_POINT('Ctrl Pts',(-0.757442676862724,1.,-2.00028834739178));
#46260=CARTESIAN_POINT('Ctrl Pts',(-0.758281796766761,-1.,-1.99399831098817));
#46261=CARTESIAN_POINT('Ctrl Pts',(-0.758281796766761,1.,-1.99399831098817));
#46262=CARTESIAN_POINT('Ctrl Pts',(-0.759080037802488,-1.,-1.98771456680874));
#46263=CARTESIAN_POINT('Ctrl Pts',(-0.759080037802488,1.,-1.98771456680874));
#46264=CARTESIAN_POINT('Ctrl Pts',(-0.75983714745219,-1.,-1.98143741418172));
#46265=CARTESIAN_POINT('Ctrl Pts',(-0.75983714745219,1.,-1.98143741418172));
#46266=CARTESIAN_POINT('Ctrl Pts',(-0.760552825409757,-1.,-1.97516705321494));
#46267=CARTESIAN_POINT('Ctrl Pts',(-0.760552825409757,1.,-1.97516705321494));
#46268=CARTESIAN_POINT('Ctrl Pts',(-0.76122669048382,-1.,-1.96890351582499));
#46269=CARTESIAN_POINT('Ctrl Pts',(-0.76122669048382,1.,-1.96890351582499));
#46270=CARTESIAN_POINT('Ctrl Pts',(-0.761858300014423,-1.,-1.96264672744186));
#46271=CARTESIAN_POINT('Ctrl Pts',(-0.761858300014423,1.,-1.96264672744186));
#46272=CARTESIAN_POINT('Ctrl Pts',(-0.762447203806179,-1.,-1.95639665309869));
#46273=CARTESIAN_POINT('Ctrl Pts',(-0.762447203806179,1.,-1.95639665309869));
#46274=CARTESIAN_POINT('Ctrl Pts',(-0.762992990878769,-1.,-1.95015342590024));
#46275=CARTESIAN_POINT('Ctrl Pts',(-0.762992990878769,1.,-1.95015342590024));
#46276=CARTESIAN_POINT('Ctrl Pts',(-0.763495333538629,-1.,-1.9439174661764));
#46277=CARTESIAN_POINT('Ctrl Pts',(-0.763495333538629,1.,-1.9439174661764));
#46278=CARTESIAN_POINT('Ctrl Pts',(-0.763954049121458,-1.,-1.93768964875886));
#46279=CARTESIAN_POINT('Ctrl Pts',(-0.763954049121458,1.,-1.93768964875886));
#46280=CARTESIAN_POINT('Ctrl Pts',(-0.764369010673941,-1.,-1.93147105496382));
#46281=CARTESIAN_POINT('Ctrl Pts',(-0.764369010673941,1.,-1.93147105496382));
#46282=CARTESIAN_POINT('Ctrl Pts',(-0.764740025488211,-1.,-1.92526263537048));
#46283=CARTESIAN_POINT('Ctrl Pts',(-0.764740025488211,1.,-1.92526263537048));
#46284=CARTESIAN_POINT('Ctrl Pts',(-0.765066729667088,-1.,-1.91906491634196));
#46285=CARTESIAN_POINT('Ctrl Pts',(-0.765066729667088,1.,-1.91906491634196));
#46286=CARTESIAN_POINT('Ctrl Pts',(-0.765348465884722,-1.,-1.91287765805169));
#46287=CARTESIAN_POINT('Ctrl Pts',(-0.765348465884722,1.,-1.91287765805169));
#46288=CARTESIAN_POINT('Ctrl Pts',(-0.765584196937919,-1.,-1.90669961402356));
#46289=CARTESIAN_POINT('Ctrl Pts',(-0.765584196937919,1.,-1.90669961402356));
#46290=CARTESIAN_POINT('Ctrl Pts',(-0.765772772593386,-1.,-1.90052930393596));
#46291=CARTESIAN_POINT('Ctrl Pts',(-0.765772772593386,1.,-1.90052930393596));
#46292=CARTESIAN_POINT('Ctrl Pts',(-0.765913193856978,-1.,-1.89436577771388));
#46293=CARTESIAN_POINT('Ctrl Pts',(-0.765913193856978,1.,-1.89436577771388));
#46294=CARTESIAN_POINT('Ctrl Pts',(-0.766004837062091,-1.,-1.88820926433409));
#46295=CARTESIAN_POINT('Ctrl Pts',(-0.766004837062091,1.,-1.88820926433409));
#46296=CARTESIAN_POINT('Ctrl Pts',(-0.766047794851865,-1.,-1.88206215302561));
#46297=CARTESIAN_POINT('Ctrl Pts',(-0.766047794851865,1.,-1.88206215302561));
#46298=CARTESIAN_POINT('Ctrl Pts',(-0.766042837036744,-1.,-1.87592888967883));
#46299=CARTESIAN_POINT('Ctrl Pts',(-0.766042837036744,1.,-1.87592888967883));
#46300=CARTESIAN_POINT('Ctrl Pts',(-0.765990708546091,-1.,-1.86981398314341));
#46301=CARTESIAN_POINT('Ctrl Pts',(-0.765990708546091,1.,-1.86981398314341));
#46302=CARTESIAN_POINT('Ctrl Pts',(-0.765891519092547,-1.,-1.86372027063312));
#46303=CARTESIAN_POINT('Ctrl Pts',(-0.765891519092547,1.,-1.86372027063312));
#46304=CARTESIAN_POINT('Ctrl Pts',(-0.765744212909318,-1.,-1.85764741390394));
#46305=CARTESIAN_POINT('Ctrl Pts',(-0.765744212909318,1.,-1.85764741390394));
#46306=CARTESIAN_POINT('Ctrl Pts',(-0.765545710619062,-1.,-1.85158945130063));
#46307=CARTESIAN_POINT('Ctrl Pts',(-0.765545710619062,1.,-1.85158945130063));
#46308=CARTESIAN_POINT('Ctrl Pts',(-0.765291664862029,-1.,-1.84553698875924));
#46309=CARTESIAN_POINT('Ctrl Pts',(-0.765291664862029,1.,-1.84553698875924));
#46310=CARTESIAN_POINT('Ctrl Pts',(-0.764978057881737,-1.,-1.83948181064835));
#46311=CARTESIAN_POINT('Ctrl Pts',(-0.764978057881737,1.,-1.83948181064835));
#46312=CARTESIAN_POINT('Ctrl Pts',(-0.764602549687853,-1.,-1.83342077227142));
#46313=CARTESIAN_POINT('Ctrl Pts',(-0.764602549687853,1.,-1.83342077227142));
#46314=CARTESIAN_POINT('Ctrl Pts',(-0.764165902605995,-1.,-1.82735991200065));
#46315=CARTESIAN_POINT('Ctrl Pts',(-0.764165902605995,1.,-1.82735991200065));
#46316=CARTESIAN_POINT('Ctrl Pts',(-0.763673465462726,-1.,-1.82131873145266));
#46317=CARTESIAN_POINT('Ctrl Pts',(-0.763673465462726,1.,-1.82131873145266));
#46318=CARTESIAN_POINT('Ctrl Pts',(-0.763132003836634,-1.,-1.8153211840553));
#46319=CARTESIAN_POINT('Ctrl Pts',(-0.763132003836634,1.,-1.8153211840553));
#46320=CARTESIAN_POINT('Ctrl Pts',(-0.762546129463938,-1.,-1.80938551463965));
#46321=CARTESIAN_POINT('Ctrl Pts',(-0.762546129463938,1.,-1.80938551463965));
#46322=CARTESIAN_POINT('Ctrl Pts',(-0.761915336443547,-1.,-1.80351583877342));
#46323=CARTESIAN_POINT('Ctrl Pts',(-0.761915336443547,1.,-1.80351583877342));
#46324=CARTESIAN_POINT('Ctrl Pts',(-0.761229695230558,-1.,-1.79768986997783));
#46325=CARTESIAN_POINT('Ctrl Pts',(-0.761229695230558,1.,-1.79768986997783));
#46326=CARTESIAN_POINT('Ctrl Pts',(-0.760469555880749,-1.,-1.7918581561088));
#46327=CARTESIAN_POINT('Ctrl Pts',(-0.760469555880749,1.,-1.7918581561088));
#46328=CARTESIAN_POINT('Ctrl Pts',(-0.759614401110189,-1.,-1.78596964884604));
#46329=CARTESIAN_POINT('Ctrl Pts',(-0.759614401110189,1.,-1.78596964884604));
#46330=CARTESIAN_POINT('Ctrl Pts',(-0.758650626677518,-1.,-1.77999411220945));
#46331=CARTESIAN_POINT('Ctrl Pts',(-0.758650626677518,1.,-1.77999411220945));
#46332=CARTESIAN_POINT('Ctrl Pts',(-0.757578264077029,-1.,-1.77394167108292));
#46333=CARTESIAN_POINT('Ctrl Pts',(-0.757578264077029,1.,-1.77394167108292));
#46334=CARTESIAN_POINT('Ctrl Pts',(-0.75642189602781,-1.,-1.76789396002998));
#46335=CARTESIAN_POINT('Ctrl Pts',(-0.75642189602781,1.,-1.76789396002998));
#46336=CARTESIAN_POINT('Ctrl Pts',(-0.755220979974461,-1.,-1.76197817240128));
#46337=CARTESIAN_POINT('Ctrl Pts',(-0.755220979974461,1.,-1.76197817240128));
#46338=CARTESIAN_POINT('Ctrl Pts',(-0.754009254027829,-1.,-1.75631083600019));
#46339=CARTESIAN_POINT('Ctrl Pts',(-0.754009254027829,1.,-1.75631083600019));
#46340=CARTESIAN_POINT('Ctrl Pts',(-0.752797683531314,-1.,-1.75095139468794));
#46341=CARTESIAN_POINT('Ctrl Pts',(-0.752797683531314,1.,-1.75095139468794));
#46342=CARTESIAN_POINT('Ctrl Pts',(-0.751555614164482,-1.,-1.74585086852502));
#46343=CARTESIAN_POINT('Ctrl Pts',(-0.751555614164482,1.,-1.74585086852502));
#46344=CARTESIAN_POINT('Ctrl Pts',(-0.750193435981249,-1.,-1.74080458267114));
#46345=CARTESIAN_POINT('Ctrl Pts',(-0.750193435981249,1.,-1.74080458267114));
#46346=CARTESIAN_POINT('Ctrl Pts',(-0.74858246295687,-1.,-1.7355035168033));
#46347=CARTESIAN_POINT('Ctrl Pts',(-0.74858246295687,1.,-1.7355035168033));
#46348=CARTESIAN_POINT('Ctrl Pts',(-0.746574710097752,-1.,-1.72958533647714));
#46349=CARTESIAN_POINT('Ctrl Pts',(-0.746574710097752,1.,-1.72958533647714));
#46350=CARTESIAN_POINT('Ctrl Pts',(-0.744021445433093,-1.,-1.72268229916769));
#46351=CARTESIAN_POINT('Ctrl Pts',(-0.744021445433093,1.,-1.72268229916769));
#46352=CARTESIAN_POINT('Ctrl Pts',(-0.74079516202821,-1.,-1.71447789751001));
#46353=CARTESIAN_POINT('Ctrl Pts',(-0.74079516202821,1.,-1.71447789751001));
#46354=CARTESIAN_POINT('Ctrl Pts',(-0.736799665716932,-1.,-1.70473309004249));
#46355=CARTESIAN_POINT('Ctrl Pts',(-0.736799665716932,1.,-1.70473309004249));
#46356=CARTESIAN_POINT('Ctrl Pts',(-0.731963238685357,-1.,-1.69326921972915));
#46357=CARTESIAN_POINT('Ctrl Pts',(-0.731963238685357,1.,-1.69326921972915));
#46358=CARTESIAN_POINT('Ctrl Pts',(-0.726235967982445,-1.,-1.67996158451922));
#46359=CARTESIAN_POINT('Ctrl Pts',(-0.726235967982445,1.,-1.67996158451922));
#46360=CARTESIAN_POINT('Ctrl Pts',(-0.71958543378795,-1.,-1.66472880551777));
#46361=CARTESIAN_POINT('Ctrl Pts',(-0.71958543378795,1.,-1.66472880551777));
#46362=CARTESIAN_POINT('Ctrl Pts',(-0.711993139340447,-1.,-1.64752408828442));
#46363=CARTESIAN_POINT('Ctrl Pts',(-0.711993139340447,1.,-1.64752408828442));
#46364=CARTESIAN_POINT('Ctrl Pts',(-0.705159151977294,-1.,-1.6321654166204));
#46365=CARTESIAN_POINT('Ctrl Pts',(-0.705159151977294,1.,-1.6321654166204));
#46366=CARTESIAN_POINT('Ctrl Pts',(-0.699605146398837,-1.,-1.61974673471117));
#46367=CARTESIAN_POINT('Ctrl Pts',(-0.699605146398837,1.,-1.61974673471117));
#46368=CARTESIAN_POINT('Ctrl Pts',(-0.69571209787897,-1.,-1.61106790957619));
#46369=CARTESIAN_POINT('Ctrl Pts',(-0.69571209787897,1.,-1.61106790957619));
#46370=CARTESIAN_POINT('Ctrl Pts',(-0.693717979106305,-1.,-1.60662857109684));
#46371=CARTESIAN_POINT('Ctrl Pts',(-0.693717979106305,1.,-1.60662857109684));
#46372=CARTESIAN_POINT('',(-0.745574324794401,1.,-2.0698113262342));
#46373=CARTESIAN_POINT('Ctrl Pts',(-0.745574324794401,1.,-2.0698113262342));
#46374=CARTESIAN_POINT('Ctrl Pts',(-0.745832791378367,1.,-2.06854248895728));
#46375=CARTESIAN_POINT('Ctrl Pts',(-0.7463458715442,1.,-2.06600523016815));
#46376=CARTESIAN_POINT('Ctrl Pts',(-0.747103932787919,1.,-2.06220058927826));
#46377=CARTESIAN_POINT('Ctrl Pts',(-0.748091554183802,1.,-2.05713023031006));
#46378=CARTESIAN_POINT('Ctrl Pts',(-0.749287468665046,1.,-2.05079645592154));
#46379=CARTESIAN_POINT('Ctrl Pts',(-0.750444657875576,1.,-2.04446689147979));
#46380=CARTESIAN_POINT('Ctrl Pts',(-0.751562963361115,1.,-2.03814160092099));
#46381=CARTESIAN_POINT('Ctrl Pts',(-0.752642180487211,1.,-2.03182068456221));
#46382=CARTESIAN_POINT('Ctrl Pts',(-0.753682061112768,1.,-2.02550428623313));
#46383=CARTESIAN_POINT('Ctrl Pts',(-0.754682330722816,1.,-2.01919259405809));
#46384=CARTESIAN_POINT('Ctrl Pts',(-0.755642704957865,1.,-2.01288584328084));
#46385=CARTESIAN_POINT('Ctrl Pts',(-0.75656290464667,1.,-2.0065843158773));
#46386=CARTESIAN_POINT('Ctrl Pts',(-0.757442676862724,1.,-2.00028834739178));
#46387=CARTESIAN_POINT('Ctrl Pts',(-0.758281796766761,1.,-1.99399831098817));
#46388=CARTESIAN_POINT('Ctrl Pts',(-0.759080037802488,1.,-1.98771456680874));
#46389=CARTESIAN_POINT('Ctrl Pts',(-0.75983714745219,1.,-1.98143741418172));
#46390=CARTESIAN_POINT('Ctrl Pts',(-0.760552825409757,1.,-1.97516705321494));
#46391=CARTESIAN_POINT('Ctrl Pts',(-0.76122669048382,1.,-1.96890351582499));
#46392=CARTESIAN_POINT('Ctrl Pts',(-0.761858300014423,1.,-1.96264672744186));
#46393=CARTESIAN_POINT('Ctrl Pts',(-0.762447203806179,1.,-1.95639665309869));
#46394=CARTESIAN_POINT('Ctrl Pts',(-0.762992990878769,1.,-1.95015342590024));
#46395=CARTESIAN_POINT('Ctrl Pts',(-0.763495333538629,1.,-1.9439174661764));
#46396=CARTESIAN_POINT('Ctrl Pts',(-0.763954049121458,1.,-1.93768964875886));
#46397=CARTESIAN_POINT('Ctrl Pts',(-0.764369010673941,1.,-1.93147105496382));
#46398=CARTESIAN_POINT('Ctrl Pts',(-0.764740025488211,1.,-1.92526263537048));
#46399=CARTESIAN_POINT('Ctrl Pts',(-0.765066729667088,1.,-1.91906491634196));
#46400=CARTESIAN_POINT('Ctrl Pts',(-0.765348465884722,1.,-1.91287765805169));
#46401=CARTESIAN_POINT('Ctrl Pts',(-0.765584196937919,1.,-1.90669961402356));
#46402=CARTESIAN_POINT('Ctrl Pts',(-0.765772772593386,1.,-1.90052930393596));
#46403=CARTESIAN_POINT('Ctrl Pts',(-0.765913193856978,1.,-1.89436577771388));
#46404=CARTESIAN_POINT('Ctrl Pts',(-0.766004837062091,1.,-1.88820926433409));
#46405=CARTESIAN_POINT('Ctrl Pts',(-0.766047794851865,1.,-1.88206215302561));
#46406=CARTESIAN_POINT('Ctrl Pts',(-0.766042837036744,1.,-1.87592888967883));
#46407=CARTESIAN_POINT('Ctrl Pts',(-0.765990708546091,1.,-1.86981398314341));
#46408=CARTESIAN_POINT('Ctrl Pts',(-0.765891519092547,1.,-1.86372027063312));
#46409=CARTESIAN_POINT('Ctrl Pts',(-0.765744212909318,1.,-1.85764741390394));
#46410=CARTESIAN_POINT('Ctrl Pts',(-0.765545710619062,1.,-1.85158945130063));
#46411=CARTESIAN_POINT('Ctrl Pts',(-0.765291664862029,1.,-1.84553698875924));
#46412=CARTESIAN_POINT('Ctrl Pts',(-0.764978057881737,1.,-1.83948181064835));
#46413=CARTESIAN_POINT('Ctrl Pts',(-0.764602549687853,1.,-1.83342077227142));
#46414=CARTESIAN_POINT('Ctrl Pts',(-0.764165902605995,1.,-1.82735991200065));
#46415=CARTESIAN_POINT('Ctrl Pts',(-0.763673465462726,1.,-1.82131873145266));
#46416=CARTESIAN_POINT('Ctrl Pts',(-0.763132003836634,1.,-1.8153211840553));
#46417=CARTESIAN_POINT('Ctrl Pts',(-0.762546129463938,1.,-1.80938551463965));
#46418=CARTESIAN_POINT('Ctrl Pts',(-0.761915336443547,1.,-1.80351583877342));
#46419=CARTESIAN_POINT('Ctrl Pts',(-0.761229695230558,1.,-1.79768986997783));
#46420=CARTESIAN_POINT('Ctrl Pts',(-0.760469555880749,1.,-1.7918581561088));
#46421=CARTESIAN_POINT('Ctrl Pts',(-0.759614401110189,1.,-1.78596964884604));
#46422=CARTESIAN_POINT('Ctrl Pts',(-0.758650626677518,1.,-1.77999411220945));
#46423=CARTESIAN_POINT('Ctrl Pts',(-0.757578264077029,1.,-1.77394167108292));
#46424=CARTESIAN_POINT('Ctrl Pts',(-0.75642189602781,1.,-1.76789396002998));
#46425=CARTESIAN_POINT('Ctrl Pts',(-0.755220979974461,1.,-1.76197817240128));
#46426=CARTESIAN_POINT('Ctrl Pts',(-0.754009254027829,1.,-1.75631083600019));
#46427=CARTESIAN_POINT('Ctrl Pts',(-0.752797683531314,1.,-1.75095139468794));
#46428=CARTESIAN_POINT('Ctrl Pts',(-0.751555614164482,1.,-1.74585086852502));
#46429=CARTESIAN_POINT('Ctrl Pts',(-0.750193435981249,1.,-1.74080458267114));
#46430=CARTESIAN_POINT('Ctrl Pts',(-0.74858246295687,1.,-1.7355035168033));
#46431=CARTESIAN_POINT('Ctrl Pts',(-0.746574710097752,1.,-1.72958533647714));
#46432=CARTESIAN_POINT('Ctrl Pts',(-0.744021445433093,1.,-1.72268229916769));
#46433=CARTESIAN_POINT('Ctrl Pts',(-0.74079516202821,1.,-1.71447789751001));
#46434=CARTESIAN_POINT('Ctrl Pts',(-0.736799665716932,1.,-1.70473309004249));
#46435=CARTESIAN_POINT('Ctrl Pts',(-0.731963238685357,1.,-1.69326921972915));
#46436=CARTESIAN_POINT('Ctrl Pts',(-0.726235967982445,1.,-1.67996158451922));
#46437=CARTESIAN_POINT('Ctrl Pts',(-0.71958543378795,1.,-1.66472880551777));
#46438=CARTESIAN_POINT('Ctrl Pts',(-0.711993139340447,1.,-1.64752408828442));
#46439=CARTESIAN_POINT('Ctrl Pts',(-0.705159151977294,1.,-1.6321654166204));
#46440=CARTESIAN_POINT('Ctrl Pts',(-0.699605146398837,1.,-1.61974673471117));
#46441=CARTESIAN_POINT('Ctrl Pts',(-0.69571209787897,1.,-1.61106790957619));
#46442=CARTESIAN_POINT('Ctrl Pts',(-0.693717979106305,1.,-1.60662857109684));
#46443=CARTESIAN_POINT('',(-0.745574324794401,0.,-2.0698113262342));
#46444=CARTESIAN_POINT('Origin',(-0.61342227326009,0.,-2.11275013067528));
#46445=CARTESIAN_POINT('',(-0.61342227326009,1.,-2.11275013067528));
#46446=CARTESIAN_POINT('',(-0.745574324794401,1.,-2.0698113262342));
#46447=CARTESIAN_POINT('',(-0.61342227326009,0.,-2.11275013067528));
#46448=CARTESIAN_POINT('Ctrl Pts',(-0.383122945602004,-1.,-1.7075470150345));
#46449=CARTESIAN_POINT('Ctrl Pts',(-0.383122945602004,1.,-1.7075470150345));
#46450=CARTESIAN_POINT('Ctrl Pts',(-0.384119047315542,-1.,-1.71231062891958));
#46451=CARTESIAN_POINT('Ctrl Pts',(-0.384119047315542,1.,-1.71231062891958));
#46452=CARTESIAN_POINT('Ctrl Pts',(-0.38607079032701,-1.,-1.72162022246158));
#46453=CARTESIAN_POINT('Ctrl Pts',(-0.38607079032701,1.,-1.72162022246158));
#46454=CARTESIAN_POINT('Ctrl Pts',(-0.388877023509191,-1.,-1.7349317097561));
#46455=CARTESIAN_POINT('Ctrl Pts',(-0.388877023509191,1.,-1.7349317097561));
#46456=CARTESIAN_POINT('Ctrl Pts',(-0.392375812294307,-1.,-1.75137405313962));
#46457=CARTESIAN_POINT('Ctrl Pts',(-0.392375812294307,1.,-1.75137405313962));
#46458=CARTESIAN_POINT('Ctrl Pts',(-0.39634619612042,-1.,-1.7697556004756));
#46459=CARTESIAN_POINT('Ctrl Pts',(-0.39634619612042,1.,-1.7697556004756));
#46460=CARTESIAN_POINT('Ctrl Pts',(-0.39991940378308,-1.,-1.78598826347533));
#46461=CARTESIAN_POINT('Ctrl Pts',(-0.39991940378308,1.,-1.78598826347533));
#46462=CARTESIAN_POINT('Ctrl Pts',(-0.403107976170441,-1.,-1.80012077176221));
#46463=CARTESIAN_POINT('Ctrl Pts',(-0.403107976170441,1.,-1.80012077176221));
#46464=CARTESIAN_POINT('Ctrl Pts',(-0.405933518411838,-1.,-1.81223801813988));
#46465=CARTESIAN_POINT('Ctrl Pts',(-0.405933518411838,1.,-1.81223801813988));
#46466=CARTESIAN_POINT('Ctrl Pts',(-0.408428948108533,-1.,-1.8224702267854));
#46467=CARTESIAN_POINT('Ctrl Pts',(-0.408428948108533,1.,-1.8224702267854));
#46468=CARTESIAN_POINT('Ctrl Pts',(-0.410641256301675,-1.,-1.83100408895216));
#46469=CARTESIAN_POINT('Ctrl Pts',(-0.410641256301675,1.,-1.83100408895216));
#46470=CARTESIAN_POINT('Ctrl Pts',(-0.412633125322162,-1.,-1.83808953475839));
#46471=CARTESIAN_POINT('Ctrl Pts',(-0.412633125322162,1.,-1.83808953475839));
#46472=CARTESIAN_POINT('Ctrl Pts',(-0.41448743825434,-1.,-1.8440575707371));
#46473=CARTESIAN_POINT('Ctrl Pts',(-0.41448743825434,1.,-1.8440575707371));
#46474=CARTESIAN_POINT('Ctrl Pts',(-0.416300022038864,-1.,-1.84929312929882));
#46475=CARTESIAN_POINT('Ctrl Pts',(-0.416300022038864,1.,-1.84929312929882));
#46476=CARTESIAN_POINT('Ctrl Pts',(-0.418164129143534,-1.,-1.85417632856234));
#46477=CARTESIAN_POINT('Ctrl Pts',(-0.418164129143534,1.,-1.85417632856234));
#46478=CARTESIAN_POINT('Ctrl Pts',(-0.420157287975619,-1.,-1.85903281096686));
#46479=CARTESIAN_POINT('Ctrl Pts',(-0.420157287975619,1.,-1.85903281096686));
#46480=CARTESIAN_POINT('Ctrl Pts',(-0.422327307418275,-1.,-1.86408083334028));
#46481=CARTESIAN_POINT('Ctrl Pts',(-0.422327307418275,1.,-1.86408083334028));
#46482=CARTESIAN_POINT('Ctrl Pts',(-0.424678177291359,-1.,-1.86937803944323));
#46483=CARTESIAN_POINT('Ctrl Pts',(-0.424678177291359,1.,-1.86937803944323));
#46484=CARTESIAN_POINT('Ctrl Pts',(-0.427183828519102,-1.,-1.87486989291484));
#46485=CARTESIAN_POINT('Ctrl Pts',(-0.427183828519102,1.,-1.87486989291484));
#46486=CARTESIAN_POINT('Ctrl Pts',(-0.429803062482344,-1.,-1.88044229001832));
#46487=CARTESIAN_POINT('Ctrl Pts',(-0.429803062482344,1.,-1.88044229001832));
#46488=CARTESIAN_POINT('Ctrl Pts',(-0.432493038548748,-1.,-1.88596913666793));
#46489=CARTESIAN_POINT('Ctrl Pts',(-0.432493038548748,1.,-1.88596913666793));
#46490=CARTESIAN_POINT('Ctrl Pts',(-0.435225660963383,-1.,-1.89136993975504));
#46491=CARTESIAN_POINT('Ctrl Pts',(-0.435225660963383,1.,-1.89136993975504));
#46492=CARTESIAN_POINT('Ctrl Pts',(-0.437995003948244,-1.,-1.89663648956466));
#46493=CARTESIAN_POINT('Ctrl Pts',(-0.437995003948244,1.,-1.89663648956466));
#46494=CARTESIAN_POINT('Ctrl Pts',(-0.440807833704038,-1.,-1.90180124389086));
#46495=CARTESIAN_POINT('Ctrl Pts',(-0.440807833704038,1.,-1.90180124389086));
#46496=CARTESIAN_POINT('Ctrl Pts',(-0.443677556849151,-1.,-1.90691756144898));
#46497=CARTESIAN_POINT('Ctrl Pts',(-0.443677556849151,1.,-1.90691756144898));
#46498=CARTESIAN_POINT('Ctrl Pts',(-0.446617343485711,-1.,-1.9120369998112));
#46499=CARTESIAN_POINT('Ctrl Pts',(-0.446617343485711,1.,-1.9120369998112));
#46500=CARTESIAN_POINT('Ctrl Pts',(-0.449632260106662,-1.,-1.91718342555755));
#46501=CARTESIAN_POINT('Ctrl Pts',(-0.449632260106662,1.,-1.91718342555755));
#46502=CARTESIAN_POINT('Ctrl Pts',(-0.452719478359432,-1.,-1.92235380648502));
#46503=CARTESIAN_POINT('Ctrl Pts',(-0.452719478359432,1.,-1.92235380648502));
#46504=CARTESIAN_POINT('Ctrl Pts',(-0.455872005174371,-1.,-1.92753067150476));
#46505=CARTESIAN_POINT('Ctrl Pts',(-0.455872005174371,1.,-1.92753067150476));
#46506=CARTESIAN_POINT('Ctrl Pts',(-0.459081234547926,-1.,-1.93269066517934));
#46507=CARTESIAN_POINT('Ctrl Pts',(-0.459081234547926,1.,-1.93269066517934));
#46508=CARTESIAN_POINT('Ctrl Pts',(-0.462340031009056,-1.,-1.93781486640821));
#46509=CARTESIAN_POINT('Ctrl Pts',(-0.462340031009056,1.,-1.93781486640821));
#46510=CARTESIAN_POINT('Ctrl Pts',(-0.46564546202603,-1.,-1.9428979419619));
#46511=CARTESIAN_POINT('Ctrl Pts',(-0.46564546202603,1.,-1.9428979419619));
#46512=CARTESIAN_POINT('Ctrl Pts',(-0.468997482913135,-1.,-1.94794381136514));
#46513=CARTESIAN_POINT('Ctrl Pts',(-0.468997482913135,1.,-1.94794381136514));
#46514=CARTESIAN_POINT('Ctrl Pts',(-0.472397672264072,-1.,-1.95296148278133));
#46515=CARTESIAN_POINT('Ctrl Pts',(-0.472397672264072,1.,-1.95296148278133));
#46516=CARTESIAN_POINT('Ctrl Pts',(-0.475848034683176,-1.,-1.95796111148177));
#46517=CARTESIAN_POINT('Ctrl Pts',(-0.475848034683176,1.,-1.95796111148177));
#46518=CARTESIAN_POINT('Ctrl Pts',(-0.479349583074855,-1.,-1.96294933055943));
#46519=CARTESIAN_POINT('Ctrl Pts',(-0.479349583074855,1.,-1.96294933055943));
#46520=CARTESIAN_POINT('Ctrl Pts',(-0.482901662120691,-1.,-1.96792703422362));
#46521=CARTESIAN_POINT('Ctrl Pts',(-0.482901662120691,1.,-1.96792703422362));
#46522=CARTESIAN_POINT('Ctrl Pts',(-0.486502692907659,-1.,-1.97289186263272));
#46523=CARTESIAN_POINT('Ctrl Pts',(-0.486502692907659,1.,-1.97289186263272));
#46524=CARTESIAN_POINT('Ctrl Pts',(-0.490150627860952,-1.,-1.97783973019229));
#46525=CARTESIAN_POINT('Ctrl Pts',(-0.490150627860952,1.,-1.97783973019229));
#46526=CARTESIAN_POINT('Ctrl Pts',(-0.493843476541495,-1.,-1.98276658761821));
#46527=CARTESIAN_POINT('Ctrl Pts',(-0.493843476541495,1.,-1.98276658761821));
#46528=CARTESIAN_POINT('Ctrl Pts',(-0.497579909545574,-1.,-1.98767044752932));
#46529=CARTESIAN_POINT('Ctrl Pts',(-0.497579909545574,1.,-1.98767044752932));
#46530=CARTESIAN_POINT('Ctrl Pts',(-0.501359287727146,-1.,-1.99255149126155));
#46531=CARTESIAN_POINT('Ctrl Pts',(-0.501359287727146,1.,-1.99255149126155));
#46532=CARTESIAN_POINT('Ctrl Pts',(-0.505181361323026,-1.,-1.99741107463572));
#46533=CARTESIAN_POINT('Ctrl Pts',(-0.505181361323026,1.,-1.99741107463572));
#46534=CARTESIAN_POINT('Ctrl Pts',(-0.509046069886157,-1.,-2.00225107134734));
#46535=CARTESIAN_POINT('Ctrl Pts',(-0.509046069886157,1.,-2.00225107134734));
#46536=CARTESIAN_POINT('Ctrl Pts',(-0.512953306961792,-1.,-2.00707309946949));
#46537=CARTESIAN_POINT('Ctrl Pts',(-0.512953306961792,1.,-2.00707309946949));
#46538=CARTESIAN_POINT('Ctrl Pts',(-0.516902681728687,-1.,-2.01187773939242));
#46539=CARTESIAN_POINT('Ctrl Pts',(-0.516902681728687,1.,-2.01187773939242));
#46540=CARTESIAN_POINT('Ctrl Pts',(-0.52089359039937,-1.,-2.01666477917286));
#46541=CARTESIAN_POINT('Ctrl Pts',(-0.52089359039937,1.,-2.01666477917286));
#46542=CARTESIAN_POINT('Ctrl Pts',(-0.524925318333476,-1.,-2.02143356304698));
#46543=CARTESIAN_POINT('Ctrl Pts',(-0.524925318333476,1.,-2.02143356304698));
#46544=CARTESIAN_POINT('Ctrl Pts',(-0.528997127241914,-1.,-2.0261832908329));
#46545=CARTESIAN_POINT('Ctrl Pts',(-0.528997127241914,1.,-2.0261832908329));
#46546=CARTESIAN_POINT('Ctrl Pts',(-0.533108355132977,-1.,-2.03091336214426));
#46547=CARTESIAN_POINT('Ctrl Pts',(-0.533108355132977,1.,-2.03091336214426));
#46548=CARTESIAN_POINT('Ctrl Pts',(-0.537258489833262,-1.,-2.03562362954037));
#46549=CARTESIAN_POINT('Ctrl Pts',(-0.537258489833262,1.,-2.03562362954037));
#46550=CARTESIAN_POINT('Ctrl Pts',(-0.541447120615659,-1.,-2.04031422690527));
#46551=CARTESIAN_POINT('Ctrl Pts',(-0.541447120615659,1.,-2.04031422690527));
#46552=CARTESIAN_POINT('Ctrl Pts',(-0.54567390381743,-1.,-2.04498544714588));
#46553=CARTESIAN_POINT('Ctrl Pts',(-0.54567390381743,1.,-2.04498544714588));
#46554=CARTESIAN_POINT('Ctrl Pts',(-0.549938525150295,-1.,-2.04963761077958));
#46555=CARTESIAN_POINT('Ctrl Pts',(-0.549938525150295,1.,-2.04963761077958));
#46556=CARTESIAN_POINT('Ctrl Pts',(-0.554240657463906,-1.,-2.05427091604413));
#46557=CARTESIAN_POINT('Ctrl Pts',(-0.554240657463906,1.,-2.05427091604413));
#46558=CARTESIAN_POINT('Ctrl Pts',(-0.558579940185151,-1.,-2.05888537756462));
#46559=CARTESIAN_POINT('Ctrl Pts',(-0.558579940185151,1.,-2.05888537756462));
#46560=CARTESIAN_POINT('Ctrl Pts',(-0.562955993082261,-1.,-2.06348090160589));
#46561=CARTESIAN_POINT('Ctrl Pts',(-0.562955993082261,1.,-2.06348090160589));
#46562=CARTESIAN_POINT('Ctrl Pts',(-0.567368421181087,-1.,-2.06805732997334));
#46563=CARTESIAN_POINT('Ctrl Pts',(-0.567368421181087,1.,-2.06805732997334));
#46564=CARTESIAN_POINT('Ctrl Pts',(-0.571816823242603,-1.,-2.07261449292824));
#46565=CARTESIAN_POINT('Ctrl Pts',(-0.571816823242603,1.,-2.07261449292824));
#46566=CARTESIAN_POINT('Ctrl Pts',(-0.576300797416844,-1.,-2.07715226767559));
#46567=CARTESIAN_POINT('Ctrl Pts',(-0.576300797416844,1.,-2.07715226767559));
#46568=CARTESIAN_POINT('Ctrl Pts',(-0.580819952108063,-1.,-2.08167059018418));
#46569=CARTESIAN_POINT('Ctrl Pts',(-0.580819952108063,1.,-2.08167059018418));
#46570=CARTESIAN_POINT('Ctrl Pts',(-0.585373918991617,-1.,-2.08616943727951));
#46571=CARTESIAN_POINT('Ctrl Pts',(-0.585373918991617,1.,-2.08616943727951));
#46572=CARTESIAN_POINT('Ctrl Pts',(-0.589962365403406,-1.,-2.09064881812129));
#46573=CARTESIAN_POINT('Ctrl Pts',(-0.589962365403406,1.,-2.09064881812129));
#46574=CARTESIAN_POINT('Ctrl Pts',(-0.594585006052162,-1.,-2.0951087622027));
#46575=CARTESIAN_POINT('Ctrl Pts',(-0.594585006052162,1.,-2.0951087622027));
#46576=CARTESIAN_POINT('Ctrl Pts',(-0.599241616420533,-1.,-2.0995493086477));
#46577=CARTESIAN_POINT('Ctrl Pts',(-0.599241616420533,1.,-2.0995493086477));
#46578=CARTESIAN_POINT('Ctrl Pts',(-0.60393203073603,-1.,-2.10397049886949));
#46579=CARTESIAN_POINT('Ctrl Pts',(-0.60393203073603,1.,-2.10397049886949));
#46580=CARTESIAN_POINT('Ctrl Pts',(-0.607711315454876,-1.,-2.1074919961518));
#46581=CARTESIAN_POINT('Ctrl Pts',(-0.607711315454876,1.,-2.1074919961518));
#46582=CARTESIAN_POINT('Ctrl Pts',(-0.610560911689899,-1.,-2.11012443807238));
#46583=CARTESIAN_POINT('Ctrl Pts',(-0.610560911689899,1.,-2.11012443807238));
#46584=CARTESIAN_POINT('Ctrl Pts',(-0.6124673655618,-1.,-2.11187554259986));
#46585=CARTESIAN_POINT('Ctrl Pts',(-0.6124673655618,1.,-2.11187554259986));
#46586=CARTESIAN_POINT('Ctrl Pts',(-0.61342227326009,-1.,-2.11275013067528));
#46587=CARTESIAN_POINT('Ctrl Pts',(-0.61342227326009,1.,-2.11275013067528));
#46588=CARTESIAN_POINT('',(-0.383122945602004,1.,-1.7075470150345));
#46589=CARTESIAN_POINT('Ctrl Pts',(-0.383122945602004,1.,-1.7075470150345));
#46590=CARTESIAN_POINT('Ctrl Pts',(-0.384119047315542,1.,-1.71231062891958));
#46591=CARTESIAN_POINT('Ctrl Pts',(-0.38607079032701,1.,-1.72162022246158));
#46592=CARTESIAN_POINT('Ctrl Pts',(-0.388877023509191,1.,-1.7349317097561));
#46593=CARTESIAN_POINT('Ctrl Pts',(-0.392375812294307,1.,-1.75137405313962));
#46594=CARTESIAN_POINT('Ctrl Pts',(-0.39634619612042,1.,-1.7697556004756));
#46595=CARTESIAN_POINT('Ctrl Pts',(-0.39991940378308,1.,-1.78598826347533));
#46596=CARTESIAN_POINT('Ctrl Pts',(-0.403107976170441,1.,-1.80012077176221));
#46597=CARTESIAN_POINT('Ctrl Pts',(-0.405933518411838,1.,-1.81223801813988));
#46598=CARTESIAN_POINT('Ctrl Pts',(-0.408428948108533,1.,-1.8224702267854));
#46599=CARTESIAN_POINT('Ctrl Pts',(-0.410641256301675,1.,-1.83100408895216));
#46600=CARTESIAN_POINT('Ctrl Pts',(-0.412633125322162,1.,-1.83808953475839));
#46601=CARTESIAN_POINT('Ctrl Pts',(-0.41448743825434,1.,-1.8440575707371));
#46602=CARTESIAN_POINT('Ctrl Pts',(-0.416300022038864,1.,-1.84929312929882));
#46603=CARTESIAN_POINT('Ctrl Pts',(-0.418164129143534,1.,-1.85417632856234));
#46604=CARTESIAN_POINT('Ctrl Pts',(-0.420157287975619,1.,-1.85903281096686));
#46605=CARTESIAN_POINT('Ctrl Pts',(-0.422327307418275,1.,-1.86408083334028));
#46606=CARTESIAN_POINT('Ctrl Pts',(-0.424678177291359,1.,-1.86937803944323));
#46607=CARTESIAN_POINT('Ctrl Pts',(-0.427183828519102,1.,-1.87486989291484));
#46608=CARTESIAN_POINT('Ctrl Pts',(-0.429803062482344,1.,-1.88044229001832));
#46609=CARTESIAN_POINT('Ctrl Pts',(-0.432493038548748,1.,-1.88596913666793));
#46610=CARTESIAN_POINT('Ctrl Pts',(-0.435225660963383,1.,-1.89136993975504));
#46611=CARTESIAN_POINT('Ctrl Pts',(-0.437995003948244,1.,-1.89663648956466));
#46612=CARTESIAN_POINT('Ctrl Pts',(-0.440807833704038,1.,-1.90180124389086));
#46613=CARTESIAN_POINT('Ctrl Pts',(-0.443677556849151,1.,-1.90691756144898));
#46614=CARTESIAN_POINT('Ctrl Pts',(-0.446617343485711,1.,-1.9120369998112));
#46615=CARTESIAN_POINT('Ctrl Pts',(-0.449632260106662,1.,-1.91718342555755));
#46616=CARTESIAN_POINT('Ctrl Pts',(-0.452719478359432,1.,-1.92235380648502));
#46617=CARTESIAN_POINT('Ctrl Pts',(-0.455872005174371,1.,-1.92753067150476));
#46618=CARTESIAN_POINT('Ctrl Pts',(-0.459081234547926,1.,-1.93269066517934));
#46619=CARTESIAN_POINT('Ctrl Pts',(-0.462340031009056,1.,-1.93781486640821));
#46620=CARTESIAN_POINT('Ctrl Pts',(-0.46564546202603,1.,-1.9428979419619));
#46621=CARTESIAN_POINT('Ctrl Pts',(-0.468997482913135,1.,-1.94794381136514));
#46622=CARTESIAN_POINT('Ctrl Pts',(-0.472397672264072,1.,-1.95296148278133));
#46623=CARTESIAN_POINT('Ctrl Pts',(-0.475848034683176,1.,-1.95796111148177));
#46624=CARTESIAN_POINT('Ctrl Pts',(-0.479349583074855,1.,-1.96294933055943));
#46625=CARTESIAN_POINT('Ctrl Pts',(-0.482901662120691,1.,-1.96792703422362));
#46626=CARTESIAN_POINT('Ctrl Pts',(-0.486502692907659,1.,-1.97289186263272));
#46627=CARTESIAN_POINT('Ctrl Pts',(-0.490150627860952,1.,-1.97783973019229));
#46628=CARTESIAN_POINT('Ctrl Pts',(-0.493843476541495,1.,-1.98276658761821));
#46629=CARTESIAN_POINT('Ctrl Pts',(-0.497579909545574,1.,-1.98767044752932));
#46630=CARTESIAN_POINT('Ctrl Pts',(-0.501359287727146,1.,-1.99255149126155));
#46631=CARTESIAN_POINT('Ctrl Pts',(-0.505181361323026,1.,-1.99741107463572));
#46632=CARTESIAN_POINT('Ctrl Pts',(-0.509046069886157,1.,-2.00225107134734));
#46633=CARTESIAN_POINT('Ctrl Pts',(-0.512953306961792,1.,-2.00707309946949));
#46634=CARTESIAN_POINT('Ctrl Pts',(-0.516902681728687,1.,-2.01187773939242));
#46635=CARTESIAN_POINT('Ctrl Pts',(-0.52089359039937,1.,-2.01666477917286));
#46636=CARTESIAN_POINT('Ctrl Pts',(-0.524925318333476,1.,-2.02143356304698));
#46637=CARTESIAN_POINT('Ctrl Pts',(-0.528997127241914,1.,-2.0261832908329));
#46638=CARTESIAN_POINT('Ctrl Pts',(-0.533108355132977,1.,-2.03091336214426));
#46639=CARTESIAN_POINT('Ctrl Pts',(-0.537258489833262,1.,-2.03562362954037));
#46640=CARTESIAN_POINT('Ctrl Pts',(-0.541447120615659,1.,-2.04031422690527));
#46641=CARTESIAN_POINT('Ctrl Pts',(-0.54567390381743,1.,-2.04498544714588));
#46642=CARTESIAN_POINT('Ctrl Pts',(-0.549938525150295,1.,-2.04963761077958));
#46643=CARTESIAN_POINT('Ctrl Pts',(-0.554240657463906,1.,-2.05427091604413));
#46644=CARTESIAN_POINT('Ctrl Pts',(-0.558579940185151,1.,-2.05888537756462));
#46645=CARTESIAN_POINT('Ctrl Pts',(-0.562955993082261,1.,-2.06348090160589));
#46646=CARTESIAN_POINT('Ctrl Pts',(-0.567368421181087,1.,-2.06805732997334));
#46647=CARTESIAN_POINT('Ctrl Pts',(-0.571816823242603,1.,-2.07261449292824));
#46648=CARTESIAN_POINT('Ctrl Pts',(-0.576300797416844,1.,-2.07715226767559));
#46649=CARTESIAN_POINT('Ctrl Pts',(-0.580819952108063,1.,-2.08167059018418));
#46650=CARTESIAN_POINT('Ctrl Pts',(-0.585373918991617,1.,-2.08616943727951));
#46651=CARTESIAN_POINT('Ctrl Pts',(-0.589962365403406,1.,-2.09064881812129));
#46652=CARTESIAN_POINT('Ctrl Pts',(-0.594585006052162,1.,-2.0951087622027));
#46653=CARTESIAN_POINT('Ctrl Pts',(-0.599241616420533,1.,-2.0995493086477));
#46654=CARTESIAN_POINT('Ctrl Pts',(-0.60393203073603,1.,-2.10397049886949));
#46655=CARTESIAN_POINT('Ctrl Pts',(-0.607711315454876,1.,-2.1074919961518));
#46656=CARTESIAN_POINT('Ctrl Pts',(-0.610560911689899,1.,-2.11012443807238));
#46657=CARTESIAN_POINT('Ctrl Pts',(-0.6124673655618,1.,-2.11187554259986));
#46658=CARTESIAN_POINT('Ctrl Pts',(-0.61342227326009,1.,-2.11275013067528));
#46659=CARTESIAN_POINT('',(-0.383122945602003,0.,-1.7075470150345));
#46660=CARTESIAN_POINT('Origin',(0.,0.,0.));
#46661=CARTESIAN_POINT('',(-0.163289472382896,1.,-1.74236521665491));
#46662=CARTESIAN_POINT('Origin',(0.,1.,0.));
#46663=CARTESIAN_POINT('',(-0.163289472382896,0.,-1.74236521665491));
#46664=CARTESIAN_POINT('Ctrl Pts',(-0.0694764450219581,-1.,-2.19890268624765));
#46665=CARTESIAN_POINT('Ctrl Pts',(-0.0694764450219581,1.,-2.19890268624765));
#46666=CARTESIAN_POINT('Ctrl Pts',(-0.070114353632549,-1.,-2.19777582085423));
#46667=CARTESIAN_POINT('Ctrl Pts',(-0.070114353632549,1.,-2.19777582085423));
#46668=CARTESIAN_POINT('Ctrl Pts',(-0.0713863779526154,-1.,-2.19552129484002));
#46669=CARTESIAN_POINT('Ctrl Pts',(-0.0713863779526154,1.,-2.19552129484002));
#46670=CARTESIAN_POINT('Ctrl Pts',(-0.0732830357306725,-1.,-2.19213712013662));
#46671=CARTESIAN_POINT('Ctrl Pts',(-0.0732830357306725,1.,-2.19213712013662));
#46672=CARTESIAN_POINT('Ctrl Pts',(-0.0757891465836148,-1.,-2.1876201139953));
#46673=CARTESIAN_POINT('Ctrl Pts',(-0.0757891465836148,1.,-2.1876201139953));
#46674=CARTESIAN_POINT('Ctrl Pts',(-0.0788837727685243,-1.,-2.18196589448887));
#46675=CARTESIAN_POINT('Ctrl Pts',(-0.0788837727685243,1.,-2.18196589448887));
#46676=CARTESIAN_POINT('Ctrl Pts',(-0.0819402680872765,-1.,-2.176303712113));
#46677=CARTESIAN_POINT('Ctrl Pts',(-0.0819402680872765,1.,-2.176303712113));
#46678=CARTESIAN_POINT('Ctrl Pts',(-0.0849584620835372,-1.,-2.17063357870952));
#46679=CARTESIAN_POINT('Ctrl Pts',(-0.0849584620835372,1.,-2.17063357870952));
#46680=CARTESIAN_POINT('Ctrl Pts',(-0.0879381291386923,-1.,-2.16495552645014));
#46681=CARTESIAN_POINT('Ctrl Pts',(-0.0879381291386923,1.,-2.16495552645014));
#46682=CARTESIAN_POINT('Ctrl Pts',(-0.0908789888107265,-1.,-2.15926961544516));
#46683=CARTESIAN_POINT('Ctrl Pts',(-0.0908789888107265,1.,-2.15926961544516));
#46684=CARTESIAN_POINT('Ctrl Pts',(-0.0937807218867643,-1.,-2.1535759397817));
#46685=CARTESIAN_POINT('Ctrl Pts',(-0.0937807218867643,1.,-2.1535759397817));
#46686=CARTESIAN_POINT('Ctrl Pts',(-0.0966429852305459,-1.,-2.14787463531795));
#46687=CARTESIAN_POINT('Ctrl Pts',(-0.0966429852305459,1.,-2.14787463531795));
#46688=CARTESIAN_POINT('Ctrl Pts',(-0.0994654261990915,-1.,-2.14216588396025));
#46689=CARTESIAN_POINT('Ctrl Pts',(-0.0994654261990915,1.,-2.14216588396025));
#46690=CARTESIAN_POINT('Ctrl Pts',(-0.1022477005561,-1.,-2.13644992667165));
#46691=CARTESIAN_POINT('Ctrl Pts',(-0.1022477005561,1.,-2.13644992667165));
#46692=CARTESIAN_POINT('Ctrl Pts',(-0.104989479152739,-1.,-2.13072704887293));
#46693=CARTESIAN_POINT('Ctrl Pts',(-0.104989479152739,1.,-2.13072704887293));
#46694=CARTESIAN_POINT('Ctrl Pts',(-0.10769043523109,-1.,-2.12499752307));
#46695=CARTESIAN_POINT('Ctrl Pts',(-0.10769043523109,1.,-2.12499752307));
#46696=CARTESIAN_POINT('Ctrl Pts',(-0.110350236135025,-1.,-2.11926155590865));
#46697=CARTESIAN_POINT('Ctrl Pts',(-0.110350236135025,1.,-2.11926155590865));
#46698=CARTESIAN_POINT('Ctrl Pts',(-0.112968534419737,-1.,-2.11351924490306));
#46699=CARTESIAN_POINT('Ctrl Pts',(-0.112968534419737,1.,-2.11351924490306));
#46700=CARTESIAN_POINT('Ctrl Pts',(-0.115544957687926,-1.,-2.10777050261309));
#46701=CARTESIAN_POINT('Ctrl Pts',(-0.115544957687926,1.,-2.10777050261309));
#46702=CARTESIAN_POINT('Ctrl Pts',(-0.118079107988355,-1.,-2.102015121329));
#46703=CARTESIAN_POINT('Ctrl Pts',(-0.118079107988355,1.,-2.102015121329));
#46704=CARTESIAN_POINT('Ctrl Pts',(-0.120570567965122,-1.,-2.0962529286773));
#46705=CARTESIAN_POINT('Ctrl Pts',(-0.120570567965122,1.,-2.0962529286773));
#46706=CARTESIAN_POINT('Ctrl Pts',(-0.123018905621083,-1.,-2.09048392424825));
#46707=CARTESIAN_POINT('Ctrl Pts',(-0.123018905621083,1.,-2.09048392424825));
#46708=CARTESIAN_POINT('Ctrl Pts',(-0.125423679412061,-1.,-2.08470840653643));
#46709=CARTESIAN_POINT('Ctrl Pts',(-0.125423679412061,1.,-2.08470840653643));
#46710=CARTESIAN_POINT('Ctrl Pts',(-0.12778444527612,-1.,-2.07892715110987));
#46711=CARTESIAN_POINT('Ctrl Pts',(-0.12778444527612,1.,-2.07892715110987));
#46712=CARTESIAN_POINT('Ctrl Pts',(-0.130100748328403,-1.,-2.07314114713063));
#46713=CARTESIAN_POINT('Ctrl Pts',(-0.130100748328403,1.,-2.07314114713063));
#46714=CARTESIAN_POINT('Ctrl Pts',(-0.13237211154771,-1.,-2.06735123910326));
#46715=CARTESIAN_POINT('Ctrl Pts',(-0.13237211154771,1.,-2.06735123910326));
#46716=CARTESIAN_POINT('Ctrl Pts',(-0.134598026192106,-1.,-2.06155781517842));
#46717=CARTESIAN_POINT('Ctrl Pts',(-0.134598026192106,1.,-2.06155781517842));
#46718=CARTESIAN_POINT('Ctrl Pts',(-0.136777941218044,-1.,-2.05576044414264));
#46719=CARTESIAN_POINT('Ctrl Pts',(-0.136777941218044,1.,-2.05576044414264));
#46720=CARTESIAN_POINT('Ctrl Pts',(-0.138911255368966,-1.,-2.04995762001328));
#46721=CARTESIAN_POINT('Ctrl Pts',(-0.138911255368966,1.,-2.04995762001328));
#46722=CARTESIAN_POINT('Ctrl Pts',(-0.140997332152546,-1.,-2.04414757947916));
#46723=CARTESIAN_POINT('Ctrl Pts',(-0.140997332152546,1.,-2.04414757947916));
#46724=CARTESIAN_POINT('Ctrl Pts',(-0.143035515058209,-1.,-2.03832911025912));
#46725=CARTESIAN_POINT('Ctrl Pts',(-0.143035515058209,1.,-2.03832911025912));
#46726=CARTESIAN_POINT('Ctrl Pts',(-0.145025140186057,-1.,-2.03250223739942));
#46727=CARTESIAN_POINT('Ctrl Pts',(-0.145025140186057,1.,-2.03250223739942));
#46728=CARTESIAN_POINT('Ctrl Pts',(-0.146965557332583,-1.,-2.02666926182017));
#46729=CARTESIAN_POINT('Ctrl Pts',(-0.146965557332583,1.,-2.02666926182017));
#46730=CARTESIAN_POINT('Ctrl Pts',(-0.148856124775337,-1.,-2.02083464969894));
#46731=CARTESIAN_POINT('Ctrl Pts',(-0.148856124775337,1.,-2.02083464969894));
#46732=CARTESIAN_POINT('Ctrl Pts',(-0.150696157673078,-1.,-2.01500291940238));
#46733=CARTESIAN_POINT('Ctrl Pts',(-0.150696157673078,1.,-2.01500291940238));
#46734=CARTESIAN_POINT('Ctrl Pts',(-0.15248488362145,-1.,-2.00917680318424));
#46735=CARTESIAN_POINT('Ctrl Pts',(-0.15248488362145,1.,-2.00917680318424));
#46736=CARTESIAN_POINT('Ctrl Pts',(-0.154221403049722,-1.,-2.00335565310543));
#46737=CARTESIAN_POINT('Ctrl Pts',(-0.154221403049722,1.,-2.00335565310543));
#46738=CARTESIAN_POINT('Ctrl Pts',(-0.155904629548783,-1.,-1.99753284771497));
#46739=CARTESIAN_POINT('Ctrl Pts',(-0.155904629548783,1.,-1.99753284771497));
#46740=CARTESIAN_POINT('Ctrl Pts',(-0.157533331459227,-1.,-1.99169810931908));
#46741=CARTESIAN_POINT('Ctrl Pts',(-0.157533331459227,1.,-1.99169810931908));
#46742=CARTESIAN_POINT('Ctrl Pts',(-0.159106226437299,-1.,-1.98584238283292));
#46743=CARTESIAN_POINT('Ctrl Pts',(-0.159106226437299,1.,-1.98584238283292));
#46744=CARTESIAN_POINT('Ctrl Pts',(-0.160622060784611,-1.,-1.97996195437559));
#46745=CARTESIAN_POINT('Ctrl Pts',(-0.160622060784611,1.,-1.97996195437559));
#46746=CARTESIAN_POINT('Ctrl Pts',(-0.162079693556289,-1.,-1.97406280235188));
#46747=CARTESIAN_POINT('Ctrl Pts',(-0.162079693556289,1.,-1.97406280235188));
#46748=CARTESIAN_POINT('Ctrl Pts',(-0.163478185457734,-1.,-1.96816512677967));
#46749=CARTESIAN_POINT('Ctrl Pts',(-0.163478185457734,1.,-1.96816512677967));
#46750=CARTESIAN_POINT('Ctrl Pts',(-0.164816568920269,-1.,-1.96229379940136));
#46751=CARTESIAN_POINT('Ctrl Pts',(-0.164816568920269,1.,-1.96229379940136));
#46752=CARTESIAN_POINT('Ctrl Pts',(-0.166093592002812,-1.,-1.9564675971873));
#46753=CARTESIAN_POINT('Ctrl Pts',(-0.166093592002812,1.,-1.9564675971873));
#46754=CARTESIAN_POINT('Ctrl Pts',(-0.167307501784475,-1.,-1.95069027794294));
#46755=CARTESIAN_POINT('Ctrl Pts',(-0.167307501784475,1.,-1.95069027794294));
#46756=CARTESIAN_POINT('Ctrl Pts',(-0.168455741607556,-1.,-1.94493757756931));
#46757=CARTESIAN_POINT('Ctrl Pts',(-0.168455741607556,1.,-1.94493757756931));
#46758=CARTESIAN_POINT('Ctrl Pts',(-0.169534904817491,-1.,-1.93915639211581));
#46759=CARTESIAN_POINT('Ctrl Pts',(-0.169534904817491,1.,-1.93915639211581));
#46760=CARTESIAN_POINT('Ctrl Pts',(-0.170541253116202,-1.,-1.93329183155539));
#46761=CARTESIAN_POINT('Ctrl Pts',(-0.170541253116202,1.,-1.93329183155539));
#46762=CARTESIAN_POINT('Ctrl Pts',(-0.171471191532988,-1.,-1.92731093582036));
#46763=CARTESIAN_POINT('Ctrl Pts',(-0.171471191532988,1.,-1.92731093582036));
#46764=CARTESIAN_POINT('Ctrl Pts',(-0.172321621259514,-1.,-1.9212233439798));
#46765=CARTESIAN_POINT('Ctrl Pts',(-0.172321621259514,1.,-1.9212233439798));
#46766=CARTESIAN_POINT('Ctrl Pts',(-0.173090695383496,-1.,-1.91511429159527));
#46767=CARTESIAN_POINT('Ctrl Pts',(-0.173090695383496,1.,-1.91511429159527));
#46768=CARTESIAN_POINT('Ctrl Pts',(-0.173776635257817,-1.,-1.90911693975267));
#46769=CARTESIAN_POINT('Ctrl Pts',(-0.173776635257817,1.,-1.90911693975267));
#46770=CARTESIAN_POINT('Ctrl Pts',(-0.174375518661085,-1.,-1.90335253862834));
#46771=CARTESIAN_POINT('Ctrl Pts',(-0.174375518661085,1.,-1.90335253862834));
#46772=CARTESIAN_POINT('Ctrl Pts',(-0.174879405091263,-1.,-1.89788101117132));
#46773=CARTESIAN_POINT('Ctrl Pts',(-0.174879405091263,1.,-1.89788101117132));
#46774=CARTESIAN_POINT('Ctrl Pts',(-0.175274276190844,-1.,-1.892646301985));
#46775=CARTESIAN_POINT('Ctrl Pts',(-0.175274276190844,1.,-1.892646301985));
#46776=CARTESIAN_POINT('Ctrl Pts',(-0.175538155840648,-1.,-1.88742606273259));
#46777=CARTESIAN_POINT('Ctrl Pts',(-0.175538155840648,1.,-1.88742606273259));
#46778=CARTESIAN_POINT('Ctrl Pts',(-0.175644148889699,-1.,-1.88188663145367));
#46779=CARTESIAN_POINT('Ctrl Pts',(-0.175644148889699,1.,-1.88188663145367));
#46780=CARTESIAN_POINT('Ctrl Pts',(-0.175563480746485,-1.,-1.87563767773588));
#46781=CARTESIAN_POINT('Ctrl Pts',(-0.175563480746485,1.,-1.87563767773588));
#46782=CARTESIAN_POINT('Ctrl Pts',(-0.175268337590758,-1.,-1.86828349694799));
#46783=CARTESIAN_POINT('Ctrl Pts',(-0.175268337590758,1.,-1.86828349694799));
#46784=CARTESIAN_POINT('Ctrl Pts',(-0.17473525927603,-1.,-1.85948367088837));
#46785=CARTESIAN_POINT('Ctrl Pts',(-0.17473525927603,1.,-1.85948367088837));
#46786=CARTESIAN_POINT('Ctrl Pts',(-0.173946627587731,-1.,-1.8489811319852));
#46787=CARTESIAN_POINT('Ctrl Pts',(-0.173946627587731,1.,-1.8489811319852));
#46788=CARTESIAN_POINT('Ctrl Pts',(-0.1728894428919,-1.,-1.83658380527692));
#46789=CARTESIAN_POINT('Ctrl Pts',(-0.1728894428919,1.,-1.83658380527692));
#46790=CARTESIAN_POINT('Ctrl Pts',(-0.171554770204119,-1.,-1.82215766811545));
#46791=CARTESIAN_POINT('Ctrl Pts',(-0.171554770204119,1.,-1.82215766811545));
#46792=CARTESIAN_POINT('Ctrl Pts',(-0.169936923904608,-1.,-1.80561530629706));
#46793=CARTESIAN_POINT('Ctrl Pts',(-0.169936923904608,1.,-1.80561530629706));
#46794=CARTESIAN_POINT('Ctrl Pts',(-0.168032772805197,-1.,-1.7869064998507));
#46795=CARTESIAN_POINT('Ctrl Pts',(-0.168032772805197,1.,-1.7869064998507));
#46796=CARTESIAN_POINT('Ctrl Pts',(-0.1662793551464,-1.,-1.77018771684844));
#46797=CARTESIAN_POINT('Ctrl Pts',(-0.1662793551464,1.,-1.77018771684844));
#46798=CARTESIAN_POINT('Ctrl Pts',(-0.164834765707158,-1.,-1.75666056638427));
#46799=CARTESIAN_POINT('Ctrl Pts',(-0.164834765707158,1.,-1.75666056638427));
#46800=CARTESIAN_POINT('Ctrl Pts',(-0.163814161002002,-1.,-1.7472034950333));
#46801=CARTESIAN_POINT('Ctrl Pts',(-0.163814161002002,1.,-1.7472034950333));
#46802=CARTESIAN_POINT('Ctrl Pts',(-0.163289472382896,-1.,-1.74236521665491));
#46803=CARTESIAN_POINT('Ctrl Pts',(-0.163289472382896,1.,-1.74236521665491));
#46804=CARTESIAN_POINT('',(-0.0694764450219581,1.,-2.19890268624765));
#46805=CARTESIAN_POINT('Ctrl Pts',(-0.0694764450219581,1.,-2.19890268624765));
#46806=CARTESIAN_POINT('Ctrl Pts',(-0.070114353632549,1.,-2.19777582085423));
#46807=CARTESIAN_POINT('Ctrl Pts',(-0.0713863779526154,1.,-2.19552129484002));
#46808=CARTESIAN_POINT('Ctrl Pts',(-0.0732830357306725,1.,-2.19213712013662));
#46809=CARTESIAN_POINT('Ctrl Pts',(-0.0757891465836148,1.,-2.1876201139953));
#46810=CARTESIAN_POINT('Ctrl Pts',(-0.0788837727685243,1.,-2.18196589448887));
#46811=CARTESIAN_POINT('Ctrl Pts',(-0.0819402680872765,1.,-2.176303712113));
#46812=CARTESIAN_POINT('Ctrl Pts',(-0.0849584620835372,1.,-2.17063357870952));
#46813=CARTESIAN_POINT('Ctrl Pts',(-0.0879381291386923,1.,-2.16495552645014));
#46814=CARTESIAN_POINT('Ctrl Pts',(-0.0908789888107265,1.,-2.15926961544516));
#46815=CARTESIAN_POINT('Ctrl Pts',(-0.0937807218867643,1.,-2.1535759397817));
#46816=CARTESIAN_POINT('Ctrl Pts',(-0.0966429852305459,1.,-2.14787463531795));
#46817=CARTESIAN_POINT('Ctrl Pts',(-0.0994654261990915,1.,-2.14216588396025));
#46818=CARTESIAN_POINT('Ctrl Pts',(-0.1022477005561,1.,-2.13644992667165));
#46819=CARTESIAN_POINT('Ctrl Pts',(-0.104989479152739,1.,-2.13072704887293));
#46820=CARTESIAN_POINT('Ctrl Pts',(-0.10769043523109,1.,-2.12499752307));
#46821=CARTESIAN_POINT('Ctrl Pts',(-0.110350236135025,1.,-2.11926155590865));
#46822=CARTESIAN_POINT('Ctrl Pts',(-0.112968534419737,1.,-2.11351924490306));
#46823=CARTESIAN_POINT('Ctrl Pts',(-0.115544957687926,1.,-2.10777050261309));
#46824=CARTESIAN_POINT('Ctrl Pts',(-0.118079107988355,1.,-2.102015121329));
#46825=CARTESIAN_POINT('Ctrl Pts',(-0.120570567965122,1.,-2.0962529286773));
#46826=CARTESIAN_POINT('Ctrl Pts',(-0.123018905621083,1.,-2.09048392424825));
#46827=CARTESIAN_POINT('Ctrl Pts',(-0.125423679412061,1.,-2.08470840653643));
#46828=CARTESIAN_POINT('Ctrl Pts',(-0.12778444527612,1.,-2.07892715110987));
#46829=CARTESIAN_POINT('Ctrl Pts',(-0.130100748328403,1.,-2.07314114713063));
#46830=CARTESIAN_POINT('Ctrl Pts',(-0.13237211154771,1.,-2.06735123910326));
#46831=CARTESIAN_POINT('Ctrl Pts',(-0.134598026192106,1.,-2.06155781517842));
#46832=CARTESIAN_POINT('Ctrl Pts',(-0.136777941218044,1.,-2.05576044414264));
#46833=CARTESIAN_POINT('Ctrl Pts',(-0.138911255368966,1.,-2.04995762001328));
#46834=CARTESIAN_POINT('Ctrl Pts',(-0.140997332152546,1.,-2.04414757947916));
#46835=CARTESIAN_POINT('Ctrl Pts',(-0.143035515058209,1.,-2.03832911025912));
#46836=CARTESIAN_POINT('Ctrl Pts',(-0.145025140186057,1.,-2.03250223739942));
#46837=CARTESIAN_POINT('Ctrl Pts',(-0.146965557332583,1.,-2.02666926182017));
#46838=CARTESIAN_POINT('Ctrl Pts',(-0.148856124775337,1.,-2.02083464969894));
#46839=CARTESIAN_POINT('Ctrl Pts',(-0.150696157673078,1.,-2.01500291940238));
#46840=CARTESIAN_POINT('Ctrl Pts',(-0.15248488362145,1.,-2.00917680318424));
#46841=CARTESIAN_POINT('Ctrl Pts',(-0.154221403049722,1.,-2.00335565310543));
#46842=CARTESIAN_POINT('Ctrl Pts',(-0.155904629548783,1.,-1.99753284771497));
#46843=CARTESIAN_POINT('Ctrl Pts',(-0.157533331459227,1.,-1.99169810931908));
#46844=CARTESIAN_POINT('Ctrl Pts',(-0.159106226437299,1.,-1.98584238283292));
#46845=CARTESIAN_POINT('Ctrl Pts',(-0.160622060784611,1.,-1.97996195437559));
#46846=CARTESIAN_POINT('Ctrl Pts',(-0.162079693556289,1.,-1.97406280235188));
#46847=CARTESIAN_POINT('Ctrl Pts',(-0.163478185457734,1.,-1.96816512677967));
#46848=CARTESIAN_POINT('Ctrl Pts',(-0.164816568920269,1.,-1.96229379940136));
#46849=CARTESIAN_POINT('Ctrl Pts',(-0.166093592002812,1.,-1.9564675971873));
#46850=CARTESIAN_POINT('Ctrl Pts',(-0.167307501784475,1.,-1.95069027794294));
#46851=CARTESIAN_POINT('Ctrl Pts',(-0.168455741607556,1.,-1.94493757756931));
#46852=CARTESIAN_POINT('Ctrl Pts',(-0.169534904817491,1.,-1.93915639211581));
#46853=CARTESIAN_POINT('Ctrl Pts',(-0.170541253116202,1.,-1.93329183155539));
#46854=CARTESIAN_POINT('Ctrl Pts',(-0.171471191532988,1.,-1.92731093582036));
#46855=CARTESIAN_POINT('Ctrl Pts',(-0.172321621259514,1.,-1.9212233439798));
#46856=CARTESIAN_POINT('Ctrl Pts',(-0.173090695383496,1.,-1.91511429159527));
#46857=CARTESIAN_POINT('Ctrl Pts',(-0.173776635257817,1.,-1.90911693975267));
#46858=CARTESIAN_POINT('Ctrl Pts',(-0.174375518661085,1.,-1.90335253862834));
#46859=CARTESIAN_POINT('Ctrl Pts',(-0.174879405091263,1.,-1.89788101117132));
#46860=CARTESIAN_POINT('Ctrl Pts',(-0.175274276190844,1.,-1.892646301985));
#46861=CARTESIAN_POINT('Ctrl Pts',(-0.175538155840648,1.,-1.88742606273259));
#46862=CARTESIAN_POINT('Ctrl Pts',(-0.175644148889699,1.,-1.88188663145367));
#46863=CARTESIAN_POINT('Ctrl Pts',(-0.175563480746485,1.,-1.87563767773588));
#46864=CARTESIAN_POINT('Ctrl Pts',(-0.175268337590758,1.,-1.86828349694799));
#46865=CARTESIAN_POINT('Ctrl Pts',(-0.17473525927603,1.,-1.85948367088837));
#46866=CARTESIAN_POINT('Ctrl Pts',(-0.173946627587731,1.,-1.8489811319852));
#46867=CARTESIAN_POINT('Ctrl Pts',(-0.1728894428919,1.,-1.83658380527692));
#46868=CARTESIAN_POINT('Ctrl Pts',(-0.171554770204119,1.,-1.82215766811545));
#46869=CARTESIAN_POINT('Ctrl Pts',(-0.169936923904608,1.,-1.80561530629706));
#46870=CARTESIAN_POINT('Ctrl Pts',(-0.168032772805197,1.,-1.7869064998507));
#46871=CARTESIAN_POINT('Ctrl Pts',(-0.1662793551464,1.,-1.77018771684844));
#46872=CARTESIAN_POINT('Ctrl Pts',(-0.164834765707158,1.,-1.75666056638427));
#46873=CARTESIAN_POINT('Ctrl Pts',(-0.163814161002002,1.,-1.7472034950333));
#46874=CARTESIAN_POINT('Ctrl Pts',(-0.163289472382896,1.,-1.74236521665491));
#46875=CARTESIAN_POINT('',(-0.0694764450219581,0.,-2.19890268624765));
#46876=CARTESIAN_POINT('Origin',(0.0694764450219584,0.,-2.19890268624765));
#46877=CARTESIAN_POINT('',(0.0694764450219584,1.,-2.19890268624765));
#46878=CARTESIAN_POINT('',(-0.0694764450219581,1.,-2.19890268624765));
#46879=CARTESIAN_POINT('',(0.0694764450219584,0.,-2.19890268624765));
#46880=CARTESIAN_POINT('Ctrl Pts',(0.163289472382896,-1.,-1.74236521665491));
#46881=CARTESIAN_POINT('Ctrl Pts',(0.163289472382896,1.,-1.74236521665491));
#46882=CARTESIAN_POINT('Ctrl Pts',(0.163814161002474,-1.,-1.74720349503904));
#46883=CARTESIAN_POINT('Ctrl Pts',(0.163814161002474,1.,-1.74720349503904));
#46884=CARTESIAN_POINT('Ctrl Pts',(0.164834765708484,-1.,-1.75666056640041));
#46885=CARTESIAN_POINT('Ctrl Pts',(0.164834765708484,1.,-1.75666056640041));
#46886=CARTESIAN_POINT('Ctrl Pts',(0.166279355148738,-1.,-1.77018771687692));
#46887=CARTESIAN_POINT('Ctrl Pts',(0.166279355148738,1.,-1.77018771687692));
#46888=CARTESIAN_POINT('Ctrl Pts',(0.16803277280837,-1.,-1.78690649988931));
#46889=CARTESIAN_POINT('Ctrl Pts',(0.16803277280837,1.,-1.78690649988931));
#46890=CARTESIAN_POINT('Ctrl Pts',(0.169936923908078,-1.,-1.80561530633924));
#46891=CARTESIAN_POINT('Ctrl Pts',(0.169936923908078,1.,-1.80561530633924));
#46892=CARTESIAN_POINT('Ctrl Pts',(0.171554770207306,-1.,-1.82215766815414));
#46893=CARTESIAN_POINT('Ctrl Pts',(0.171554770207306,1.,-1.82215766815414));
#46894=CARTESIAN_POINT('Ctrl Pts',(0.17288944289442,-1.,-1.83658380530747));
#46895=CARTESIAN_POINT('Ctrl Pts',(0.17288944289442,1.,-1.83658380530747));
#46896=CARTESIAN_POINT('Ctrl Pts',(0.173946627589401,-1.,-1.84898113200543));
#46897=CARTESIAN_POINT('Ctrl Pts',(0.173946627589401,1.,-1.84898113200543));
#46898=CARTESIAN_POINT('Ctrl Pts',(0.174735259276856,-1.,-1.85948367089838));
#46899=CARTESIAN_POINT('Ctrl Pts',(0.174735259276856,1.,-1.85948367089838));
#46900=CARTESIAN_POINT('Ctrl Pts',(0.175268337590901,-1.,-1.86828349694972));
#46901=CARTESIAN_POINT('Ctrl Pts',(0.175268337590901,1.,-1.86828349694972));
#46902=CARTESIAN_POINT('Ctrl Pts',(0.175563480746205,-1.,-1.87563767773249));
#46903=CARTESIAN_POINT('Ctrl Pts',(0.175563480746205,1.,-1.87563767773249));
#46904=CARTESIAN_POINT('Ctrl Pts',(0.175644148889271,-1.,-1.88188663144846));
#46905=CARTESIAN_POINT('Ctrl Pts',(0.175644148889271,1.,-1.88188663144846));
#46906=CARTESIAN_POINT('Ctrl Pts',(0.175538155840286,-1.,-1.88742606272818));
#46907=CARTESIAN_POINT('Ctrl Pts',(0.175538155840286,1.,-1.88742606272818));
#46908=CARTESIAN_POINT('Ctrl Pts',(0.175274276190664,-1.,-1.89264630198279));
#46909=CARTESIAN_POINT('Ctrl Pts',(0.175274276190664,1.,-1.89264630198279));
#46910=CARTESIAN_POINT('Ctrl Pts',(0.174879405091277,-1.,-1.89788101117148));
#46911=CARTESIAN_POINT('Ctrl Pts',(0.174879405091277,1.,-1.89788101117148));
#46912=CARTESIAN_POINT('Ctrl Pts',(0.174375518661222,-1.,-1.90335253863003));
#46913=CARTESIAN_POINT('Ctrl Pts',(0.174375518661222,1.,-1.90335253863003));
#46914=CARTESIAN_POINT('Ctrl Pts',(0.173776635257984,-1.,-1.90911693975475));
#46915=CARTESIAN_POINT('Ctrl Pts',(0.173776635257984,1.,-1.90911693975475));
#46916=CARTESIAN_POINT('Ctrl Pts',(0.173090695383619,-1.,-1.91511429159681));
#46917=CARTESIAN_POINT('Ctrl Pts',(0.173090695383619,1.,-1.91511429159681));
#46918=CARTESIAN_POINT('Ctrl Pts',(0.172321621259557,-1.,-1.92122334398034));
#46919=CARTESIAN_POINT('Ctrl Pts',(0.172321621259557,1.,-1.92122334398034));
#46920=CARTESIAN_POINT('Ctrl Pts',(0.17147119153296,-1.,-1.92731093582));
#46921=CARTESIAN_POINT('Ctrl Pts',(0.17147119153296,1.,-1.92731093582));
#46922=CARTESIAN_POINT('Ctrl Pts',(0.170541253116136,-1.,-1.93329183155455));
#46923=CARTESIAN_POINT('Ctrl Pts',(0.170541253116136,1.,-1.93329183155455));
#46924=CARTESIAN_POINT('Ctrl Pts',(0.169534904817425,-1.,-1.93915639211497));
#46925=CARTESIAN_POINT('Ctrl Pts',(0.169534904817425,1.,-1.93915639211497));
#46926=CARTESIAN_POINT('Ctrl Pts',(0.168455741607516,-1.,-1.94493757756879));
#46927=CARTESIAN_POINT('Ctrl Pts',(0.168455741607516,1.,-1.94493757756879));
#46928=CARTESIAN_POINT('Ctrl Pts',(0.167307501784469,-1.,-1.95069027794286));
#46929=CARTESIAN_POINT('Ctrl Pts',(0.167307501784469,1.,-1.95069027794286));
#46930=CARTESIAN_POINT('Ctrl Pts',(0.166093592002833,-1.,-1.95646759718755));
#46931=CARTESIAN_POINT('Ctrl Pts',(0.166093592002833,1.,-1.95646759718755));
#46932=CARTESIAN_POINT('Ctrl Pts',(0.1648165689203,-1.,-1.96229379940174));
#46933=CARTESIAN_POINT('Ctrl Pts',(0.1648165689203,1.,-1.96229379940174));
#46934=CARTESIAN_POINT('Ctrl Pts',(0.16347818545776,-1.,-1.96816512678));
#46935=CARTESIAN_POINT('Ctrl Pts',(0.16347818545776,1.,-1.96816512678));
#46936=CARTESIAN_POINT('Ctrl Pts',(0.162079693556302,-1.,-1.97406280235204));
#46937=CARTESIAN_POINT('Ctrl Pts',(0.162079693556302,1.,-1.97406280235204));
#46938=CARTESIAN_POINT('Ctrl Pts',(0.16062206078461,-1.,-1.97996195437557));
#46939=CARTESIAN_POINT('Ctrl Pts',(0.16062206078461,1.,-1.97996195437557));
#46940=CARTESIAN_POINT('Ctrl Pts',(0.159106226437288,-1.,-1.98584238283279));
#46941=CARTESIAN_POINT('Ctrl Pts',(0.159106226437288,1.,-1.98584238283279));
#46942=CARTESIAN_POINT('Ctrl Pts',(0.157533331459215,-1.,-1.99169810931893));
#46943=CARTESIAN_POINT('Ctrl Pts',(0.157533331459215,1.,-1.99169810931893));
#46944=CARTESIAN_POINT('Ctrl Pts',(0.155904629548774,-1.,-1.99753284771487));
#46945=CARTESIAN_POINT('Ctrl Pts',(0.155904629548774,1.,-1.99753284771487));
#46946=CARTESIAN_POINT('Ctrl Pts',(0.154221403049719,-1.,-2.00335565310539));
#46947=CARTESIAN_POINT('Ctrl Pts',(0.154221403049719,1.,-2.00335565310539));
#46948=CARTESIAN_POINT('Ctrl Pts',(0.152484883621452,-1.,-2.00917680318426));
#46949=CARTESIAN_POINT('Ctrl Pts',(0.152484883621452,1.,-2.00917680318426));
#46950=CARTESIAN_POINT('Ctrl Pts',(0.150696157673084,-1.,-2.01500291940243));
#46951=CARTESIAN_POINT('Ctrl Pts',(0.150696157673084,1.,-2.01500291940243));
#46952=CARTESIAN_POINT('Ctrl Pts',(0.148856124775343,-1.,-2.02083464969897));
#46953=CARTESIAN_POINT('Ctrl Pts',(0.148856124775343,1.,-2.02083464969897));
#46954=CARTESIAN_POINT('Ctrl Pts',(0.146965557332586,-1.,-2.02666926182017));
#46955=CARTESIAN_POINT('Ctrl Pts',(0.146965557332586,1.,-2.02666926182017));
#46956=CARTESIAN_POINT('Ctrl Pts',(0.145025140186058,-1.,-2.03250223739941));
#46957=CARTESIAN_POINT('Ctrl Pts',(0.145025140186058,1.,-2.03250223739941));
#46958=CARTESIAN_POINT('Ctrl Pts',(0.143035515058208,-1.,-2.03832911025913));
#46959=CARTESIAN_POINT('Ctrl Pts',(0.143035515058208,1.,-2.03832911025913));
#46960=CARTESIAN_POINT('Ctrl Pts',(0.140997332152545,-1.,-2.04414757947919));
#46961=CARTESIAN_POINT('Ctrl Pts',(0.140997332152545,1.,-2.04414757947919));
#46962=CARTESIAN_POINT('Ctrl Pts',(0.138911255368966,-1.,-2.04995762001333));
#46963=CARTESIAN_POINT('Ctrl Pts',(0.138911255368966,1.,-2.04995762001333));
#46964=CARTESIAN_POINT('Ctrl Pts',(0.136777941218044,-1.,-2.0557604441427));
#46965=CARTESIAN_POINT('Ctrl Pts',(0.136777941218044,1.,-2.0557604441427));
#46966=CARTESIAN_POINT('Ctrl Pts',(0.134598026192107,-1.,-2.06155781517844));
#46967=CARTESIAN_POINT('Ctrl Pts',(0.134598026192107,1.,-2.06155781517844));
#46968=CARTESIAN_POINT('Ctrl Pts',(0.13237211154771,-1.,-2.06735123910319));
#46969=CARTESIAN_POINT('Ctrl Pts',(0.13237211154771,1.,-2.06735123910319));
#46970=CARTESIAN_POINT('Ctrl Pts',(0.1301007483284,-1.,-2.07314114713047));
#46971=CARTESIAN_POINT('Ctrl Pts',(0.1301007483284,1.,-2.07314114713047));
#46972=CARTESIAN_POINT('Ctrl Pts',(0.127784445276116,-1.,-2.07892715110967));
#46973=CARTESIAN_POINT('Ctrl Pts',(0.127784445276116,1.,-2.07892715110967));
#46974=CARTESIAN_POINT('Ctrl Pts',(0.125423679412058,-1.,-2.08470840653628));
#46975=CARTESIAN_POINT('Ctrl Pts',(0.125423679412058,1.,-2.08470840653628));
#46976=CARTESIAN_POINT('Ctrl Pts',(0.123018905621083,-1.,-2.09048392424826));
#46977=CARTESIAN_POINT('Ctrl Pts',(0.123018905621083,1.,-2.09048392424826));
#46978=CARTESIAN_POINT('Ctrl Pts',(0.120570567965129,-1.,-2.09625292867756));
#46979=CARTESIAN_POINT('Ctrl Pts',(0.120570567965129,1.,-2.09625292867756));
#46980=CARTESIAN_POINT('Ctrl Pts',(0.118079107988368,-1.,-2.10201512132945));
#46981=CARTESIAN_POINT('Ctrl Pts',(0.118079107988368,1.,-2.10201512132945));
#46982=CARTESIAN_POINT('Ctrl Pts',(0.11554495768794,-1.,-2.10777050261359));
#46983=CARTESIAN_POINT('Ctrl Pts',(0.11554495768794,1.,-2.10777050261359));
#46984=CARTESIAN_POINT('Ctrl Pts',(0.112968534419746,-1.,-2.11351924490335));
#46985=CARTESIAN_POINT('Ctrl Pts',(0.112968534419746,1.,-2.11351924490335));
#46986=CARTESIAN_POINT('Ctrl Pts',(0.11035023613502,-1.,-2.11926155590849));
#46987=CARTESIAN_POINT('Ctrl Pts',(0.11035023613502,1.,-2.11926155590849));
#46988=CARTESIAN_POINT('Ctrl Pts',(0.107690435231068,-1.,-2.12499752306927));
#46989=CARTESIAN_POINT('Ctrl Pts',(0.107690435231068,1.,-2.12499752306927));
#46990=CARTESIAN_POINT('Ctrl Pts',(0.104989479152703,-1.,-2.1307270488718));
#46991=CARTESIAN_POINT('Ctrl Pts',(0.104989479152703,1.,-2.1307270488718));
#46992=CARTESIAN_POINT('Ctrl Pts',(0.102247700556064,-1.,-2.13644992667052));
#46993=CARTESIAN_POINT('Ctrl Pts',(0.102247700556064,1.,-2.13644992667052));
#46994=CARTESIAN_POINT('Ctrl Pts',(0.0994654261990743,-1.,-2.14216588395974));
#46995=CARTESIAN_POINT('Ctrl Pts',(0.0994654261990743,1.,-2.14216588395974));
#46996=CARTESIAN_POINT('Ctrl Pts',(0.0966429852305689,-1.,-2.14787463531864));
#46997=CARTESIAN_POINT('Ctrl Pts',(0.0966429852305689,1.,-2.14787463531864));
#46998=CARTESIAN_POINT('Ctrl Pts',(0.0937807218868345,-1.,-2.15357593978377));
#46999=CARTESIAN_POINT('Ctrl Pts',(0.0937807218868345,1.,-2.15357593978377));
#47000=CARTESIAN_POINT('Ctrl Pts',(0.0908789888108266,-1.,-2.15926961544808));
#47001=CARTESIAN_POINT('Ctrl Pts',(0.0908789888108266,1.,-2.15926961544808));
#47002=CARTESIAN_POINT('Ctrl Pts',(0.0879381291387823,-1.,-2.16495552645275));
#47003=CARTESIAN_POINT('Ctrl Pts',(0.0879381291387823,1.,-2.16495552645275));
#47004=CARTESIAN_POINT('Ctrl Pts',(0.0849584620835643,-1.,-2.17063357871031));
#47005=CARTESIAN_POINT('Ctrl Pts',(0.0849584620835643,1.,-2.17063357871031));
#47006=CARTESIAN_POINT('Ctrl Pts',(0.0819402680871939,-1.,-2.1763037121106));
#47007=CARTESIAN_POINT('Ctrl Pts',(0.0819402680871939,1.,-2.1763037121106));
#47008=CARTESIAN_POINT('Ctrl Pts',(0.0788837727683228,-1.,-2.18196589448304));
#47009=CARTESIAN_POINT('Ctrl Pts',(0.0788837727683228,1.,-2.18196589448304));
#47010=CARTESIAN_POINT('Ctrl Pts',(0.0757891465833411,-1.,-2.1876201139874));
#47011=CARTESIAN_POINT('Ctrl Pts',(0.0757891465833411,1.,-2.1876201139874));
#47012=CARTESIAN_POINT('Ctrl Pts',(0.0732830357304276,-1.,-2.19213712012956));
#47013=CARTESIAN_POINT('Ctrl Pts',(0.0732830357304276,1.,-2.19213712012956));
#47014=CARTESIAN_POINT('Ctrl Pts',(0.0713863779524627,-1.,-2.19552129483562));
#47015=CARTESIAN_POINT('Ctrl Pts',(0.0713863779524627,1.,-2.19552129483562));
#47016=CARTESIAN_POINT('Ctrl Pts',(0.0701143536324926,-1.,-2.19777582085261));
#47017=CARTESIAN_POINT('Ctrl Pts',(0.0701143536324926,1.,-2.19777582085261));
#47018=CARTESIAN_POINT('Ctrl Pts',(0.0694764450219584,-1.,-2.19890268624765));
#47019=CARTESIAN_POINT('Ctrl Pts',(0.0694764450219584,1.,-2.19890268624765));
#47020=CARTESIAN_POINT('',(0.163289472382896,1.,-1.74236521665491));
#47021=CARTESIAN_POINT('Ctrl Pts',(0.163289472382896,1.,-1.74236521665491));
#47022=CARTESIAN_POINT('Ctrl Pts',(0.163814161002474,1.,-1.74720349503904));
#47023=CARTESIAN_POINT('Ctrl Pts',(0.164834765708484,1.,-1.75666056640041));
#47024=CARTESIAN_POINT('Ctrl Pts',(0.166279355148738,1.,-1.77018771687692));
#47025=CARTESIAN_POINT('Ctrl Pts',(0.16803277280837,1.,-1.78690649988931));
#47026=CARTESIAN_POINT('Ctrl Pts',(0.169936923908078,1.,-1.80561530633924));
#47027=CARTESIAN_POINT('Ctrl Pts',(0.171554770207306,1.,-1.82215766815414));
#47028=CARTESIAN_POINT('Ctrl Pts',(0.17288944289442,1.,-1.83658380530747));
#47029=CARTESIAN_POINT('Ctrl Pts',(0.173946627589401,1.,-1.84898113200543));
#47030=CARTESIAN_POINT('Ctrl Pts',(0.174735259276856,1.,-1.85948367089838));
#47031=CARTESIAN_POINT('Ctrl Pts',(0.175268337590901,1.,-1.86828349694972));
#47032=CARTESIAN_POINT('Ctrl Pts',(0.175563480746205,1.,-1.87563767773249));
#47033=CARTESIAN_POINT('Ctrl Pts',(0.175644148889271,1.,-1.88188663144846));
#47034=CARTESIAN_POINT('Ctrl Pts',(0.175538155840286,1.,-1.88742606272818));
#47035=CARTESIAN_POINT('Ctrl Pts',(0.175274276190664,1.,-1.89264630198279));
#47036=CARTESIAN_POINT('Ctrl Pts',(0.174879405091277,1.,-1.89788101117148));
#47037=CARTESIAN_POINT('Ctrl Pts',(0.174375518661222,1.,-1.90335253863003));
#47038=CARTESIAN_POINT('Ctrl Pts',(0.173776635257984,1.,-1.90911693975475));
#47039=CARTESIAN_POINT('Ctrl Pts',(0.173090695383619,1.,-1.91511429159681));
#47040=CARTESIAN_POINT('Ctrl Pts',(0.172321621259557,1.,-1.92122334398034));
#47041=CARTESIAN_POINT('Ctrl Pts',(0.17147119153296,1.,-1.92731093582));
#47042=CARTESIAN_POINT('Ctrl Pts',(0.170541253116136,1.,-1.93329183155455));
#47043=CARTESIAN_POINT('Ctrl Pts',(0.169534904817425,1.,-1.93915639211497));
#47044=CARTESIAN_POINT('Ctrl Pts',(0.168455741607516,1.,-1.94493757756879));
#47045=CARTESIAN_POINT('Ctrl Pts',(0.167307501784469,1.,-1.95069027794286));
#47046=CARTESIAN_POINT('Ctrl Pts',(0.166093592002833,1.,-1.95646759718755));
#47047=CARTESIAN_POINT('Ctrl Pts',(0.1648165689203,1.,-1.96229379940174));
#47048=CARTESIAN_POINT('Ctrl Pts',(0.16347818545776,1.,-1.96816512678));
#47049=CARTESIAN_POINT('Ctrl Pts',(0.162079693556302,1.,-1.97406280235204));
#47050=CARTESIAN_POINT('Ctrl Pts',(0.16062206078461,1.,-1.97996195437557));
#47051=CARTESIAN_POINT('Ctrl Pts',(0.159106226437288,1.,-1.98584238283279));
#47052=CARTESIAN_POINT('Ctrl Pts',(0.157533331459215,1.,-1.99169810931893));
#47053=CARTESIAN_POINT('Ctrl Pts',(0.155904629548774,1.,-1.99753284771487));
#47054=CARTESIAN_POINT('Ctrl Pts',(0.154221403049719,1.,-2.00335565310539));
#47055=CARTESIAN_POINT('Ctrl Pts',(0.152484883621452,1.,-2.00917680318426));
#47056=CARTESIAN_POINT('Ctrl Pts',(0.150696157673084,1.,-2.01500291940243));
#47057=CARTESIAN_POINT('Ctrl Pts',(0.148856124775343,1.,-2.02083464969897));
#47058=CARTESIAN_POINT('Ctrl Pts',(0.146965557332586,1.,-2.02666926182017));
#47059=CARTESIAN_POINT('Ctrl Pts',(0.145025140186058,1.,-2.03250223739941));
#47060=CARTESIAN_POINT('Ctrl Pts',(0.143035515058208,1.,-2.03832911025913));
#47061=CARTESIAN_POINT('Ctrl Pts',(0.140997332152545,1.,-2.04414757947919));
#47062=CARTESIAN_POINT('Ctrl Pts',(0.138911255368966,1.,-2.04995762001333));
#47063=CARTESIAN_POINT('Ctrl Pts',(0.136777941218044,1.,-2.0557604441427));
#47064=CARTESIAN_POINT('Ctrl Pts',(0.134598026192107,1.,-2.06155781517844));
#47065=CARTESIAN_POINT('Ctrl Pts',(0.13237211154771,1.,-2.06735123910319));
#47066=CARTESIAN_POINT('Ctrl Pts',(0.1301007483284,1.,-2.07314114713047));
#47067=CARTESIAN_POINT('Ctrl Pts',(0.127784445276116,1.,-2.07892715110967));
#47068=CARTESIAN_POINT('Ctrl Pts',(0.125423679412058,1.,-2.08470840653628));
#47069=CARTESIAN_POINT('Ctrl Pts',(0.123018905621083,1.,-2.09048392424826));
#47070=CARTESIAN_POINT('Ctrl Pts',(0.120570567965129,1.,-2.09625292867756));
#47071=CARTESIAN_POINT('Ctrl Pts',(0.118079107988368,1.,-2.10201512132945));
#47072=CARTESIAN_POINT('Ctrl Pts',(0.11554495768794,1.,-2.10777050261359));
#47073=CARTESIAN_POINT('Ctrl Pts',(0.112968534419746,1.,-2.11351924490335));
#47074=CARTESIAN_POINT('Ctrl Pts',(0.11035023613502,1.,-2.11926155590849));
#47075=CARTESIAN_POINT('Ctrl Pts',(0.107690435231068,1.,-2.12499752306927));
#47076=CARTESIAN_POINT('Ctrl Pts',(0.104989479152703,1.,-2.1307270488718));
#47077=CARTESIAN_POINT('Ctrl Pts',(0.102247700556064,1.,-2.13644992667052));
#47078=CARTESIAN_POINT('Ctrl Pts',(0.0994654261990743,1.,-2.14216588395974));
#47079=CARTESIAN_POINT('Ctrl Pts',(0.0966429852305689,1.,-2.14787463531864));
#47080=CARTESIAN_POINT('Ctrl Pts',(0.0937807218868345,1.,-2.15357593978377));
#47081=CARTESIAN_POINT('Ctrl Pts',(0.0908789888108266,1.,-2.15926961544808));
#47082=CARTESIAN_POINT('Ctrl Pts',(0.0879381291387823,1.,-2.16495552645275));
#47083=CARTESIAN_POINT('Ctrl Pts',(0.0849584620835643,1.,-2.17063357871031));
#47084=CARTESIAN_POINT('Ctrl Pts',(0.0819402680871939,1.,-2.1763037121106));
#47085=CARTESIAN_POINT('Ctrl Pts',(0.0788837727683228,1.,-2.18196589448304));
#47086=CARTESIAN_POINT('Ctrl Pts',(0.0757891465833411,1.,-2.1876201139874));
#47087=CARTESIAN_POINT('Ctrl Pts',(0.0732830357304276,1.,-2.19213712012956));
#47088=CARTESIAN_POINT('Ctrl Pts',(0.0713863779524627,1.,-2.19552129483562));
#47089=CARTESIAN_POINT('Ctrl Pts',(0.0701143536324926,1.,-2.19777582085261));
#47090=CARTESIAN_POINT('Ctrl Pts',(0.0694764450219584,1.,-2.19890268624765));
#47091=CARTESIAN_POINT('',(0.163289472382896,0.,-1.74236521665491));
#47092=CARTESIAN_POINT('Origin',(0.,0.,0.));
#47093=CARTESIAN_POINT('',(0.383122945602004,1.,-1.7075470150345));
#47094=CARTESIAN_POINT('Origin',(0.,1.,0.));
#47095=CARTESIAN_POINT('',(0.383122945602004,0.,-1.7075470150345));
#47096=CARTESIAN_POINT('Ctrl Pts',(0.61342227326009,-1.,-2.11275013067528));
#47097=CARTESIAN_POINT('Ctrl Pts',(0.61342227326009,1.,-2.11275013067528));
#47098=CARTESIAN_POINT('Ctrl Pts',(0.61246736556225,-1.,-2.11187554260142));
#47099=CARTESIAN_POINT('Ctrl Pts',(0.61246736556225,1.,-2.11187554260142));
#47100=CARTESIAN_POINT('Ctrl Pts',(0.610560911691113,-1.,-2.11012443807661));
#47101=CARTESIAN_POINT('Ctrl Pts',(0.610560911691113,1.,-2.11012443807661));
#47102=CARTESIAN_POINT('Ctrl Pts',(0.607711315456826,-1.,-2.10749199615859));
#47103=CARTESIAN_POINT('Ctrl Pts',(0.607711315456826,1.,-2.10749199615859));
#47104=CARTESIAN_POINT('Ctrl Pts',(0.603932030738212,-1.,-2.10397049887709));
#47105=CARTESIAN_POINT('Ctrl Pts',(0.603932030738212,1.,-2.10397049887709));
#47106=CARTESIAN_POINT('Ctrl Pts',(0.599241616422144,-1.,-2.09954930865331));
#47107=CARTESIAN_POINT('Ctrl Pts',(0.599241616422144,1.,-2.09954930865331));
#47108=CARTESIAN_POINT('Ctrl Pts',(0.594585006052823,-1.,-2.09510876220501));
#47109=CARTESIAN_POINT('Ctrl Pts',(0.594585006052823,1.,-2.09510876220501));
#47110=CARTESIAN_POINT('Ctrl Pts',(0.589962365403189,-1.,-2.09064881812053));
#47111=CARTESIAN_POINT('Ctrl Pts',(0.589962365403189,1.,-2.09064881812053));
#47112=CARTESIAN_POINT('Ctrl Pts',(0.585373918990895,-1.,-2.086169437277));
#47113=CARTESIAN_POINT('Ctrl Pts',(0.585373918990895,1.,-2.086169437277));
#47114=CARTESIAN_POINT('Ctrl Pts',(0.580819952107256,-1.,-2.08167059018138));
#47115=CARTESIAN_POINT('Ctrl Pts',(0.580819952107256,1.,-2.08167059018138));
#47116=CARTESIAN_POINT('Ctrl Pts',(0.576300797416274,-1.,-2.07715226767361));
#47117=CARTESIAN_POINT('Ctrl Pts',(0.576300797416274,1.,-2.07715226767361));
#47118=CARTESIAN_POINT('Ctrl Pts',(0.571816823242411,-1.,-2.07261449292758));
#47119=CARTESIAN_POINT('Ctrl Pts',(0.571816823242411,1.,-2.07261449292758));
#47120=CARTESIAN_POINT('Ctrl Pts',(0.567368421181229,-1.,-2.06805732997383));
#47121=CARTESIAN_POINT('Ctrl Pts',(0.567368421181229,1.,-2.06805732997383));
#47122=CARTESIAN_POINT('Ctrl Pts',(0.562955993082574,-1.,-2.06348090160697));
#47123=CARTESIAN_POINT('Ctrl Pts',(0.562955993082574,1.,-2.06348090160697));
#47124=CARTESIAN_POINT('Ctrl Pts',(0.558579940185467,-1.,-2.05888537756571));
#47125=CARTESIAN_POINT('Ctrl Pts',(0.558579940185467,1.,-2.05888537756571));
#47126=CARTESIAN_POINT('Ctrl Pts',(0.554240657464109,-1.,-2.05427091604482));
#47127=CARTESIAN_POINT('Ctrl Pts',(0.554240657464109,1.,-2.05427091604482));
#47128=CARTESIAN_POINT('Ctrl Pts',(0.549938525150342,-1.,-2.04963761077974));
#47129=CARTESIAN_POINT('Ctrl Pts',(0.549938525150342,1.,-2.04963761077974));
#47130=CARTESIAN_POINT('Ctrl Pts',(0.545673903817348,-1.,-2.0449854471456));
#47131=CARTESIAN_POINT('Ctrl Pts',(0.545673903817348,1.,-2.0449854471456));
#47132=CARTESIAN_POINT('Ctrl Pts',(0.54144712061552,-1.,-2.0403142269048));
#47133=CARTESIAN_POINT('Ctrl Pts',(0.54144712061552,1.,-2.0403142269048));
#47134=CARTESIAN_POINT('Ctrl Pts',(0.537258489833134,-1.,-2.03562362953993));
#47135=CARTESIAN_POINT('Ctrl Pts',(0.537258489833134,1.,-2.03562362953993));
#47136=CARTESIAN_POINT('Ctrl Pts',(0.533108355132905,-1.,-2.03091336214401));
#47137=CARTESIAN_POINT('Ctrl Pts',(0.533108355132905,1.,-2.03091336214401));
#47138=CARTESIAN_POINT('Ctrl Pts',(0.52899712724191,-1.,-2.02618329083289));
#47139=CARTESIAN_POINT('Ctrl Pts',(0.52899712724191,1.,-2.02618329083289));
#47140=CARTESIAN_POINT('Ctrl Pts',(0.524925318333518,-1.,-2.02143356304712));
#47141=CARTESIAN_POINT('Ctrl Pts',(0.524925318333518,1.,-2.02143356304712));
#47142=CARTESIAN_POINT('Ctrl Pts',(0.520893590399428,-1.,-2.01666477917306));
#47143=CARTESIAN_POINT('Ctrl Pts',(0.520893590399428,1.,-2.01666477917306));
#47144=CARTESIAN_POINT('Ctrl Pts',(0.516902681728733,-1.,-2.01187773939257));
#47145=CARTESIAN_POINT('Ctrl Pts',(0.516902681728733,1.,-2.01187773939257));
#47146=CARTESIAN_POINT('Ctrl Pts',(0.512953306961813,-1.,-2.00707309946955));
#47147=CARTESIAN_POINT('Ctrl Pts',(0.512953306961813,1.,-2.00707309946955));
#47148=CARTESIAN_POINT('Ctrl Pts',(0.509046069886152,-1.,-2.00225107134733));
#47149=CARTESIAN_POINT('Ctrl Pts',(0.509046069886152,1.,-2.00225107134733));
#47150=CARTESIAN_POINT('Ctrl Pts',(0.505181361323011,-1.,-1.99741107463567));
#47151=CARTESIAN_POINT('Ctrl Pts',(0.505181361323011,1.,-1.99741107463567));
#47152=CARTESIAN_POINT('Ctrl Pts',(0.501359287727129,-1.,-1.9925514912615));
#47153=CARTESIAN_POINT('Ctrl Pts',(0.501359287727129,1.,-1.9925514912615));
#47154=CARTESIAN_POINT('Ctrl Pts',(0.497579909545564,-1.,-1.98767044752929));
#47155=CARTESIAN_POINT('Ctrl Pts',(0.497579909545564,1.,-1.98767044752929));
#47156=CARTESIAN_POINT('Ctrl Pts',(0.493843476541492,-1.,-1.9827665876182));
#47157=CARTESIAN_POINT('Ctrl Pts',(0.493843476541492,1.,-1.9827665876182));
#47158=CARTESIAN_POINT('Ctrl Pts',(0.490150627860955,-1.,-1.97783973019229));
#47159=CARTESIAN_POINT('Ctrl Pts',(0.490150627860955,1.,-1.97783973019229));
#47160=CARTESIAN_POINT('Ctrl Pts',(0.486502692907661,-1.,-1.97289186263272));
#47161=CARTESIAN_POINT('Ctrl Pts',(0.486502692907661,1.,-1.97289186263272));
#47162=CARTESIAN_POINT('Ctrl Pts',(0.482901662120686,-1.,-1.96792703422358));
#47163=CARTESIAN_POINT('Ctrl Pts',(0.482901662120686,1.,-1.96792703422358));
#47164=CARTESIAN_POINT('Ctrl Pts',(0.479349583074846,-1.,-1.96294933055938));
#47165=CARTESIAN_POINT('Ctrl Pts',(0.479349583074846,1.,-1.96294933055938));
#47166=CARTESIAN_POINT('Ctrl Pts',(0.475848034683171,-1.,-1.95796111148175));
#47167=CARTESIAN_POINT('Ctrl Pts',(0.475848034683171,1.,-1.95796111148175));
#47168=CARTESIAN_POINT('Ctrl Pts',(0.472397672264079,-1.,-1.95296148278136));
#47169=CARTESIAN_POINT('Ctrl Pts',(0.472397672264079,1.,-1.95296148278136));
#47170=CARTESIAN_POINT('Ctrl Pts',(0.468997482913158,-1.,-1.94794381136524));
#47171=CARTESIAN_POINT('Ctrl Pts',(0.468997482913158,1.,-1.94794381136524));
#47172=CARTESIAN_POINT('Ctrl Pts',(0.465645462026064,-1.,-1.94289794196205));
#47173=CARTESIAN_POINT('Ctrl Pts',(0.465645462026064,1.,-1.94289794196205));
#47174=CARTESIAN_POINT('Ctrl Pts',(0.462340031009087,-1.,-1.93781486640834));
#47175=CARTESIAN_POINT('Ctrl Pts',(0.462340031009087,1.,-1.93781486640834));
#47176=CARTESIAN_POINT('Ctrl Pts',(0.459081234547931,-1.,-1.93269066517936));
#47177=CARTESIAN_POINT('Ctrl Pts',(0.459081234547931,1.,-1.93269066517936));
#47178=CARTESIAN_POINT('Ctrl Pts',(0.455872005174335,-1.,-1.92753067150461));
#47179=CARTESIAN_POINT('Ctrl Pts',(0.455872005174335,1.,-1.92753067150461));
#47180=CARTESIAN_POINT('Ctrl Pts',(0.452719478359356,-1.,-1.9223538064847));
#47181=CARTESIAN_POINT('Ctrl Pts',(0.452719478359356,1.,-1.9223538064847));
#47182=CARTESIAN_POINT('Ctrl Pts',(0.449632260106572,-1.,-1.91718342555717));
#47183=CARTESIAN_POINT('Ctrl Pts',(0.449632260106572,1.,-1.91718342555717));
#47184=CARTESIAN_POINT('Ctrl Pts',(0.446617343485651,-1.,-1.91203699981095));
#47185=CARTESIAN_POINT('Ctrl Pts',(0.446617343485651,1.,-1.91203699981095));
#47186=CARTESIAN_POINT('Ctrl Pts',(0.44367755684917,-1.,-1.90691756144906));
#47187=CARTESIAN_POINT('Ctrl Pts',(0.44367755684917,1.,-1.90691756144906));
#47188=CARTESIAN_POINT('Ctrl Pts',(0.44080783370416,-1.,-1.90180124389137));
#47189=CARTESIAN_POINT('Ctrl Pts',(0.44080783370416,1.,-1.90180124389137));
#47190=CARTESIAN_POINT('Ctrl Pts',(0.437995003948443,-1.,-1.89663648956549));
#47191=CARTESIAN_POINT('Ctrl Pts',(0.437995003948443,1.,-1.89663648956549));
#47192=CARTESIAN_POINT('Ctrl Pts',(0.43522566096358,-1.,-1.89136993975585));
#47193=CARTESIAN_POINT('Ctrl Pts',(0.43522566096358,1.,-1.89136993975585));
#47194=CARTESIAN_POINT('Ctrl Pts',(0.432493038548833,-1.,-1.88596913666828));
#47195=CARTESIAN_POINT('Ctrl Pts',(0.432493038548833,1.,-1.88596913666828));
#47196=CARTESIAN_POINT('Ctrl Pts',(0.429803062482217,-1.,-1.88044229001779));
#47197=CARTESIAN_POINT('Ctrl Pts',(0.429803062482217,1.,-1.88044229001779));
#47198=CARTESIAN_POINT('Ctrl Pts',(0.427183828518743,-1.,-1.87486989291334));
#47199=CARTESIAN_POINT('Ctrl Pts',(0.427183828518743,1.,-1.87486989291334));
#47200=CARTESIAN_POINT('Ctrl Pts',(0.424678177290876,-1.,-1.8693780394412));
#47201=CARTESIAN_POINT('Ctrl Pts',(0.424678177290876,1.,-1.8693780394412));
#47202=CARTESIAN_POINT('Ctrl Pts',(0.422327307417884,-1.,-1.86408083333863));
#47203=CARTESIAN_POINT('Ctrl Pts',(0.422327307417884,1.,-1.86408083333863));
#47204=CARTESIAN_POINT('Ctrl Pts',(0.420157287975583,-1.,-1.8590328109667));
#47205=CARTESIAN_POINT('Ctrl Pts',(0.420157287975583,1.,-1.8590328109667));
#47206=CARTESIAN_POINT('Ctrl Pts',(0.418164129144045,-1.,-1.8541763285645));
#47207=CARTESIAN_POINT('Ctrl Pts',(0.418164129144045,1.,-1.8541763285645));
#47208=CARTESIAN_POINT('Ctrl Pts',(0.416300022039885,-1.,-1.84929312930314));
#47209=CARTESIAN_POINT('Ctrl Pts',(0.416300022039885,1.,-1.84929312930314));
#47210=CARTESIAN_POINT('Ctrl Pts',(0.414487438255542,-1.,-1.84405757074218));
#47211=CARTESIAN_POINT('Ctrl Pts',(0.414487438255542,1.,-1.84405757074218));
#47212=CARTESIAN_POINT('Ctrl Pts',(0.412633125322945,-1.,-1.8380895347617));
#47213=CARTESIAN_POINT('Ctrl Pts',(0.412633125322945,1.,-1.8380895347617));
#47214=CARTESIAN_POINT('Ctrl Pts',(0.410641256301276,-1.,-1.83100408895047));
#47215=CARTESIAN_POINT('Ctrl Pts',(0.410641256301276,1.,-1.83100408895047));
#47216=CARTESIAN_POINT('Ctrl Pts',(0.408428948106227,-1.,-1.82247022677562));
#47217=CARTESIAN_POINT('Ctrl Pts',(0.408428948106227,1.,-1.82247022677562));
#47218=CARTESIAN_POINT('Ctrl Pts',(0.405933518407175,-1.,-1.81223801812013));
#47219=CARTESIAN_POINT('Ctrl Pts',(0.405933518407175,1.,-1.81223801812013));
#47220=CARTESIAN_POINT('Ctrl Pts',(0.403107976163396,-1.,-1.80012077173238));
#47221=CARTESIAN_POINT('Ctrl Pts',(0.403107976163396,1.,-1.80012077173238));
#47222=CARTESIAN_POINT('Ctrl Pts',(0.399919403774155,-1.,-1.78598826343754));
#47223=CARTESIAN_POINT('Ctrl Pts',(0.399919403774155,1.,-1.78598826343754));
#47224=CARTESIAN_POINT('Ctrl Pts',(0.396346196110688,-1.,-1.76975560043442));
#47225=CARTESIAN_POINT('Ctrl Pts',(0.396346196110688,1.,-1.76975560043442));
#47226=CARTESIAN_POINT('Ctrl Pts',(0.392375812285395,-1.,-1.75137405310193));
#47227=CARTESIAN_POINT('Ctrl Pts',(0.392375812285395,1.,-1.75137405310193));
#47228=CARTESIAN_POINT('Ctrl Pts',(0.388877023502615,-1.,-1.73493170972829));
#47229=CARTESIAN_POINT('Ctrl Pts',(0.388877023502615,1.,-1.73493170972829));
#47230=CARTESIAN_POINT('Ctrl Pts',(0.386070790323281,-1.,-1.72162022244582));
#47231=CARTESIAN_POINT('Ctrl Pts',(0.386070790323281,1.,-1.72162022244582));
#47232=CARTESIAN_POINT('Ctrl Pts',(0.384119047314215,-1.,-1.71231062891398));
#47233=CARTESIAN_POINT('Ctrl Pts',(0.384119047314215,1.,-1.71231062891398));
#47234=CARTESIAN_POINT('Ctrl Pts',(0.383122945602004,-1.,-1.7075470150345));
#47235=CARTESIAN_POINT('Ctrl Pts',(0.383122945602004,1.,-1.7075470150345));
#47236=CARTESIAN_POINT('',(0.61342227326009,1.,-2.11275013067528));
#47237=CARTESIAN_POINT('Ctrl Pts',(0.61342227326009,1.,-2.11275013067528));
#47238=CARTESIAN_POINT('Ctrl Pts',(0.61246736556225,1.,-2.11187554260142));
#47239=CARTESIAN_POINT('Ctrl Pts',(0.610560911691113,1.,-2.11012443807661));
#47240=CARTESIAN_POINT('Ctrl Pts',(0.607711315456826,1.,-2.10749199615859));
#47241=CARTESIAN_POINT('Ctrl Pts',(0.603932030738212,1.,-2.10397049887709));
#47242=CARTESIAN_POINT('Ctrl Pts',(0.599241616422144,1.,-2.09954930865331));
#47243=CARTESIAN_POINT('Ctrl Pts',(0.594585006052823,1.,-2.09510876220501));
#47244=CARTESIAN_POINT('Ctrl Pts',(0.589962365403189,1.,-2.09064881812053));
#47245=CARTESIAN_POINT('Ctrl Pts',(0.585373918990895,1.,-2.086169437277));
#47246=CARTESIAN_POINT('Ctrl Pts',(0.580819952107256,1.,-2.08167059018138));
#47247=CARTESIAN_POINT('Ctrl Pts',(0.576300797416274,1.,-2.07715226767361));
#47248=CARTESIAN_POINT('Ctrl Pts',(0.571816823242411,1.,-2.07261449292758));
#47249=CARTESIAN_POINT('Ctrl Pts',(0.567368421181229,1.,-2.06805732997383));
#47250=CARTESIAN_POINT('Ctrl Pts',(0.562955993082574,1.,-2.06348090160697));
#47251=CARTESIAN_POINT('Ctrl Pts',(0.558579940185467,1.,-2.05888537756571));
#47252=CARTESIAN_POINT('Ctrl Pts',(0.554240657464109,1.,-2.05427091604482));
#47253=CARTESIAN_POINT('Ctrl Pts',(0.549938525150342,1.,-2.04963761077974));
#47254=CARTESIAN_POINT('Ctrl Pts',(0.545673903817348,1.,-2.0449854471456));
#47255=CARTESIAN_POINT('Ctrl Pts',(0.54144712061552,1.,-2.0403142269048));
#47256=CARTESIAN_POINT('Ctrl Pts',(0.537258489833134,1.,-2.03562362953993));
#47257=CARTESIAN_POINT('Ctrl Pts',(0.533108355132905,1.,-2.03091336214401));
#47258=CARTESIAN_POINT('Ctrl Pts',(0.52899712724191,1.,-2.02618329083289));
#47259=CARTESIAN_POINT('Ctrl Pts',(0.524925318333518,1.,-2.02143356304712));
#47260=CARTESIAN_POINT('Ctrl Pts',(0.520893590399428,1.,-2.01666477917306));
#47261=CARTESIAN_POINT('Ctrl Pts',(0.516902681728733,1.,-2.01187773939257));
#47262=CARTESIAN_POINT('Ctrl Pts',(0.512953306961813,1.,-2.00707309946955));
#47263=CARTESIAN_POINT('Ctrl Pts',(0.509046069886152,1.,-2.00225107134733));
#47264=CARTESIAN_POINT('Ctrl Pts',(0.505181361323011,1.,-1.99741107463567));
#47265=CARTESIAN_POINT('Ctrl Pts',(0.501359287727129,1.,-1.9925514912615));
#47266=CARTESIAN_POINT('Ctrl Pts',(0.497579909545564,1.,-1.98767044752929));
#47267=CARTESIAN_POINT('Ctrl Pts',(0.493843476541492,1.,-1.9827665876182));
#47268=CARTESIAN_POINT('Ctrl Pts',(0.490150627860955,1.,-1.97783973019229));
#47269=CARTESIAN_POINT('Ctrl Pts',(0.486502692907661,1.,-1.97289186263272));
#47270=CARTESIAN_POINT('Ctrl Pts',(0.482901662120686,1.,-1.96792703422358));
#47271=CARTESIAN_POINT('Ctrl Pts',(0.479349583074846,1.,-1.96294933055938));
#47272=CARTESIAN_POINT('Ctrl Pts',(0.475848034683171,1.,-1.95796111148175));
#47273=CARTESIAN_POINT('Ctrl Pts',(0.472397672264079,1.,-1.95296148278136));
#47274=CARTESIAN_POINT('Ctrl Pts',(0.468997482913158,1.,-1.94794381136524));
#47275=CARTESIAN_POINT('Ctrl Pts',(0.465645462026064,1.,-1.94289794196205));
#47276=CARTESIAN_POINT('Ctrl Pts',(0.462340031009087,1.,-1.93781486640834));
#47277=CARTESIAN_POINT('Ctrl Pts',(0.459081234547931,1.,-1.93269066517936));
#47278=CARTESIAN_POINT('Ctrl Pts',(0.455872005174335,1.,-1.92753067150461));
#47279=CARTESIAN_POINT('Ctrl Pts',(0.452719478359356,1.,-1.9223538064847));
#47280=CARTESIAN_POINT('Ctrl Pts',(0.449632260106572,1.,-1.91718342555717));
#47281=CARTESIAN_POINT('Ctrl Pts',(0.446617343485651,1.,-1.91203699981095));
#47282=CARTESIAN_POINT('Ctrl Pts',(0.44367755684917,1.,-1.90691756144906));
#47283=CARTESIAN_POINT('Ctrl Pts',(0.44080783370416,1.,-1.90180124389137));
#47284=CARTESIAN_POINT('Ctrl Pts',(0.437995003948443,1.,-1.89663648956549));
#47285=CARTESIAN_POINT('Ctrl Pts',(0.43522566096358,1.,-1.89136993975585));
#47286=CARTESIAN_POINT('Ctrl Pts',(0.432493038548833,1.,-1.88596913666828));
#47287=CARTESIAN_POINT('Ctrl Pts',(0.429803062482217,1.,-1.88044229001779));
#47288=CARTESIAN_POINT('Ctrl Pts',(0.427183828518743,1.,-1.87486989291334));
#47289=CARTESIAN_POINT('Ctrl Pts',(0.424678177290876,1.,-1.8693780394412));
#47290=CARTESIAN_POINT('Ctrl Pts',(0.422327307417884,1.,-1.86408083333863));
#47291=CARTESIAN_POINT('Ctrl Pts',(0.420157287975583,1.,-1.8590328109667));
#47292=CARTESIAN_POINT('Ctrl Pts',(0.418164129144045,1.,-1.8541763285645));
#47293=CARTESIAN_POINT('Ctrl Pts',(0.416300022039885,1.,-1.84929312930314));
#47294=CARTESIAN_POINT('Ctrl Pts',(0.414487438255542,1.,-1.84405757074218));
#47295=CARTESIAN_POINT('Ctrl Pts',(0.412633125322945,1.,-1.8380895347617));
#47296=CARTESIAN_POINT('Ctrl Pts',(0.410641256301276,1.,-1.83100408895047));
#47297=CARTESIAN_POINT('Ctrl Pts',(0.408428948106227,1.,-1.82247022677562));
#47298=CARTESIAN_POINT('Ctrl Pts',(0.405933518407175,1.,-1.81223801812013));
#47299=CARTESIAN_POINT('Ctrl Pts',(0.403107976163396,1.,-1.80012077173238));
#47300=CARTESIAN_POINT('Ctrl Pts',(0.399919403774155,1.,-1.78598826343754));
#47301=CARTESIAN_POINT('Ctrl Pts',(0.396346196110688,1.,-1.76975560043442));
#47302=CARTESIAN_POINT('Ctrl Pts',(0.392375812285395,1.,-1.75137405310193));
#47303=CARTESIAN_POINT('Ctrl Pts',(0.388877023502615,1.,-1.73493170972829));
#47304=CARTESIAN_POINT('Ctrl Pts',(0.386070790323281,1.,-1.72162022244582));
#47305=CARTESIAN_POINT('Ctrl Pts',(0.384119047314215,1.,-1.71231062891398));
#47306=CARTESIAN_POINT('Ctrl Pts',(0.383122945602004,1.,-1.7075470150345));
#47307=CARTESIAN_POINT('',(0.61342227326009,0.,-2.11275013067528));
#47308=CARTESIAN_POINT('Origin',(0.745574324794401,0.,-2.0698113262342));
#47309=CARTESIAN_POINT('',(0.745574324794401,1.,-2.0698113262342));
#47310=CARTESIAN_POINT('',(0.61342227326009,1.,-2.11275013067528));
#47311=CARTESIAN_POINT('',(0.745574324794401,0.,-2.0698113262342));
#47312=CARTESIAN_POINT('Ctrl Pts',(0.693717979106306,-1.,-1.60662857109684));
#47313=CARTESIAN_POINT('Ctrl Pts',(0.693717979106306,1.,-1.60662857109684));
#47314=CARTESIAN_POINT('Ctrl Pts',(0.695712097881194,-1.,-1.61106790958151));
#47315=CARTESIAN_POINT('Ctrl Pts',(0.695712097881194,1.,-1.61106790958151));
#47316=CARTESIAN_POINT('Ctrl Pts',(0.699605146405088,-1.,-1.61974673472612));
#47317=CARTESIAN_POINT('Ctrl Pts',(0.699605146405088,1.,-1.61974673472612));
#47318=CARTESIAN_POINT('Ctrl Pts',(0.705159151988319,-1.,-1.63216541664676));
#47319=CARTESIAN_POINT('Ctrl Pts',(0.705159151988319,1.,-1.63216541664676));
#47320=CARTESIAN_POINT('Ctrl Pts',(0.711993139355394,-1.,-1.64752408832016));
#47321=CARTESIAN_POINT('Ctrl Pts',(0.711993139355394,1.,-1.64752408832016));
#47322=CARTESIAN_POINT('Ctrl Pts',(0.719585433804282,-1.,-1.6647288055568));
#47323=CARTESIAN_POINT('Ctrl Pts',(0.719585433804282,1.,-1.6647288055568));
#47324=CARTESIAN_POINT('Ctrl Pts',(0.726235967997433,-1.,-1.67996158455503));
#47325=CARTESIAN_POINT('Ctrl Pts',(0.726235967997433,1.,-1.67996158455503));
#47326=CARTESIAN_POINT('Ctrl Pts',(0.731963238697195,-1.,-1.69326921975743));
#47327=CARTESIAN_POINT('Ctrl Pts',(0.731963238697195,1.,-1.69326921975743));
#47328=CARTESIAN_POINT('Ctrl Pts',(0.736799665724771,-1.,-1.70473309006121));
#47329=CARTESIAN_POINT('Ctrl Pts',(0.736799665724771,1.,-1.70473309006121));
#47330=CARTESIAN_POINT('Ctrl Pts',(0.740795162032087,-1.,-1.71447789751927));
#47331=CARTESIAN_POINT('Ctrl Pts',(0.740795162032087,1.,-1.71447789751927));
#47332=CARTESIAN_POINT('Ctrl Pts',(0.744021445433764,-1.,-1.7226822991693));
#47333=CARTESIAN_POINT('Ctrl Pts',(0.744021445433764,1.,-1.7226822991693));
#47334=CARTESIAN_POINT('Ctrl Pts',(0.746574710096436,-1.,-1.72958533647399));
#47335=CARTESIAN_POINT('Ctrl Pts',(0.746574710096436,1.,-1.72958533647399));
#47336=CARTESIAN_POINT('Ctrl Pts',(0.748582462954854,-1.,-1.73550351679848));
#47337=CARTESIAN_POINT('Ctrl Pts',(0.748582462954854,1.,-1.73550351679848));
#47338=CARTESIAN_POINT('Ctrl Pts',(0.75019343597954,-1.,-1.74080458266705));
#47339=CARTESIAN_POINT('Ctrl Pts',(0.75019343597954,1.,-1.74080458266705));
#47340=CARTESIAN_POINT('Ctrl Pts',(0.751555614163629,-1.,-1.74585086852298));
#47341=CARTESIAN_POINT('Ctrl Pts',(0.751555614163629,1.,-1.74585086852298));
#47342=CARTESIAN_POINT('Ctrl Pts',(0.752797683531377,-1.,-1.75095139468809));
#47343=CARTESIAN_POINT('Ctrl Pts',(0.752797683531377,1.,-1.75095139468809));
#47344=CARTESIAN_POINT('Ctrl Pts',(0.75400925402848,-1.,-1.75631083600175));
#47345=CARTESIAN_POINT('Ctrl Pts',(0.75400925402848,1.,-1.75631083600175));
#47346=CARTESIAN_POINT('Ctrl Pts',(0.755220979975262,-1.,-1.7619781724032));
#47347=CARTESIAN_POINT('Ctrl Pts',(0.755220979975262,1.,-1.7619781724032));
#47348=CARTESIAN_POINT('Ctrl Pts',(0.756421896028403,-1.,-1.76789396003141));
#47349=CARTESIAN_POINT('Ctrl Pts',(0.756421896028403,1.,-1.76789396003141));
#47350=CARTESIAN_POINT('Ctrl Pts',(0.757578264077238,-1.,-1.77394167108342));
#47351=CARTESIAN_POINT('Ctrl Pts',(0.757578264077238,1.,-1.77394167108342));
#47352=CARTESIAN_POINT('Ctrl Pts',(0.75865062667738,-1.,-1.77999411220912));
#47353=CARTESIAN_POINT('Ctrl Pts',(0.75865062667738,1.,-1.77999411220912));
#47354=CARTESIAN_POINT('Ctrl Pts',(0.759614401109868,-1.,-1.78596964884527));
#47355=CARTESIAN_POINT('Ctrl Pts',(0.759614401109868,1.,-1.78596964884527));
#47356=CARTESIAN_POINT('Ctrl Pts',(0.760469555880425,-1.,-1.79185815610802));
#47357=CARTESIAN_POINT('Ctrl Pts',(0.760469555880425,1.,-1.79185815610802));
#47358=CARTESIAN_POINT('Ctrl Pts',(0.761229695230359,-1.,-1.79768986997735));
#47359=CARTESIAN_POINT('Ctrl Pts',(0.761229695230359,1.,-1.79768986997735));
#47360=CARTESIAN_POINT('Ctrl Pts',(0.761915336443515,-1.,-1.80351583877334));
#47361=CARTESIAN_POINT('Ctrl Pts',(0.761915336443515,1.,-1.80351583877334));
#47362=CARTESIAN_POINT('Ctrl Pts',(0.762546129464036,-1.,-1.80938551463989));
#47363=CARTESIAN_POINT('Ctrl Pts',(0.762546129464036,1.,-1.80938551463989));
#47364=CARTESIAN_POINT('Ctrl Pts',(0.763132003836783,-1.,-1.81532118405566));
#47365=CARTESIAN_POINT('Ctrl Pts',(0.763132003836783,1.,-1.81532118405566));
#47366=CARTESIAN_POINT('Ctrl Pts',(0.763673465462854,-1.,-1.82131873145297));
#47367=CARTESIAN_POINT('Ctrl Pts',(0.763673465462854,1.,-1.82131873145297));
#47368=CARTESIAN_POINT('Ctrl Pts',(0.764165902606055,-1.,-1.8273599120008));
#47369=CARTESIAN_POINT('Ctrl Pts',(0.764165902606055,1.,-1.8273599120008));
#47370=CARTESIAN_POINT('Ctrl Pts',(0.764602549687845,-1.,-1.8334207722714));
#47371=CARTESIAN_POINT('Ctrl Pts',(0.764602549687845,1.,-1.8334207722714));
#47372=CARTESIAN_POINT('Ctrl Pts',(0.764978057881687,-1.,-1.83948181064823));
#47373=CARTESIAN_POINT('Ctrl Pts',(0.764978057881687,1.,-1.83948181064823));
#47374=CARTESIAN_POINT('Ctrl Pts',(0.765291664861971,-1.,-1.84553698875911));
#47375=CARTESIAN_POINT('Ctrl Pts',(0.765291664861971,1.,-1.84553698875911));
#47376=CARTESIAN_POINT('Ctrl Pts',(0.765545710619023,-1.,-1.85158945130054));
#47377=CARTESIAN_POINT('Ctrl Pts',(0.765545710619023,1.,-1.85158945130054));
#47378=CARTESIAN_POINT('Ctrl Pts',(0.765744212909305,-1.,-1.85764741390391));
#47379=CARTESIAN_POINT('Ctrl Pts',(0.765744212909305,1.,-1.85764741390391));
#47380=CARTESIAN_POINT('Ctrl Pts',(0.765891519092557,-1.,-1.86372027063315));
#47381=CARTESIAN_POINT('Ctrl Pts',(0.765891519092557,1.,-1.86372027063315));
#47382=CARTESIAN_POINT('Ctrl Pts',(0.765990708546111,-1.,-1.86981398314345));
#47383=CARTESIAN_POINT('Ctrl Pts',(0.765990708546111,1.,-1.86981398314345));
#47384=CARTESIAN_POINT('Ctrl Pts',(0.766042837036759,-1.,-1.87592888967886));
#47385=CARTESIAN_POINT('Ctrl Pts',(0.766042837036759,1.,-1.87592888967886));
#47386=CARTESIAN_POINT('Ctrl Pts',(0.766047794851868,-1.,-1.88206215302561));
#47387=CARTESIAN_POINT('Ctrl Pts',(0.766047794851868,1.,-1.88206215302561));
#47388=CARTESIAN_POINT('Ctrl Pts',(0.76600483706209,-1.,-1.88820926433409));
#47389=CARTESIAN_POINT('Ctrl Pts',(0.76600483706209,1.,-1.88820926433409));
#47390=CARTESIAN_POINT('Ctrl Pts',(0.765913193856979,-1.,-1.89436577771389));
#47391=CARTESIAN_POINT('Ctrl Pts',(0.765913193856979,1.,-1.89436577771389));
#47392=CARTESIAN_POINT('Ctrl Pts',(0.765772772593395,-1.,-1.90052930393599));
#47393=CARTESIAN_POINT('Ctrl Pts',(0.765772772593395,1.,-1.90052930393599));
#47394=CARTESIAN_POINT('Ctrl Pts',(0.765584196937936,-1.,-1.90669961402362));
#47395=CARTESIAN_POINT('Ctrl Pts',(0.765584196937936,1.,-1.90669961402362));
#47396=CARTESIAN_POINT('Ctrl Pts',(0.765348465884739,-1.,-1.91287765805174));
#47397=CARTESIAN_POINT('Ctrl Pts',(0.765348465884739,1.,-1.91287765805174));
#47398=CARTESIAN_POINT('Ctrl Pts',(0.765066729667095,-1.,-1.91906491634197));
#47399=CARTESIAN_POINT('Ctrl Pts',(0.765066729667095,1.,-1.91906491634197));
#47400=CARTESIAN_POINT('Ctrl Pts',(0.764740025488189,-1.,-1.92526263537041));
#47401=CARTESIAN_POINT('Ctrl Pts',(0.764740025488189,1.,-1.92526263537041));
#47402=CARTESIAN_POINT('Ctrl Pts',(0.764369010673889,-1.,-1.93147105496367));
#47403=CARTESIAN_POINT('Ctrl Pts',(0.764369010673889,1.,-1.93147105496367));
#47404=CARTESIAN_POINT('Ctrl Pts',(0.763954049121393,-1.,-1.93768964875867));
#47405=CARTESIAN_POINT('Ctrl Pts',(0.763954049121393,1.,-1.93768964875867));
#47406=CARTESIAN_POINT('Ctrl Pts',(0.76349533353858,-1.,-1.94391746617626));
#47407=CARTESIAN_POINT('Ctrl Pts',(0.76349533353858,1.,-1.94391746617626));
#47408=CARTESIAN_POINT('Ctrl Pts',(0.762992990878774,-1.,-1.95015342590025));
#47409=CARTESIAN_POINT('Ctrl Pts',(0.762992990878774,1.,-1.95015342590025));
#47410=CARTESIAN_POINT('Ctrl Pts',(0.762447203806263,-1.,-1.95639665309893));
#47411=CARTESIAN_POINT('Ctrl Pts',(0.762447203806263,1.,-1.95639665309893));
#47412=CARTESIAN_POINT('Ctrl Pts',(0.761858300014575,-1.,-1.96264672744229));
#47413=CARTESIAN_POINT('Ctrl Pts',(0.761858300014575,1.,-1.96264672744229));
#47414=CARTESIAN_POINT('Ctrl Pts',(0.761226690483986,-1.,-1.96890351582545));
#47415=CARTESIAN_POINT('Ctrl Pts',(0.761226690483986,1.,-1.96890351582545));
#47416=CARTESIAN_POINT('Ctrl Pts',(0.760552825409855,-1.,-1.97516705321521));
#47417=CARTESIAN_POINT('Ctrl Pts',(0.760552825409855,1.,-1.97516705321521));
#47418=CARTESIAN_POINT('Ctrl Pts',(0.759837147452135,-1.,-1.98143741418156));
#47419=CARTESIAN_POINT('Ctrl Pts',(0.759837147452135,1.,-1.98143741418156));
#47420=CARTESIAN_POINT('Ctrl Pts',(0.759080037802242,-1.,-1.98771456680806));
#47421=CARTESIAN_POINT('Ctrl Pts',(0.759080037802242,1.,-1.98771456680806));
#47422=CARTESIAN_POINT('Ctrl Pts',(0.758281796766377,-1.,-1.9939983109871));
#47423=CARTESIAN_POINT('Ctrl Pts',(0.758281796766377,1.,-1.9939983109871));
#47424=CARTESIAN_POINT('Ctrl Pts',(0.757442676862341,-1.,-2.00028834739072));
#47425=CARTESIAN_POINT('Ctrl Pts',(0.757442676862341,1.,-2.00028834739072));
#47426=CARTESIAN_POINT('Ctrl Pts',(0.756562904646496,-1.,-2.00658431587682));
#47427=CARTESIAN_POINT('Ctrl Pts',(0.756562904646496,1.,-2.00658431587682));
#47428=CARTESIAN_POINT('Ctrl Pts',(0.7556427049581,-1.,-2.01288584328149));
#47429=CARTESIAN_POINT('Ctrl Pts',(0.7556427049581,1.,-2.01288584328149));
#47430=CARTESIAN_POINT('Ctrl Pts',(0.75468233072352,-1.,-2.01919259406003));
#47431=CARTESIAN_POINT('Ctrl Pts',(0.75468233072352,1.,-2.01919259406003));
#47432=CARTESIAN_POINT('Ctrl Pts',(0.753682061113765,-1.,-2.02550428623587));
#47433=CARTESIAN_POINT('Ctrl Pts',(0.753682061113765,1.,-2.02550428623587));
#47434=CARTESIAN_POINT('Ctrl Pts',(0.752642180488104,-1.,-2.03182068456467));
#47435=CARTESIAN_POINT('Ctrl Pts',(0.752642180488104,1.,-2.03182068456467));
#47436=CARTESIAN_POINT('Ctrl Pts',(0.751562963361383,-1.,-2.03814160092173));
#47437=CARTESIAN_POINT('Ctrl Pts',(0.751562963361383,1.,-2.03814160092173));
#47438=CARTESIAN_POINT('Ctrl Pts',(0.750444657874758,-1.,-2.04446689147754));
#47439=CARTESIAN_POINT('Ctrl Pts',(0.750444657874758,1.,-2.04446689147754));
#47440=CARTESIAN_POINT('Ctrl Pts',(0.749287468663053,-1.,-2.05079645591606));
#47441=CARTESIAN_POINT('Ctrl Pts',(0.749287468663053,1.,-2.05079645591606));
#47442=CARTESIAN_POINT('Ctrl Pts',(0.748091554181101,-1.,-2.05713023030263));
#47443=CARTESIAN_POINT('Ctrl Pts',(0.748091554181101,1.,-2.05713023030263));
#47444=CARTESIAN_POINT('Ctrl Pts',(0.747103932785504,-1.,-2.06220058927162));
#47445=CARTESIAN_POINT('Ctrl Pts',(0.747103932785504,1.,-2.06220058927162));
#47446=CARTESIAN_POINT('Ctrl Pts',(0.746345871542695,-1.,-2.06600523016401));
#47447=CARTESIAN_POINT('Ctrl Pts',(0.746345871542695,1.,-2.06600523016401));
#47448=CARTESIAN_POINT('Ctrl Pts',(0.74583279137781,-1.,-2.06854248895575));
#47449=CARTESIAN_POINT('Ctrl Pts',(0.74583279137781,1.,-2.06854248895575));
#47450=CARTESIAN_POINT('Ctrl Pts',(0.745574324794401,-1.,-2.0698113262342));
#47451=CARTESIAN_POINT('Ctrl Pts',(0.745574324794401,1.,-2.0698113262342));
#47452=CARTESIAN_POINT('',(0.693717979106306,1.,-1.60662857109684));
#47453=CARTESIAN_POINT('Ctrl Pts',(0.693717979106306,1.,-1.60662857109684));
#47454=CARTESIAN_POINT('Ctrl Pts',(0.695712097881194,1.,-1.61106790958151));
#47455=CARTESIAN_POINT('Ctrl Pts',(0.699605146405088,1.,-1.61974673472612));
#47456=CARTESIAN_POINT('Ctrl Pts',(0.705159151988319,1.,-1.63216541664676));
#47457=CARTESIAN_POINT('Ctrl Pts',(0.711993139355394,1.,-1.64752408832016));
#47458=CARTESIAN_POINT('Ctrl Pts',(0.719585433804282,1.,-1.6647288055568));
#47459=CARTESIAN_POINT('Ctrl Pts',(0.726235967997433,1.,-1.67996158455503));
#47460=CARTESIAN_POINT('Ctrl Pts',(0.731963238697195,1.,-1.69326921975743));
#47461=CARTESIAN_POINT('Ctrl Pts',(0.736799665724771,1.,-1.70473309006121));
#47462=CARTESIAN_POINT('Ctrl Pts',(0.740795162032087,1.,-1.71447789751927));
#47463=CARTESIAN_POINT('Ctrl Pts',(0.744021445433764,1.,-1.7226822991693));
#47464=CARTESIAN_POINT('Ctrl Pts',(0.746574710096436,1.,-1.72958533647399));
#47465=CARTESIAN_POINT('Ctrl Pts',(0.748582462954854,1.,-1.73550351679848));
#47466=CARTESIAN_POINT('Ctrl Pts',(0.75019343597954,1.,-1.74080458266705));
#47467=CARTESIAN_POINT('Ctrl Pts',(0.751555614163629,1.,-1.74585086852298));
#47468=CARTESIAN_POINT('Ctrl Pts',(0.752797683531377,1.,-1.75095139468809));
#47469=CARTESIAN_POINT('Ctrl Pts',(0.75400925402848,1.,-1.75631083600175));
#47470=CARTESIAN_POINT('Ctrl Pts',(0.755220979975262,1.,-1.7619781724032));
#47471=CARTESIAN_POINT('Ctrl Pts',(0.756421896028403,1.,-1.76789396003141));
#47472=CARTESIAN_POINT('Ctrl Pts',(0.757578264077238,1.,-1.77394167108342));
#47473=CARTESIAN_POINT('Ctrl Pts',(0.75865062667738,1.,-1.77999411220912));
#47474=CARTESIAN_POINT('Ctrl Pts',(0.759614401109868,1.,-1.78596964884527));
#47475=CARTESIAN_POINT('Ctrl Pts',(0.760469555880425,1.,-1.79185815610802));
#47476=CARTESIAN_POINT('Ctrl Pts',(0.761229695230359,1.,-1.79768986997735));
#47477=CARTESIAN_POINT('Ctrl Pts',(0.761915336443515,1.,-1.80351583877334));
#47478=CARTESIAN_POINT('Ctrl Pts',(0.762546129464036,1.,-1.80938551463989));
#47479=CARTESIAN_POINT('Ctrl Pts',(0.763132003836783,1.,-1.81532118405566));
#47480=CARTESIAN_POINT('Ctrl Pts',(0.763673465462854,1.,-1.82131873145297));
#47481=CARTESIAN_POINT('Ctrl Pts',(0.764165902606055,1.,-1.8273599120008));
#47482=CARTESIAN_POINT('Ctrl Pts',(0.764602549687845,1.,-1.8334207722714));
#47483=CARTESIAN_POINT('Ctrl Pts',(0.764978057881687,1.,-1.83948181064823));
#47484=CARTESIAN_POINT('Ctrl Pts',(0.765291664861971,1.,-1.84553698875911));
#47485=CARTESIAN_POINT('Ctrl Pts',(0.765545710619023,1.,-1.85158945130054));
#47486=CARTESIAN_POINT('Ctrl Pts',(0.765744212909305,1.,-1.85764741390391));
#47487=CARTESIAN_POINT('Ctrl Pts',(0.765891519092557,1.,-1.86372027063315));
#47488=CARTESIAN_POINT('Ctrl Pts',(0.765990708546111,1.,-1.86981398314345));
#47489=CARTESIAN_POINT('Ctrl Pts',(0.766042837036759,1.,-1.87592888967886));
#47490=CARTESIAN_POINT('Ctrl Pts',(0.766047794851868,1.,-1.88206215302561));
#47491=CARTESIAN_POINT('Ctrl Pts',(0.76600483706209,1.,-1.88820926433409));
#47492=CARTESIAN_POINT('Ctrl Pts',(0.765913193856979,1.,-1.89436577771389));
#47493=CARTESIAN_POINT('Ctrl Pts',(0.765772772593395,1.,-1.90052930393599));
#47494=CARTESIAN_POINT('Ctrl Pts',(0.765584196937936,1.,-1.90669961402362));
#47495=CARTESIAN_POINT('Ctrl Pts',(0.765348465884739,1.,-1.91287765805174));
#47496=CARTESIAN_POINT('Ctrl Pts',(0.765066729667095,1.,-1.91906491634197));
#47497=CARTESIAN_POINT('Ctrl Pts',(0.764740025488189,1.,-1.92526263537041));
#47498=CARTESIAN_POINT('Ctrl Pts',(0.764369010673889,1.,-1.93147105496367));
#47499=CARTESIAN_POINT('Ctrl Pts',(0.763954049121393,1.,-1.93768964875867));
#47500=CARTESIAN_POINT('Ctrl Pts',(0.76349533353858,1.,-1.94391746617626));
#47501=CARTESIAN_POINT('Ctrl Pts',(0.762992990878774,1.,-1.95015342590025));
#47502=CARTESIAN_POINT('Ctrl Pts',(0.762447203806263,1.,-1.95639665309893));
#47503=CARTESIAN_POINT('Ctrl Pts',(0.761858300014575,1.,-1.96264672744229));
#47504=CARTESIAN_POINT('Ctrl Pts',(0.761226690483986,1.,-1.96890351582545));
#47505=CARTESIAN_POINT('Ctrl Pts',(0.760552825409855,1.,-1.97516705321521));
#47506=CARTESIAN_POINT('Ctrl Pts',(0.759837147452135,1.,-1.98143741418156));
#47507=CARTESIAN_POINT('Ctrl Pts',(0.759080037802242,1.,-1.98771456680806));
#47508=CARTESIAN_POINT('Ctrl Pts',(0.758281796766377,1.,-1.9939983109871));
#47509=CARTESIAN_POINT('Ctrl Pts',(0.757442676862341,1.,-2.00028834739072));
#47510=CARTESIAN_POINT('Ctrl Pts',(0.756562904646496,1.,-2.00658431587682));
#47511=CARTESIAN_POINT('Ctrl Pts',(0.7556427049581,1.,-2.01288584328149));
#47512=CARTESIAN_POINT('Ctrl Pts',(0.75468233072352,1.,-2.01919259406003));
#47513=CARTESIAN_POINT('Ctrl Pts',(0.753682061113765,1.,-2.02550428623587));
#47514=CARTESIAN_POINT('Ctrl Pts',(0.752642180488104,1.,-2.03182068456467));
#47515=CARTESIAN_POINT('Ctrl Pts',(0.751562963361383,1.,-2.03814160092173));
#47516=CARTESIAN_POINT('Ctrl Pts',(0.750444657874758,1.,-2.04446689147754));
#47517=CARTESIAN_POINT('Ctrl Pts',(0.749287468663053,1.,-2.05079645591606));
#47518=CARTESIAN_POINT('Ctrl Pts',(0.748091554181101,1.,-2.05713023030263));
#47519=CARTESIAN_POINT('Ctrl Pts',(0.747103932785504,1.,-2.06220058927162));
#47520=CARTESIAN_POINT('Ctrl Pts',(0.746345871542695,1.,-2.06600523016401));
#47521=CARTESIAN_POINT('Ctrl Pts',(0.74583279137781,1.,-2.06854248895575));
#47522=CARTESIAN_POINT('Ctrl Pts',(0.745574324794401,1.,-2.0698113262342));
#47523=CARTESIAN_POINT('',(0.693717979106306,0.,-1.60662857109684));
#47524=CARTESIAN_POINT('Origin',(0.,0.,0.));
#47525=CARTESIAN_POINT('',(0.892032620296855,1.,-1.5055822144029));
#47526=CARTESIAN_POINT('Origin',(0.,1.,0.));
#47527=CARTESIAN_POINT('',(0.892032620296855,0.,-1.5055822144029));
#47528=CARTESIAN_POINT('Ctrl Pts',(1.23627494547115,-1.,-1.81978687191668));
#47529=CARTESIAN_POINT('Ctrl Pts',(1.23627494547115,1.,-1.81978687191668));
#47530=CARTESIAN_POINT('Ctrl Pts',(1.23509651170476,-1.,-1.81925017193666));
#47531=CARTESIAN_POINT('Ctrl Pts',(1.23509651170476,1.,-1.81925017193666));
#47532=CARTESIAN_POINT('Ctrl Pts',(1.2327422452705,-1.,-1.81817389921279));
#47533=CARTESIAN_POINT('Ctrl Pts',(1.2327422452705,1.,-1.81817389921279));
#47534=CARTESIAN_POINT('Ctrl Pts',(1.2292186489137,-1.,-1.8165508718364));
#47535=CARTESIAN_POINT('Ctrl Pts',(1.2292186489137,1.,-1.8165508718364));
#47536=CARTESIAN_POINT('Ctrl Pts',(1.2245361330495,-1.,-1.81436959210434));
#47537=CARTESIAN_POINT('Ctrl Pts',(1.2245361330495,1.,-1.81436959210434));
#47538=CARTESIAN_POINT('Ctrl Pts',(1.21870906103557,-1.,-1.81161420806656));
#47539=CARTESIAN_POINT('Ctrl Pts',(1.21870906103557,1.,-1.81161420806656));
#47540=CARTESIAN_POINT('Ctrl Pts',(1.21290815708314,-1.,-1.80882996917129));
#47541=CARTESIAN_POINT('Ctrl Pts',(1.21290815708314,1.,-1.80882996917129));
#47542=CARTESIAN_POINT('Ctrl Pts',(1.20713356605475,-1.,-1.80601678480707));
#47543=CARTESIAN_POINT('Ctrl Pts',(1.20713356605475,1.,-1.80601678480707));
#47544=CARTESIAN_POINT('Ctrl Pts',(1.20138548938974,-1.,-1.80317454838603));
#47545=CARTESIAN_POINT('Ctrl Pts',(1.20138548938974,1.,-1.80317454838603));
#47546=CARTESIAN_POINT('Ctrl Pts',(1.19566418930242,-1.,-1.80030314369879));
#47547=CARTESIAN_POINT('Ctrl Pts',(1.19566418930242,1.,-1.80030314369879));
#47548=CARTESIAN_POINT('Ctrl Pts',(1.18996997934445,-1.,-1.79740245923478));
#47549=CARTESIAN_POINT('Ctrl Pts',(1.18996997934445,1.,-1.79740245923478));
#47550=CARTESIAN_POINT('Ctrl Pts',(1.18430321697432,-1.,-1.79447240321515));
#47551=CARTESIAN_POINT('Ctrl Pts',(1.18430321697432,1.,-1.79447240321515));
#47552=CARTESIAN_POINT('Ctrl Pts',(1.17866429440809,-1.,-1.79151291552689));
#47553=CARTESIAN_POINT('Ctrl Pts',(1.17866429440809,1.,-1.79151291552689));
#47554=CARTESIAN_POINT('Ctrl Pts',(1.17305363177328,-1.,-1.78852398877617));
#47555=CARTESIAN_POINT('Ctrl Pts',(1.17305363177328,1.,-1.78852398877617));
#47556=CARTESIAN_POINT('Ctrl Pts',(1.16747166312303,-1.,-1.78550566040443));
#47557=CARTESIAN_POINT('Ctrl Pts',(1.16747166312303,1.,-1.78550566040443));
#47558=CARTESIAN_POINT('Ctrl Pts',(1.16191881298499,-1.,-1.78245795881009));
#47559=CARTESIAN_POINT('Ctrl Pts',(1.16191881298499,1.,-1.78245795881009));
#47560=CARTESIAN_POINT('Ctrl Pts',(1.15639547194698,-1.,-1.77938085564275));
#47561=CARTESIAN_POINT('Ctrl Pts',(1.15639547194698,1.,-1.77938085564275));
#47562=CARTESIAN_POINT('Ctrl Pts',(1.15090197841514,-1.,-1.7762742255701));
#47563=CARTESIAN_POINT('Ctrl Pts',(1.15090197841514,1.,-1.7762742255701));
#47564=CARTESIAN_POINT('Ctrl Pts',(1.1454385822692,-1.,-1.77313777896194));
#47565=CARTESIAN_POINT('Ctrl Pts',(1.1454385822692,1.,-1.77313777896194));
#47566=CARTESIAN_POINT('Ctrl Pts',(1.14000548336975,-1.,-1.76997111386769));
#47567=CARTESIAN_POINT('Ctrl Pts',(1.14000548336975,1.,-1.76997111386769));
#47568=CARTESIAN_POINT('Ctrl Pts',(1.1346029180462,-1.,-1.76677384551862));
#47569=CARTESIAN_POINT('Ctrl Pts',(1.1346029180462,1.,-1.76677384551862));
#47570=CARTESIAN_POINT('Ctrl Pts',(1.12923123555075,-1.,-1.7635457196617));
#47571=CARTESIAN_POINT('Ctrl Pts',(1.12923123555075,1.,-1.7635457196617));
#47572=CARTESIAN_POINT('Ctrl Pts',(1.12389096855086,-1.,-1.76028671825096));
#47573=CARTESIAN_POINT('Ctrl Pts',(1.12389096855086,1.,-1.76028671825096));
#47574=CARTESIAN_POINT('Ctrl Pts',(1.11858293216763,-1.,-1.75699720772105));
#47575=CARTESIAN_POINT('Ctrl Pts',(1.11858293216763,1.,-1.75699720772105));
#47576=CARTESIAN_POINT('Ctrl Pts',(1.11330807582551,-1.,-1.7536777209463));
#47577=CARTESIAN_POINT('Ctrl Pts',(1.11330807582551,1.,-1.7536777209463));
#47578=CARTESIAN_POINT('Ctrl Pts',(1.10806728183007,-1.,-1.7503286607592));
#47579=CARTESIAN_POINT('Ctrl Pts',(1.10806728183007,1.,-1.7503286607592));
#47580=CARTESIAN_POINT('Ctrl Pts',(1.10286118991143,-1.,-1.74695004214923));
#47581=CARTESIAN_POINT('Ctrl Pts',(1.10286118991143,1.,-1.74695004214923));
#47582=CARTESIAN_POINT('Ctrl Pts',(1.09768999241225,-1.,-1.74354119236208));
#47583=CARTESIAN_POINT('Ctrl Pts',(1.09768999241225,1.,-1.74354119236208));
#47584=CARTESIAN_POINT('Ctrl Pts',(1.09255329056493,-1.,-1.74010053962247));
#47585=CARTESIAN_POINT('Ctrl Pts',(1.09255329056493,1.,-1.74010053962247));
#47586=CARTESIAN_POINT('Ctrl Pts',(1.08745056285427,-1.,-1.73662628326091));
#47587=CARTESIAN_POINT('Ctrl Pts',(1.08745056285427,1.,-1.73662628326091));
#47588=CARTESIAN_POINT('Ctrl Pts',(1.08238162784749,-1.,-1.73311705663407));
#47589=CARTESIAN_POINT('Ctrl Pts',(1.08238162784749,1.,-1.73311705663407));
#47590=CARTESIAN_POINT('Ctrl Pts',(1.0773470373727,-1.,-1.72957248977424));
#47591=CARTESIAN_POINT('Ctrl Pts',(1.0773470373727,1.,-1.72957248977424));
#47592=CARTESIAN_POINT('Ctrl Pts',(1.07234866990252,-1.,-1.72599406198488));
#47593=CARTESIAN_POINT('Ctrl Pts',(1.07234866990252,1.,-1.72599406198488));
#47594=CARTESIAN_POINT('Ctrl Pts',(1.06738966975462,-1.,-1.72238500928453));
#47595=CARTESIAN_POINT('Ctrl Pts',(1.06738966975462,1.,-1.72238500928453));
#47596=CARTESIAN_POINT('Ctrl Pts',(1.06247324680647,-1.,-1.71874858456904));
#47597=CARTESIAN_POINT('Ctrl Pts',(1.06247324680647,1.,-1.71874858456904));
#47598=CARTESIAN_POINT('Ctrl Pts',(1.05760163192479,-1.,-1.7150865442702));
#47599=CARTESIAN_POINT('Ctrl Pts',(1.05760163192479,1.,-1.7150865442702));
#47600=CARTESIAN_POINT('Ctrl Pts',(1.05277517202855,-1.,-1.71139783543989));
#47601=CARTESIAN_POINT('Ctrl Pts',(1.05277517202855,1.,-1.71139783543989));
#47602=CARTESIAN_POINT('Ctrl Pts',(1.04799085404995,-1.,-1.70767646263649));
#47603=CARTESIAN_POINT('Ctrl Pts',(1.04799085404995,1.,-1.70767646263649));
#47604=CARTESIAN_POINT('Ctrl Pts',(1.04324363334554,-1.,-1.70391338707982));
#47605=CARTESIAN_POINT('Ctrl Pts',(1.04324363334554,1.,-1.70391338707982));
#47606=CARTESIAN_POINT('Ctrl Pts',(1.03852922490789,-1.,-1.70010052930962));
#47607=CARTESIAN_POINT('Ctrl Pts',(1.03852922490789,1.,-1.70010052930962));
#47608=CARTESIAN_POINT('Ctrl Pts',(1.03384646003588,-1.,-1.69623414782771));
#47609=CARTESIAN_POINT('Ctrl Pts',(1.03384646003588,1.,-1.69623414782771));
#47610=CARTESIAN_POINT('Ctrl Pts',(1.02919977579147,-1.,-1.69231840863458));
#47611=CARTESIAN_POINT('Ctrl Pts',(1.02919977579147,1.,-1.69231840863458));
#47612=CARTESIAN_POINT('Ctrl Pts',(1.02460180535255,-1.,-1.68836910178447));
#47613=CARTESIAN_POINT('Ctrl Pts',(1.02460180535255,1.,-1.68836910178447));
#47614=CARTESIAN_POINT('Ctrl Pts',(1.02006795074201,-1.,-1.68440578021706));
#47615=CARTESIAN_POINT('Ctrl Pts',(1.02006795074201,1.,-1.68440578021706));
#47616=CARTESIAN_POINT('Ctrl Pts',(1.01561026162773,-1.,-1.68044289894798));
#47617=CARTESIAN_POINT('Ctrl Pts',(1.01561026162773,1.,-1.68044289894798));
#47618=CARTESIAN_POINT('Ctrl Pts',(1.01123236493511,-1.,-1.67648246776464));
#47619=CARTESIAN_POINT('Ctrl Pts',(1.01123236493511,1.,-1.67648246776464));
#47620=CARTESIAN_POINT('Ctrl Pts',(1.00692206696414,-1.,-1.67250335383293));
#47621=CARTESIAN_POINT('Ctrl Pts',(1.00692206696414,1.,-1.67250335383293));
#47622=CARTESIAN_POINT('Ctrl Pts',(1.00265091003727,-1.,-1.66846059277303));
#47623=CARTESIAN_POINT('Ctrl Pts',(1.00265091003727,1.,-1.66846059277303));
#47624=CARTESIAN_POINT('Ctrl Pts',(0.998389654952757,-1.,-1.66430758030376));
#47625=CARTESIAN_POINT('Ctrl Pts',(0.998389654952757,1.,-1.66430758030376));
#47626=CARTESIAN_POINT('Ctrl Pts',(0.994121836661305,-1.,-1.66001553809947));
#47627=CARTESIAN_POINT('Ctrl Pts',(0.994121836661305,1.,-1.66001553809947));
#47628=CARTESIAN_POINT('Ctrl Pts',(0.989855627854164,-1.,-1.65559044289699));
#47629=CARTESIAN_POINT('Ctrl Pts',(0.989855627854164,1.,-1.65559044289699));
#47630=CARTESIAN_POINT('Ctrl Pts',(0.98564262292082,-1.,-1.65110016612638));
#47631=CARTESIAN_POINT('Ctrl Pts',(0.98564262292082,1.,-1.65110016612638));
#47632=CARTESIAN_POINT('Ctrl Pts',(0.981562530939489,-1.,-1.64665139190656));
#47633=CARTESIAN_POINT('Ctrl Pts',(0.981562530939489,1.,-1.64665139190656));
#47634=CARTESIAN_POINT('Ctrl Pts',(0.977689794119416,-1.,-1.64233990826687));
#47635=CARTESIAN_POINT('Ctrl Pts',(0.977689794119416,1.,-1.64233990826687));
#47636=CARTESIAN_POINT('Ctrl Pts',(0.974066058287418,-1.,-1.63820952658144));
#47637=CARTESIAN_POINT('Ctrl Pts',(0.974066058287418,1.,-1.63820952658144));
#47638=CARTESIAN_POINT('Ctrl Pts',(0.970669715997509,-1.,-1.63420665729798));
#47639=CARTESIAN_POINT('Ctrl Pts',(0.970669715997509,1.,-1.63420665729798));
#47640=CARTESIAN_POINT('Ctrl Pts',(0.967387853230345,-1.,-1.63013849959462));
#47641=CARTESIAN_POINT('Ctrl Pts',(0.967387853230345,1.,-1.63013849959462));
#47642=CARTESIAN_POINT('Ctrl Pts',(0.964046107040535,-1.,-1.62571930670187));
#47643=CARTESIAN_POINT('Ctrl Pts',(0.964046107040535,1.,-1.62571930670187));
#47644=CARTESIAN_POINT('Ctrl Pts',(0.960438326101728,-1.,-1.62061638140221));
#47645=CARTESIAN_POINT('Ctrl Pts',(0.960438326101728,1.,-1.62061638140221));
#47646=CARTESIAN_POINT('Ctrl Pts',(0.95635442292067,-1.,-1.61449324337085));
#47647=CARTESIAN_POINT('Ctrl Pts',(0.95635442292067,1.,-1.61449324337085));
#47648=CARTESIAN_POINT('Ctrl Pts',(0.951613284356035,-1.,-1.60706069896936));
#47649=CARTESIAN_POINT('Ctrl Pts',(0.951613284356035,1.,-1.60706069896936));
#47650=CARTESIAN_POINT('Ctrl Pts',(0.946078063315257,-1.,-1.59810042043673));
#47651=CARTESIAN_POINT('Ctrl Pts',(0.946078063315257,1.,-1.59810042043673));
#47652=CARTESIAN_POINT('Ctrl Pts',(0.939646377893399,-1.,-1.58744937487176));
#47653=CARTESIAN_POINT('Ctrl Pts',(0.939646377893399,1.,-1.58744937487176));
#47654=CARTESIAN_POINT('Ctrl Pts',(0.932246680108685,-1.,-1.57499388382243));
#47655=CARTESIAN_POINT('Ctrl Pts',(0.932246680108685,1.,-1.57499388382243));
#47656=CARTESIAN_POINT('Ctrl Pts',(0.923832188944341,-1.,-1.56065988578893));
#47657=CARTESIAN_POINT('Ctrl Pts',(0.923832188944341,1.,-1.56065988578893));
#47658=CARTESIAN_POINT('Ctrl Pts',(0.914375919026456,-1.,-1.54440491149498));
#47659=CARTESIAN_POINT('Ctrl Pts',(0.914375919026456,1.,-1.54440491149498));
#47660=CARTESIAN_POINT('Ctrl Pts',(0.905967409625651,-1.,-1.52984849887993));
#47661=CARTESIAN_POINT('Ctrl Pts',(0.905967409625651,1.,-1.52984849887993));
#47662=CARTESIAN_POINT('Ctrl Pts',(0.89918504748351,-1.,-1.51805569590094));
#47663=CARTESIAN_POINT('Ctrl Pts',(0.89918504748351,1.,-1.51805569590094));
#47664=CARTESIAN_POINT('Ctrl Pts',(0.894452006964543,-1.,-1.50980486806688));
#47665=CARTESIAN_POINT('Ctrl Pts',(0.894452006964543,1.,-1.50980486806688));
#47666=CARTESIAN_POINT('Ctrl Pts',(0.892032620296855,-1.,-1.5055822144029));
#47667=CARTESIAN_POINT('Ctrl Pts',(0.892032620296855,1.,-1.5055822144029));
#47668=CARTESIAN_POINT('',(1.23627494547115,1.,-1.81978687191668));
#47669=CARTESIAN_POINT('Ctrl Pts',(1.23627494547115,1.,-1.81978687191668));
#47670=CARTESIAN_POINT('Ctrl Pts',(1.23509651170476,1.,-1.81925017193666));
#47671=CARTESIAN_POINT('Ctrl Pts',(1.2327422452705,1.,-1.81817389921279));
#47672=CARTESIAN_POINT('Ctrl Pts',(1.2292186489137,1.,-1.8165508718364));
#47673=CARTESIAN_POINT('Ctrl Pts',(1.2245361330495,1.,-1.81436959210434));
#47674=CARTESIAN_POINT('Ctrl Pts',(1.21870906103557,1.,-1.81161420806656));
#47675=CARTESIAN_POINT('Ctrl Pts',(1.21290815708314,1.,-1.80882996917129));
#47676=CARTESIAN_POINT('Ctrl Pts',(1.20713356605475,1.,-1.80601678480707));
#47677=CARTESIAN_POINT('Ctrl Pts',(1.20138548938974,1.,-1.80317454838603));
#47678=CARTESIAN_POINT('Ctrl Pts',(1.19566418930242,1.,-1.80030314369879));
#47679=CARTESIAN_POINT('Ctrl Pts',(1.18996997934445,1.,-1.79740245923478));
#47680=CARTESIAN_POINT('Ctrl Pts',(1.18430321697432,1.,-1.79447240321515));
#47681=CARTESIAN_POINT('Ctrl Pts',(1.17866429440809,1.,-1.79151291552689));
#47682=CARTESIAN_POINT('Ctrl Pts',(1.17305363177328,1.,-1.78852398877617));
#47683=CARTESIAN_POINT('Ctrl Pts',(1.16747166312303,1.,-1.78550566040443));
#47684=CARTESIAN_POINT('Ctrl Pts',(1.16191881298499,1.,-1.78245795881009));
#47685=CARTESIAN_POINT('Ctrl Pts',(1.15639547194698,1.,-1.77938085564275));
#47686=CARTESIAN_POINT('Ctrl Pts',(1.15090197841514,1.,-1.7762742255701));
#47687=CARTESIAN_POINT('Ctrl Pts',(1.1454385822692,1.,-1.77313777896194));
#47688=CARTESIAN_POINT('Ctrl Pts',(1.14000548336975,1.,-1.76997111386769));
#47689=CARTESIAN_POINT('Ctrl Pts',(1.1346029180462,1.,-1.76677384551862));
#47690=CARTESIAN_POINT('Ctrl Pts',(1.12923123555075,1.,-1.7635457196617));
#47691=CARTESIAN_POINT('Ctrl Pts',(1.12389096855086,1.,-1.76028671825096));
#47692=CARTESIAN_POINT('Ctrl Pts',(1.11858293216763,1.,-1.75699720772105));
#47693=CARTESIAN_POINT('Ctrl Pts',(1.11330807582551,1.,-1.7536777209463));
#47694=CARTESIAN_POINT('Ctrl Pts',(1.10806728183007,1.,-1.7503286607592));
#47695=CARTESIAN_POINT('Ctrl Pts',(1.10286118991143,1.,-1.74695004214923));
#47696=CARTESIAN_POINT('Ctrl Pts',(1.09768999241225,1.,-1.74354119236208));
#47697=CARTESIAN_POINT('Ctrl Pts',(1.09255329056493,1.,-1.74010053962247));
#47698=CARTESIAN_POINT('Ctrl Pts',(1.08745056285427,1.,-1.73662628326091));
#47699=CARTESIAN_POINT('Ctrl Pts',(1.08238162784749,1.,-1.73311705663407));
#47700=CARTESIAN_POINT('Ctrl Pts',(1.0773470373727,1.,-1.72957248977424));
#47701=CARTESIAN_POINT('Ctrl Pts',(1.07234866990252,1.,-1.72599406198488));
#47702=CARTESIAN_POINT('Ctrl Pts',(1.06738966975462,1.,-1.72238500928453));
#47703=CARTESIAN_POINT('Ctrl Pts',(1.06247324680647,1.,-1.71874858456904));
#47704=CARTESIAN_POINT('Ctrl Pts',(1.05760163192479,1.,-1.7150865442702));
#47705=CARTESIAN_POINT('Ctrl Pts',(1.05277517202855,1.,-1.71139783543989));
#47706=CARTESIAN_POINT('Ctrl Pts',(1.04799085404995,1.,-1.70767646263649));
#47707=CARTESIAN_POINT('Ctrl Pts',(1.04324363334554,1.,-1.70391338707982));
#47708=CARTESIAN_POINT('Ctrl Pts',(1.03852922490789,1.,-1.70010052930962));
#47709=CARTESIAN_POINT('Ctrl Pts',(1.03384646003588,1.,-1.69623414782771));
#47710=CARTESIAN_POINT('Ctrl Pts',(1.02919977579147,1.,-1.69231840863458));
#47711=CARTESIAN_POINT('Ctrl Pts',(1.02460180535255,1.,-1.68836910178447));
#47712=CARTESIAN_POINT('Ctrl Pts',(1.02006795074201,1.,-1.68440578021706));
#47713=CARTESIAN_POINT('Ctrl Pts',(1.01561026162773,1.,-1.68044289894798));
#47714=CARTESIAN_POINT('Ctrl Pts',(1.01123236493511,1.,-1.67648246776464));
#47715=CARTESIAN_POINT('Ctrl Pts',(1.00692206696414,1.,-1.67250335383293));
#47716=CARTESIAN_POINT('Ctrl Pts',(1.00265091003727,1.,-1.66846059277303));
#47717=CARTESIAN_POINT('Ctrl Pts',(0.998389654952757,1.,-1.66430758030376));
#47718=CARTESIAN_POINT('Ctrl Pts',(0.994121836661305,1.,-1.66001553809947));
#47719=CARTESIAN_POINT('Ctrl Pts',(0.989855627854164,1.,-1.65559044289699));
#47720=CARTESIAN_POINT('Ctrl Pts',(0.98564262292082,1.,-1.65110016612638));
#47721=CARTESIAN_POINT('Ctrl Pts',(0.981562530939489,1.,-1.64665139190656));
#47722=CARTESIAN_POINT('Ctrl Pts',(0.977689794119416,1.,-1.64233990826687));
#47723=CARTESIAN_POINT('Ctrl Pts',(0.974066058287418,1.,-1.63820952658144));
#47724=CARTESIAN_POINT('Ctrl Pts',(0.970669715997509,1.,-1.63420665729798));
#47725=CARTESIAN_POINT('Ctrl Pts',(0.967387853230345,1.,-1.63013849959462));
#47726=CARTESIAN_POINT('Ctrl Pts',(0.964046107040535,1.,-1.62571930670187));
#47727=CARTESIAN_POINT('Ctrl Pts',(0.960438326101728,1.,-1.62061638140221));
#47728=CARTESIAN_POINT('Ctrl Pts',(0.95635442292067,1.,-1.61449324337085));
#47729=CARTESIAN_POINT('Ctrl Pts',(0.951613284356035,1.,-1.60706069896936));
#47730=CARTESIAN_POINT('Ctrl Pts',(0.946078063315257,1.,-1.59810042043673));
#47731=CARTESIAN_POINT('Ctrl Pts',(0.939646377893399,1.,-1.58744937487176));
#47732=CARTESIAN_POINT('Ctrl Pts',(0.932246680108685,1.,-1.57499388382243));
#47733=CARTESIAN_POINT('Ctrl Pts',(0.923832188944341,1.,-1.56065988578893));
#47734=CARTESIAN_POINT('Ctrl Pts',(0.914375919026456,1.,-1.54440491149498));
#47735=CARTESIAN_POINT('Ctrl Pts',(0.905967409625651,1.,-1.52984849887993));
#47736=CARTESIAN_POINT('Ctrl Pts',(0.89918504748351,1.,-1.51805569590094));
#47737=CARTESIAN_POINT('Ctrl Pts',(0.894452006964543,1.,-1.50980486806688));
#47738=CARTESIAN_POINT('Ctrl Pts',(0.892032620296855,1.,-1.5055822144029));
#47739=CARTESIAN_POINT('',(1.23627494547115,0.,-1.81978687191668));
#47740=CARTESIAN_POINT('Origin',(1.34869019493419,0.,-1.73811241238545));
#47741=CARTESIAN_POINT('',(1.34869019493419,1.,-1.73811241238545));
#47742=CARTESIAN_POINT('',(1.23627494547115,1.,-1.81978687191668));
#47743=CARTESIAN_POINT('',(1.34869019493419,0.,-1.73811241238545));
#47744=CARTESIAN_POINT('Ctrl Pts',(1.15624053661742,-1.,-1.31362392696032));
#47745=CARTESIAN_POINT('Ctrl Pts',(1.15624053661742,1.,-1.31362392696032));
#47746=CARTESIAN_POINT('Ctrl Pts',(1.15950888730809,-1.,-1.31722977216397));
#47747=CARTESIAN_POINT('Ctrl Pts',(1.15950888730809,1.,-1.31722977216397));
#47748=CARTESIAN_POINT('Ctrl Pts',(1.16589330093588,-1.,-1.32428080721772));
#47749=CARTESIAN_POINT('Ctrl Pts',(1.16589330093588,1.,-1.32428080721772));
#47750=CARTESIAN_POINT('Ctrl Pts',(1.17501305789857,-1.,-1.33437539347008));
#47751=CARTESIAN_POINT('Ctrl Pts',(1.17501305789857,1.,-1.33437539347008));
#47752=CARTESIAN_POINT('Ctrl Pts',(1.18625865667441,-1.,-1.34687054001093));
#47753=CARTESIAN_POINT('Ctrl Pts',(1.18625865667441,1.,-1.34687054001093));
#47754=CARTESIAN_POINT('Ctrl Pts',(1.1987959077932,-1.,-1.36088705043885));
#47755=CARTESIAN_POINT('Ctrl Pts',(1.1987959077932,1.,-1.36088705043885));
#47756=CARTESIAN_POINT('Ctrl Pts',(1.20982812925645,-1.,-1.37331915607905));
#47757=CARTESIAN_POINT('Ctrl Pts',(1.20982812925645,1.,-1.37331915607905));
#47758=CARTESIAN_POINT('Ctrl Pts',(1.21938737280852,-1.,-1.38420564527715));
#47759=CARTESIAN_POINT('Ctrl Pts',(1.21938737280852,1.,-1.38420564527715));
#47760=CARTESIAN_POINT('Ctrl Pts',(1.22752961899387,-1.,-1.39361389568796));
#47761=CARTESIAN_POINT('Ctrl Pts',(1.22752961899387,1.,-1.39361389568796));
#47762=CARTESIAN_POINT('Ctrl Pts',(1.23434087290423,-1.,-1.40164708206106));
#47763=CARTESIAN_POINT('Ctrl Pts',(1.23434087290423,1.,-1.40164708206106));
#47764=CARTESIAN_POINT('Ctrl Pts',(1.23994455029534,-1.,-1.40845295531283));
#47765=CARTESIAN_POINT('Ctrl Pts',(1.23994455029534,1.,-1.40845295531283));
#47766=CARTESIAN_POINT('Ctrl Pts',(1.24450600513056,-1.,-1.41422913175179));
#47767=CARTESIAN_POINT('Ctrl Pts',(1.24450600513056,1.,-1.41422913175179));
#47768=CARTESIAN_POINT('Ctrl Pts',(1.24824430986571,-1.,-1.41923722596025));
#47769=CARTESIAN_POINT('Ctrl Pts',(1.24824430986571,1.,-1.41923722596025));
#47770=CARTESIAN_POINT('Ctrl Pts',(1.2514145557001,-1.,-1.42378102115575));
#47771=CARTESIAN_POINT('Ctrl Pts',(1.2514145557001,1.,-1.42378102115575));
#47772=CARTESIAN_POINT('Ctrl Pts',(1.25426945222639,-1.,-1.42815938799387));
#47773=CARTESIAN_POINT('Ctrl Pts',(1.25426945222639,1.,-1.42815938799387));
#47774=CARTESIAN_POINT('Ctrl Pts',(1.25702687965755,-1.,-1.43262645609691));
#47775=CARTESIAN_POINT('Ctrl Pts',(1.25702687965755,1.,-1.43262645609691));
#47776=CARTESIAN_POINT('Ctrl Pts',(1.25983531012005,-1.,-1.43734919180848));
#47777=CARTESIAN_POINT('Ctrl Pts',(1.25983531012005,1.,-1.43734919180848));
#47778=CARTESIAN_POINT('Ctrl Pts',(1.26273903323858,-1.,-1.44236470511303));
#47779=CARTESIAN_POINT('Ctrl Pts',(1.26273903323858,1.,-1.44236470511303));
#47780=CARTESIAN_POINT('Ctrl Pts',(1.26570925118868,-1.,-1.44761985001662));
#47781=CARTESIAN_POINT('Ctrl Pts',(1.26570925118868,1.,-1.44761985001662));
#47782=CARTESIAN_POINT('Ctrl Pts',(1.2686778680489,-1.,-1.45301422764247));
#47783=CARTESIAN_POINT('Ctrl Pts',(1.2686778680489,1.,-1.45301422764247));
#47784=CARTESIAN_POINT('Ctrl Pts',(1.27156805265289,-1.,-1.45843906294697));
#47785=CARTESIAN_POINT('Ctrl Pts',(1.27156805265289,1.,-1.45843906294697));
#47786=CARTESIAN_POINT('Ctrl Pts',(1.27433119897822,-1.,-1.46382431332476));
#47787=CARTESIAN_POINT('Ctrl Pts',(1.27433119897822,1.,-1.46382431332476));
#47788=CARTESIAN_POINT('Ctrl Pts',(1.27696414831089,-1.,-1.46916035917133));
#47789=CARTESIAN_POINT('Ctrl Pts',(1.27696414831089,1.,-1.46916035917133));
#47790=CARTESIAN_POINT('Ctrl Pts',(1.2794891824849,-1.,-1.4744717526707));
#47791=CARTESIAN_POINT('Ctrl Pts',(1.2794891824849,1.,-1.4744717526707));
#47792=CARTESIAN_POINT('Ctrl Pts',(1.28194158939517,-1.,-1.47980070347096));
#47793=CARTESIAN_POINT('Ctrl Pts',(1.28194158939517,1.,-1.47980070347096));
#47794=CARTESIAN_POINT('Ctrl Pts',(1.28435533880201,-1.,-1.4851881711891));
#47795=CARTESIAN_POINT('Ctrl Pts',(1.28435533880201,1.,-1.4851881711891));
#47796=CARTESIAN_POINT('Ctrl Pts',(1.2867467611644,-1.,-1.4906522831278));
#47797=CARTESIAN_POINT('Ctrl Pts',(1.2867467611644,1.,-1.4906522831278));
#47798=CARTESIAN_POINT('Ctrl Pts',(1.28911506584254,-1.,-1.49618896881754));
#47799=CARTESIAN_POINT('Ctrl Pts',(1.28911506584254,1.,-1.49618896881754));
#47800=CARTESIAN_POINT('Ctrl Pts',(1.29145022885181,-1.,-1.50178230149776));
#47801=CARTESIAN_POINT('Ctrl Pts',(1.29145022885181,1.,-1.50178230149776));
#47802=CARTESIAN_POINT('Ctrl Pts',(1.29373841372842,-1.,-1.50741159078365));
#47803=CARTESIAN_POINT('Ctrl Pts',(1.29373841372842,1.,-1.50741159078365));
#47804=CARTESIAN_POINT('Ctrl Pts',(1.29596850710509,-1.,-1.51305994241402));
#47805=CARTESIAN_POINT('Ctrl Pts',(1.29596850710509,1.,-1.51305994241402));
#47806=CARTESIAN_POINT('Ctrl Pts',(1.29813791800747,-1.,-1.51872184912724));
#47807=CARTESIAN_POINT('Ctrl Pts',(1.29813791800747,1.,-1.51872184912724));
#47808=CARTESIAN_POINT('Ctrl Pts',(1.30024984366328,-1.,-1.52439957861062));
#47809=CARTESIAN_POINT('Ctrl Pts',(1.30024984366328,1.,-1.52439957861062));
#47810=CARTESIAN_POINT('Ctrl Pts',(1.30231064395568,-1.,-1.53009970283891));
#47811=CARTESIAN_POINT('Ctrl Pts',(1.30231064395568,1.,-1.53009970283891));
#47812=CARTESIAN_POINT('Ctrl Pts',(1.30432735639489,-1.,-1.53582981268977));
#47813=CARTESIAN_POINT('Ctrl Pts',(1.30432735639489,1.,-1.53582981268977));
#47814=CARTESIAN_POINT('Ctrl Pts',(1.30630475189556,-1.,-1.54159462645432));
#47815=CARTESIAN_POINT('Ctrl Pts',(1.30630475189556,1.,-1.54159462645432));
#47816=CARTESIAN_POINT('Ctrl Pts',(1.30824393907473,-1.,-1.54739413957185));
#47817=CARTESIAN_POINT('Ctrl Pts',(1.30824393907473,1.,-1.54739413957185));
#47818=CARTESIAN_POINT('Ctrl Pts',(1.31014393684222,-1.,-1.55322568759481));
#47819=CARTESIAN_POINT('Ctrl Pts',(1.31014393684222,1.,-1.55322568759481));
#47820=CARTESIAN_POINT('Ctrl Pts',(1.31200264341696,-1.,-1.55908521254821));
#47821=CARTESIAN_POINT('Ctrl Pts',(1.31200264341696,1.,-1.55908521254821));
#47822=CARTESIAN_POINT('Ctrl Pts',(1.31381795281002,-1.,-1.56496872402353));
#47823=CARTESIAN_POINT('Ctrl Pts',(1.31381795281002,1.,-1.56496872402353));
#47824=CARTESIAN_POINT('Ctrl Pts',(1.31558903860016,-1.,-1.57087397835723));
#47825=CARTESIAN_POINT('Ctrl Pts',(1.31558903860016,1.,-1.57087397835723));
#47826=CARTESIAN_POINT('Ctrl Pts',(1.31731642317187,-1.,-1.5768005650559));
#47827=CARTESIAN_POINT('Ctrl Pts',(1.31731642317187,1.,-1.5768005650559));
#47828=CARTESIAN_POINT('Ctrl Pts',(1.31900135021432,-1.,-1.58274907898834));
#47829=CARTESIAN_POINT('Ctrl Pts',(1.31900135021432,1.,-1.58274907898834));
#47830=CARTESIAN_POINT('Ctrl Pts',(1.32064537110892,-1.,-1.58872057258245));
#47831=CARTESIAN_POINT('Ctrl Pts',(1.32064537110892,1.,-1.58872057258245));
#47832=CARTESIAN_POINT('Ctrl Pts',(1.32224985747682,-1.,-1.59471591079403));
#47833=CARTESIAN_POINT('Ctrl Pts',(1.32224985747682,1.,-1.59471591079403));
#47834=CARTESIAN_POINT('Ctrl Pts',(1.32381550858256,-1.,-1.60073511858687));
#47835=CARTESIAN_POINT('Ctrl Pts',(1.32381550858256,1.,-1.60073511858687));
#47836=CARTESIAN_POINT('Ctrl Pts',(1.32534250785782,-1.,-1.60677758290954));
#47837=CARTESIAN_POINT('Ctrl Pts',(1.32534250785782,1.,-1.60677758290954));
#47838=CARTESIAN_POINT('Ctrl Pts',(1.32683074483356,-1.,-1.6128423401575));
#47839=CARTESIAN_POINT('Ctrl Pts',(1.32683074483356,1.,-1.6128423401575));
#47840=CARTESIAN_POINT('Ctrl Pts',(1.32828000610449,-1.,-1.61892832270724));
#47841=CARTESIAN_POINT('Ctrl Pts',(1.32828000610449,1.,-1.61892832270724));
#47842=CARTESIAN_POINT('Ctrl Pts',(1.3296901950568,-1.,-1.62503464209797));
#47843=CARTESIAN_POINT('Ctrl Pts',(1.3296901950568,1.,-1.62503464209797));
#47844=CARTESIAN_POINT('Ctrl Pts',(1.33106149345645,-1.,-1.63116079730923));
#47845=CARTESIAN_POINT('Ctrl Pts',(1.33106149345645,1.,-1.63116079730923));
#47846=CARTESIAN_POINT('Ctrl Pts',(1.33239425103724,-1.,-1.63730653475089));
#47847=CARTESIAN_POINT('Ctrl Pts',(1.33239425103724,1.,-1.63730653475089));
#47848=CARTESIAN_POINT('Ctrl Pts',(1.33368890676572,-1.,-1.6434717485603));
#47849=CARTESIAN_POINT('Ctrl Pts',(1.33368890676572,1.,-1.6434717485603));
#47850=CARTESIAN_POINT('Ctrl Pts',(1.33494590467993,-1.,-1.6496563728683));
#47851=CARTESIAN_POINT('Ctrl Pts',(1.33494590467993,1.,-1.6496563728683));
#47852=CARTESIAN_POINT('Ctrl Pts',(1.33616559745172,-1.,-1.65586025952593));
#47853=CARTESIAN_POINT('Ctrl Pts',(1.33616559745172,1.,-1.65586025952593));
#47854=CARTESIAN_POINT('Ctrl Pts',(1.33734820885262,-1.,-1.66208312541983));
#47855=CARTESIAN_POINT('Ctrl Pts',(1.33734820885262,1.,-1.66208312541983));
#47856=CARTESIAN_POINT('Ctrl Pts',(1.33849388654388,-1.,-1.66832460783989));
#47857=CARTESIAN_POINT('Ctrl Pts',(1.33849388654388,1.,-1.66832460783989));
#47858=CARTESIAN_POINT('Ctrl Pts',(1.3396027347034,-1.,-1.67458429426086));
#47859=CARTESIAN_POINT('Ctrl Pts',(1.3396027347034,1.,-1.67458429426086));
#47860=CARTESIAN_POINT('Ctrl Pts',(1.34067485185203,-1.,-1.68086176030362));
#47861=CARTESIAN_POINT('Ctrl Pts',(1.34067485185203,1.,-1.68086176030362));
#47862=CARTESIAN_POINT('Ctrl Pts',(1.341710374848,-1.,-1.68715660868764));
#47863=CARTESIAN_POINT('Ctrl Pts',(1.341710374848,1.,-1.68715660868764));
#47864=CARTESIAN_POINT('Ctrl Pts',(1.34270948206319,-1.,-1.6934684849687));
#47865=CARTESIAN_POINT('Ctrl Pts',(1.34270948206319,1.,-1.6934684849687));
#47866=CARTESIAN_POINT('Ctrl Pts',(1.34367237124483,-1.,-1.69979707754427));
#47867=CARTESIAN_POINT('Ctrl Pts',(1.34367237124483,1.,-1.69979707754427));
#47868=CARTESIAN_POINT('Ctrl Pts',(1.34459924533831,-1.,-1.70614212266738));
#47869=CARTESIAN_POINT('Ctrl Pts',(1.34459924533831,1.,-1.70614212266738));
#47870=CARTESIAN_POINT('Ctrl Pts',(1.34549029589416,-1.,-1.71250340686822));
#47871=CARTESIAN_POINT('Ctrl Pts',(1.34549029589416,1.,-1.71250340686822));
#47872=CARTESIAN_POINT('Ctrl Pts',(1.34634568653227,-1.,-1.7188807715049));
#47873=CARTESIAN_POINT('Ctrl Pts',(1.34634568653227,1.,-1.7188807715049));
#47874=CARTESIAN_POINT('Ctrl Pts',(1.34716554819527,-1.,-1.72527410680674));
#47875=CARTESIAN_POINT('Ctrl Pts',(1.34716554819527,1.,-1.72527410680674));
#47876=CARTESIAN_POINT('Ctrl Pts',(1.34779309152035,-1.,-1.7304014965394));
#47877=CARTESIAN_POINT('Ctrl Pts',(1.34779309152035,1.,-1.7304014965394));
#47878=CARTESIAN_POINT('Ctrl Pts',(1.34824783112887,-1.,-1.73425417885907));
#47879=CARTESIAN_POINT('Ctrl Pts',(1.34824783112887,1.,-1.73425417885907));
#47880=CARTESIAN_POINT('Ctrl Pts',(1.34854391898045,-1.,-1.73682580585691));
#47881=CARTESIAN_POINT('Ctrl Pts',(1.34854391898045,1.,-1.73682580585691));
#47882=CARTESIAN_POINT('Ctrl Pts',(1.34869019493419,-1.,-1.73811241238545));
#47883=CARTESIAN_POINT('Ctrl Pts',(1.34869019493419,1.,-1.73811241238545));
#47884=CARTESIAN_POINT('',(1.15624053661742,1.,-1.31362392696032));
#47885=CARTESIAN_POINT('Ctrl Pts',(1.15624053661742,1.,-1.31362392696032));
#47886=CARTESIAN_POINT('Ctrl Pts',(1.15950888730809,1.,-1.31722977216397));
#47887=CARTESIAN_POINT('Ctrl Pts',(1.16589330093588,1.,-1.32428080721772));
#47888=CARTESIAN_POINT('Ctrl Pts',(1.17501305789857,1.,-1.33437539347008));
#47889=CARTESIAN_POINT('Ctrl Pts',(1.18625865667441,1.,-1.34687054001093));
#47890=CARTESIAN_POINT('Ctrl Pts',(1.1987959077932,1.,-1.36088705043885));
#47891=CARTESIAN_POINT('Ctrl Pts',(1.20982812925645,1.,-1.37331915607905));
#47892=CARTESIAN_POINT('Ctrl Pts',(1.21938737280852,1.,-1.38420564527715));
#47893=CARTESIAN_POINT('Ctrl Pts',(1.22752961899387,1.,-1.39361389568796));
#47894=CARTESIAN_POINT('Ctrl Pts',(1.23434087290423,1.,-1.40164708206106));
#47895=CARTESIAN_POINT('Ctrl Pts',(1.23994455029534,1.,-1.40845295531283));
#47896=CARTESIAN_POINT('Ctrl Pts',(1.24450600513056,1.,-1.41422913175179));
#47897=CARTESIAN_POINT('Ctrl Pts',(1.24824430986571,1.,-1.41923722596025));
#47898=CARTESIAN_POINT('Ctrl Pts',(1.2514145557001,1.,-1.42378102115575));
#47899=CARTESIAN_POINT('Ctrl Pts',(1.25426945222639,1.,-1.42815938799387));
#47900=CARTESIAN_POINT('Ctrl Pts',(1.25702687965755,1.,-1.43262645609691));
#47901=CARTESIAN_POINT('Ctrl Pts',(1.25983531012005,1.,-1.43734919180848));
#47902=CARTESIAN_POINT('Ctrl Pts',(1.26273903323858,1.,-1.44236470511303));
#47903=CARTESIAN_POINT('Ctrl Pts',(1.26570925118868,1.,-1.44761985001662));
#47904=CARTESIAN_POINT('Ctrl Pts',(1.2686778680489,1.,-1.45301422764247));
#47905=CARTESIAN_POINT('Ctrl Pts',(1.27156805265289,1.,-1.45843906294697));
#47906=CARTESIAN_POINT('Ctrl Pts',(1.27433119897822,1.,-1.46382431332476));
#47907=CARTESIAN_POINT('Ctrl Pts',(1.27696414831089,1.,-1.46916035917133));
#47908=CARTESIAN_POINT('Ctrl Pts',(1.2794891824849,1.,-1.4744717526707));
#47909=CARTESIAN_POINT('Ctrl Pts',(1.28194158939517,1.,-1.47980070347096));
#47910=CARTESIAN_POINT('Ctrl Pts',(1.28435533880201,1.,-1.4851881711891));
#47911=CARTESIAN_POINT('Ctrl Pts',(1.2867467611644,1.,-1.4906522831278));
#47912=CARTESIAN_POINT('Ctrl Pts',(1.28911506584254,1.,-1.49618896881754));
#47913=CARTESIAN_POINT('Ctrl Pts',(1.29145022885181,1.,-1.50178230149776));
#47914=CARTESIAN_POINT('Ctrl Pts',(1.29373841372842,1.,-1.50741159078365));
#47915=CARTESIAN_POINT('Ctrl Pts',(1.29596850710509,1.,-1.51305994241402));
#47916=CARTESIAN_POINT('Ctrl Pts',(1.29813791800747,1.,-1.51872184912724));
#47917=CARTESIAN_POINT('Ctrl Pts',(1.30024984366328,1.,-1.52439957861062));
#47918=CARTESIAN_POINT('Ctrl Pts',(1.30231064395568,1.,-1.53009970283891));
#47919=CARTESIAN_POINT('Ctrl Pts',(1.30432735639489,1.,-1.53582981268977));
#47920=CARTESIAN_POINT('Ctrl Pts',(1.30630475189556,1.,-1.54159462645432));
#47921=CARTESIAN_POINT('Ctrl Pts',(1.30824393907473,1.,-1.54739413957185));
#47922=CARTESIAN_POINT('Ctrl Pts',(1.31014393684222,1.,-1.55322568759481));
#47923=CARTESIAN_POINT('Ctrl Pts',(1.31200264341696,1.,-1.55908521254821));
#47924=CARTESIAN_POINT('Ctrl Pts',(1.31381795281002,1.,-1.56496872402353));
#47925=CARTESIAN_POINT('Ctrl Pts',(1.31558903860016,1.,-1.57087397835723));
#47926=CARTESIAN_POINT('Ctrl Pts',(1.31731642317187,1.,-1.5768005650559));
#47927=CARTESIAN_POINT('Ctrl Pts',(1.31900135021432,1.,-1.58274907898834));
#47928=CARTESIAN_POINT('Ctrl Pts',(1.32064537110892,1.,-1.58872057258245));
#47929=CARTESIAN_POINT('Ctrl Pts',(1.32224985747682,1.,-1.59471591079403));
#47930=CARTESIAN_POINT('Ctrl Pts',(1.32381550858256,1.,-1.60073511858687));
#47931=CARTESIAN_POINT('Ctrl Pts',(1.32534250785782,1.,-1.60677758290954));
#47932=CARTESIAN_POINT('Ctrl Pts',(1.32683074483356,1.,-1.6128423401575));
#47933=CARTESIAN_POINT('Ctrl Pts',(1.32828000610449,1.,-1.61892832270724));
#47934=CARTESIAN_POINT('Ctrl Pts',(1.3296901950568,1.,-1.62503464209797));
#47935=CARTESIAN_POINT('Ctrl Pts',(1.33106149345645,1.,-1.63116079730923));
#47936=CARTESIAN_POINT('Ctrl Pts',(1.33239425103724,1.,-1.63730653475089));
#47937=CARTESIAN_POINT('Ctrl Pts',(1.33368890676572,1.,-1.6434717485603));
#47938=CARTESIAN_POINT('Ctrl Pts',(1.33494590467993,1.,-1.6496563728683));
#47939=CARTESIAN_POINT('Ctrl Pts',(1.33616559745172,1.,-1.65586025952593));
#47940=CARTESIAN_POINT('Ctrl Pts',(1.33734820885262,1.,-1.66208312541983));
#47941=CARTESIAN_POINT('Ctrl Pts',(1.33849388654388,1.,-1.66832460783989));
#47942=CARTESIAN_POINT('Ctrl Pts',(1.3396027347034,1.,-1.67458429426086));
#47943=CARTESIAN_POINT('Ctrl Pts',(1.34067485185203,1.,-1.68086176030362));
#47944=CARTESIAN_POINT('Ctrl Pts',(1.341710374848,1.,-1.68715660868764));
#47945=CARTESIAN_POINT('Ctrl Pts',(1.34270948206319,1.,-1.6934684849687));
#47946=CARTESIAN_POINT('Ctrl Pts',(1.34367237124483,1.,-1.69979707754427));
#47947=CARTESIAN_POINT('Ctrl Pts',(1.34459924533831,1.,-1.70614212266738));
#47948=CARTESIAN_POINT('Ctrl Pts',(1.34549029589416,1.,-1.71250340686822));
#47949=CARTESIAN_POINT('Ctrl Pts',(1.34634568653227,1.,-1.7188807715049));
#47950=CARTESIAN_POINT('Ctrl Pts',(1.34716554819527,1.,-1.72527410680674));
#47951=CARTESIAN_POINT('Ctrl Pts',(1.34779309152035,1.,-1.7304014965394));
#47952=CARTESIAN_POINT('Ctrl Pts',(1.34824783112887,1.,-1.73425417885907));
#47953=CARTESIAN_POINT('Ctrl Pts',(1.34854391898045,1.,-1.73682580585691));
#47954=CARTESIAN_POINT('Ctrl Pts',(1.34869019493419,1.,-1.73811241238545));
#47955=CARTESIAN_POINT('',(1.15624053661742,0.,-1.31362392696032));
#47956=CARTESIAN_POINT('Origin',(0.,0.,0.));
#47957=CARTESIAN_POINT('',(1.31362392696032,1.,-1.15624053661742));
#47958=CARTESIAN_POINT('Origin',(0.,1.,0.));
#47959=CARTESIAN_POINT('',(1.31362392696032,0.,-1.15624053661742));
#47960=CARTESIAN_POINT('Ctrl Pts',(1.73811241238545,-1.,-1.34869019493419));
#47961=CARTESIAN_POINT('Ctrl Pts',(1.73811241238545,1.,-1.34869019493419));
#47962=CARTESIAN_POINT('Ctrl Pts',(1.73682580585819,-1.,-1.34854391898145));
#47963=CARTESIAN_POINT('Ctrl Pts',(1.73682580585819,1.,-1.34854391898145));
#47964=CARTESIAN_POINT('Ctrl Pts',(1.73425417886254,-1.,-1.34824783113158));
#47965=CARTESIAN_POINT('Ctrl Pts',(1.73425417886254,1.,-1.34824783113158));
#47966=CARTESIAN_POINT('Ctrl Pts',(1.73040149654497,-1.,-1.3477930915247));
#47967=CARTESIAN_POINT('Ctrl Pts',(1.73040149654497,1.,-1.3477930915247));
#47968=CARTESIAN_POINT('Ctrl Pts',(1.72527410681298,-1.,-1.34716554820013));
#47969=CARTESIAN_POINT('Ctrl Pts',(1.72527410681298,1.,-1.34716554820013));
#47970=CARTESIAN_POINT('Ctrl Pts',(1.7188807715095,-1.,-1.34634568653586));
#47971=CARTESIAN_POINT('Ctrl Pts',(1.7188807715095,1.,-1.34634568653586));
#47972=CARTESIAN_POINT('Ctrl Pts',(1.71250340687011,-1.,-1.34549029589563));
#47973=CARTESIAN_POINT('Ctrl Pts',(1.71250340687011,1.,-1.34549029589563));
#47974=CARTESIAN_POINT('Ctrl Pts',(1.70614212266676,-1.,-1.34459924533783));
#47975=CARTESIAN_POINT('Ctrl Pts',(1.70614212266676,1.,-1.34459924533783));
#47976=CARTESIAN_POINT('Ctrl Pts',(1.69979707754221,-1.,-1.34367237124322));
#47977=CARTESIAN_POINT('Ctrl Pts',(1.69979707754221,1.,-1.34367237124322));
#47978=CARTESIAN_POINT('Ctrl Pts',(1.6934684849664,-1.,-1.34270948206139));
#47979=CARTESIAN_POINT('Ctrl Pts',(1.6934684849664,1.,-1.34270948206139));
#47980=CARTESIAN_POINT('Ctrl Pts',(1.68715660868602,-1.,-1.34171037484673));
#47981=CARTESIAN_POINT('Ctrl Pts',(1.68715660868602,1.,-1.34171037484673));
#47982=CARTESIAN_POINT('Ctrl Pts',(1.68086176030308,-1.,-1.3406748518516));
#47983=CARTESIAN_POINT('Ctrl Pts',(1.68086176030308,1.,-1.3406748518516));
#47984=CARTESIAN_POINT('Ctrl Pts',(1.67458429426126,-1.,-1.33960273470372));
#47985=CARTESIAN_POINT('Ctrl Pts',(1.67458429426126,1.,-1.33960273470372));
#47986=CARTESIAN_POINT('Ctrl Pts',(1.66832460784078,-1.,-1.33849388654458));
#47987=CARTESIAN_POINT('Ctrl Pts',(1.66832460784078,1.,-1.33849388654458));
#47988=CARTESIAN_POINT('Ctrl Pts',(1.66208312542073,-1.,-1.33734820885331));
#47989=CARTESIAN_POINT('Ctrl Pts',(1.66208312542073,1.,-1.33734820885331));
#47990=CARTESIAN_POINT('Ctrl Pts',(1.65586025952651,-1.,-1.33616559745217));
#47991=CARTESIAN_POINT('Ctrl Pts',(1.65586025952651,1.,-1.33616559745217));
#47992=CARTESIAN_POINT('Ctrl Pts',(1.64965637286843,-1.,-1.33494590468003));
#47993=CARTESIAN_POINT('Ctrl Pts',(1.64965637286843,1.,-1.33494590468003));
#47994=CARTESIAN_POINT('Ctrl Pts',(1.64347174856007,-1.,-1.33368890676554));
#47995=CARTESIAN_POINT('Ctrl Pts',(1.64347174856007,1.,-1.33368890676554));
#47996=CARTESIAN_POINT('Ctrl Pts',(1.63730653475049,-1.,-1.33239425103694));
#47997=CARTESIAN_POINT('Ctrl Pts',(1.63730653475049,1.,-1.33239425103694));
#47998=CARTESIAN_POINT('Ctrl Pts',(1.63116079730887,-1.,-1.33106149345618));
#47999=CARTESIAN_POINT('Ctrl Pts',(1.63116079730887,1.,-1.33106149345618));
#48000=CARTESIAN_POINT('Ctrl Pts',(1.62503464209777,-1.,-1.32969019505665));
#48001=CARTESIAN_POINT('Ctrl Pts',(1.62503464209777,1.,-1.32969019505665));
#48002=CARTESIAN_POINT('Ctrl Pts',(1.61892832270723,-1.,-1.32828000610448));
#48003=CARTESIAN_POINT('Ctrl Pts',(1.61892832270723,1.,-1.32828000610448));
#48004=CARTESIAN_POINT('Ctrl Pts',(1.61284234015762,-1.,-1.32683074483365));
#48005=CARTESIAN_POINT('Ctrl Pts',(1.61284234015762,1.,-1.32683074483365));
#48006=CARTESIAN_POINT('Ctrl Pts',(1.6067775829097,-1.,-1.32534250785794));
#48007=CARTESIAN_POINT('Ctrl Pts',(1.6067775829097,1.,-1.32534250785794));
#48008=CARTESIAN_POINT('Ctrl Pts',(1.600735118587,-1.,-1.32381550858266));
#48009=CARTESIAN_POINT('Ctrl Pts',(1.600735118587,1.,-1.32381550858266));
#48010=CARTESIAN_POINT('Ctrl Pts',(1.59471591079408,-1.,-1.32224985747686));
#48011=CARTESIAN_POINT('Ctrl Pts',(1.59471591079408,1.,-1.32224985747686));
#48012=CARTESIAN_POINT('Ctrl Pts',(1.58872057258244,-1.,-1.32064537110891));
#48013=CARTESIAN_POINT('Ctrl Pts',(1.58872057258244,1.,-1.32064537110891));
#48014=CARTESIAN_POINT('Ctrl Pts',(1.58274907898829,-1.,-1.31900135021428));
#48015=CARTESIAN_POINT('Ctrl Pts',(1.58274907898829,1.,-1.31900135021428));
#48016=CARTESIAN_POINT('Ctrl Pts',(1.57680056505585,-1.,-1.31731642317183));
#48017=CARTESIAN_POINT('Ctrl Pts',(1.57680056505585,1.,-1.31731642317183));
#48018=CARTESIAN_POINT('Ctrl Pts',(1.57087397835721,-1.,-1.31558903860015));
#48019=CARTESIAN_POINT('Ctrl Pts',(1.57087397835721,1.,-1.31558903860015));
#48020=CARTESIAN_POINT('Ctrl Pts',(1.56496872402352,-1.,-1.31381795281002));
#48021=CARTESIAN_POINT('Ctrl Pts',(1.56496872402352,1.,-1.31381795281002));
#48022=CARTESIAN_POINT('Ctrl Pts',(1.55908521254822,-1.,-1.31200264341696));
#48023=CARTESIAN_POINT('Ctrl Pts',(1.55908521254822,1.,-1.31200264341696));
#48024=CARTESIAN_POINT('Ctrl Pts',(1.55322568759481,-1.,-1.31014393684221));
#48025=CARTESIAN_POINT('Ctrl Pts',(1.55322568759481,1.,-1.31014393684221));
#48026=CARTESIAN_POINT('Ctrl Pts',(1.54739413957183,-1.,-1.30824393907471));
#48027=CARTESIAN_POINT('Ctrl Pts',(1.54739413957183,1.,-1.30824393907471));
#48028=CARTESIAN_POINT('Ctrl Pts',(1.54159462645428,-1.,-1.30630475189553));
#48029=CARTESIAN_POINT('Ctrl Pts',(1.54159462645428,1.,-1.30630475189553));
#48030=CARTESIAN_POINT('Ctrl Pts',(1.53582981268976,-1.,-1.30432735639487));
#48031=CARTESIAN_POINT('Ctrl Pts',(1.53582981268976,1.,-1.30432735639487));
#48032=CARTESIAN_POINT('Ctrl Pts',(1.53009970283893,-1.,-1.3023106439557));
#48033=CARTESIAN_POINT('Ctrl Pts',(1.53009970283893,1.,-1.3023106439557));
#48034=CARTESIAN_POINT('Ctrl Pts',(1.5243995786107,-1.,-1.30024984366334));
#48035=CARTESIAN_POINT('Ctrl Pts',(1.5243995786107,1.,-1.30024984366334));
#48036=CARTESIAN_POINT('Ctrl Pts',(1.51872184912735,-1.,-1.29813791800757));
#48037=CARTESIAN_POINT('Ctrl Pts',(1.51872184912735,1.,-1.29813791800757));
#48038=CARTESIAN_POINT('Ctrl Pts',(1.51305994241412,-1.,-1.29596850710518));
#48039=CARTESIAN_POINT('Ctrl Pts',(1.51305994241412,1.,-1.29596850710518));
#48040=CARTESIAN_POINT('Ctrl Pts',(1.50741159078367,-1.,-1.29373841372843));
#48041=CARTESIAN_POINT('Ctrl Pts',(1.50741159078367,1.,-1.29373841372843));
#48042=CARTESIAN_POINT('Ctrl Pts',(1.50178230149764,-1.,-1.29145022885171));
#48043=CARTESIAN_POINT('Ctrl Pts',(1.50178230149764,1.,-1.29145022885171));
#48044=CARTESIAN_POINT('Ctrl Pts',(1.49618896881729,-1.,-1.28911506584232));
#48045=CARTESIAN_POINT('Ctrl Pts',(1.49618896881729,1.,-1.28911506584232));
#48046=CARTESIAN_POINT('Ctrl Pts',(1.4906522831275,-1.,-1.28674676116415));
#48047=CARTESIAN_POINT('Ctrl Pts',(1.4906522831275,1.,-1.28674676116415));
#48048=CARTESIAN_POINT('Ctrl Pts',(1.48518817118891,-1.,-1.28435533880184));
#48049=CARTESIAN_POINT('Ctrl Pts',(1.48518817118891,1.,-1.28435533880184));
#48050=CARTESIAN_POINT('Ctrl Pts',(1.47980070347102,-1.,-1.28194158939522));
#48051=CARTESIAN_POINT('Ctrl Pts',(1.47980070347102,1.,-1.28194158939522));
#48052=CARTESIAN_POINT('Ctrl Pts',(1.4744717526711,-1.,-1.27948918248524));
#48053=CARTESIAN_POINT('Ctrl Pts',(1.4744717526711,1.,-1.27948918248524));
#48054=CARTESIAN_POINT('Ctrl Pts',(1.46916035917197,-1.,-1.27696414831144));
#48055=CARTESIAN_POINT('Ctrl Pts',(1.46916035917197,1.,-1.27696414831144));
#48056=CARTESIAN_POINT('Ctrl Pts',(1.4638243133254,-1.,-1.27433119897877));
#48057=CARTESIAN_POINT('Ctrl Pts',(1.4638243133254,1.,-1.27433119897877));
#48058=CARTESIAN_POINT('Ctrl Pts',(1.45843906294725,-1.,-1.27156805265312));
#48059=CARTESIAN_POINT('Ctrl Pts',(1.45843906294725,1.,-1.27156805265312));
#48060=CARTESIAN_POINT('Ctrl Pts',(1.45301422764205,-1.,-1.26867786804854));
#48061=CARTESIAN_POINT('Ctrl Pts',(1.45301422764205,1.,-1.26867786804854));
#48062=CARTESIAN_POINT('Ctrl Pts',(1.44761985001544,-1.,-1.26570925118767));
#48063=CARTESIAN_POINT('Ctrl Pts',(1.44761985001544,1.,-1.26570925118767));
#48064=CARTESIAN_POINT('Ctrl Pts',(1.44236470511145,-1.,-1.26273903323723));
#48065=CARTESIAN_POINT('Ctrl Pts',(1.44236470511145,1.,-1.26273903323723));
#48066=CARTESIAN_POINT('Ctrl Pts',(1.43734919180719,-1.,-1.25983531011894));
#48067=CARTESIAN_POINT('Ctrl Pts',(1.43734919180719,1.,-1.25983531011894));
#48068=CARTESIAN_POINT('Ctrl Pts',(1.43262645609679,-1.,-1.25702687965744));
#48069=CARTESIAN_POINT('Ctrl Pts',(1.43262645609679,1.,-1.25702687965744));
#48070=CARTESIAN_POINT('Ctrl Pts',(1.42815938799555,-1.,-1.25426945222783));
#48071=CARTESIAN_POINT('Ctrl Pts',(1.42815938799555,1.,-1.25426945222783));
#48072=CARTESIAN_POINT('Ctrl Pts',(1.42378102115911,-1.,-1.25141455570299));
#48073=CARTESIAN_POINT('Ctrl Pts',(1.42378102115911,1.,-1.25141455570299));
#48074=CARTESIAN_POINT('Ctrl Pts',(1.41923722596421,-1.,-1.24824430986911));
#48075=CARTESIAN_POINT('Ctrl Pts',(1.41923722596421,1.,-1.24824430986911));
#48076=CARTESIAN_POINT('Ctrl Pts',(1.41422913175437,-1.,-1.24450600513278));
#48077=CARTESIAN_POINT('Ctrl Pts',(1.41422913175437,1.,-1.24450600513278));
#48078=CARTESIAN_POINT('Ctrl Pts',(1.40845295531151,-1.,-1.23994455029421));
#48079=CARTESIAN_POINT('Ctrl Pts',(1.40845295531151,1.,-1.23994455029421));
#48080=CARTESIAN_POINT('Ctrl Pts',(1.40164708205345,-1.,-1.23434087289768));
#48081=CARTESIAN_POINT('Ctrl Pts',(1.40164708205345,1.,-1.23434087289768));
#48082=CARTESIAN_POINT('Ctrl Pts',(1.39361389567257,-1.,-1.22752961898063));
#48083=CARTESIAN_POINT('Ctrl Pts',(1.39361389567257,1.,-1.22752961898063));
#48084=CARTESIAN_POINT('Ctrl Pts',(1.38420564525391,-1.,-1.21938737278853));
#48085=CARTESIAN_POINT('Ctrl Pts',(1.38420564525391,1.,-1.21938737278853));
#48086=CARTESIAN_POINT('Ctrl Pts',(1.37331915604962,-1.,-1.20982812923113));
#48087=CARTESIAN_POINT('Ctrl Pts',(1.37331915604962,1.,-1.20982812923113));
#48088=CARTESIAN_POINT('Ctrl Pts',(1.36088705040677,-1.,-1.1987959077656));
#48089=CARTESIAN_POINT('Ctrl Pts',(1.36088705040677,1.,-1.1987959077656));
#48090=CARTESIAN_POINT('Ctrl Pts',(1.34687053998157,-1.,-1.18625865664915));
#48091=CARTESIAN_POINT('Ctrl Pts',(1.34687053998157,1.,-1.18625865664915));
#48092=CARTESIAN_POINT('Ctrl Pts',(1.33437539344842,-1.,-1.17501305787994));
#48093=CARTESIAN_POINT('Ctrl Pts',(1.33437539344842,1.,-1.17501305787994));
#48094=CARTESIAN_POINT('Ctrl Pts',(1.32428080720544,-1.,-1.16589330092532));
#48095=CARTESIAN_POINT('Ctrl Pts',(1.32428080720544,1.,-1.16589330092532));
#48096=CARTESIAN_POINT('Ctrl Pts',(1.3172297721596,-1.,-1.15950888730433));
#48097=CARTESIAN_POINT('Ctrl Pts',(1.3172297721596,1.,-1.15950888730433));
#48098=CARTESIAN_POINT('Ctrl Pts',(1.31362392696032,-1.,-1.15624053661742));
#48099=CARTESIAN_POINT('Ctrl Pts',(1.31362392696032,1.,-1.15624053661742));
#48100=CARTESIAN_POINT('',(1.73811241238545,1.,-1.34869019493419));
#48101=CARTESIAN_POINT('Ctrl Pts',(1.73811241238545,1.,-1.34869019493419));
#48102=CARTESIAN_POINT('Ctrl Pts',(1.73682580585819,1.,-1.34854391898145));
#48103=CARTESIAN_POINT('Ctrl Pts',(1.73425417886254,1.,-1.34824783113158));
#48104=CARTESIAN_POINT('Ctrl Pts',(1.73040149654497,1.,-1.3477930915247));
#48105=CARTESIAN_POINT('Ctrl Pts',(1.72527410681298,1.,-1.34716554820013));
#48106=CARTESIAN_POINT('Ctrl Pts',(1.7188807715095,1.,-1.34634568653586));
#48107=CARTESIAN_POINT('Ctrl Pts',(1.71250340687011,1.,-1.34549029589563));
#48108=CARTESIAN_POINT('Ctrl Pts',(1.70614212266676,1.,-1.34459924533783));
#48109=CARTESIAN_POINT('Ctrl Pts',(1.69979707754221,1.,-1.34367237124322));
#48110=CARTESIAN_POINT('Ctrl Pts',(1.6934684849664,1.,-1.34270948206139));
#48111=CARTESIAN_POINT('Ctrl Pts',(1.68715660868602,1.,-1.34171037484673));
#48112=CARTESIAN_POINT('Ctrl Pts',(1.68086176030308,1.,-1.3406748518516));
#48113=CARTESIAN_POINT('Ctrl Pts',(1.67458429426126,1.,-1.33960273470372));
#48114=CARTESIAN_POINT('Ctrl Pts',(1.66832460784078,1.,-1.33849388654458));
#48115=CARTESIAN_POINT('Ctrl Pts',(1.66208312542073,1.,-1.33734820885331));
#48116=CARTESIAN_POINT('Ctrl Pts',(1.65586025952651,1.,-1.33616559745217));
#48117=CARTESIAN_POINT('Ctrl Pts',(1.64965637286843,1.,-1.33494590468003));
#48118=CARTESIAN_POINT('Ctrl Pts',(1.64347174856007,1.,-1.33368890676554));
#48119=CARTESIAN_POINT('Ctrl Pts',(1.63730653475049,1.,-1.33239425103694));
#48120=CARTESIAN_POINT('Ctrl Pts',(1.63116079730887,1.,-1.33106149345618));
#48121=CARTESIAN_POINT('Ctrl Pts',(1.62503464209777,1.,-1.32969019505665));
#48122=CARTESIAN_POINT('Ctrl Pts',(1.61892832270723,1.,-1.32828000610448));
#48123=CARTESIAN_POINT('Ctrl Pts',(1.61284234015762,1.,-1.32683074483365));
#48124=CARTESIAN_POINT('Ctrl Pts',(1.6067775829097,1.,-1.32534250785794));
#48125=CARTESIAN_POINT('Ctrl Pts',(1.600735118587,1.,-1.32381550858266));
#48126=CARTESIAN_POINT('Ctrl Pts',(1.59471591079408,1.,-1.32224985747686));
#48127=CARTESIAN_POINT('Ctrl Pts',(1.58872057258244,1.,-1.32064537110891));
#48128=CARTESIAN_POINT('Ctrl Pts',(1.58274907898829,1.,-1.31900135021428));
#48129=CARTESIAN_POINT('Ctrl Pts',(1.57680056505585,1.,-1.31731642317183));
#48130=CARTESIAN_POINT('Ctrl Pts',(1.57087397835721,1.,-1.31558903860015));
#48131=CARTESIAN_POINT('Ctrl Pts',(1.56496872402352,1.,-1.31381795281002));
#48132=CARTESIAN_POINT('Ctrl Pts',(1.55908521254822,1.,-1.31200264341696));
#48133=CARTESIAN_POINT('Ctrl Pts',(1.55322568759481,1.,-1.31014393684221));
#48134=CARTESIAN_POINT('Ctrl Pts',(1.54739413957183,1.,-1.30824393907471));
#48135=CARTESIAN_POINT('Ctrl Pts',(1.54159462645428,1.,-1.30630475189553));
#48136=CARTESIAN_POINT('Ctrl Pts',(1.53582981268976,1.,-1.30432735639487));
#48137=CARTESIAN_POINT('Ctrl Pts',(1.53009970283893,1.,-1.3023106439557));
#48138=CARTESIAN_POINT('Ctrl Pts',(1.5243995786107,1.,-1.30024984366334));
#48139=CARTESIAN_POINT('Ctrl Pts',(1.51872184912735,1.,-1.29813791800757));
#48140=CARTESIAN_POINT('Ctrl Pts',(1.51305994241412,1.,-1.29596850710518));
#48141=CARTESIAN_POINT('Ctrl Pts',(1.50741159078367,1.,-1.29373841372843));
#48142=CARTESIAN_POINT('Ctrl Pts',(1.50178230149764,1.,-1.29145022885171));
#48143=CARTESIAN_POINT('Ctrl Pts',(1.49618896881729,1.,-1.28911506584232));
#48144=CARTESIAN_POINT('Ctrl Pts',(1.4906522831275,1.,-1.28674676116415));
#48145=CARTESIAN_POINT('Ctrl Pts',(1.48518817118891,1.,-1.28435533880184));
#48146=CARTESIAN_POINT('Ctrl Pts',(1.47980070347102,1.,-1.28194158939522));
#48147=CARTESIAN_POINT('Ctrl Pts',(1.4744717526711,1.,-1.27948918248524));
#48148=CARTESIAN_POINT('Ctrl Pts',(1.46916035917197,1.,-1.27696414831144));
#48149=CARTESIAN_POINT('Ctrl Pts',(1.4638243133254,1.,-1.27433119897877));
#48150=CARTESIAN_POINT('Ctrl Pts',(1.45843906294725,1.,-1.27156805265312));
#48151=CARTESIAN_POINT('Ctrl Pts',(1.45301422764205,1.,-1.26867786804854));
#48152=CARTESIAN_POINT('Ctrl Pts',(1.44761985001544,1.,-1.26570925118767));
#48153=CARTESIAN_POINT('Ctrl Pts',(1.44236470511145,1.,-1.26273903323723));
#48154=CARTESIAN_POINT('Ctrl Pts',(1.43734919180719,1.,-1.25983531011894));
#48155=CARTESIAN_POINT('Ctrl Pts',(1.43262645609679,1.,-1.25702687965744));
#48156=CARTESIAN_POINT('Ctrl Pts',(1.42815938799555,1.,-1.25426945222783));
#48157=CARTESIAN_POINT('Ctrl Pts',(1.42378102115911,1.,-1.25141455570299));
#48158=CARTESIAN_POINT('Ctrl Pts',(1.41923722596421,1.,-1.24824430986911));
#48159=CARTESIAN_POINT('Ctrl Pts',(1.41422913175437,1.,-1.24450600513278));
#48160=CARTESIAN_POINT('Ctrl Pts',(1.40845295531151,1.,-1.23994455029421));
#48161=CARTESIAN_POINT('Ctrl Pts',(1.40164708205345,1.,-1.23434087289768));
#48162=CARTESIAN_POINT('Ctrl Pts',(1.39361389567257,1.,-1.22752961898063));
#48163=CARTESIAN_POINT('Ctrl Pts',(1.38420564525391,1.,-1.21938737278853));
#48164=CARTESIAN_POINT('Ctrl Pts',(1.37331915604962,1.,-1.20982812923113));
#48165=CARTESIAN_POINT('Ctrl Pts',(1.36088705040677,1.,-1.1987959077656));
#48166=CARTESIAN_POINT('Ctrl Pts',(1.34687053998157,1.,-1.18625865664915));
#48167=CARTESIAN_POINT('Ctrl Pts',(1.33437539344842,1.,-1.17501305787994));
#48168=CARTESIAN_POINT('Ctrl Pts',(1.32428080720544,1.,-1.16589330092532));
#48169=CARTESIAN_POINT('Ctrl Pts',(1.3172297721596,1.,-1.15950888730433));
#48170=CARTESIAN_POINT('Ctrl Pts',(1.31362392696032,1.,-1.15624053661742));
#48171=CARTESIAN_POINT('',(1.73811241238545,0.,-1.34869019493419));
#48172=CARTESIAN_POINT('Origin',(1.81978687191668,0.,-1.23627494547115));
#48173=CARTESIAN_POINT('',(1.81978687191668,1.,-1.23627494547115));
#48174=CARTESIAN_POINT('',(1.73811241238545,1.,-1.34869019493419));
#48175=CARTESIAN_POINT('',(1.81978687191668,0.,-1.23627494547115));
#48176=CARTESIAN_POINT('Ctrl Pts',(1.5055822144029,-1.,-0.892032620296855));
#48177=CARTESIAN_POINT('Ctrl Pts',(1.5055822144029,1.,-0.892032620296855));
#48178=CARTESIAN_POINT('Ctrl Pts',(1.50980486807181,-1.,-0.894452006967538));
#48179=CARTESIAN_POINT('Ctrl Pts',(1.50980486807181,1.,-0.894452006967538));
#48180=CARTESIAN_POINT('Ctrl Pts',(1.51805569591479,-1.,-0.89918504749193));
#48181=CARTESIAN_POINT('Ctrl Pts',(1.51805569591479,1.,-0.89918504749193));
#48182=CARTESIAN_POINT('Ctrl Pts',(1.52984849890434,-1.,-0.905967409640499));
#48183=CARTESIAN_POINT('Ctrl Pts',(1.52984849890434,1.,-0.905967409640499));
#48184=CARTESIAN_POINT('Ctrl Pts',(1.54440491152807,-1.,-0.91437591904658));
#48185=CARTESIAN_POINT('Ctrl Pts',(1.54440491152807,1.,-0.91437591904658));
#48186=CARTESIAN_POINT('Ctrl Pts',(1.56065988582509,-1.,-0.923832188966322));
#48187=CARTESIAN_POINT('Ctrl Pts',(1.56065988582509,1.,-0.923832188966322));
#48188=CARTESIAN_POINT('Ctrl Pts',(1.57499388385561,-1.,-0.932246680128849));
#48189=CARTESIAN_POINT('Ctrl Pts',(1.57499388385561,1.,-0.932246680128849));
#48190=CARTESIAN_POINT('Ctrl Pts',(1.58744937489796,-1.,-0.939646377909319));
#48191=CARTESIAN_POINT('Ctrl Pts',(1.58744937489796,1.,-0.939646377909319));
#48192=CARTESIAN_POINT('Ctrl Pts',(1.59810042045408,-1.,-0.946078063325796));
#48193=CARTESIAN_POINT('Ctrl Pts',(1.59810042045408,1.,-0.946078063325796));
#48194=CARTESIAN_POINT('Ctrl Pts',(1.60706069897794,-1.,-0.951613284361248));
#48195=CARTESIAN_POINT('Ctrl Pts',(1.60706069897794,1.,-0.951613284361248));
#48196=CARTESIAN_POINT('Ctrl Pts',(1.61449324337233,-1.,-0.956354422921573));
#48197=CARTESIAN_POINT('Ctrl Pts',(1.61449324337233,1.,-0.956354422921573));
#48198=CARTESIAN_POINT('Ctrl Pts',(1.62061638139929,-1.,-0.960438326099958));
#48199=CARTESIAN_POINT('Ctrl Pts',(1.62061638139929,1.,-0.960438326099958));
#48200=CARTESIAN_POINT('Ctrl Pts',(1.6257193066974,-1.,-0.964046107037821));
#48201=CARTESIAN_POINT('Ctrl Pts',(1.6257193066974,1.,-0.964046107037821));
#48202=CARTESIAN_POINT('Ctrl Pts',(1.63013849959083,-1.,-0.967387853228041));
#48203=CARTESIAN_POINT('Ctrl Pts',(1.63013849959083,1.,-0.967387853228041));
#48204=CARTESIAN_POINT('Ctrl Pts',(1.63420665729609,-1.,-0.970669715996356));
#48205=CARTESIAN_POINT('Ctrl Pts',(1.63420665729609,1.,-0.970669715996356));
#48206=CARTESIAN_POINT('Ctrl Pts',(1.63820952658157,-1.,-0.974066058287501));
#48207=CARTESIAN_POINT('Ctrl Pts',(1.63820952658157,1.,-0.974066058287501));
#48208=CARTESIAN_POINT('Ctrl Pts',(1.64233990826831,-1.,-0.977689794120297));
#48209=CARTESIAN_POINT('Ctrl Pts',(1.64233990826831,1.,-0.977689794120297));
#48210=CARTESIAN_POINT('Ctrl Pts',(1.64665139190834,-1.,-0.981562530940574));
#48211=CARTESIAN_POINT('Ctrl Pts',(1.64665139190834,1.,-0.981562530940574));
#48212=CARTESIAN_POINT('Ctrl Pts',(1.6511001661277,-1.,-0.985642622921626));
#48213=CARTESIAN_POINT('Ctrl Pts',(1.6511001661277,1.,-0.985642622921626));
#48214=CARTESIAN_POINT('Ctrl Pts',(1.65559044289746,-1.,-0.98985562785445));
#48215=CARTESIAN_POINT('Ctrl Pts',(1.65559044289746,1.,-0.98985562785445));
#48216=CARTESIAN_POINT('Ctrl Pts',(1.66001553809916,-1.,-0.994121836661116));
#48217=CARTESIAN_POINT('Ctrl Pts',(1.66001553809916,1.,-0.994121836661116));
#48218=CARTESIAN_POINT('Ctrl Pts',(1.66430758030304,-1.,-0.998389654952317));
#48219=CARTESIAN_POINT('Ctrl Pts',(1.66430758030304,1.,-0.998389654952317));
#48220=CARTESIAN_POINT('Ctrl Pts',(1.66846059277231,-1.,-1.00265091003682));
#48221=CARTESIAN_POINT('Ctrl Pts',(1.66846059277231,1.,-1.00265091003682));
#48222=CARTESIAN_POINT('Ctrl Pts',(1.67250335383248,-1.,-1.00692206696387));
#48223=CARTESIAN_POINT('Ctrl Pts',(1.67250335383248,1.,-1.00692206696387));
#48224=CARTESIAN_POINT('Ctrl Pts',(1.67648246776457,-1.,-1.01123236493507));
#48225=CARTESIAN_POINT('Ctrl Pts',(1.67648246776457,1.,-1.01123236493507));
#48226=CARTESIAN_POINT('Ctrl Pts',(1.6804428989482,-1.,-1.01561026162787));
#48227=CARTESIAN_POINT('Ctrl Pts',(1.6804428989482,1.,-1.01561026162787));
#48228=CARTESIAN_POINT('Ctrl Pts',(1.68440578021739,-1.,-1.02006795074222));
#48229=CARTESIAN_POINT('Ctrl Pts',(1.68440578021739,1.,-1.02006795074222));
#48230=CARTESIAN_POINT('Ctrl Pts',(1.68836910178475,-1.,-1.02460180535272));
#48231=CARTESIAN_POINT('Ctrl Pts',(1.68836910178475,1.,-1.02460180535272));
#48232=CARTESIAN_POINT('Ctrl Pts',(1.69231840863471,-1.,-1.02919977579155));
#48233=CARTESIAN_POINT('Ctrl Pts',(1.69231840863471,1.,-1.02919977579155));
#48234=CARTESIAN_POINT('Ctrl Pts',(1.69623414782769,-1.,-1.03384646003587));
#48235=CARTESIAN_POINT('Ctrl Pts',(1.69623414782769,1.,-1.03384646003587));
#48236=CARTESIAN_POINT('Ctrl Pts',(1.70010052930951,-1.,-1.03852922490782));
#48237=CARTESIAN_POINT('Ctrl Pts',(1.70010052930951,1.,-1.03852922490782));
#48238=CARTESIAN_POINT('Ctrl Pts',(1.70391338707969,-1.,-1.04324363334546));
#48239=CARTESIAN_POINT('Ctrl Pts',(1.70391338707969,1.,-1.04324363334546));
#48240=CARTESIAN_POINT('Ctrl Pts',(1.70767646263641,-1.,-1.0479908540499));
#48241=CARTESIAN_POINT('Ctrl Pts',(1.70767646263641,1.,-1.0479908540499));
#48242=CARTESIAN_POINT('Ctrl Pts',(1.71139783543986,-1.,-1.05277517202854));
#48243=CARTESIAN_POINT('Ctrl Pts',(1.71139783543986,1.,-1.05277517202854));
#48244=CARTESIAN_POINT('Ctrl Pts',(1.71508654427022,-1.,-1.05760163192481));
#48245=CARTESIAN_POINT('Ctrl Pts',(1.71508654427022,1.,-1.05760163192481));
#48246=CARTESIAN_POINT('Ctrl Pts',(1.71874858456908,-1.,-1.0624732468065));
#48247=CARTESIAN_POINT('Ctrl Pts',(1.71874858456908,1.,-1.0624732468065));
#48248=CARTESIAN_POINT('Ctrl Pts',(1.72238500928456,-1.,-1.06738966975463));
#48249=CARTESIAN_POINT('Ctrl Pts',(1.72238500928456,1.,-1.06738966975463));
#48250=CARTESIAN_POINT('Ctrl Pts',(1.72599406198489,-1.,-1.07234866990252));
#48251=CARTESIAN_POINT('Ctrl Pts',(1.72599406198489,1.,-1.07234866990252));
#48252=CARTESIAN_POINT('Ctrl Pts',(1.72957248977424,-1.,-1.0773470373727));
#48253=CARTESIAN_POINT('Ctrl Pts',(1.72957248977424,1.,-1.0773470373727));
#48254=CARTESIAN_POINT('Ctrl Pts',(1.73311705663407,-1.,-1.08238162784749));
#48255=CARTESIAN_POINT('Ctrl Pts',(1.73311705663407,1.,-1.08238162784749));
#48256=CARTESIAN_POINT('Ctrl Pts',(1.73662628326093,-1.,-1.08745056285429));
#48257=CARTESIAN_POINT('Ctrl Pts',(1.73662628326093,1.,-1.08745056285429));
#48258=CARTESIAN_POINT('Ctrl Pts',(1.74010053962252,-1.,-1.09255329056496));
#48259=CARTESIAN_POINT('Ctrl Pts',(1.74010053962252,1.,-1.09255329056496));
#48260=CARTESIAN_POINT('Ctrl Pts',(1.74354119236212,-1.,-1.09768999241229));
#48261=CARTESIAN_POINT('Ctrl Pts',(1.74354119236212,1.,-1.09768999241229));
#48262=CARTESIAN_POINT('Ctrl Pts',(1.74695004214924,-1.,-1.10286118991144));
#48263=CARTESIAN_POINT('Ctrl Pts',(1.74695004214924,1.,-1.10286118991144));
#48264=CARTESIAN_POINT('Ctrl Pts',(1.75032866075914,-1.,-1.10806728183003));
#48265=CARTESIAN_POINT('Ctrl Pts',(1.75032866075914,1.,-1.10806728183003));
#48266=CARTESIAN_POINT('Ctrl Pts',(1.75367772094617,-1.,-1.11330807582542));
#48267=CARTESIAN_POINT('Ctrl Pts',(1.75367772094617,1.,-1.11330807582542));
#48268=CARTESIAN_POINT('Ctrl Pts',(1.75699720772089,-1.,-1.11858293216752));
#48269=CARTESIAN_POINT('Ctrl Pts',(1.75699720772089,1.,-1.11858293216752));
#48270=CARTESIAN_POINT('Ctrl Pts',(1.76028671825084,-1.,-1.12389096855078));
#48271=CARTESIAN_POINT('Ctrl Pts',(1.76028671825084,1.,-1.12389096855078));
#48272=CARTESIAN_POINT('Ctrl Pts',(1.76354571966171,-1.,-1.12923123555076));
#48273=CARTESIAN_POINT('Ctrl Pts',(1.76354571966171,1.,-1.12923123555076));
#48274=CARTESIAN_POINT('Ctrl Pts',(1.76677384551883,-1.,-1.13460291804635));
#48275=CARTESIAN_POINT('Ctrl Pts',(1.76677384551883,1.,-1.13460291804635));
#48276=CARTESIAN_POINT('Ctrl Pts',(1.76997111386806,-1.,-1.14000548337));
#48277=CARTESIAN_POINT('Ctrl Pts',(1.76997111386806,1.,-1.14000548337));
#48278=CARTESIAN_POINT('Ctrl Pts',(1.77313777896234,-1.,-1.14543858226948));
#48279=CARTESIAN_POINT('Ctrl Pts',(1.77313777896234,1.,-1.14543858226948));
#48280=CARTESIAN_POINT('Ctrl Pts',(1.77627422557034,-1.,-1.15090197841531));
#48281=CARTESIAN_POINT('Ctrl Pts',(1.77627422557034,1.,-1.15090197841531));
#48282=CARTESIAN_POINT('Ctrl Pts',(1.77938085564261,-1.,-1.15639547194689));
#48283=CARTESIAN_POINT('Ctrl Pts',(1.77938085564261,1.,-1.15639547194689));
#48284=CARTESIAN_POINT('Ctrl Pts',(1.78245795880949,-1.,-1.16191881298458));
#48285=CARTESIAN_POINT('Ctrl Pts',(1.78245795880949,1.,-1.16191881298458));
#48286=CARTESIAN_POINT('Ctrl Pts',(1.78550566040349,-1.,-1.16747166312239));
#48287=CARTESIAN_POINT('Ctrl Pts',(1.78550566040349,1.,-1.16747166312239));
#48288=CARTESIAN_POINT('Ctrl Pts',(1.78852398877523,-1.,-1.17305363177265));
#48289=CARTESIAN_POINT('Ctrl Pts',(1.78852398877523,1.,-1.17305363177265));
#48290=CARTESIAN_POINT('Ctrl Pts',(1.79151291552646,-1.,-1.17866429440781));
#48291=CARTESIAN_POINT('Ctrl Pts',(1.79151291552646,1.,-1.17866429440781));
#48292=CARTESIAN_POINT('Ctrl Pts',(1.79447240321572,-1.,-1.18430321697471));
#48293=CARTESIAN_POINT('Ctrl Pts',(1.79447240321572,1.,-1.18430321697471));
#48294=CARTESIAN_POINT('Ctrl Pts',(1.79740245923649,-1.,-1.1899699793456));
#48295=CARTESIAN_POINT('Ctrl Pts',(1.79740245923649,1.,-1.1899699793456));
#48296=CARTESIAN_POINT('Ctrl Pts',(1.80030314370121,-1.,-1.19566418930405));
#48297=CARTESIAN_POINT('Ctrl Pts',(1.80030314370121,1.,-1.19566418930405));
#48298=CARTESIAN_POINT('Ctrl Pts',(1.8031745483882,-1.,-1.2013854893912));
#48299=CARTESIAN_POINT('Ctrl Pts',(1.8031745483882,1.,-1.2013854893912));
#48300=CARTESIAN_POINT('Ctrl Pts',(1.80601678480772,-1.,-1.20713356605519));
#48301=CARTESIAN_POINT('Ctrl Pts',(1.80601678480772,1.,-1.20713356605519));
#48302=CARTESIAN_POINT('Ctrl Pts',(1.80882996916931,-1.,-1.2129081570818));
#48303=CARTESIAN_POINT('Ctrl Pts',(1.80882996916931,1.,-1.2129081570818));
#48304=CARTESIAN_POINT('Ctrl Pts',(1.81161420806172,-1.,-1.2187090610323));
#48305=CARTESIAN_POINT('Ctrl Pts',(1.81161420806172,1.,-1.2187090610323));
#48306=CARTESIAN_POINT('Ctrl Pts',(1.81436959209778,-1.,-1.22453613304507));
#48307=CARTESIAN_POINT('Ctrl Pts',(1.81436959209778,1.,-1.22453613304507));
#48308=CARTESIAN_POINT('Ctrl Pts',(1.81655087183054,-1.,-1.22921864890975));
#48309=CARTESIAN_POINT('Ctrl Pts',(1.81655087183054,1.,-1.22921864890975));
#48310=CARTESIAN_POINT('Ctrl Pts',(1.81817389920914,-1.,-1.23274224526804));
#48311=CARTESIAN_POINT('Ctrl Pts',(1.81817389920914,1.,-1.23274224526804));
#48312=CARTESIAN_POINT('Ctrl Pts',(1.81925017193531,-1.,-1.23509651170384));
#48313=CARTESIAN_POINT('Ctrl Pts',(1.81925017193531,1.,-1.23509651170384));
#48314=CARTESIAN_POINT('Ctrl Pts',(1.81978687191668,-1.,-1.23627494547115));
#48315=CARTESIAN_POINT('Ctrl Pts',(1.81978687191668,1.,-1.23627494547115));
#48316=CARTESIAN_POINT('',(1.5055822144029,1.,-0.892032620296855));
#48317=CARTESIAN_POINT('Ctrl Pts',(1.5055822144029,1.,-0.892032620296855));
#48318=CARTESIAN_POINT('Ctrl Pts',(1.50980486807181,1.,-0.894452006967538));
#48319=CARTESIAN_POINT('Ctrl Pts',(1.51805569591479,1.,-0.89918504749193));
#48320=CARTESIAN_POINT('Ctrl Pts',(1.52984849890434,1.,-0.905967409640499));
#48321=CARTESIAN_POINT('Ctrl Pts',(1.54440491152807,1.,-0.91437591904658));
#48322=CARTESIAN_POINT('Ctrl Pts',(1.56065988582509,1.,-0.923832188966322));
#48323=CARTESIAN_POINT('Ctrl Pts',(1.57499388385561,1.,-0.932246680128849));
#48324=CARTESIAN_POINT('Ctrl Pts',(1.58744937489796,1.,-0.939646377909319));
#48325=CARTESIAN_POINT('Ctrl Pts',(1.59810042045408,1.,-0.946078063325796));
#48326=CARTESIAN_POINT('Ctrl Pts',(1.60706069897794,1.,-0.951613284361248));
#48327=CARTESIAN_POINT('Ctrl Pts',(1.61449324337233,1.,-0.956354422921573));
#48328=CARTESIAN_POINT('Ctrl Pts',(1.62061638139929,1.,-0.960438326099958));
#48329=CARTESIAN_POINT('Ctrl Pts',(1.6257193066974,1.,-0.964046107037821));
#48330=CARTESIAN_POINT('Ctrl Pts',(1.63013849959083,1.,-0.967387853228041));
#48331=CARTESIAN_POINT('Ctrl Pts',(1.63420665729609,1.,-0.970669715996356));
#48332=CARTESIAN_POINT('Ctrl Pts',(1.63820952658157,1.,-0.974066058287501));
#48333=CARTESIAN_POINT('Ctrl Pts',(1.64233990826831,1.,-0.977689794120297));
#48334=CARTESIAN_POINT('Ctrl Pts',(1.64665139190834,1.,-0.981562530940574));
#48335=CARTESIAN_POINT('Ctrl Pts',(1.6511001661277,1.,-0.985642622921626));
#48336=CARTESIAN_POINT('Ctrl Pts',(1.65559044289746,1.,-0.98985562785445));
#48337=CARTESIAN_POINT('Ctrl Pts',(1.66001553809916,1.,-0.994121836661116));
#48338=CARTESIAN_POINT('Ctrl Pts',(1.66430758030304,1.,-0.998389654952317));
#48339=CARTESIAN_POINT('Ctrl Pts',(1.66846059277231,1.,-1.00265091003682));
#48340=CARTESIAN_POINT('Ctrl Pts',(1.67250335383248,1.,-1.00692206696387));
#48341=CARTESIAN_POINT('Ctrl Pts',(1.67648246776457,1.,-1.01123236493507));
#48342=CARTESIAN_POINT('Ctrl Pts',(1.6804428989482,1.,-1.01561026162787));
#48343=CARTESIAN_POINT('Ctrl Pts',(1.68440578021739,1.,-1.02006795074222));
#48344=CARTESIAN_POINT('Ctrl Pts',(1.68836910178475,1.,-1.02460180535272));
#48345=CARTESIAN_POINT('Ctrl Pts',(1.69231840863471,1.,-1.02919977579155));
#48346=CARTESIAN_POINT('Ctrl Pts',(1.69623414782769,1.,-1.03384646003587));
#48347=CARTESIAN_POINT('Ctrl Pts',(1.70010052930951,1.,-1.03852922490782));
#48348=CARTESIAN_POINT('Ctrl Pts',(1.70391338707969,1.,-1.04324363334546));
#48349=CARTESIAN_POINT('Ctrl Pts',(1.70767646263641,1.,-1.0479908540499));
#48350=CARTESIAN_POINT('Ctrl Pts',(1.71139783543986,1.,-1.05277517202854));
#48351=CARTESIAN_POINT('Ctrl Pts',(1.71508654427022,1.,-1.05760163192481));
#48352=CARTESIAN_POINT('Ctrl Pts',(1.71874858456908,1.,-1.0624732468065));
#48353=CARTESIAN_POINT('Ctrl Pts',(1.72238500928456,1.,-1.06738966975463));
#48354=CARTESIAN_POINT('Ctrl Pts',(1.72599406198489,1.,-1.07234866990252));
#48355=CARTESIAN_POINT('Ctrl Pts',(1.72957248977424,1.,-1.0773470373727));
#48356=CARTESIAN_POINT('Ctrl Pts',(1.73311705663407,1.,-1.08238162784749));
#48357=CARTESIAN_POINT('Ctrl Pts',(1.73662628326093,1.,-1.08745056285429));
#48358=CARTESIAN_POINT('Ctrl Pts',(1.74010053962252,1.,-1.09255329056496));
#48359=CARTESIAN_POINT('Ctrl Pts',(1.74354119236212,1.,-1.09768999241229));
#48360=CARTESIAN_POINT('Ctrl Pts',(1.74695004214924,1.,-1.10286118991144));
#48361=CARTESIAN_POINT('Ctrl Pts',(1.75032866075914,1.,-1.10806728183003));
#48362=CARTESIAN_POINT('Ctrl Pts',(1.75367772094617,1.,-1.11330807582542));
#48363=CARTESIAN_POINT('Ctrl Pts',(1.75699720772089,1.,-1.11858293216752));
#48364=CARTESIAN_POINT('Ctrl Pts',(1.76028671825084,1.,-1.12389096855078));
#48365=CARTESIAN_POINT('Ctrl Pts',(1.76354571966171,1.,-1.12923123555076));
#48366=CARTESIAN_POINT('Ctrl Pts',(1.76677384551883,1.,-1.13460291804635));
#48367=CARTESIAN_POINT('Ctrl Pts',(1.76997111386806,1.,-1.14000548337));
#48368=CARTESIAN_POINT('Ctrl Pts',(1.77313777896234,1.,-1.14543858226948));
#48369=CARTESIAN_POINT('Ctrl Pts',(1.77627422557034,1.,-1.15090197841531));
#48370=CARTESIAN_POINT('Ctrl Pts',(1.77938085564261,1.,-1.15639547194689));
#48371=CARTESIAN_POINT('Ctrl Pts',(1.78245795880949,1.,-1.16191881298458));
#48372=CARTESIAN_POINT('Ctrl Pts',(1.78550566040349,1.,-1.16747166312239));
#48373=CARTESIAN_POINT('Ctrl Pts',(1.78852398877523,1.,-1.17305363177265));
#48374=CARTESIAN_POINT('Ctrl Pts',(1.79151291552646,1.,-1.17866429440781));
#48375=CARTESIAN_POINT('Ctrl Pts',(1.79447240321572,1.,-1.18430321697471));
#48376=CARTESIAN_POINT('Ctrl Pts',(1.79740245923649,1.,-1.1899699793456));
#48377=CARTESIAN_POINT('Ctrl Pts',(1.80030314370121,1.,-1.19566418930405));
#48378=CARTESIAN_POINT('Ctrl Pts',(1.8031745483882,1.,-1.2013854893912));
#48379=CARTESIAN_POINT('Ctrl Pts',(1.80601678480772,1.,-1.20713356605519));
#48380=CARTESIAN_POINT('Ctrl Pts',(1.80882996916931,1.,-1.2129081570818));
#48381=CARTESIAN_POINT('Ctrl Pts',(1.81161420806172,1.,-1.2187090610323));
#48382=CARTESIAN_POINT('Ctrl Pts',(1.81436959209778,1.,-1.22453613304507));
#48383=CARTESIAN_POINT('Ctrl Pts',(1.81655087183054,1.,-1.22921864890975));
#48384=CARTESIAN_POINT('Ctrl Pts',(1.81817389920914,1.,-1.23274224526804));
#48385=CARTESIAN_POINT('Ctrl Pts',(1.81925017193531,1.,-1.23509651170384));
#48386=CARTESIAN_POINT('Ctrl Pts',(1.81978687191668,1.,-1.23627494547115));
#48387=CARTESIAN_POINT('',(1.5055822144029,0.,-0.892032620296855));
#48388=CARTESIAN_POINT('Origin',(0.,0.,0.));
#48389=CARTESIAN_POINT('',(1.60662857109684,1.,-0.693717979106306));
#48390=CARTESIAN_POINT('Origin',(0.,1.,0.));
#48391=CARTESIAN_POINT('',(1.60662857109684,0.,-0.693717979106308));
#48392=CARTESIAN_POINT('Ctrl Pts',(2.0698113262342,-1.,-0.745574324794401));
#48393=CARTESIAN_POINT('Ctrl Pts',(2.0698113262342,1.,-0.745574324794401));
#48394=CARTESIAN_POINT('Ctrl Pts',(2.06854248895728,-1.,-0.745832791378367));
#48395=CARTESIAN_POINT('Ctrl Pts',(2.06854248895728,1.,-0.745832791378367));
#48396=CARTESIAN_POINT('Ctrl Pts',(2.06600523016815,-1.,-0.746345871544201));
#48397=CARTESIAN_POINT('Ctrl Pts',(2.06600523016815,1.,-0.746345871544201));
#48398=CARTESIAN_POINT('Ctrl Pts',(2.06220058927826,-1.,-0.74710393278792));
#48399=CARTESIAN_POINT('Ctrl Pts',(2.06220058927826,1.,-0.74710393278792));
#48400=CARTESIAN_POINT('Ctrl Pts',(2.05713023031006,-1.,-0.748091554183803));
#48401=CARTESIAN_POINT('Ctrl Pts',(2.05713023031006,1.,-0.748091554183803));
#48402=CARTESIAN_POINT('Ctrl Pts',(2.05079645592154,-1.,-0.749287468665046));
#48403=CARTESIAN_POINT('Ctrl Pts',(2.05079645592154,1.,-0.749287468665046));
#48404=CARTESIAN_POINT('Ctrl Pts',(2.04446689147979,-1.,-0.750444657875576));
#48405=CARTESIAN_POINT('Ctrl Pts',(2.04446689147979,1.,-0.750444657875576));
#48406=CARTESIAN_POINT('Ctrl Pts',(2.03814160092099,-1.,-0.751562963361115));
#48407=CARTESIAN_POINT('Ctrl Pts',(2.03814160092099,1.,-0.751562963361115));
#48408=CARTESIAN_POINT('Ctrl Pts',(2.03182068456221,-1.,-0.752642180487211));
#48409=CARTESIAN_POINT('Ctrl Pts',(2.03182068456221,1.,-0.752642180487211));
#48410=CARTESIAN_POINT('Ctrl Pts',(2.02550428623313,-1.,-0.753682061112768));
#48411=CARTESIAN_POINT('Ctrl Pts',(2.02550428623313,1.,-0.753682061112768));
#48412=CARTESIAN_POINT('Ctrl Pts',(2.01919259405809,-1.,-0.754682330722816));
#48413=CARTESIAN_POINT('Ctrl Pts',(2.01919259405809,1.,-0.754682330722816));
#48414=CARTESIAN_POINT('Ctrl Pts',(2.01288584328084,-1.,-0.755642704957865));
#48415=CARTESIAN_POINT('Ctrl Pts',(2.01288584328084,1.,-0.755642704957865));
#48416=CARTESIAN_POINT('Ctrl Pts',(2.0065843158773,-1.,-0.756562904646671));
#48417=CARTESIAN_POINT('Ctrl Pts',(2.0065843158773,1.,-0.756562904646671));
#48418=CARTESIAN_POINT('Ctrl Pts',(2.00028834739178,-1.,-0.757442676862724));
#48419=CARTESIAN_POINT('Ctrl Pts',(2.00028834739178,1.,-0.757442676862724));
#48420=CARTESIAN_POINT('Ctrl Pts',(1.99399831098817,-1.,-0.758281796766761));
#48421=CARTESIAN_POINT('Ctrl Pts',(1.99399831098817,1.,-0.758281796766761));
#48422=CARTESIAN_POINT('Ctrl Pts',(1.98771456680874,-1.,-0.759080037802488));
#48423=CARTESIAN_POINT('Ctrl Pts',(1.98771456680874,1.,-0.759080037802488));
#48424=CARTESIAN_POINT('Ctrl Pts',(1.98143741418172,-1.,-0.75983714745219));
#48425=CARTESIAN_POINT('Ctrl Pts',(1.98143741418172,1.,-0.75983714745219));
#48426=CARTESIAN_POINT('Ctrl Pts',(1.97516705321494,-1.,-0.760552825409757));
#48427=CARTESIAN_POINT('Ctrl Pts',(1.97516705321494,1.,-0.760552825409757));
#48428=CARTESIAN_POINT('Ctrl Pts',(1.96890351582499,-1.,-0.761226690483821));
#48429=CARTESIAN_POINT('Ctrl Pts',(1.96890351582499,1.,-0.761226690483821));
#48430=CARTESIAN_POINT('Ctrl Pts',(1.96264672744186,-1.,-0.761858300014424));
#48431=CARTESIAN_POINT('Ctrl Pts',(1.96264672744186,1.,-0.761858300014424));
#48432=CARTESIAN_POINT('Ctrl Pts',(1.95639665309869,-1.,-0.762447203806179));
#48433=CARTESIAN_POINT('Ctrl Pts',(1.95639665309869,1.,-0.762447203806179));
#48434=CARTESIAN_POINT('Ctrl Pts',(1.95015342590024,-1.,-0.762992990878769));
#48435=CARTESIAN_POINT('Ctrl Pts',(1.95015342590024,1.,-0.762992990878769));
#48436=CARTESIAN_POINT('Ctrl Pts',(1.9439174661764,-1.,-0.763495333538629));
#48437=CARTESIAN_POINT('Ctrl Pts',(1.9439174661764,1.,-0.763495333538629));
#48438=CARTESIAN_POINT('Ctrl Pts',(1.93768964875886,-1.,-0.763954049121459));
#48439=CARTESIAN_POINT('Ctrl Pts',(1.93768964875886,1.,-0.763954049121459));
#48440=CARTESIAN_POINT('Ctrl Pts',(1.93147105496382,-1.,-0.764369010673941));
#48441=CARTESIAN_POINT('Ctrl Pts',(1.93147105496382,1.,-0.764369010673941));
#48442=CARTESIAN_POINT('Ctrl Pts',(1.92526263537048,-1.,-0.764740025488212));
#48443=CARTESIAN_POINT('Ctrl Pts',(1.92526263537048,1.,-0.764740025488212));
#48444=CARTESIAN_POINT('Ctrl Pts',(1.91906491634196,-1.,-0.765066729667089));
#48445=CARTESIAN_POINT('Ctrl Pts',(1.91906491634196,1.,-0.765066729667089));
#48446=CARTESIAN_POINT('Ctrl Pts',(1.91287765805169,-1.,-0.765348465884722));
#48447=CARTESIAN_POINT('Ctrl Pts',(1.91287765805169,1.,-0.765348465884722));
#48448=CARTESIAN_POINT('Ctrl Pts',(1.90669961402356,-1.,-0.765584196937919));
#48449=CARTESIAN_POINT('Ctrl Pts',(1.90669961402356,1.,-0.765584196937919));
#48450=CARTESIAN_POINT('Ctrl Pts',(1.90052930393596,-1.,-0.765772772593386));
#48451=CARTESIAN_POINT('Ctrl Pts',(1.90052930393596,1.,-0.765772772593386));
#48452=CARTESIAN_POINT('Ctrl Pts',(1.89436577771388,-1.,-0.765913193856978));
#48453=CARTESIAN_POINT('Ctrl Pts',(1.89436577771388,1.,-0.765913193856978));
#48454=CARTESIAN_POINT('Ctrl Pts',(1.88820926433409,-1.,-0.766004837062091));
#48455=CARTESIAN_POINT('Ctrl Pts',(1.88820926433409,1.,-0.766004837062091));
#48456=CARTESIAN_POINT('Ctrl Pts',(1.88206215302561,-1.,-0.766047794851865));
#48457=CARTESIAN_POINT('Ctrl Pts',(1.88206215302561,1.,-0.766047794851865));
#48458=CARTESIAN_POINT('Ctrl Pts',(1.87592888967883,-1.,-0.766042837036744));
#48459=CARTESIAN_POINT('Ctrl Pts',(1.87592888967883,1.,-0.766042837036744));
#48460=CARTESIAN_POINT('Ctrl Pts',(1.86981398314341,-1.,-0.765990708546091));
#48461=CARTESIAN_POINT('Ctrl Pts',(1.86981398314341,1.,-0.765990708546091));
#48462=CARTESIAN_POINT('Ctrl Pts',(1.86372027063312,-1.,-0.765891519092547));
#48463=CARTESIAN_POINT('Ctrl Pts',(1.86372027063312,1.,-0.765891519092547));
#48464=CARTESIAN_POINT('Ctrl Pts',(1.85764741390394,-1.,-0.765744212909319));
#48465=CARTESIAN_POINT('Ctrl Pts',(1.85764741390394,1.,-0.765744212909319));
#48466=CARTESIAN_POINT('Ctrl Pts',(1.85158945130063,-1.,-0.765545710619063));
#48467=CARTESIAN_POINT('Ctrl Pts',(1.85158945130063,1.,-0.765545710619063));
#48468=CARTESIAN_POINT('Ctrl Pts',(1.84553698875924,-1.,-0.765291664862029));
#48469=CARTESIAN_POINT('Ctrl Pts',(1.84553698875924,1.,-0.765291664862029));
#48470=CARTESIAN_POINT('Ctrl Pts',(1.83948181064835,-1.,-0.764978057881738));
#48471=CARTESIAN_POINT('Ctrl Pts',(1.83948181064835,1.,-0.764978057881738));
#48472=CARTESIAN_POINT('Ctrl Pts',(1.83342077227142,-1.,-0.764602549687853));
#48473=CARTESIAN_POINT('Ctrl Pts',(1.83342077227142,1.,-0.764602549687853));
#48474=CARTESIAN_POINT('Ctrl Pts',(1.82735991200065,-1.,-0.764165902605995));
#48475=CARTESIAN_POINT('Ctrl Pts',(1.82735991200065,1.,-0.764165902605995));
#48476=CARTESIAN_POINT('Ctrl Pts',(1.82131873145266,-1.,-0.763673465462727));
#48477=CARTESIAN_POINT('Ctrl Pts',(1.82131873145266,1.,-0.763673465462727));
#48478=CARTESIAN_POINT('Ctrl Pts',(1.8153211840553,-1.,-0.763132003836634));
#48479=CARTESIAN_POINT('Ctrl Pts',(1.8153211840553,1.,-0.763132003836634));
#48480=CARTESIAN_POINT('Ctrl Pts',(1.80938551463965,-1.,-0.762546129463938));
#48481=CARTESIAN_POINT('Ctrl Pts',(1.80938551463965,1.,-0.762546129463938));
#48482=CARTESIAN_POINT('Ctrl Pts',(1.80351583877342,-1.,-0.761915336443547));
#48483=CARTESIAN_POINT('Ctrl Pts',(1.80351583877342,1.,-0.761915336443547));
#48484=CARTESIAN_POINT('Ctrl Pts',(1.79768986997783,-1.,-0.761229695230558));
#48485=CARTESIAN_POINT('Ctrl Pts',(1.79768986997783,1.,-0.761229695230558));
#48486=CARTESIAN_POINT('Ctrl Pts',(1.7918581561088,-1.,-0.760469555880749));
#48487=CARTESIAN_POINT('Ctrl Pts',(1.7918581561088,1.,-0.760469555880749));
#48488=CARTESIAN_POINT('Ctrl Pts',(1.78596964884604,-1.,-0.75961440111019));
#48489=CARTESIAN_POINT('Ctrl Pts',(1.78596964884604,1.,-0.75961440111019));
#48490=CARTESIAN_POINT('Ctrl Pts',(1.77999411220945,-1.,-0.758650626677519));
#48491=CARTESIAN_POINT('Ctrl Pts',(1.77999411220945,1.,-0.758650626677519));
#48492=CARTESIAN_POINT('Ctrl Pts',(1.77394167108292,-1.,-0.757578264077029));
#48493=CARTESIAN_POINT('Ctrl Pts',(1.77394167108292,1.,-0.757578264077029));
#48494=CARTESIAN_POINT('Ctrl Pts',(1.76789396002998,-1.,-0.75642189602781));
#48495=CARTESIAN_POINT('Ctrl Pts',(1.76789396002998,1.,-0.75642189602781));
#48496=CARTESIAN_POINT('Ctrl Pts',(1.76197817240128,-1.,-0.755220979974462));
#48497=CARTESIAN_POINT('Ctrl Pts',(1.76197817240128,1.,-0.755220979974462));
#48498=CARTESIAN_POINT('Ctrl Pts',(1.75631083600019,-1.,-0.754009254027829));
#48499=CARTESIAN_POINT('Ctrl Pts',(1.75631083600019,1.,-0.754009254027829));
#48500=CARTESIAN_POINT('Ctrl Pts',(1.75095139468794,-1.,-0.752797683531314));
#48501=CARTESIAN_POINT('Ctrl Pts',(1.75095139468794,1.,-0.752797683531314));
#48502=CARTESIAN_POINT('Ctrl Pts',(1.74585086852502,-1.,-0.751555614164483));
#48503=CARTESIAN_POINT('Ctrl Pts',(1.74585086852502,1.,-0.751555614164483));
#48504=CARTESIAN_POINT('Ctrl Pts',(1.74080458267114,-1.,-0.75019343598125));
#48505=CARTESIAN_POINT('Ctrl Pts',(1.74080458267114,1.,-0.75019343598125));
#48506=CARTESIAN_POINT('Ctrl Pts',(1.7355035168033,-1.,-0.74858246295687));
#48507=CARTESIAN_POINT('Ctrl Pts',(1.7355035168033,1.,-0.74858246295687));
#48508=CARTESIAN_POINT('Ctrl Pts',(1.72958533647714,-1.,-0.746574710097752));
#48509=CARTESIAN_POINT('Ctrl Pts',(1.72958533647714,1.,-0.746574710097752));
#48510=CARTESIAN_POINT('Ctrl Pts',(1.72268229916769,-1.,-0.744021445433094));
#48511=CARTESIAN_POINT('Ctrl Pts',(1.72268229916769,1.,-0.744021445433094));
#48512=CARTESIAN_POINT('Ctrl Pts',(1.71447789751001,-1.,-0.74079516202821));
#48513=CARTESIAN_POINT('Ctrl Pts',(1.71447789751001,1.,-0.74079516202821));
#48514=CARTESIAN_POINT('Ctrl Pts',(1.70473309004249,-1.,-0.736799665716932));
#48515=CARTESIAN_POINT('Ctrl Pts',(1.70473309004249,1.,-0.736799665716932));
#48516=CARTESIAN_POINT('Ctrl Pts',(1.69326921972915,-1.,-0.731963238685357));
#48517=CARTESIAN_POINT('Ctrl Pts',(1.69326921972915,1.,-0.731963238685357));
#48518=CARTESIAN_POINT('Ctrl Pts',(1.67996158451922,-1.,-0.726235967982445));
#48519=CARTESIAN_POINT('Ctrl Pts',(1.67996158451922,1.,-0.726235967982445));
#48520=CARTESIAN_POINT('Ctrl Pts',(1.66472880551777,-1.,-0.71958543378795));
#48521=CARTESIAN_POINT('Ctrl Pts',(1.66472880551777,1.,-0.71958543378795));
#48522=CARTESIAN_POINT('Ctrl Pts',(1.64752408828442,-1.,-0.711993139340448));
#48523=CARTESIAN_POINT('Ctrl Pts',(1.64752408828442,1.,-0.711993139340448));
#48524=CARTESIAN_POINT('Ctrl Pts',(1.6321654166204,-1.,-0.705159151977294));
#48525=CARTESIAN_POINT('Ctrl Pts',(1.6321654166204,1.,-0.705159151977294));
#48526=CARTESIAN_POINT('Ctrl Pts',(1.61974673471117,-1.,-0.699605146398837));
#48527=CARTESIAN_POINT('Ctrl Pts',(1.61974673471117,1.,-0.699605146398837));
#48528=CARTESIAN_POINT('Ctrl Pts',(1.61106790957619,-1.,-0.69571209787897));
#48529=CARTESIAN_POINT('Ctrl Pts',(1.61106790957619,1.,-0.69571209787897));
#48530=CARTESIAN_POINT('Ctrl Pts',(1.60662857109684,-1.,-0.693717979106306));
#48531=CARTESIAN_POINT('Ctrl Pts',(1.60662857109684,1.,-0.693717979106306));
#48532=CARTESIAN_POINT('',(2.0698113262342,1.,-0.745574324794401));
#48533=CARTESIAN_POINT('Ctrl Pts',(2.0698113262342,1.,-0.745574324794401));
#48534=CARTESIAN_POINT('Ctrl Pts',(2.06854248895728,1.,-0.745832791378367));
#48535=CARTESIAN_POINT('Ctrl Pts',(2.06600523016815,1.,-0.746345871544201));
#48536=CARTESIAN_POINT('Ctrl Pts',(2.06220058927826,1.,-0.74710393278792));
#48537=CARTESIAN_POINT('Ctrl Pts',(2.05713023031006,1.,-0.748091554183803));
#48538=CARTESIAN_POINT('Ctrl Pts',(2.05079645592154,1.,-0.749287468665046));
#48539=CARTESIAN_POINT('Ctrl Pts',(2.04446689147979,1.,-0.750444657875576));
#48540=CARTESIAN_POINT('Ctrl Pts',(2.03814160092099,1.,-0.751562963361115));
#48541=CARTESIAN_POINT('Ctrl Pts',(2.03182068456221,1.,-0.752642180487211));
#48542=CARTESIAN_POINT('Ctrl Pts',(2.02550428623313,1.,-0.753682061112768));
#48543=CARTESIAN_POINT('Ctrl Pts',(2.01919259405809,1.,-0.754682330722816));
#48544=CARTESIAN_POINT('Ctrl Pts',(2.01288584328084,1.,-0.755642704957865));
#48545=CARTESIAN_POINT('Ctrl Pts',(2.0065843158773,1.,-0.756562904646671));
#48546=CARTESIAN_POINT('Ctrl Pts',(2.00028834739178,1.,-0.757442676862724));
#48547=CARTESIAN_POINT('Ctrl Pts',(1.99399831098817,1.,-0.758281796766761));
#48548=CARTESIAN_POINT('Ctrl Pts',(1.98771456680874,1.,-0.759080037802488));
#48549=CARTESIAN_POINT('Ctrl Pts',(1.98143741418172,1.,-0.75983714745219));
#48550=CARTESIAN_POINT('Ctrl Pts',(1.97516705321494,1.,-0.760552825409757));
#48551=CARTESIAN_POINT('Ctrl Pts',(1.96890351582499,1.,-0.761226690483821));
#48552=CARTESIAN_POINT('Ctrl Pts',(1.96264672744186,1.,-0.761858300014424));
#48553=CARTESIAN_POINT('Ctrl Pts',(1.95639665309869,1.,-0.762447203806179));
#48554=CARTESIAN_POINT('Ctrl Pts',(1.95015342590024,1.,-0.762992990878769));
#48555=CARTESIAN_POINT('Ctrl Pts',(1.9439174661764,1.,-0.763495333538629));
#48556=CARTESIAN_POINT('Ctrl Pts',(1.93768964875886,1.,-0.763954049121459));
#48557=CARTESIAN_POINT('Ctrl Pts',(1.93147105496382,1.,-0.764369010673941));
#48558=CARTESIAN_POINT('Ctrl Pts',(1.92526263537048,1.,-0.764740025488212));
#48559=CARTESIAN_POINT('Ctrl Pts',(1.91906491634196,1.,-0.765066729667089));
#48560=CARTESIAN_POINT('Ctrl Pts',(1.91287765805169,1.,-0.765348465884722));
#48561=CARTESIAN_POINT('Ctrl Pts',(1.90669961402356,1.,-0.765584196937919));
#48562=CARTESIAN_POINT('Ctrl Pts',(1.90052930393596,1.,-0.765772772593386));
#48563=CARTESIAN_POINT('Ctrl Pts',(1.89436577771388,1.,-0.765913193856978));
#48564=CARTESIAN_POINT('Ctrl Pts',(1.88820926433409,1.,-0.766004837062091));
#48565=CARTESIAN_POINT('Ctrl Pts',(1.88206215302561,1.,-0.766047794851865));
#48566=CARTESIAN_POINT('Ctrl Pts',(1.87592888967883,1.,-0.766042837036744));
#48567=CARTESIAN_POINT('Ctrl Pts',(1.86981398314341,1.,-0.765990708546091));
#48568=CARTESIAN_POINT('Ctrl Pts',(1.86372027063312,1.,-0.765891519092547));
#48569=CARTESIAN_POINT('Ctrl Pts',(1.85764741390394,1.,-0.765744212909319));
#48570=CARTESIAN_POINT('Ctrl Pts',(1.85158945130063,1.,-0.765545710619063));
#48571=CARTESIAN_POINT('Ctrl Pts',(1.84553698875924,1.,-0.765291664862029));
#48572=CARTESIAN_POINT('Ctrl Pts',(1.83948181064835,1.,-0.764978057881738));
#48573=CARTESIAN_POINT('Ctrl Pts',(1.83342077227142,1.,-0.764602549687853));
#48574=CARTESIAN_POINT('Ctrl Pts',(1.82735991200065,1.,-0.764165902605995));
#48575=CARTESIAN_POINT('Ctrl Pts',(1.82131873145266,1.,-0.763673465462727));
#48576=CARTESIAN_POINT('Ctrl Pts',(1.8153211840553,1.,-0.763132003836634));
#48577=CARTESIAN_POINT('Ctrl Pts',(1.80938551463965,1.,-0.762546129463938));
#48578=CARTESIAN_POINT('Ctrl Pts',(1.80351583877342,1.,-0.761915336443547));
#48579=CARTESIAN_POINT('Ctrl Pts',(1.79768986997783,1.,-0.761229695230558));
#48580=CARTESIAN_POINT('Ctrl Pts',(1.7918581561088,1.,-0.760469555880749));
#48581=CARTESIAN_POINT('Ctrl Pts',(1.78596964884604,1.,-0.75961440111019));
#48582=CARTESIAN_POINT('Ctrl Pts',(1.77999411220945,1.,-0.758650626677519));
#48583=CARTESIAN_POINT('Ctrl Pts',(1.77394167108292,1.,-0.757578264077029));
#48584=CARTESIAN_POINT('Ctrl Pts',(1.76789396002998,1.,-0.75642189602781));
#48585=CARTESIAN_POINT('Ctrl Pts',(1.76197817240128,1.,-0.755220979974462));
#48586=CARTESIAN_POINT('Ctrl Pts',(1.75631083600019,1.,-0.754009254027829));
#48587=CARTESIAN_POINT('Ctrl Pts',(1.75095139468794,1.,-0.752797683531314));
#48588=CARTESIAN_POINT('Ctrl Pts',(1.74585086852502,1.,-0.751555614164483));
#48589=CARTESIAN_POINT('Ctrl Pts',(1.74080458267114,1.,-0.75019343598125));
#48590=CARTESIAN_POINT('Ctrl Pts',(1.7355035168033,1.,-0.74858246295687));
#48591=CARTESIAN_POINT('Ctrl Pts',(1.72958533647714,1.,-0.746574710097752));
#48592=CARTESIAN_POINT('Ctrl Pts',(1.72268229916769,1.,-0.744021445433094));
#48593=CARTESIAN_POINT('Ctrl Pts',(1.71447789751001,1.,-0.74079516202821));
#48594=CARTESIAN_POINT('Ctrl Pts',(1.70473309004249,1.,-0.736799665716932));
#48595=CARTESIAN_POINT('Ctrl Pts',(1.69326921972915,1.,-0.731963238685357));
#48596=CARTESIAN_POINT('Ctrl Pts',(1.67996158451922,1.,-0.726235967982445));
#48597=CARTESIAN_POINT('Ctrl Pts',(1.66472880551777,1.,-0.71958543378795));
#48598=CARTESIAN_POINT('Ctrl Pts',(1.64752408828442,1.,-0.711993139340448));
#48599=CARTESIAN_POINT('Ctrl Pts',(1.6321654166204,1.,-0.705159151977294));
#48600=CARTESIAN_POINT('Ctrl Pts',(1.61974673471117,1.,-0.699605146398837));
#48601=CARTESIAN_POINT('Ctrl Pts',(1.61106790957619,1.,-0.69571209787897));
#48602=CARTESIAN_POINT('Ctrl Pts',(1.60662857109684,1.,-0.693717979106306));
#48603=CARTESIAN_POINT('',(2.0698113262342,0.,-0.745574324794401));
#48604=CARTESIAN_POINT('Origin',(2.11275013067528,0.,-0.61342227326009));
#48605=CARTESIAN_POINT('',(2.11275013067528,1.,-0.61342227326009));
#48606=CARTESIAN_POINT('',(2.0698113262342,1.,-0.745574324794401));
#48607=CARTESIAN_POINT('',(2.11275013067528,0.,-0.61342227326009));
#48608=CARTESIAN_POINT('Ctrl Pts',(1.7075470150345,-1.,-0.383122945602004));
#48609=CARTESIAN_POINT('Ctrl Pts',(1.7075470150345,1.,-0.383122945602004));
#48610=CARTESIAN_POINT('Ctrl Pts',(1.71231062891958,-1.,-0.384119047315542));
#48611=CARTESIAN_POINT('Ctrl Pts',(1.71231062891958,1.,-0.384119047315542));
#48612=CARTESIAN_POINT('Ctrl Pts',(1.72162022246158,-1.,-0.38607079032701));
#48613=CARTESIAN_POINT('Ctrl Pts',(1.72162022246158,1.,-0.38607079032701));
#48614=CARTESIAN_POINT('Ctrl Pts',(1.7349317097561,-1.,-0.388877023509192));
#48615=CARTESIAN_POINT('Ctrl Pts',(1.7349317097561,1.,-0.388877023509192));
#48616=CARTESIAN_POINT('Ctrl Pts',(1.75137405313962,-1.,-0.392375812294307));
#48617=CARTESIAN_POINT('Ctrl Pts',(1.75137405313962,1.,-0.392375812294307));
#48618=CARTESIAN_POINT('Ctrl Pts',(1.7697556004756,-1.,-0.39634619612042));
#48619=CARTESIAN_POINT('Ctrl Pts',(1.7697556004756,1.,-0.39634619612042));
#48620=CARTESIAN_POINT('Ctrl Pts',(1.78598826347533,-1.,-0.399919403783081));
#48621=CARTESIAN_POINT('Ctrl Pts',(1.78598826347533,1.,-0.399919403783081));
#48622=CARTESIAN_POINT('Ctrl Pts',(1.80012077176221,-1.,-0.403107976170441));
#48623=CARTESIAN_POINT('Ctrl Pts',(1.80012077176221,1.,-0.403107976170441));
#48624=CARTESIAN_POINT('Ctrl Pts',(1.81223801813988,-1.,-0.405933518411838));
#48625=CARTESIAN_POINT('Ctrl Pts',(1.81223801813988,1.,-0.405933518411838));
#48626=CARTESIAN_POINT('Ctrl Pts',(1.8224702267854,-1.,-0.408428948108534));
#48627=CARTESIAN_POINT('Ctrl Pts',(1.8224702267854,1.,-0.408428948108534));
#48628=CARTESIAN_POINT('Ctrl Pts',(1.83100408895216,-1.,-0.410641256301675));
#48629=CARTESIAN_POINT('Ctrl Pts',(1.83100408895216,1.,-0.410641256301675));
#48630=CARTESIAN_POINT('Ctrl Pts',(1.83808953475839,-1.,-0.412633125322162));
#48631=CARTESIAN_POINT('Ctrl Pts',(1.83808953475839,1.,-0.412633125322162));
#48632=CARTESIAN_POINT('Ctrl Pts',(1.8440575707371,-1.,-0.41448743825434));
#48633=CARTESIAN_POINT('Ctrl Pts',(1.8440575707371,1.,-0.41448743825434));
#48634=CARTESIAN_POINT('Ctrl Pts',(1.84929312929882,-1.,-0.416300022038864));
#48635=CARTESIAN_POINT('Ctrl Pts',(1.84929312929882,1.,-0.416300022038864));
#48636=CARTESIAN_POINT('Ctrl Pts',(1.85417632856234,-1.,-0.418164129143534));
#48637=CARTESIAN_POINT('Ctrl Pts',(1.85417632856234,1.,-0.418164129143534));
#48638=CARTESIAN_POINT('Ctrl Pts',(1.85903281096686,-1.,-0.42015728797562));
#48639=CARTESIAN_POINT('Ctrl Pts',(1.85903281096686,1.,-0.42015728797562));
#48640=CARTESIAN_POINT('Ctrl Pts',(1.86408083334028,-1.,-0.422327307418275));
#48641=CARTESIAN_POINT('Ctrl Pts',(1.86408083334028,1.,-0.422327307418275));
#48642=CARTESIAN_POINT('Ctrl Pts',(1.86937803944323,-1.,-0.424678177291359));
#48643=CARTESIAN_POINT('Ctrl Pts',(1.86937803944323,1.,-0.424678177291359));
#48644=CARTESIAN_POINT('Ctrl Pts',(1.87486989291484,-1.,-0.427183828519102));
#48645=CARTESIAN_POINT('Ctrl Pts',(1.87486989291484,1.,-0.427183828519102));
#48646=CARTESIAN_POINT('Ctrl Pts',(1.88044229001832,-1.,-0.429803062482345));
#48647=CARTESIAN_POINT('Ctrl Pts',(1.88044229001832,1.,-0.429803062482345));
#48648=CARTESIAN_POINT('Ctrl Pts',(1.88596913666793,-1.,-0.432493038548748));
#48649=CARTESIAN_POINT('Ctrl Pts',(1.88596913666793,1.,-0.432493038548748));
#48650=CARTESIAN_POINT('Ctrl Pts',(1.89136993975504,-1.,-0.435225660963383));
#48651=CARTESIAN_POINT('Ctrl Pts',(1.89136993975504,1.,-0.435225660963383));
#48652=CARTESIAN_POINT('Ctrl Pts',(1.89663648956466,-1.,-0.437995003948244));
#48653=CARTESIAN_POINT('Ctrl Pts',(1.89663648956466,1.,-0.437995003948244));
#48654=CARTESIAN_POINT('Ctrl Pts',(1.90180124389086,-1.,-0.440807833704038));
#48655=CARTESIAN_POINT('Ctrl Pts',(1.90180124389086,1.,-0.440807833704038));
#48656=CARTESIAN_POINT('Ctrl Pts',(1.90691756144898,-1.,-0.443677556849151));
#48657=CARTESIAN_POINT('Ctrl Pts',(1.90691756144898,1.,-0.443677556849151));
#48658=CARTESIAN_POINT('Ctrl Pts',(1.9120369998112,-1.,-0.446617343485711));
#48659=CARTESIAN_POINT('Ctrl Pts',(1.9120369998112,1.,-0.446617343485711));
#48660=CARTESIAN_POINT('Ctrl Pts',(1.91718342555755,-1.,-0.449632260106662));
#48661=CARTESIAN_POINT('Ctrl Pts',(1.91718342555755,1.,-0.449632260106662));
#48662=CARTESIAN_POINT('Ctrl Pts',(1.92235380648502,-1.,-0.452719478359433));
#48663=CARTESIAN_POINT('Ctrl Pts',(1.92235380648502,1.,-0.452719478359433));
#48664=CARTESIAN_POINT('Ctrl Pts',(1.92753067150476,-1.,-0.455872005174371));
#48665=CARTESIAN_POINT('Ctrl Pts',(1.92753067150476,1.,-0.455872005174371));
#48666=CARTESIAN_POINT('Ctrl Pts',(1.93269066517934,-1.,-0.459081234547926));
#48667=CARTESIAN_POINT('Ctrl Pts',(1.93269066517934,1.,-0.459081234547926));
#48668=CARTESIAN_POINT('Ctrl Pts',(1.93781486640821,-1.,-0.462340031009057));
#48669=CARTESIAN_POINT('Ctrl Pts',(1.93781486640821,1.,-0.462340031009057));
#48670=CARTESIAN_POINT('Ctrl Pts',(1.9428979419619,-1.,-0.46564546202603));
#48671=CARTESIAN_POINT('Ctrl Pts',(1.9428979419619,1.,-0.46564546202603));
#48672=CARTESIAN_POINT('Ctrl Pts',(1.94794381136514,-1.,-0.468997482913135));
#48673=CARTESIAN_POINT('Ctrl Pts',(1.94794381136514,1.,-0.468997482913135));
#48674=CARTESIAN_POINT('Ctrl Pts',(1.95296148278133,-1.,-0.472397672264072));
#48675=CARTESIAN_POINT('Ctrl Pts',(1.95296148278133,1.,-0.472397672264072));
#48676=CARTESIAN_POINT('Ctrl Pts',(1.95796111148177,-1.,-0.475848034683176));
#48677=CARTESIAN_POINT('Ctrl Pts',(1.95796111148177,1.,-0.475848034683176));
#48678=CARTESIAN_POINT('Ctrl Pts',(1.96294933055943,-1.,-0.479349583074855));
#48679=CARTESIAN_POINT('Ctrl Pts',(1.96294933055943,1.,-0.479349583074855));
#48680=CARTESIAN_POINT('Ctrl Pts',(1.96792703422362,-1.,-0.482901662120691));
#48681=CARTESIAN_POINT('Ctrl Pts',(1.96792703422362,1.,-0.482901662120691));
#48682=CARTESIAN_POINT('Ctrl Pts',(1.97289186263272,-1.,-0.486502692907659));
#48683=CARTESIAN_POINT('Ctrl Pts',(1.97289186263272,1.,-0.486502692907659));
#48684=CARTESIAN_POINT('Ctrl Pts',(1.97783973019229,-1.,-0.490150627860953));
#48685=CARTESIAN_POINT('Ctrl Pts',(1.97783973019229,1.,-0.490150627860953));
#48686=CARTESIAN_POINT('Ctrl Pts',(1.98276658761821,-1.,-0.493843476541495));
#48687=CARTESIAN_POINT('Ctrl Pts',(1.98276658761821,1.,-0.493843476541495));
#48688=CARTESIAN_POINT('Ctrl Pts',(1.98767044752932,-1.,-0.497579909545574));
#48689=CARTESIAN_POINT('Ctrl Pts',(1.98767044752932,1.,-0.497579909545574));
#48690=CARTESIAN_POINT('Ctrl Pts',(1.99255149126155,-1.,-0.501359287727146));
#48691=CARTESIAN_POINT('Ctrl Pts',(1.99255149126155,1.,-0.501359287727146));
#48692=CARTESIAN_POINT('Ctrl Pts',(1.99741107463572,-1.,-0.505181361323026));
#48693=CARTESIAN_POINT('Ctrl Pts',(1.99741107463572,1.,-0.505181361323026));
#48694=CARTESIAN_POINT('Ctrl Pts',(2.00225107134734,-1.,-0.509046069886157));
#48695=CARTESIAN_POINT('Ctrl Pts',(2.00225107134734,1.,-0.509046069886157));
#48696=CARTESIAN_POINT('Ctrl Pts',(2.00707309946949,-1.,-0.512953306961793));
#48697=CARTESIAN_POINT('Ctrl Pts',(2.00707309946949,1.,-0.512953306961793));
#48698=CARTESIAN_POINT('Ctrl Pts',(2.01187773939242,-1.,-0.516902681728687));
#48699=CARTESIAN_POINT('Ctrl Pts',(2.01187773939242,1.,-0.516902681728687));
#48700=CARTESIAN_POINT('Ctrl Pts',(2.01666477917286,-1.,-0.520893590399371));
#48701=CARTESIAN_POINT('Ctrl Pts',(2.01666477917286,1.,-0.520893590399371));
#48702=CARTESIAN_POINT('Ctrl Pts',(2.02143356304698,-1.,-0.524925318333476));
#48703=CARTESIAN_POINT('Ctrl Pts',(2.02143356304698,1.,-0.524925318333476));
#48704=CARTESIAN_POINT('Ctrl Pts',(2.0261832908329,-1.,-0.528997127241914));
#48705=CARTESIAN_POINT('Ctrl Pts',(2.0261832908329,1.,-0.528997127241914));
#48706=CARTESIAN_POINT('Ctrl Pts',(2.03091336214426,-1.,-0.533108355132977));
#48707=CARTESIAN_POINT('Ctrl Pts',(2.03091336214426,1.,-0.533108355132977));
#48708=CARTESIAN_POINT('Ctrl Pts',(2.03562362954037,-1.,-0.537258489833262));
#48709=CARTESIAN_POINT('Ctrl Pts',(2.03562362954037,1.,-0.537258489833262));
#48710=CARTESIAN_POINT('Ctrl Pts',(2.04031422690527,-1.,-0.541447120615659));
#48711=CARTESIAN_POINT('Ctrl Pts',(2.04031422690527,1.,-0.541447120615659));
#48712=CARTESIAN_POINT('Ctrl Pts',(2.04498544714588,-1.,-0.54567390381743));
#48713=CARTESIAN_POINT('Ctrl Pts',(2.04498544714588,1.,-0.54567390381743));
#48714=CARTESIAN_POINT('Ctrl Pts',(2.04963761077958,-1.,-0.549938525150295));
#48715=CARTESIAN_POINT('Ctrl Pts',(2.04963761077958,1.,-0.549938525150295));
#48716=CARTESIAN_POINT('Ctrl Pts',(2.05427091604413,-1.,-0.554240657463906));
#48717=CARTESIAN_POINT('Ctrl Pts',(2.05427091604413,1.,-0.554240657463906));
#48718=CARTESIAN_POINT('Ctrl Pts',(2.05888537756462,-1.,-0.558579940185152));
#48719=CARTESIAN_POINT('Ctrl Pts',(2.05888537756462,1.,-0.558579940185152));
#48720=CARTESIAN_POINT('Ctrl Pts',(2.06348090160589,-1.,-0.562955993082262));
#48721=CARTESIAN_POINT('Ctrl Pts',(2.06348090160589,1.,-0.562955993082262));
#48722=CARTESIAN_POINT('Ctrl Pts',(2.06805732997334,-1.,-0.567368421181087));
#48723=CARTESIAN_POINT('Ctrl Pts',(2.06805732997334,1.,-0.567368421181087));
#48724=CARTESIAN_POINT('Ctrl Pts',(2.07261449292824,-1.,-0.571816823242603));
#48725=CARTESIAN_POINT('Ctrl Pts',(2.07261449292824,1.,-0.571816823242603));
#48726=CARTESIAN_POINT('Ctrl Pts',(2.07715226767559,-1.,-0.576300797416845));
#48727=CARTESIAN_POINT('Ctrl Pts',(2.07715226767559,1.,-0.576300797416845));
#48728=CARTESIAN_POINT('Ctrl Pts',(2.08167059018418,-1.,-0.580819952108064));
#48729=CARTESIAN_POINT('Ctrl Pts',(2.08167059018418,1.,-0.580819952108064));
#48730=CARTESIAN_POINT('Ctrl Pts',(2.08616943727951,-1.,-0.585373918991617));
#48731=CARTESIAN_POINT('Ctrl Pts',(2.08616943727951,1.,-0.585373918991617));
#48732=CARTESIAN_POINT('Ctrl Pts',(2.09064881812129,-1.,-0.589962365403406));
#48733=CARTESIAN_POINT('Ctrl Pts',(2.09064881812129,1.,-0.589962365403406));
#48734=CARTESIAN_POINT('Ctrl Pts',(2.0951087622027,-1.,-0.594585006052162));
#48735=CARTESIAN_POINT('Ctrl Pts',(2.0951087622027,1.,-0.594585006052162));
#48736=CARTESIAN_POINT('Ctrl Pts',(2.0995493086477,-1.,-0.599241616420534));
#48737=CARTESIAN_POINT('Ctrl Pts',(2.0995493086477,1.,-0.599241616420534));
#48738=CARTESIAN_POINT('Ctrl Pts',(2.10397049886949,-1.,-0.60393203073603));
#48739=CARTESIAN_POINT('Ctrl Pts',(2.10397049886949,1.,-0.60393203073603));
#48740=CARTESIAN_POINT('Ctrl Pts',(2.1074919961518,-1.,-0.607711315454876));
#48741=CARTESIAN_POINT('Ctrl Pts',(2.1074919961518,1.,-0.607711315454876));
#48742=CARTESIAN_POINT('Ctrl Pts',(2.11012443807238,-1.,-0.610560911689899));
#48743=CARTESIAN_POINT('Ctrl Pts',(2.11012443807238,1.,-0.610560911689899));
#48744=CARTESIAN_POINT('Ctrl Pts',(2.11187554259986,-1.,-0.6124673655618));
#48745=CARTESIAN_POINT('Ctrl Pts',(2.11187554259986,1.,-0.6124673655618));
#48746=CARTESIAN_POINT('Ctrl Pts',(2.11275013067528,-1.,-0.61342227326009));
#48747=CARTESIAN_POINT('Ctrl Pts',(2.11275013067528,1.,-0.61342227326009));
#48748=CARTESIAN_POINT('',(1.7075470150345,1.,-0.383122945602004));
#48749=CARTESIAN_POINT('Ctrl Pts',(1.7075470150345,1.,-0.383122945602004));
#48750=CARTESIAN_POINT('Ctrl Pts',(1.71231062891958,1.,-0.384119047315542));
#48751=CARTESIAN_POINT('Ctrl Pts',(1.72162022246158,1.,-0.38607079032701));
#48752=CARTESIAN_POINT('Ctrl Pts',(1.7349317097561,1.,-0.388877023509192));
#48753=CARTESIAN_POINT('Ctrl Pts',(1.75137405313962,1.,-0.392375812294307));
#48754=CARTESIAN_POINT('Ctrl Pts',(1.7697556004756,1.,-0.39634619612042));
#48755=CARTESIAN_POINT('Ctrl Pts',(1.78598826347533,1.,-0.399919403783081));
#48756=CARTESIAN_POINT('Ctrl Pts',(1.80012077176221,1.,-0.403107976170441));
#48757=CARTESIAN_POINT('Ctrl Pts',(1.81223801813988,1.,-0.405933518411838));
#48758=CARTESIAN_POINT('Ctrl Pts',(1.8224702267854,1.,-0.408428948108534));
#48759=CARTESIAN_POINT('Ctrl Pts',(1.83100408895216,1.,-0.410641256301675));
#48760=CARTESIAN_POINT('Ctrl Pts',(1.83808953475839,1.,-0.412633125322162));
#48761=CARTESIAN_POINT('Ctrl Pts',(1.8440575707371,1.,-0.41448743825434));
#48762=CARTESIAN_POINT('Ctrl Pts',(1.84929312929882,1.,-0.416300022038864));
#48763=CARTESIAN_POINT('Ctrl Pts',(1.85417632856234,1.,-0.418164129143534));
#48764=CARTESIAN_POINT('Ctrl Pts',(1.85903281096686,1.,-0.42015728797562));
#48765=CARTESIAN_POINT('Ctrl Pts',(1.86408083334028,1.,-0.422327307418275));
#48766=CARTESIAN_POINT('Ctrl Pts',(1.86937803944323,1.,-0.424678177291359));
#48767=CARTESIAN_POINT('Ctrl Pts',(1.87486989291484,1.,-0.427183828519102));
#48768=CARTESIAN_POINT('Ctrl Pts',(1.88044229001832,1.,-0.429803062482345));
#48769=CARTESIAN_POINT('Ctrl Pts',(1.88596913666793,1.,-0.432493038548748));
#48770=CARTESIAN_POINT('Ctrl Pts',(1.89136993975504,1.,-0.435225660963383));
#48771=CARTESIAN_POINT('Ctrl Pts',(1.89663648956466,1.,-0.437995003948244));
#48772=CARTESIAN_POINT('Ctrl Pts',(1.90180124389086,1.,-0.440807833704038));
#48773=CARTESIAN_POINT('Ctrl Pts',(1.90691756144898,1.,-0.443677556849151));
#48774=CARTESIAN_POINT('Ctrl Pts',(1.9120369998112,1.,-0.446617343485711));
#48775=CARTESIAN_POINT('Ctrl Pts',(1.91718342555755,1.,-0.449632260106662));
#48776=CARTESIAN_POINT('Ctrl Pts',(1.92235380648502,1.,-0.452719478359433));
#48777=CARTESIAN_POINT('Ctrl Pts',(1.92753067150476,1.,-0.455872005174371));
#48778=CARTESIAN_POINT('Ctrl Pts',(1.93269066517934,1.,-0.459081234547926));
#48779=CARTESIAN_POINT('Ctrl Pts',(1.93781486640821,1.,-0.462340031009057));
#48780=CARTESIAN_POINT('Ctrl Pts',(1.9428979419619,1.,-0.46564546202603));
#48781=CARTESIAN_POINT('Ctrl Pts',(1.94794381136514,1.,-0.468997482913135));
#48782=CARTESIAN_POINT('Ctrl Pts',(1.95296148278133,1.,-0.472397672264072));
#48783=CARTESIAN_POINT('Ctrl Pts',(1.95796111148177,1.,-0.475848034683176));
#48784=CARTESIAN_POINT('Ctrl Pts',(1.96294933055943,1.,-0.479349583074855));
#48785=CARTESIAN_POINT('Ctrl Pts',(1.96792703422362,1.,-0.482901662120691));
#48786=CARTESIAN_POINT('Ctrl Pts',(1.97289186263272,1.,-0.486502692907659));
#48787=CARTESIAN_POINT('Ctrl Pts',(1.97783973019229,1.,-0.490150627860953));
#48788=CARTESIAN_POINT('Ctrl Pts',(1.98276658761821,1.,-0.493843476541495));
#48789=CARTESIAN_POINT('Ctrl Pts',(1.98767044752932,1.,-0.497579909545574));
#48790=CARTESIAN_POINT('Ctrl Pts',(1.99255149126155,1.,-0.501359287727146));
#48791=CARTESIAN_POINT('Ctrl Pts',(1.99741107463572,1.,-0.505181361323026));
#48792=CARTESIAN_POINT('Ctrl Pts',(2.00225107134734,1.,-0.509046069886157));
#48793=CARTESIAN_POINT('Ctrl Pts',(2.00707309946949,1.,-0.512953306961793));
#48794=CARTESIAN_POINT('Ctrl Pts',(2.01187773939242,1.,-0.516902681728687));
#48795=CARTESIAN_POINT('Ctrl Pts',(2.01666477917286,1.,-0.520893590399371));
#48796=CARTESIAN_POINT('Ctrl Pts',(2.02143356304698,1.,-0.524925318333476));
#48797=CARTESIAN_POINT('Ctrl Pts',(2.0261832908329,1.,-0.528997127241914));
#48798=CARTESIAN_POINT('Ctrl Pts',(2.03091336214426,1.,-0.533108355132977));
#48799=CARTESIAN_POINT('Ctrl Pts',(2.03562362954037,1.,-0.537258489833262));
#48800=CARTESIAN_POINT('Ctrl Pts',(2.04031422690527,1.,-0.541447120615659));
#48801=CARTESIAN_POINT('Ctrl Pts',(2.04498544714588,1.,-0.54567390381743));
#48802=CARTESIAN_POINT('Ctrl Pts',(2.04963761077958,1.,-0.549938525150295));
#48803=CARTESIAN_POINT('Ctrl Pts',(2.05427091604413,1.,-0.554240657463906));
#48804=CARTESIAN_POINT('Ctrl Pts',(2.05888537756462,1.,-0.558579940185152));
#48805=CARTESIAN_POINT('Ctrl Pts',(2.06348090160589,1.,-0.562955993082262));
#48806=CARTESIAN_POINT('Ctrl Pts',(2.06805732997334,1.,-0.567368421181087));
#48807=CARTESIAN_POINT('Ctrl Pts',(2.07261449292824,1.,-0.571816823242603));
#48808=CARTESIAN_POINT('Ctrl Pts',(2.07715226767559,1.,-0.576300797416845));
#48809=CARTESIAN_POINT('Ctrl Pts',(2.08167059018418,1.,-0.580819952108064));
#48810=CARTESIAN_POINT('Ctrl Pts',(2.08616943727951,1.,-0.585373918991617));
#48811=CARTESIAN_POINT('Ctrl Pts',(2.09064881812129,1.,-0.589962365403406));
#48812=CARTESIAN_POINT('Ctrl Pts',(2.0951087622027,1.,-0.594585006052162));
#48813=CARTESIAN_POINT('Ctrl Pts',(2.0995493086477,1.,-0.599241616420534));
#48814=CARTESIAN_POINT('Ctrl Pts',(2.10397049886949,1.,-0.60393203073603));
#48815=CARTESIAN_POINT('Ctrl Pts',(2.1074919961518,1.,-0.607711315454876));
#48816=CARTESIAN_POINT('Ctrl Pts',(2.11012443807238,1.,-0.610560911689899));
#48817=CARTESIAN_POINT('Ctrl Pts',(2.11187554259986,1.,-0.6124673655618));
#48818=CARTESIAN_POINT('Ctrl Pts',(2.11275013067528,1.,-0.61342227326009));
#48819=CARTESIAN_POINT('',(1.7075470150345,0.,-0.383122945602001));
#48820=CARTESIAN_POINT('Origin',(0.,0.,0.));
#48821=CARTESIAN_POINT('',(1.74236521665491,1.,-0.163289472382896));
#48822=CARTESIAN_POINT('Origin',(0.,1.,0.));
#48823=CARTESIAN_POINT('',(1.74236521665491,0.,-0.163289472382896));
#48824=CARTESIAN_POINT('Ctrl Pts',(2.19890268624765,-1.,-0.0694764450219582));
#48825=CARTESIAN_POINT('Ctrl Pts',(2.19890268624765,1.,-0.0694764450219582));
#48826=CARTESIAN_POINT('Ctrl Pts',(2.19777582085423,-1.,-0.0701143536325491));
#48827=CARTESIAN_POINT('Ctrl Pts',(2.19777582085423,1.,-0.0701143536325491));
#48828=CARTESIAN_POINT('Ctrl Pts',(2.19552129484002,-1.,-0.0713863779526155));
#48829=CARTESIAN_POINT('Ctrl Pts',(2.19552129484002,1.,-0.0713863779526155));
#48830=CARTESIAN_POINT('Ctrl Pts',(2.19213712013662,-1.,-0.0732830357306726));
#48831=CARTESIAN_POINT('Ctrl Pts',(2.19213712013662,1.,-0.0732830357306726));
#48832=CARTESIAN_POINT('Ctrl Pts',(2.1876201139953,-1.,-0.0757891465836149));
#48833=CARTESIAN_POINT('Ctrl Pts',(2.1876201139953,1.,-0.0757891465836149));
#48834=CARTESIAN_POINT('Ctrl Pts',(2.18196589448887,-1.,-0.0788837727685244));
#48835=CARTESIAN_POINT('Ctrl Pts',(2.18196589448887,1.,-0.0788837727685244));
#48836=CARTESIAN_POINT('Ctrl Pts',(2.176303712113,-1.,-0.0819402680872767));
#48837=CARTESIAN_POINT('Ctrl Pts',(2.176303712113,1.,-0.0819402680872767));
#48838=CARTESIAN_POINT('Ctrl Pts',(2.17063357870952,-1.,-0.0849584620835374));
#48839=CARTESIAN_POINT('Ctrl Pts',(2.17063357870952,1.,-0.0849584620835374));
#48840=CARTESIAN_POINT('Ctrl Pts',(2.16495552645014,-1.,-0.0879381291386924));
#48841=CARTESIAN_POINT('Ctrl Pts',(2.16495552645014,1.,-0.0879381291386924));
#48842=CARTESIAN_POINT('Ctrl Pts',(2.15926961544516,-1.,-0.0908789888107267));
#48843=CARTESIAN_POINT('Ctrl Pts',(2.15926961544516,1.,-0.0908789888107267));
#48844=CARTESIAN_POINT('Ctrl Pts',(2.1535759397817,-1.,-0.0937807218867645));
#48845=CARTESIAN_POINT('Ctrl Pts',(2.1535759397817,1.,-0.0937807218867645));
#48846=CARTESIAN_POINT('Ctrl Pts',(2.14787463531795,-1.,-0.096642985230546));
#48847=CARTESIAN_POINT('Ctrl Pts',(2.14787463531795,1.,-0.096642985230546));
#48848=CARTESIAN_POINT('Ctrl Pts',(2.14216588396025,-1.,-0.0994654261990917));
#48849=CARTESIAN_POINT('Ctrl Pts',(2.14216588396025,1.,-0.0994654261990917));
#48850=CARTESIAN_POINT('Ctrl Pts',(2.13644992667165,-1.,-0.102247700556101));
#48851=CARTESIAN_POINT('Ctrl Pts',(2.13644992667165,1.,-0.102247700556101));
#48852=CARTESIAN_POINT('Ctrl Pts',(2.13072704887293,-1.,-0.10498947915274));
#48853=CARTESIAN_POINT('Ctrl Pts',(2.13072704887293,1.,-0.10498947915274));
#48854=CARTESIAN_POINT('Ctrl Pts',(2.12499752307,-1.,-0.10769043523109));
#48855=CARTESIAN_POINT('Ctrl Pts',(2.12499752307,1.,-0.10769043523109));
#48856=CARTESIAN_POINT('Ctrl Pts',(2.11926155590865,-1.,-0.110350236135025));
#48857=CARTESIAN_POINT('Ctrl Pts',(2.11926155590865,1.,-0.110350236135025));
#48858=CARTESIAN_POINT('Ctrl Pts',(2.11351924490306,-1.,-0.112968534419737));
#48859=CARTESIAN_POINT('Ctrl Pts',(2.11351924490306,1.,-0.112968534419737));
#48860=CARTESIAN_POINT('Ctrl Pts',(2.10777050261309,-1.,-0.115544957687927));
#48861=CARTESIAN_POINT('Ctrl Pts',(2.10777050261309,1.,-0.115544957687927));
#48862=CARTESIAN_POINT('Ctrl Pts',(2.102015121329,-1.,-0.118079107988356));
#48863=CARTESIAN_POINT('Ctrl Pts',(2.102015121329,1.,-0.118079107988356));
#48864=CARTESIAN_POINT('Ctrl Pts',(2.0962529286773,-1.,-0.120570567965122));
#48865=CARTESIAN_POINT('Ctrl Pts',(2.0962529286773,1.,-0.120570567965122));
#48866=CARTESIAN_POINT('Ctrl Pts',(2.09048392424825,-1.,-0.123018905621083));
#48867=CARTESIAN_POINT('Ctrl Pts',(2.09048392424825,1.,-0.123018905621083));
#48868=CARTESIAN_POINT('Ctrl Pts',(2.08470840653643,-1.,-0.125423679412062));
#48869=CARTESIAN_POINT('Ctrl Pts',(2.08470840653643,1.,-0.125423679412062));
#48870=CARTESIAN_POINT('Ctrl Pts',(2.07892715110987,-1.,-0.12778444527612));
#48871=CARTESIAN_POINT('Ctrl Pts',(2.07892715110987,1.,-0.12778444527612));
#48872=CARTESIAN_POINT('Ctrl Pts',(2.07314114713063,-1.,-0.130100748328404));
#48873=CARTESIAN_POINT('Ctrl Pts',(2.07314114713063,1.,-0.130100748328404));
#48874=CARTESIAN_POINT('Ctrl Pts',(2.06735123910326,-1.,-0.132372111547711));
#48875=CARTESIAN_POINT('Ctrl Pts',(2.06735123910326,1.,-0.132372111547711));
#48876=CARTESIAN_POINT('Ctrl Pts',(2.06155781517842,-1.,-0.134598026192106));
#48877=CARTESIAN_POINT('Ctrl Pts',(2.06155781517842,1.,-0.134598026192106));
#48878=CARTESIAN_POINT('Ctrl Pts',(2.05576044414264,-1.,-0.136777941218044));
#48879=CARTESIAN_POINT('Ctrl Pts',(2.05576044414264,1.,-0.136777941218044));
#48880=CARTESIAN_POINT('Ctrl Pts',(2.04995762001328,-1.,-0.138911255368966));
#48881=CARTESIAN_POINT('Ctrl Pts',(2.04995762001328,1.,-0.138911255368966));
#48882=CARTESIAN_POINT('Ctrl Pts',(2.04414757947916,-1.,-0.140997332152546));
#48883=CARTESIAN_POINT('Ctrl Pts',(2.04414757947916,1.,-0.140997332152546));
#48884=CARTESIAN_POINT('Ctrl Pts',(2.03832911025912,-1.,-0.143035515058209));
#48885=CARTESIAN_POINT('Ctrl Pts',(2.03832911025912,1.,-0.143035515058209));
#48886=CARTESIAN_POINT('Ctrl Pts',(2.03250223739942,-1.,-0.145025140186058));
#48887=CARTESIAN_POINT('Ctrl Pts',(2.03250223739942,1.,-0.145025140186058));
#48888=CARTESIAN_POINT('Ctrl Pts',(2.02666926182017,-1.,-0.146965557332583));
#48889=CARTESIAN_POINT('Ctrl Pts',(2.02666926182017,1.,-0.146965557332583));
#48890=CARTESIAN_POINT('Ctrl Pts',(2.02083464969894,-1.,-0.148856124775337));
#48891=CARTESIAN_POINT('Ctrl Pts',(2.02083464969894,1.,-0.148856124775337));
#48892=CARTESIAN_POINT('Ctrl Pts',(2.01500291940238,-1.,-0.150696157673078));
#48893=CARTESIAN_POINT('Ctrl Pts',(2.01500291940238,1.,-0.150696157673078));
#48894=CARTESIAN_POINT('Ctrl Pts',(2.00917680318424,-1.,-0.15248488362145));
#48895=CARTESIAN_POINT('Ctrl Pts',(2.00917680318424,1.,-0.15248488362145));
#48896=CARTESIAN_POINT('Ctrl Pts',(2.00335565310543,-1.,-0.154221403049722));
#48897=CARTESIAN_POINT('Ctrl Pts',(2.00335565310543,1.,-0.154221403049722));
#48898=CARTESIAN_POINT('Ctrl Pts',(1.99753284771497,-1.,-0.155904629548784));
#48899=CARTESIAN_POINT('Ctrl Pts',(1.99753284771497,1.,-0.155904629548784));
#48900=CARTESIAN_POINT('Ctrl Pts',(1.99169810931908,-1.,-0.157533331459227));
#48901=CARTESIAN_POINT('Ctrl Pts',(1.99169810931908,1.,-0.157533331459227));
#48902=CARTESIAN_POINT('Ctrl Pts',(1.98584238283292,-1.,-0.159106226437299));
#48903=CARTESIAN_POINT('Ctrl Pts',(1.98584238283292,1.,-0.159106226437299));
#48904=CARTESIAN_POINT('Ctrl Pts',(1.97996195437559,-1.,-0.160622060784611));
#48905=CARTESIAN_POINT('Ctrl Pts',(1.97996195437559,1.,-0.160622060784611));
#48906=CARTESIAN_POINT('Ctrl Pts',(1.97406280235188,-1.,-0.162079693556289));
#48907=CARTESIAN_POINT('Ctrl Pts',(1.97406280235188,1.,-0.162079693556289));
#48908=CARTESIAN_POINT('Ctrl Pts',(1.96816512677967,-1.,-0.163478185457734));
#48909=CARTESIAN_POINT('Ctrl Pts',(1.96816512677967,1.,-0.163478185457734));
#48910=CARTESIAN_POINT('Ctrl Pts',(1.96229379940136,-1.,-0.164816568920269));
#48911=CARTESIAN_POINT('Ctrl Pts',(1.96229379940136,1.,-0.164816568920269));
#48912=CARTESIAN_POINT('Ctrl Pts',(1.9564675971873,-1.,-0.166093592002813));
#48913=CARTESIAN_POINT('Ctrl Pts',(1.9564675971873,1.,-0.166093592002813));
#48914=CARTESIAN_POINT('Ctrl Pts',(1.95069027794294,-1.,-0.167307501784476));
#48915=CARTESIAN_POINT('Ctrl Pts',(1.95069027794294,1.,-0.167307501784476));
#48916=CARTESIAN_POINT('Ctrl Pts',(1.94493757756931,-1.,-0.168455741607556));
#48917=CARTESIAN_POINT('Ctrl Pts',(1.94493757756931,1.,-0.168455741607556));
#48918=CARTESIAN_POINT('Ctrl Pts',(1.93915639211581,-1.,-0.169534904817491));
#48919=CARTESIAN_POINT('Ctrl Pts',(1.93915639211581,1.,-0.169534904817491));
#48920=CARTESIAN_POINT('Ctrl Pts',(1.93329183155539,-1.,-0.170541253116202));
#48921=CARTESIAN_POINT('Ctrl Pts',(1.93329183155539,1.,-0.170541253116202));
#48922=CARTESIAN_POINT('Ctrl Pts',(1.92731093582036,-1.,-0.171471191532988));
#48923=CARTESIAN_POINT('Ctrl Pts',(1.92731093582036,1.,-0.171471191532988));
#48924=CARTESIAN_POINT('Ctrl Pts',(1.9212233439798,-1.,-0.172321621259514));
#48925=CARTESIAN_POINT('Ctrl Pts',(1.9212233439798,1.,-0.172321621259514));
#48926=CARTESIAN_POINT('Ctrl Pts',(1.91511429159527,-1.,-0.173090695383496));
#48927=CARTESIAN_POINT('Ctrl Pts',(1.91511429159527,1.,-0.173090695383496));
#48928=CARTESIAN_POINT('Ctrl Pts',(1.90911693975267,-1.,-0.173776635257817));
#48929=CARTESIAN_POINT('Ctrl Pts',(1.90911693975267,1.,-0.173776635257817));
#48930=CARTESIAN_POINT('Ctrl Pts',(1.90335253862834,-1.,-0.174375518661085));
#48931=CARTESIAN_POINT('Ctrl Pts',(1.90335253862834,1.,-0.174375518661085));
#48932=CARTESIAN_POINT('Ctrl Pts',(1.89788101117132,-1.,-0.174879405091263));
#48933=CARTESIAN_POINT('Ctrl Pts',(1.89788101117132,1.,-0.174879405091263));
#48934=CARTESIAN_POINT('Ctrl Pts',(1.892646301985,-1.,-0.175274276190844));
#48935=CARTESIAN_POINT('Ctrl Pts',(1.892646301985,1.,-0.175274276190844));
#48936=CARTESIAN_POINT('Ctrl Pts',(1.88742606273259,-1.,-0.175538155840648));
#48937=CARTESIAN_POINT('Ctrl Pts',(1.88742606273259,1.,-0.175538155840648));
#48938=CARTESIAN_POINT('Ctrl Pts',(1.88188663145367,-1.,-0.175644148889699));
#48939=CARTESIAN_POINT('Ctrl Pts',(1.88188663145367,1.,-0.175644148889699));
#48940=CARTESIAN_POINT('Ctrl Pts',(1.87563767773588,-1.,-0.175563480746485));
#48941=CARTESIAN_POINT('Ctrl Pts',(1.87563767773588,1.,-0.175563480746485));
#48942=CARTESIAN_POINT('Ctrl Pts',(1.86828349694799,-1.,-0.175268337590758));
#48943=CARTESIAN_POINT('Ctrl Pts',(1.86828349694799,1.,-0.175268337590758));
#48944=CARTESIAN_POINT('Ctrl Pts',(1.85948367088837,-1.,-0.17473525927603));
#48945=CARTESIAN_POINT('Ctrl Pts',(1.85948367088837,1.,-0.17473525927603));
#48946=CARTESIAN_POINT('Ctrl Pts',(1.8489811319852,-1.,-0.173946627587732));
#48947=CARTESIAN_POINT('Ctrl Pts',(1.8489811319852,1.,-0.173946627587732));
#48948=CARTESIAN_POINT('Ctrl Pts',(1.83658380527692,-1.,-0.1728894428919));
#48949=CARTESIAN_POINT('Ctrl Pts',(1.83658380527692,1.,-0.1728894428919));
#48950=CARTESIAN_POINT('Ctrl Pts',(1.82215766811545,-1.,-0.171554770204119));
#48951=CARTESIAN_POINT('Ctrl Pts',(1.82215766811545,1.,-0.171554770204119));
#48952=CARTESIAN_POINT('Ctrl Pts',(1.80561530629706,-1.,-0.169936923904608));
#48953=CARTESIAN_POINT('Ctrl Pts',(1.80561530629706,1.,-0.169936923904608));
#48954=CARTESIAN_POINT('Ctrl Pts',(1.7869064998507,-1.,-0.168032772805197));
#48955=CARTESIAN_POINT('Ctrl Pts',(1.7869064998507,1.,-0.168032772805197));
#48956=CARTESIAN_POINT('Ctrl Pts',(1.77018771684844,-1.,-0.1662793551464));
#48957=CARTESIAN_POINT('Ctrl Pts',(1.77018771684844,1.,-0.1662793551464));
#48958=CARTESIAN_POINT('Ctrl Pts',(1.75666056638427,-1.,-0.164834765707159));
#48959=CARTESIAN_POINT('Ctrl Pts',(1.75666056638427,1.,-0.164834765707159));
#48960=CARTESIAN_POINT('Ctrl Pts',(1.7472034950333,-1.,-0.163814161002002));
#48961=CARTESIAN_POINT('Ctrl Pts',(1.7472034950333,1.,-0.163814161002002));
#48962=CARTESIAN_POINT('Ctrl Pts',(1.74236521665491,-1.,-0.163289472382896));
#48963=CARTESIAN_POINT('Ctrl Pts',(1.74236521665491,1.,-0.163289472382896));
#48964=CARTESIAN_POINT('',(2.19890268624765,1.,-0.0694764450219582));
#48965=CARTESIAN_POINT('Ctrl Pts',(2.19890268624765,1.,-0.0694764450219582));
#48966=CARTESIAN_POINT('Ctrl Pts',(2.19777582085423,1.,-0.0701143536325491));
#48967=CARTESIAN_POINT('Ctrl Pts',(2.19552129484002,1.,-0.0713863779526155));
#48968=CARTESIAN_POINT('Ctrl Pts',(2.19213712013662,1.,-0.0732830357306726));
#48969=CARTESIAN_POINT('Ctrl Pts',(2.1876201139953,1.,-0.0757891465836149));
#48970=CARTESIAN_POINT('Ctrl Pts',(2.18196589448887,1.,-0.0788837727685244));
#48971=CARTESIAN_POINT('Ctrl Pts',(2.176303712113,1.,-0.0819402680872767));
#48972=CARTESIAN_POINT('Ctrl Pts',(2.17063357870952,1.,-0.0849584620835374));
#48973=CARTESIAN_POINT('Ctrl Pts',(2.16495552645014,1.,-0.0879381291386924));
#48974=CARTESIAN_POINT('Ctrl Pts',(2.15926961544516,1.,-0.0908789888107267));
#48975=CARTESIAN_POINT('Ctrl Pts',(2.1535759397817,1.,-0.0937807218867645));
#48976=CARTESIAN_POINT('Ctrl Pts',(2.14787463531795,1.,-0.096642985230546));
#48977=CARTESIAN_POINT('Ctrl Pts',(2.14216588396025,1.,-0.0994654261990917));
#48978=CARTESIAN_POINT('Ctrl Pts',(2.13644992667165,1.,-0.102247700556101));
#48979=CARTESIAN_POINT('Ctrl Pts',(2.13072704887293,1.,-0.10498947915274));
#48980=CARTESIAN_POINT('Ctrl Pts',(2.12499752307,1.,-0.10769043523109));
#48981=CARTESIAN_POINT('Ctrl Pts',(2.11926155590865,1.,-0.110350236135025));
#48982=CARTESIAN_POINT('Ctrl Pts',(2.11351924490306,1.,-0.112968534419737));
#48983=CARTESIAN_POINT('Ctrl Pts',(2.10777050261309,1.,-0.115544957687927));
#48984=CARTESIAN_POINT('Ctrl Pts',(2.102015121329,1.,-0.118079107988356));
#48985=CARTESIAN_POINT('Ctrl Pts',(2.0962529286773,1.,-0.120570567965122));
#48986=CARTESIAN_POINT('Ctrl Pts',(2.09048392424825,1.,-0.123018905621083));
#48987=CARTESIAN_POINT('Ctrl Pts',(2.08470840653643,1.,-0.125423679412062));
#48988=CARTESIAN_POINT('Ctrl Pts',(2.07892715110987,1.,-0.12778444527612));
#48989=CARTESIAN_POINT('Ctrl Pts',(2.07314114713063,1.,-0.130100748328404));
#48990=CARTESIAN_POINT('Ctrl Pts',(2.06735123910326,1.,-0.132372111547711));
#48991=CARTESIAN_POINT('Ctrl Pts',(2.06155781517842,1.,-0.134598026192106));
#48992=CARTESIAN_POINT('Ctrl Pts',(2.05576044414264,1.,-0.136777941218044));
#48993=CARTESIAN_POINT('Ctrl Pts',(2.04995762001328,1.,-0.138911255368966));
#48994=CARTESIAN_POINT('Ctrl Pts',(2.04414757947916,1.,-0.140997332152546));
#48995=CARTESIAN_POINT('Ctrl Pts',(2.03832911025912,1.,-0.143035515058209));
#48996=CARTESIAN_POINT('Ctrl Pts',(2.03250223739942,1.,-0.145025140186058));
#48997=CARTESIAN_POINT('Ctrl Pts',(2.02666926182017,1.,-0.146965557332583));
#48998=CARTESIAN_POINT('Ctrl Pts',(2.02083464969894,1.,-0.148856124775337));
#48999=CARTESIAN_POINT('Ctrl Pts',(2.01500291940238,1.,-0.150696157673078));
#49000=CARTESIAN_POINT('Ctrl Pts',(2.00917680318424,1.,-0.15248488362145));
#49001=CARTESIAN_POINT('Ctrl Pts',(2.00335565310543,1.,-0.154221403049722));
#49002=CARTESIAN_POINT('Ctrl Pts',(1.99753284771497,1.,-0.155904629548784));
#49003=CARTESIAN_POINT('Ctrl Pts',(1.99169810931908,1.,-0.157533331459227));
#49004=CARTESIAN_POINT('Ctrl Pts',(1.98584238283292,1.,-0.159106226437299));
#49005=CARTESIAN_POINT('Ctrl Pts',(1.97996195437559,1.,-0.160622060784611));
#49006=CARTESIAN_POINT('Ctrl Pts',(1.97406280235188,1.,-0.162079693556289));
#49007=CARTESIAN_POINT('Ctrl Pts',(1.96816512677967,1.,-0.163478185457734));
#49008=CARTESIAN_POINT('Ctrl Pts',(1.96229379940136,1.,-0.164816568920269));
#49009=CARTESIAN_POINT('Ctrl Pts',(1.9564675971873,1.,-0.166093592002813));
#49010=CARTESIAN_POINT('Ctrl Pts',(1.95069027794294,1.,-0.167307501784476));
#49011=CARTESIAN_POINT('Ctrl Pts',(1.94493757756931,1.,-0.168455741607556));
#49012=CARTESIAN_POINT('Ctrl Pts',(1.93915639211581,1.,-0.169534904817491));
#49013=CARTESIAN_POINT('Ctrl Pts',(1.93329183155539,1.,-0.170541253116202));
#49014=CARTESIAN_POINT('Ctrl Pts',(1.92731093582036,1.,-0.171471191532988));
#49015=CARTESIAN_POINT('Ctrl Pts',(1.9212233439798,1.,-0.172321621259514));
#49016=CARTESIAN_POINT('Ctrl Pts',(1.91511429159527,1.,-0.173090695383496));
#49017=CARTESIAN_POINT('Ctrl Pts',(1.90911693975267,1.,-0.173776635257817));
#49018=CARTESIAN_POINT('Ctrl Pts',(1.90335253862834,1.,-0.174375518661085));
#49019=CARTESIAN_POINT('Ctrl Pts',(1.89788101117132,1.,-0.174879405091263));
#49020=CARTESIAN_POINT('Ctrl Pts',(1.892646301985,1.,-0.175274276190844));
#49021=CARTESIAN_POINT('Ctrl Pts',(1.88742606273259,1.,-0.175538155840648));
#49022=CARTESIAN_POINT('Ctrl Pts',(1.88188663145367,1.,-0.175644148889699));
#49023=CARTESIAN_POINT('Ctrl Pts',(1.87563767773588,1.,-0.175563480746485));
#49024=CARTESIAN_POINT('Ctrl Pts',(1.86828349694799,1.,-0.175268337590758));
#49025=CARTESIAN_POINT('Ctrl Pts',(1.85948367088837,1.,-0.17473525927603));
#49026=CARTESIAN_POINT('Ctrl Pts',(1.8489811319852,1.,-0.173946627587732));
#49027=CARTESIAN_POINT('Ctrl Pts',(1.83658380527692,1.,-0.1728894428919));
#49028=CARTESIAN_POINT('Ctrl Pts',(1.82215766811545,1.,-0.171554770204119));
#49029=CARTESIAN_POINT('Ctrl Pts',(1.80561530629706,1.,-0.169936923904608));
#49030=CARTESIAN_POINT('Ctrl Pts',(1.7869064998507,1.,-0.168032772805197));
#49031=CARTESIAN_POINT('Ctrl Pts',(1.77018771684844,1.,-0.1662793551464));
#49032=CARTESIAN_POINT('Ctrl Pts',(1.75666056638427,1.,-0.164834765707159));
#49033=CARTESIAN_POINT('Ctrl Pts',(1.7472034950333,1.,-0.163814161002002));
#49034=CARTESIAN_POINT('Ctrl Pts',(1.74236521665491,1.,-0.163289472382896));
#49035=CARTESIAN_POINT('',(2.19890268624765,0.,-0.0694764450219582));
#49036=CARTESIAN_POINT('Origin',(2.19890268624765,0.,0.0694764450219582));
#49037=CARTESIAN_POINT('',(2.19890268624765,1.,0.0694764450219582));
#49038=CARTESIAN_POINT('',(2.19890268624765,1.,-0.0694764450219582));
#49039=CARTESIAN_POINT('',(2.19890268624765,0.,0.0694764450219582));
#49040=CARTESIAN_POINT('Ctrl Pts',(1.74236521665491,-1.,0.163289472382896));
#49041=CARTESIAN_POINT('Ctrl Pts',(1.74236521665491,1.,0.163289472382896));
#49042=CARTESIAN_POINT('Ctrl Pts',(1.74720349503904,-1.,0.163814161002474));
#49043=CARTESIAN_POINT('Ctrl Pts',(1.74720349503904,1.,0.163814161002474));
#49044=CARTESIAN_POINT('Ctrl Pts',(1.75666056640041,-1.,0.164834765708484));
#49045=CARTESIAN_POINT('Ctrl Pts',(1.75666056640041,1.,0.164834765708484));
#49046=CARTESIAN_POINT('Ctrl Pts',(1.77018771687692,-1.,0.166279355148738));
#49047=CARTESIAN_POINT('Ctrl Pts',(1.77018771687692,1.,0.166279355148738));
#49048=CARTESIAN_POINT('Ctrl Pts',(1.78690649988931,-1.,0.16803277280837));
#49049=CARTESIAN_POINT('Ctrl Pts',(1.78690649988931,1.,0.16803277280837));
#49050=CARTESIAN_POINT('Ctrl Pts',(1.80561530633924,-1.,0.169936923908078));
#49051=CARTESIAN_POINT('Ctrl Pts',(1.80561530633924,1.,0.169936923908078));
#49052=CARTESIAN_POINT('Ctrl Pts',(1.82215766815414,-1.,0.171554770207306));
#49053=CARTESIAN_POINT('Ctrl Pts',(1.82215766815414,1.,0.171554770207306));
#49054=CARTESIAN_POINT('Ctrl Pts',(1.83658380530747,-1.,0.17288944289442));
#49055=CARTESIAN_POINT('Ctrl Pts',(1.83658380530747,1.,0.17288944289442));
#49056=CARTESIAN_POINT('Ctrl Pts',(1.84898113200543,-1.,0.173946627589401));
#49057=CARTESIAN_POINT('Ctrl Pts',(1.84898113200543,1.,0.173946627589401));
#49058=CARTESIAN_POINT('Ctrl Pts',(1.85948367089838,-1.,0.174735259276856));
#49059=CARTESIAN_POINT('Ctrl Pts',(1.85948367089838,1.,0.174735259276856));
#49060=CARTESIAN_POINT('Ctrl Pts',(1.86828349694972,-1.,0.1752683375909));
#49061=CARTESIAN_POINT('Ctrl Pts',(1.86828349694972,1.,0.1752683375909));
#49062=CARTESIAN_POINT('Ctrl Pts',(1.87563767773249,-1.,0.175563480746205));
#49063=CARTESIAN_POINT('Ctrl Pts',(1.87563767773249,1.,0.175563480746205));
#49064=CARTESIAN_POINT('Ctrl Pts',(1.88188663144846,-1.,0.175644148889271));
#49065=CARTESIAN_POINT('Ctrl Pts',(1.88188663144846,1.,0.175644148889271));
#49066=CARTESIAN_POINT('Ctrl Pts',(1.88742606272818,-1.,0.175538155840286));
#49067=CARTESIAN_POINT('Ctrl Pts',(1.88742606272818,1.,0.175538155840286));
#49068=CARTESIAN_POINT('Ctrl Pts',(1.89264630198279,-1.,0.175274276190664));
#49069=CARTESIAN_POINT('Ctrl Pts',(1.89264630198279,1.,0.175274276190664));
#49070=CARTESIAN_POINT('Ctrl Pts',(1.89788101117148,-1.,0.174879405091277));
#49071=CARTESIAN_POINT('Ctrl Pts',(1.89788101117148,1.,0.174879405091277));
#49072=CARTESIAN_POINT('Ctrl Pts',(1.90335253863003,-1.,0.174375518661222));
#49073=CARTESIAN_POINT('Ctrl Pts',(1.90335253863003,1.,0.174375518661222));
#49074=CARTESIAN_POINT('Ctrl Pts',(1.90911693975475,-1.,0.173776635257983));
#49075=CARTESIAN_POINT('Ctrl Pts',(1.90911693975475,1.,0.173776635257983));
#49076=CARTESIAN_POINT('Ctrl Pts',(1.91511429159681,-1.,0.173090695383619));
#49077=CARTESIAN_POINT('Ctrl Pts',(1.91511429159681,1.,0.173090695383619));
#49078=CARTESIAN_POINT('Ctrl Pts',(1.92122334398034,-1.,0.172321621259556));
#49079=CARTESIAN_POINT('Ctrl Pts',(1.92122334398034,1.,0.172321621259556));
#49080=CARTESIAN_POINT('Ctrl Pts',(1.92731093582,-1.,0.17147119153296));
#49081=CARTESIAN_POINT('Ctrl Pts',(1.92731093582,1.,0.17147119153296));
#49082=CARTESIAN_POINT('Ctrl Pts',(1.93329183155455,-1.,0.170541253116136));
#49083=CARTESIAN_POINT('Ctrl Pts',(1.93329183155455,1.,0.170541253116136));
#49084=CARTESIAN_POINT('Ctrl Pts',(1.93915639211497,-1.,0.169534904817425));
#49085=CARTESIAN_POINT('Ctrl Pts',(1.93915639211497,1.,0.169534904817425));
#49086=CARTESIAN_POINT('Ctrl Pts',(1.94493757756879,-1.,0.168455741607515));
#49087=CARTESIAN_POINT('Ctrl Pts',(1.94493757756879,1.,0.168455741607515));
#49088=CARTESIAN_POINT('Ctrl Pts',(1.95069027794286,-1.,0.167307501784469));
#49089=CARTESIAN_POINT('Ctrl Pts',(1.95069027794286,1.,0.167307501784469));
#49090=CARTESIAN_POINT('Ctrl Pts',(1.95646759718755,-1.,0.166093592002832));
#49091=CARTESIAN_POINT('Ctrl Pts',(1.95646759718755,1.,0.166093592002832));
#49092=CARTESIAN_POINT('Ctrl Pts',(1.96229379940174,-1.,0.1648165689203));
#49093=CARTESIAN_POINT('Ctrl Pts',(1.96229379940174,1.,0.1648165689203));
#49094=CARTESIAN_POINT('Ctrl Pts',(1.96816512678,-1.,0.16347818545776));
#49095=CARTESIAN_POINT('Ctrl Pts',(1.96816512678,1.,0.16347818545776));
#49096=CARTESIAN_POINT('Ctrl Pts',(1.97406280235204,-1.,0.162079693556302));
#49097=CARTESIAN_POINT('Ctrl Pts',(1.97406280235204,1.,0.162079693556302));
#49098=CARTESIAN_POINT('Ctrl Pts',(1.97996195437557,-1.,0.16062206078461));
#49099=CARTESIAN_POINT('Ctrl Pts',(1.97996195437557,1.,0.16062206078461));
#49100=CARTESIAN_POINT('Ctrl Pts',(1.98584238283279,-1.,0.159106226437288));
#49101=CARTESIAN_POINT('Ctrl Pts',(1.98584238283279,1.,0.159106226437288));
#49102=CARTESIAN_POINT('Ctrl Pts',(1.99169810931893,-1.,0.157533331459215));
#49103=CARTESIAN_POINT('Ctrl Pts',(1.99169810931893,1.,0.157533331459215));
#49104=CARTESIAN_POINT('Ctrl Pts',(1.99753284771487,-1.,0.155904629548774));
#49105=CARTESIAN_POINT('Ctrl Pts',(1.99753284771487,1.,0.155904629548774));
#49106=CARTESIAN_POINT('Ctrl Pts',(2.00335565310539,-1.,0.154221403049719));
#49107=CARTESIAN_POINT('Ctrl Pts',(2.00335565310539,1.,0.154221403049719));
#49108=CARTESIAN_POINT('Ctrl Pts',(2.00917680318426,-1.,0.152484883621452));
#49109=CARTESIAN_POINT('Ctrl Pts',(2.00917680318426,1.,0.152484883621452));
#49110=CARTESIAN_POINT('Ctrl Pts',(2.01500291940243,-1.,0.150696157673084));
#49111=CARTESIAN_POINT('Ctrl Pts',(2.01500291940243,1.,0.150696157673084));
#49112=CARTESIAN_POINT('Ctrl Pts',(2.02083464969897,-1.,0.148856124775342));
#49113=CARTESIAN_POINT('Ctrl Pts',(2.02083464969897,1.,0.148856124775342));
#49114=CARTESIAN_POINT('Ctrl Pts',(2.02666926182017,-1.,0.146965557332586));
#49115=CARTESIAN_POINT('Ctrl Pts',(2.02666926182017,1.,0.146965557332586));
#49116=CARTESIAN_POINT('Ctrl Pts',(2.03250223739941,-1.,0.145025140186058));
#49117=CARTESIAN_POINT('Ctrl Pts',(2.03250223739941,1.,0.145025140186058));
#49118=CARTESIAN_POINT('Ctrl Pts',(2.03832911025913,-1.,0.143035515058208));
#49119=CARTESIAN_POINT('Ctrl Pts',(2.03832911025913,1.,0.143035515058208));
#49120=CARTESIAN_POINT('Ctrl Pts',(2.04414757947919,-1.,0.140997332152545));
#49121=CARTESIAN_POINT('Ctrl Pts',(2.04414757947919,1.,0.140997332152545));
#49122=CARTESIAN_POINT('Ctrl Pts',(2.04995762001333,-1.,0.138911255368966));
#49123=CARTESIAN_POINT('Ctrl Pts',(2.04995762001333,1.,0.138911255368966));
#49124=CARTESIAN_POINT('Ctrl Pts',(2.0557604441427,-1.,0.136777941218044));
#49125=CARTESIAN_POINT('Ctrl Pts',(2.0557604441427,1.,0.136777941218044));
#49126=CARTESIAN_POINT('Ctrl Pts',(2.06155781517844,-1.,0.134598026192107));
#49127=CARTESIAN_POINT('Ctrl Pts',(2.06155781517844,1.,0.134598026192107));
#49128=CARTESIAN_POINT('Ctrl Pts',(2.06735123910319,-1.,0.132372111547709));
#49129=CARTESIAN_POINT('Ctrl Pts',(2.06735123910319,1.,0.132372111547709));
#49130=CARTESIAN_POINT('Ctrl Pts',(2.07314114713047,-1.,0.1301007483284));
#49131=CARTESIAN_POINT('Ctrl Pts',(2.07314114713047,1.,0.1301007483284));
#49132=CARTESIAN_POINT('Ctrl Pts',(2.07892715110967,-1.,0.127784445276116));
#49133=CARTESIAN_POINT('Ctrl Pts',(2.07892715110967,1.,0.127784445276116));
#49134=CARTESIAN_POINT('Ctrl Pts',(2.08470840653628,-1.,0.125423679412058));
#49135=CARTESIAN_POINT('Ctrl Pts',(2.08470840653628,1.,0.125423679412058));
#49136=CARTESIAN_POINT('Ctrl Pts',(2.09048392424826,-1.,0.123018905621083));
#49137=CARTESIAN_POINT('Ctrl Pts',(2.09048392424826,1.,0.123018905621083));
#49138=CARTESIAN_POINT('Ctrl Pts',(2.09625292867756,-1.,0.120570567965129));
#49139=CARTESIAN_POINT('Ctrl Pts',(2.09625292867756,1.,0.120570567965129));
#49140=CARTESIAN_POINT('Ctrl Pts',(2.10201512132945,-1.,0.118079107988368));
#49141=CARTESIAN_POINT('Ctrl Pts',(2.10201512132945,1.,0.118079107988368));
#49142=CARTESIAN_POINT('Ctrl Pts',(2.10777050261359,-1.,0.11554495768794));
#49143=CARTESIAN_POINT('Ctrl Pts',(2.10777050261359,1.,0.11554495768794));
#49144=CARTESIAN_POINT('Ctrl Pts',(2.11351924490335,-1.,0.112968534419746));
#49145=CARTESIAN_POINT('Ctrl Pts',(2.11351924490335,1.,0.112968534419746));
#49146=CARTESIAN_POINT('Ctrl Pts',(2.11926155590849,-1.,0.11035023613502));
#49147=CARTESIAN_POINT('Ctrl Pts',(2.11926155590849,1.,0.11035023613502));
#49148=CARTESIAN_POINT('Ctrl Pts',(2.12499752306927,-1.,0.107690435231068));
#49149=CARTESIAN_POINT('Ctrl Pts',(2.12499752306927,1.,0.107690435231068));
#49150=CARTESIAN_POINT('Ctrl Pts',(2.1307270488718,-1.,0.104989479152703));
#49151=CARTESIAN_POINT('Ctrl Pts',(2.1307270488718,1.,0.104989479152703));
#49152=CARTESIAN_POINT('Ctrl Pts',(2.13644992667052,-1.,0.102247700556063));
#49153=CARTESIAN_POINT('Ctrl Pts',(2.13644992667052,1.,0.102247700556063));
#49154=CARTESIAN_POINT('Ctrl Pts',(2.14216588395974,-1.,0.0994654261990741));
#49155=CARTESIAN_POINT('Ctrl Pts',(2.14216588395974,1.,0.0994654261990741));
#49156=CARTESIAN_POINT('Ctrl Pts',(2.14787463531864,-1.,0.0966429852305688));
#49157=CARTESIAN_POINT('Ctrl Pts',(2.14787463531864,1.,0.0966429852305688));
#49158=CARTESIAN_POINT('Ctrl Pts',(2.15357593978377,-1.,0.0937807218868344));
#49159=CARTESIAN_POINT('Ctrl Pts',(2.15357593978377,1.,0.0937807218868344));
#49160=CARTESIAN_POINT('Ctrl Pts',(2.15926961544808,-1.,0.0908789888108265));
#49161=CARTESIAN_POINT('Ctrl Pts',(2.15926961544808,1.,0.0908789888108265));
#49162=CARTESIAN_POINT('Ctrl Pts',(2.16495552645275,-1.,0.0879381291387821));
#49163=CARTESIAN_POINT('Ctrl Pts',(2.16495552645275,1.,0.0879381291387821));
#49164=CARTESIAN_POINT('Ctrl Pts',(2.17063357871031,-1.,0.0849584620835642));
#49165=CARTESIAN_POINT('Ctrl Pts',(2.17063357871031,1.,0.0849584620835642));
#49166=CARTESIAN_POINT('Ctrl Pts',(2.1763037121106,-1.,0.0819402680871938));
#49167=CARTESIAN_POINT('Ctrl Pts',(2.1763037121106,1.,0.0819402680871938));
#49168=CARTESIAN_POINT('Ctrl Pts',(2.18196589448304,-1.,0.0788837727683226));
#49169=CARTESIAN_POINT('Ctrl Pts',(2.18196589448304,1.,0.0788837727683226));
#49170=CARTESIAN_POINT('Ctrl Pts',(2.1876201139874,-1.,0.075789146583341));
#49171=CARTESIAN_POINT('Ctrl Pts',(2.1876201139874,1.,0.075789146583341));
#49172=CARTESIAN_POINT('Ctrl Pts',(2.19213712012956,-1.,0.0732830357304275));
#49173=CARTESIAN_POINT('Ctrl Pts',(2.19213712012956,1.,0.0732830357304275));
#49174=CARTESIAN_POINT('Ctrl Pts',(2.19552129483562,-1.,0.0713863779524626));
#49175=CARTESIAN_POINT('Ctrl Pts',(2.19552129483562,1.,0.0713863779524626));
#49176=CARTESIAN_POINT('Ctrl Pts',(2.19777582085261,-1.,0.0701143536324925));
#49177=CARTESIAN_POINT('Ctrl Pts',(2.19777582085261,1.,0.0701143536324925));
#49178=CARTESIAN_POINT('Ctrl Pts',(2.19890268624765,-1.,0.0694764450219582));
#49179=CARTESIAN_POINT('Ctrl Pts',(2.19890268624765,1.,0.0694764450219582));
#49180=CARTESIAN_POINT('',(1.74236521665491,1.,0.163289472382896));
#49181=CARTESIAN_POINT('Ctrl Pts',(1.74236521665491,1.,0.163289472382896));
#49182=CARTESIAN_POINT('Ctrl Pts',(1.74720349503904,1.,0.163814161002474));
#49183=CARTESIAN_POINT('Ctrl Pts',(1.75666056640041,1.,0.164834765708484));
#49184=CARTESIAN_POINT('Ctrl Pts',(1.77018771687692,1.,0.166279355148738));
#49185=CARTESIAN_POINT('Ctrl Pts',(1.78690649988931,1.,0.16803277280837));
#49186=CARTESIAN_POINT('Ctrl Pts',(1.80561530633924,1.,0.169936923908078));
#49187=CARTESIAN_POINT('Ctrl Pts',(1.82215766815414,1.,0.171554770207306));
#49188=CARTESIAN_POINT('Ctrl Pts',(1.83658380530747,1.,0.17288944289442));
#49189=CARTESIAN_POINT('Ctrl Pts',(1.84898113200543,1.,0.173946627589401));
#49190=CARTESIAN_POINT('Ctrl Pts',(1.85948367089838,1.,0.174735259276856));
#49191=CARTESIAN_POINT('Ctrl Pts',(1.86828349694972,1.,0.1752683375909));
#49192=CARTESIAN_POINT('Ctrl Pts',(1.87563767773249,1.,0.175563480746205));
#49193=CARTESIAN_POINT('Ctrl Pts',(1.88188663144846,1.,0.175644148889271));
#49194=CARTESIAN_POINT('Ctrl Pts',(1.88742606272818,1.,0.175538155840286));
#49195=CARTESIAN_POINT('Ctrl Pts',(1.89264630198279,1.,0.175274276190664));
#49196=CARTESIAN_POINT('Ctrl Pts',(1.89788101117148,1.,0.174879405091277));
#49197=CARTESIAN_POINT('Ctrl Pts',(1.90335253863003,1.,0.174375518661222));
#49198=CARTESIAN_POINT('Ctrl Pts',(1.90911693975475,1.,0.173776635257983));
#49199=CARTESIAN_POINT('Ctrl Pts',(1.91511429159681,1.,0.173090695383619));
#49200=CARTESIAN_POINT('Ctrl Pts',(1.92122334398034,1.,0.172321621259556));
#49201=CARTESIAN_POINT('Ctrl Pts',(1.92731093582,1.,0.17147119153296));
#49202=CARTESIAN_POINT('Ctrl Pts',(1.93329183155455,1.,0.170541253116136));
#49203=CARTESIAN_POINT('Ctrl Pts',(1.93915639211497,1.,0.169534904817425));
#49204=CARTESIAN_POINT('Ctrl Pts',(1.94493757756879,1.,0.168455741607515));
#49205=CARTESIAN_POINT('Ctrl Pts',(1.95069027794286,1.,0.167307501784469));
#49206=CARTESIAN_POINT('Ctrl Pts',(1.95646759718755,1.,0.166093592002832));
#49207=CARTESIAN_POINT('Ctrl Pts',(1.96229379940174,1.,0.1648165689203));
#49208=CARTESIAN_POINT('Ctrl Pts',(1.96816512678,1.,0.16347818545776));
#49209=CARTESIAN_POINT('Ctrl Pts',(1.97406280235204,1.,0.162079693556302));
#49210=CARTESIAN_POINT('Ctrl Pts',(1.97996195437557,1.,0.16062206078461));
#49211=CARTESIAN_POINT('Ctrl Pts',(1.98584238283279,1.,0.159106226437288));
#49212=CARTESIAN_POINT('Ctrl Pts',(1.99169810931893,1.,0.157533331459215));
#49213=CARTESIAN_POINT('Ctrl Pts',(1.99753284771487,1.,0.155904629548774));
#49214=CARTESIAN_POINT('Ctrl Pts',(2.00335565310539,1.,0.154221403049719));
#49215=CARTESIAN_POINT('Ctrl Pts',(2.00917680318426,1.,0.152484883621452));
#49216=CARTESIAN_POINT('Ctrl Pts',(2.01500291940243,1.,0.150696157673084));
#49217=CARTESIAN_POINT('Ctrl Pts',(2.02083464969897,1.,0.148856124775342));
#49218=CARTESIAN_POINT('Ctrl Pts',(2.02666926182017,1.,0.146965557332586));
#49219=CARTESIAN_POINT('Ctrl Pts',(2.03250223739941,1.,0.145025140186058));
#49220=CARTESIAN_POINT('Ctrl Pts',(2.03832911025913,1.,0.143035515058208));
#49221=CARTESIAN_POINT('Ctrl Pts',(2.04414757947919,1.,0.140997332152545));
#49222=CARTESIAN_POINT('Ctrl Pts',(2.04995762001333,1.,0.138911255368966));
#49223=CARTESIAN_POINT('Ctrl Pts',(2.0557604441427,1.,0.136777941218044));
#49224=CARTESIAN_POINT('Ctrl Pts',(2.06155781517844,1.,0.134598026192107));
#49225=CARTESIAN_POINT('Ctrl Pts',(2.06735123910319,1.,0.132372111547709));
#49226=CARTESIAN_POINT('Ctrl Pts',(2.07314114713047,1.,0.1301007483284));
#49227=CARTESIAN_POINT('Ctrl Pts',(2.07892715110967,1.,0.127784445276116));
#49228=CARTESIAN_POINT('Ctrl Pts',(2.08470840653628,1.,0.125423679412058));
#49229=CARTESIAN_POINT('Ctrl Pts',(2.09048392424826,1.,0.123018905621083));
#49230=CARTESIAN_POINT('Ctrl Pts',(2.09625292867756,1.,0.120570567965129));
#49231=CARTESIAN_POINT('Ctrl Pts',(2.10201512132945,1.,0.118079107988368));
#49232=CARTESIAN_POINT('Ctrl Pts',(2.10777050261359,1.,0.11554495768794));
#49233=CARTESIAN_POINT('Ctrl Pts',(2.11351924490335,1.,0.112968534419746));
#49234=CARTESIAN_POINT('Ctrl Pts',(2.11926155590849,1.,0.11035023613502));
#49235=CARTESIAN_POINT('Ctrl Pts',(2.12499752306927,1.,0.107690435231068));
#49236=CARTESIAN_POINT('Ctrl Pts',(2.1307270488718,1.,0.104989479152703));
#49237=CARTESIAN_POINT('Ctrl Pts',(2.13644992667052,1.,0.102247700556063));
#49238=CARTESIAN_POINT('Ctrl Pts',(2.14216588395974,1.,0.0994654261990741));
#49239=CARTESIAN_POINT('Ctrl Pts',(2.14787463531864,1.,0.0966429852305688));
#49240=CARTESIAN_POINT('Ctrl Pts',(2.15357593978377,1.,0.0937807218868344));
#49241=CARTESIAN_POINT('Ctrl Pts',(2.15926961544808,1.,0.0908789888108265));
#49242=CARTESIAN_POINT('Ctrl Pts',(2.16495552645275,1.,0.0879381291387821));
#49243=CARTESIAN_POINT('Ctrl Pts',(2.17063357871031,1.,0.0849584620835642));
#49244=CARTESIAN_POINT('Ctrl Pts',(2.1763037121106,1.,0.0819402680871938));
#49245=CARTESIAN_POINT('Ctrl Pts',(2.18196589448304,1.,0.0788837727683226));
#49246=CARTESIAN_POINT('Ctrl Pts',(2.1876201139874,1.,0.075789146583341));
#49247=CARTESIAN_POINT('Ctrl Pts',(2.19213712012956,1.,0.0732830357304275));
#49248=CARTESIAN_POINT('Ctrl Pts',(2.19552129483562,1.,0.0713863779524626));
#49249=CARTESIAN_POINT('Ctrl Pts',(2.19777582085261,1.,0.0701143536324925));
#49250=CARTESIAN_POINT('Ctrl Pts',(2.19890268624765,1.,0.0694764450219582));
#49251=CARTESIAN_POINT('',(1.74236521665491,0.,0.163289472382896));
#49252=CARTESIAN_POINT('Origin',(0.,1.,0.));
#49253=CARTESIAN_POINT('Origin',(0.,1.,0.));
#49254=CARTESIAN_POINT('Origin',(0.,0.,0.));
#49255=CARTESIAN_POINT('',(0.,0.,0.));
#49256=CARTESIAN_POINT('',(0.,0.,0.));
#49257=CARTESIAN_POINT('Origin',(11.5440066084244,1.6,8.0297030612521));
#49258=CARTESIAN_POINT('',(11.6260795927575,3.6,9.07253920349826));
#49259=CARTESIAN_POINT('',(11.6260795927575,1.6,9.07253920349826));
#49260=CARTESIAN_POINT('',(11.6260795927575,-9.4,9.07253920349826));
#49261=CARTESIAN_POINT('',(11.649926387657,3.6,9.37554146179182));
#49262=CARTESIAN_POINT('',(11.649926387657,3.6,9.37554146179182));
#49263=CARTESIAN_POINT('',(11.649926387657,1.6,9.37554146179182));
#49264=CARTESIAN_POINT('',(11.649926387657,1.6,9.37554146179182));
#49265=CARTESIAN_POINT('',(11.649926387657,1.6,9.37554146179182));
#49266=CARTESIAN_POINT('Origin',(11.8960416981606,1.6,8.67908453280361));
#49267=CARTESIAN_POINT('',(12.2242299929974,1.6,9.02546374606156));
#49268=CARTESIAN_POINT('Origin',(12.,1.6,10.));
#49269=CARTESIAN_POINT('',(12.2480767878968,1.6,9.32846600435511));
#49270=CARTESIAN_POINT('',(12.2480767878968,1.6,9.32846600435511));
#49271=CARTESIAN_POINT('',(12.1421570086642,1.6,7.98262760381539));
#49272=CARTESIAN_POINT('Origin',(12.2480767878968,1.6,9.32846600435511));
#49273=CARTESIAN_POINT('',(12.2242299929974,3.6,9.02546374606156));
#49274=CARTESIAN_POINT('',(12.2242299929974,-9.4,9.02546374606156));
#49275=CARTESIAN_POINT('',(12.2480767878968,3.6,9.32846600435511));
#49276=CARTESIAN_POINT('',(12.2480767878968,1.6,9.32846600435511));
#49277=CARTESIAN_POINT('',(12.1421570086642,3.6,7.98262760381539));
#49278=CARTESIAN_POINT('Origin',(11.649926387657,1.6,9.37554146179182));
#49279=CARTESIAN_POINT('',(12.2480767878968,3.6,9.32846600435511));
#49280=CARTESIAN_POINT('Origin',(11.8960416981606,3.6,8.67908453280361));
#49281=CARTESIAN_POINT('Origin',(12.,3.6,10.));
#49282=CARTESIAN_POINT('Origin',(12.,-9.4,10.));
#49283=CARTESIAN_POINT('',(11.,9.4,10.));
#49284=CARTESIAN_POINT('Origin',(12.,9.4,10.));
#49285=CARTESIAN_POINT('',(11.,-9.4,10.));
#49286=CARTESIAN_POINT('',(11.,-9.4,10.));
#49287=CARTESIAN_POINT('Origin',(12.,-9.4,10.));
#49288=CARTESIAN_POINT('Origin',(12.,9.4,10.));
#49289=CARTESIAN_POINT('Origin',(12.,-9.4,10.));
#49290=CARTESIAN_POINT('',(0.,0.,0.));
#49291=CARTESIAN_POINT('Origin',(12.,-8.2,10.99));
#49292=CARTESIAN_POINT('',(12.1729884389201,-8.31905880899792,10.99));
#49293=CARTESIAN_POINT('',(12.1729884389201,-8.08094119100208,10.99));
#49294=CARTESIAN_POINT('',(12.1729884389201,-8.6,10.99));
#49295=CARTESIAN_POINT('Origin',(12.,-8.2,10.99));
#49296=CARTESIAN_POINT('Origin',(12.,-8.2,10.99));
#49297=CARTESIAN_POINT('',(11.8270115610799,-8.31905880899792,10.99));
#49298=CARTESIAN_POINT('Ctrl Pts',(11.8270115610799,-8.31905880899792,10.99));
#49299=CARTESIAN_POINT('Ctrl Pts',(11.8344051346887,-8.3298014223953,10.9912919219764));
#49300=CARTESIAN_POINT('Ctrl Pts',(11.8427028612744,-8.33968770937274,10.992653949439));
#49301=CARTESIAN_POINT('Ctrl Pts',(11.8701079261549,-8.36709277425327,10.9967480843909));
#49302=CARTESIAN_POINT('Ctrl Pts',(11.8936698322407,-8.38324205633295,10.9996958932764));
#49303=CARTESIAN_POINT('Ctrl Pts',(11.9453870953676,-8.40469779396491,11.0038502947236));
#49304=CARTESIAN_POINT('Ctrl Pts',(11.9735487691701,-8.41,11.005));
#49305=CARTESIAN_POINT('Ctrl Pts',(12.0264512308299,-8.41,11.005));
#49306=CARTESIAN_POINT('Ctrl Pts',(12.0546129046324,-8.40469779396491,11.0038502947236));
#49307=CARTESIAN_POINT('Ctrl Pts',(12.1063301677593,-8.38324205633295,10.9996958932764));
#49308=CARTESIAN_POINT('Ctrl Pts',(12.1298920738451,-8.36709277425327,10.9967480843909));
#49309=CARTESIAN_POINT('Ctrl Pts',(12.1572971387256,-8.33968770937274,10.992653949439));
#49310=CARTESIAN_POINT('Ctrl Pts',(12.1655948653113,-8.32980142239529,10.9912919219764));
#49311=CARTESIAN_POINT('Ctrl Pts',(12.1729884389201,-8.31905880899792,10.99));
#49312=CARTESIAN_POINT('',(11.79,-8.2,10.99));
#49313=CARTESIAN_POINT('Origin',(12.,-8.2,10.99));
#49314=CARTESIAN_POINT('',(11.79,-8.2,11.38416039533));
#49315=CARTESIAN_POINT('',(11.79,-8.2,10.99));
#49316=CARTESIAN_POINT('',(12.21,-8.2,11.38416039533));
#49317=CARTESIAN_POINT('Ctrl Pts',(12.21,-8.2,11.38416039533));
#49318=CARTESIAN_POINT('Ctrl Pts',(12.21,-8.22641116018714,11.38416039533));
#49319=CARTESIAN_POINT('Ctrl Pts',(12.2047135491119,-8.2545550596171,11.3849944296993));
#49320=CARTESIAN_POINT('Ctrl Pts',(12.1832699958585,-8.30628264999174,11.3879947099895));
#49321=CARTESIAN_POINT('Ctrl Pts',(12.1671150376064,-8.32986981049192,11.3901162943626));
#49322=CARTESIAN_POINT('Ctrl Pts',(12.1298701351968,-8.36711471290156,11.394089123191));
#49323=CARTESIAN_POINT('Ctrl Pts',(12.1062828345902,-8.38326992585508,11.3962002442067));
#49324=CARTESIAN_POINT('Ctrl Pts',(12.0545547656039,-8.40471366447292,11.3991765222353));
#49325=CARTESIAN_POINT('Ctrl Pts',(12.0264106996808,-8.41,11.4));
#49326=CARTESIAN_POINT('Ctrl Pts',(11.9735893003192,-8.41,11.4));
#49327=CARTESIAN_POINT('Ctrl Pts',(11.9454452343961,-8.40471366447292,11.3991765222353));
#49328=CARTESIAN_POINT('Ctrl Pts',(11.8937171654098,-8.38326992585508,11.3962002442067));
#49329=CARTESIAN_POINT('Ctrl Pts',(11.8701298648032,-8.36711471290156,11.394089123191));
#49330=CARTESIAN_POINT('Ctrl Pts',(11.8328849623936,-8.32986981049192,11.3901162943626));
#49331=CARTESIAN_POINT('Ctrl Pts',(11.8167300041415,-8.30628264999174,11.3879947099895));
#49332=CARTESIAN_POINT('Ctrl Pts',(11.7952864508881,-8.2545550596171,11.3849944296993));
#49333=CARTESIAN_POINT('Ctrl Pts',(11.79,-8.22641116018714,11.38416039533));
#49334=CARTESIAN_POINT('Ctrl Pts',(11.79,-8.2,11.38416039533));
#49335=CARTESIAN_POINT('Ctrl Pts',(11.79,-8.2,11.38416039533));
#49336=CARTESIAN_POINT('Ctrl Pts',(11.79,-8.17358883981285,11.38416039533));
#49337=CARTESIAN_POINT('Ctrl Pts',(11.7952864508881,-8.1454449403829,11.3849944296993));
#49338=CARTESIAN_POINT('Ctrl Pts',(11.8167300041415,-8.09371735000826,11.3879947099895));
#49339=CARTESIAN_POINT('Ctrl Pts',(11.8328849623936,-8.07013018950807,11.3901162943626));
#49340=CARTESIAN_POINT('Ctrl Pts',(11.8701298648032,-8.03288528709843,11.394089123191));
#49341=CARTESIAN_POINT('Ctrl Pts',(11.8937171654098,-8.01673007414492,11.3962002442067));
#49342=CARTESIAN_POINT('Ctrl Pts',(11.9454452343961,-7.99528633552708,11.3991765222353));
#49343=CARTESIAN_POINT('Ctrl Pts',(11.9735893003192,-7.99,11.4));
#49344=CARTESIAN_POINT('Ctrl Pts',(12.0264106996808,-7.99,11.4));
#49345=CARTESIAN_POINT('Ctrl Pts',(12.0545547656039,-7.99528633552708,11.3991765222353));
#49346=CARTESIAN_POINT('Ctrl Pts',(12.1062828345902,-8.01673007414492,11.3962002442067));
#49347=CARTESIAN_POINT('Ctrl Pts',(12.1298701351968,-8.03288528709843,11.394089123191));
#49348=CARTESIAN_POINT('Ctrl Pts',(12.1671150376064,-8.07013018950807,11.3901162943626));
#49349=CARTESIAN_POINT('Ctrl Pts',(12.1832699958585,-8.09371735000826,11.3879947099895));
#49350=CARTESIAN_POINT('Ctrl Pts',(12.2047135491119,-8.1454449403829,11.3849944296993));
#49351=CARTESIAN_POINT('Ctrl Pts',(12.21,-8.17358883981285,11.38416039533));
#49352=CARTESIAN_POINT('Ctrl Pts',(12.21,-8.2,11.38416039533));
#49353=CARTESIAN_POINT('',(11.8270115610799,-8.08094119100208,10.99));
#49354=CARTESIAN_POINT('Origin',(12.,-8.2,10.99));
#49355=CARTESIAN_POINT('Ctrl Pts',(12.1729884389201,-8.08094119100208,10.99));
#49356=CARTESIAN_POINT('Ctrl Pts',(12.1655948653113,-8.07019857760471,10.9912919219764));
#49357=CARTESIAN_POINT('Ctrl Pts',(12.1572971387256,-8.06031229062725,10.992653949439));
#49358=CARTESIAN_POINT('Ctrl Pts',(12.1298920738451,-8.03290722574673,10.9967480843909));
#49359=CARTESIAN_POINT('Ctrl Pts',(12.1063301677593,-8.01675794366705,10.9996958932764));
#49360=CARTESIAN_POINT('Ctrl Pts',(12.0546129046324,-7.99530220603509,11.0038502947236));
#49361=CARTESIAN_POINT('Ctrl Pts',(12.0264512308299,-7.99,11.005));
#49362=CARTESIAN_POINT('Ctrl Pts',(11.9735487691701,-7.99,11.005));
#49363=CARTESIAN_POINT('Ctrl Pts',(11.9453870953676,-7.99530220603509,11.0038502947236));
#49364=CARTESIAN_POINT('Ctrl Pts',(11.8936698322407,-8.01675794366705,10.9996958932764));
#49365=CARTESIAN_POINT('Ctrl Pts',(11.8701079261549,-8.03290722574673,10.9967480843909));
#49366=CARTESIAN_POINT('Ctrl Pts',(11.8427028612744,-8.06031229062725,10.992653949439));
#49367=CARTESIAN_POINT('Ctrl Pts',(11.8344051346887,-8.0701985776047,10.9912919219764));
#49368=CARTESIAN_POINT('Ctrl Pts',(11.8270115610799,-8.08094119100208,10.99));
#49369=CARTESIAN_POINT('Origin',(12.,-8.2,10.99));
#49370=CARTESIAN_POINT('',(11.8270115610799,-8.6,10.99));
#49371=CARTESIAN_POINT('Origin',(12.,-8.6,10.));
#49372=CARTESIAN_POINT('',(10.995,-7.8,10.));
#49373=CARTESIAN_POINT('Origin',(12.,-7.8,10.));
#49374=CARTESIAN_POINT('',(10.995,-8.6,10.));
#49375=CARTESIAN_POINT('',(10.995,-8.6,10.));
#49376=CARTESIAN_POINT('Origin',(12.,-8.6,10.));
#49377=CARTESIAN_POINT('Origin',(12.,-8.6,10.));
#49378=CARTESIAN_POINT('',(10.6,-7.8,10.));
#49379=CARTESIAN_POINT('Origin',(12.,-7.8,10.));
#49380=CARTESIAN_POINT('',(10.6,-8.6,10.));
#49381=CARTESIAN_POINT('',(10.6,-8.6,10.));
#49382=CARTESIAN_POINT('Origin',(12.,-8.6,10.));
#49383=CARTESIAN_POINT('Origin',(12.,-7.8,10.));
#49384=CARTESIAN_POINT('Origin',(12.,-8.6,10.));
#49385=CARTESIAN_POINT('',(0.,0.,0.));
#49386=CARTESIAN_POINT('Origin',(12.,8.2,10.99));
#49387=CARTESIAN_POINT('',(12.1729884389201,8.08094119100208,10.99));
#49388=CARTESIAN_POINT('',(12.1729884389201,8.31905880899792,10.99));
#49389=CARTESIAN_POINT('',(12.1729884389201,7.8,10.99));
#49390=CARTESIAN_POINT('Origin',(12.,8.2,10.99));
#49391=CARTESIAN_POINT('Origin',(12.,8.2,10.99));
#49392=CARTESIAN_POINT('',(11.8270115610799,8.08094119100208,10.99));
#49393=CARTESIAN_POINT('Ctrl Pts',(11.8270115610799,8.08094119100208,10.99));
#49394=CARTESIAN_POINT('Ctrl Pts',(11.8344051346887,8.0701985776047,10.9912919219764));
#49395=CARTESIAN_POINT('Ctrl Pts',(11.8427028612744,8.06031229062725,10.992653949439));
#49396=CARTESIAN_POINT('Ctrl Pts',(11.8701079261549,8.03290722574673,10.9967480843909));
#49397=CARTESIAN_POINT('Ctrl Pts',(11.8936698322407,8.01675794366705,10.9996958932764));
#49398=CARTESIAN_POINT('Ctrl Pts',(11.9453870953676,7.99530220603509,11.0038502947236));
#49399=CARTESIAN_POINT('Ctrl Pts',(11.9735487691701,7.99,11.005));
#49400=CARTESIAN_POINT('Ctrl Pts',(12.0264512308299,7.99,11.005));
#49401=CARTESIAN_POINT('Ctrl Pts',(12.0546129046324,7.99530220603509,11.0038502947236));
#49402=CARTESIAN_POINT('Ctrl Pts',(12.1063301677593,8.01675794366705,10.9996958932764));
#49403=CARTESIAN_POINT('Ctrl Pts',(12.1298920738451,8.03290722574673,10.9967480843909));
#49404=CARTESIAN_POINT('Ctrl Pts',(12.1572971387256,8.06031229062725,10.992653949439));
#49405=CARTESIAN_POINT('Ctrl Pts',(12.1655948653113,8.0701985776047,10.9912919219764));
#49406=CARTESIAN_POINT('Ctrl Pts',(12.1729884389201,8.08094119100208,10.99));
#49407=CARTESIAN_POINT('',(11.79,8.2,10.99));
#49408=CARTESIAN_POINT('Origin',(12.,8.2,10.99));
#49409=CARTESIAN_POINT('',(11.79,8.2,11.38416039533));
#49410=CARTESIAN_POINT('',(11.79,8.2,10.99));
#49411=CARTESIAN_POINT('',(12.21,8.2,11.38416039533));
#49412=CARTESIAN_POINT('Ctrl Pts',(12.21,8.2,11.38416039533));
#49413=CARTESIAN_POINT('Ctrl Pts',(12.21,8.17358883981285,11.38416039533));
#49414=CARTESIAN_POINT('Ctrl Pts',(12.2047135491119,8.1454449403829,11.3849944296993));
#49415=CARTESIAN_POINT('Ctrl Pts',(12.1832699958585,8.09371735000826,11.3879947099895));
#49416=CARTESIAN_POINT('Ctrl Pts',(12.1671150376064,8.07013018950807,11.3901162943626));
#49417=CARTESIAN_POINT('Ctrl Pts',(12.1298701351968,8.03288528709843,11.394089123191));
#49418=CARTESIAN_POINT('Ctrl Pts',(12.1062828345902,8.01673007414492,11.3962002442067));
#49419=CARTESIAN_POINT('Ctrl Pts',(12.0545547656039,7.99528633552708,11.3991765222353));
#49420=CARTESIAN_POINT('Ctrl Pts',(12.0264106996808,7.99,11.4));
#49421=CARTESIAN_POINT('Ctrl Pts',(11.9735893003192,7.99,11.4));
#49422=CARTESIAN_POINT('Ctrl Pts',(11.9454452343961,7.99528633552708,11.3991765222353));
#49423=CARTESIAN_POINT('Ctrl Pts',(11.8937171654098,8.01673007414492,11.3962002442067));
#49424=CARTESIAN_POINT('Ctrl Pts',(11.8701298648032,8.03288528709843,11.394089123191));
#49425=CARTESIAN_POINT('Ctrl Pts',(11.8328849623936,8.07013018950807,11.3901162943626));
#49426=CARTESIAN_POINT('Ctrl Pts',(11.8167300041415,8.09371735000826,11.3879947099895));
#49427=CARTESIAN_POINT('Ctrl Pts',(11.7952864508881,8.1454449403829,11.3849944296993));
#49428=CARTESIAN_POINT('Ctrl Pts',(11.79,8.17358883981285,11.38416039533));
#49429=CARTESIAN_POINT('Ctrl Pts',(11.79,8.2,11.38416039533));
#49430=CARTESIAN_POINT('Ctrl Pts',(11.79,8.2,11.38416039533));
#49431=CARTESIAN_POINT('Ctrl Pts',(11.79,8.22641116018714,11.38416039533));
#49432=CARTESIAN_POINT('Ctrl Pts',(11.7952864508881,8.2545550596171,11.3849944296993));
#49433=CARTESIAN_POINT('Ctrl Pts',(11.8167300041415,8.30628264999174,11.3879947099895));
#49434=CARTESIAN_POINT('Ctrl Pts',(11.8328849623936,8.32986981049192,11.3901162943626));
#49435=CARTESIAN_POINT('Ctrl Pts',(11.8701298648032,8.36711471290156,11.394089123191));
#49436=CARTESIAN_POINT('Ctrl Pts',(11.8937171654098,8.38326992585508,11.3962002442067));
#49437=CARTESIAN_POINT('Ctrl Pts',(11.9454452343961,8.40471366447292,11.3991765222353));
#49438=CARTESIAN_POINT('Ctrl Pts',(11.9735893003192,8.41,11.4));
#49439=CARTESIAN_POINT('Ctrl Pts',(12.0264106996808,8.41,11.4));
#49440=CARTESIAN_POINT('Ctrl Pts',(12.0545547656039,8.40471366447292,11.3991765222353));
#49441=CARTESIAN_POINT('Ctrl Pts',(12.1062828345902,8.38326992585508,11.3962002442067));
#49442=CARTESIAN_POINT('Ctrl Pts',(12.1298701351968,8.36711471290156,11.394089123191));
#49443=CARTESIAN_POINT('Ctrl Pts',(12.1671150376064,8.32986981049192,11.3901162943626));
#49444=CARTESIAN_POINT('Ctrl Pts',(12.1832699958585,8.30628264999174,11.3879947099895));
#49445=CARTESIAN_POINT('Ctrl Pts',(12.2047135491119,8.2545550596171,11.3849944296993));
#49446=CARTESIAN_POINT('Ctrl Pts',(12.21,8.22641116018714,11.38416039533));
#49447=CARTESIAN_POINT('Ctrl Pts',(12.21,8.2,11.38416039533));
#49448=CARTESIAN_POINT('',(11.8270115610799,8.31905880899792,10.99));
#49449=CARTESIAN_POINT('Origin',(12.,8.2,10.99));
#49450=CARTESIAN_POINT('Ctrl Pts',(12.1729884389201,8.31905880899792,10.99));
#49451=CARTESIAN_POINT('Ctrl Pts',(12.1655948653113,8.32980142239529,10.9912919219764));
#49452=CARTESIAN_POINT('Ctrl Pts',(12.1572971387256,8.33968770937275,10.992653949439));
#49453=CARTESIAN_POINT('Ctrl Pts',(12.1298920738451,8.36709277425327,10.9967480843909));
#49454=CARTESIAN_POINT('Ctrl Pts',(12.1063301677593,8.38324205633295,10.9996958932764));
#49455=CARTESIAN_POINT('Ctrl Pts',(12.0546129046324,8.40469779396491,11.0038502947236));
#49456=CARTESIAN_POINT('Ctrl Pts',(12.0264512308299,8.41,11.005));
#49457=CARTESIAN_POINT('Ctrl Pts',(11.9735487691701,8.41,11.005));
#49458=CARTESIAN_POINT('Ctrl Pts',(11.9453870953676,8.40469779396491,11.0038502947236));
#49459=CARTESIAN_POINT('Ctrl Pts',(11.8936698322407,8.38324205633295,10.9996958932764));
#49460=CARTESIAN_POINT('Ctrl Pts',(11.8701079261549,8.36709277425327,10.9967480843909));
#49461=CARTESIAN_POINT('Ctrl Pts',(11.8427028612744,8.33968770937274,10.992653949439));
#49462=CARTESIAN_POINT('Ctrl Pts',(11.8344051346887,8.3298014223953,10.9912919219764));
#49463=CARTESIAN_POINT('Ctrl Pts',(11.8270115610799,8.31905880899792,10.99));
#49464=CARTESIAN_POINT('Origin',(12.,8.2,10.99));
#49465=CARTESIAN_POINT('',(11.8270115610799,7.8,10.99));
#49466=CARTESIAN_POINT('Origin',(12.,7.8,10.));
#49467=CARTESIAN_POINT('',(10.995,8.6,10.));
#49468=CARTESIAN_POINT('Origin',(12.,8.6,10.));
#49469=CARTESIAN_POINT('',(10.995,7.8,10.));
#49470=CARTESIAN_POINT('',(10.995,7.8,10.));
#49471=CARTESIAN_POINT('Origin',(12.,7.8,10.));
#49472=CARTESIAN_POINT('Origin',(12.,7.8,10.));
#49473=CARTESIAN_POINT('',(10.6,8.6,10.));
#49474=CARTESIAN_POINT('Origin',(12.,8.6,10.));
#49475=CARTESIAN_POINT('',(10.6,7.8,10.));
#49476=CARTESIAN_POINT('',(10.6,7.8,10.));
#49477=CARTESIAN_POINT('Origin',(12.,7.8,10.));
#49478=CARTESIAN_POINT('Origin',(12.,8.6,10.));
#49479=CARTESIAN_POINT('Origin',(12.,7.8,10.));
#49480=CARTESIAN_POINT('',(0.,0.,0.));
#49481=CARTESIAN_POINT('Origin',(12.,-7.8,10.));
#49482=CARTESIAN_POINT('',(10.995,-6.7,10.));
#49483=CARTESIAN_POINT('Origin',(12.,-6.7,10.));
#49484=CARTESIAN_POINT('',(10.995,-7.8,10.));
#49485=CARTESIAN_POINT('',(10.995,-7.8,10.));
#49486=CARTESIAN_POINT('Origin',(12.,-7.8,10.));
#49487=CARTESIAN_POINT('Origin',(12.,-7.8,10.));
#49488=CARTESIAN_POINT('',(10.7,-6.7,10.));
#49489=CARTESIAN_POINT('Origin',(12.,-6.7,10.));
#49490=CARTESIAN_POINT('',(10.7,-7.8,10.));
#49491=CARTESIAN_POINT('',(10.7,-7.8,10.));
#49492=CARTESIAN_POINT('Origin',(12.,-7.8,10.));
#49493=CARTESIAN_POINT('Origin',(12.,-6.7,10.));
#49494=CARTESIAN_POINT('Origin',(12.,-7.8,10.));
#49495=CARTESIAN_POINT('',(0.,0.,0.));
#49496=CARTESIAN_POINT('Origin',(12.,6.7,10.));
#49497=CARTESIAN_POINT('',(10.995,7.8,10.));
#49498=CARTESIAN_POINT('Origin',(12.,7.8,10.));
#49499=CARTESIAN_POINT('',(10.995,6.7,10.));
#49500=CARTESIAN_POINT('',(10.995,6.7,10.));
#49501=CARTESIAN_POINT('Origin',(12.,6.7,10.));
#49502=CARTESIAN_POINT('Origin',(12.,6.7,10.));
#49503=CARTESIAN_POINT('',(10.7,7.8,10.));
#49504=CARTESIAN_POINT('Origin',(12.,7.8,10.));
#49505=CARTESIAN_POINT('',(10.7,6.7,10.));
#49506=CARTESIAN_POINT('',(10.7,6.7,10.));
#49507=CARTESIAN_POINT('Origin',(12.,6.7,10.));
#49508=CARTESIAN_POINT('Origin',(12.,7.8,10.));
#49509=CARTESIAN_POINT('Origin',(12.,6.7,10.));
#49510=CARTESIAN_POINT('',(0.,0.,0.));
#49511=CARTESIAN_POINT('Origin',(12.,-5.3,10.));
#49512=CARTESIAN_POINT('',(10.995,1.,10.));
#49513=CARTESIAN_POINT('Origin',(12.,1.,10.));
#49514=CARTESIAN_POINT('',(10.995,-5.3,10.));
#49515=CARTESIAN_POINT('',(10.995,-5.3,10.));
#49516=CARTESIAN_POINT('Origin',(12.,-5.3,10.));
#49517=CARTESIAN_POINT('Origin',(12.,-5.3,10.));
#49518=CARTESIAN_POINT('',(10.7,1.,10.));
#49519=CARTESIAN_POINT('Origin',(12.,1.,10.));
#49520=CARTESIAN_POINT('',(10.7,-5.3,10.));
#49521=CARTESIAN_POINT('',(10.7,-5.3,10.));
#49522=CARTESIAN_POINT('Origin',(12.,-5.3,10.));
#49523=CARTESIAN_POINT('Origin',(12.,1.,10.));
#49524=CARTESIAN_POINT('Origin',(12.,-5.3,10.));
#49525=CARTESIAN_POINT('',(0.,0.,0.));
#49526=CARTESIAN_POINT('Origin',(12.,4.2,10.));
#49527=CARTESIAN_POINT('',(10.995,5.3,10.));
#49528=CARTESIAN_POINT('Origin',(12.,5.3,10.));
#49529=CARTESIAN_POINT('',(10.995,4.2,10.));
#49530=CARTESIAN_POINT('',(10.995,4.2,10.));
#49531=CARTESIAN_POINT('Origin',(12.,4.2,10.));
#49532=CARTESIAN_POINT('Origin',(12.,4.2,10.));
#49533=CARTESIAN_POINT('',(10.7,5.3,10.));
#49534=CARTESIAN_POINT('Origin',(12.,5.3,10.));
#49535=CARTESIAN_POINT('',(10.7,4.2,10.));
#49536=CARTESIAN_POINT('',(10.7,4.2,10.));
#49537=CARTESIAN_POINT('Origin',(12.,4.2,10.));
#49538=CARTESIAN_POINT('Origin',(12.,5.3,10.));
#49539=CARTESIAN_POINT('Origin',(12.,4.2,10.));
#49540=CARTESIAN_POINT('',(0.,0.,0.));
#49541=CARTESIAN_POINT('Origin',(0.0721687836487032,0.,-0.125));
#49542=CARTESIAN_POINT('',(0.0721687836487032,0.,-0.125));
#49543=CARTESIAN_POINT('',(0.144337567297406,0.,0.));
#49544=CARTESIAN_POINT('',(0.117710979560879,0.,-0.0461186027918559));
#49545=CARTESIAN_POINT('',(0.0721687836487032,-0.25,-0.125));
#49546=CARTESIAN_POINT('',(0.0721687836487032,0.,-0.125));
#49547=CARTESIAN_POINT('',(0.144337567297406,-0.25,0.));
#49548=CARTESIAN_POINT('',(0.144337567297406,-0.25,0.));
#49549=CARTESIAN_POINT('',(0.144337567297406,0.,0.));
#49550=CARTESIAN_POINT('Origin',(-0.0721687836487032,0.,-0.125));
#49551=CARTESIAN_POINT('',(-0.0721687836487032,0.,-0.125));
#49552=CARTESIAN_POINT('',(0.0739156081756484,0.,-0.125));
#49553=CARTESIAN_POINT('',(-0.0721687836487032,-0.25,-0.125));
#49554=CARTESIAN_POINT('',(-0.0721687836487032,0.,-0.125));
#49555=CARTESIAN_POINT('',(0.0721687836487032,-0.25,-0.125));
#49556=CARTESIAN_POINT('Origin',(-0.144337567297406,0.,-4.16333634234434E-17));
#49557=CARTESIAN_POINT('',(-0.144337567297406,0.,-1.76762539787485E-17));
#49558=CARTESIAN_POINT('',(-0.0987953713852306,0.,-0.0788813972081442));
#49559=CARTESIAN_POINT('',(-0.144337567297406,-0.25,-2.77555756156289E-17));
#49560=CARTESIAN_POINT('',(-0.144337567297406,0.,-1.76762539787485E-17));
#49561=CARTESIAN_POINT('',(-0.0721687836487032,-0.25,-0.125));
#49562=CARTESIAN_POINT('Origin',(-0.0721687836487033,0.,0.125));
#49563=CARTESIAN_POINT('',(-0.0721687836487033,0.,0.125));
#49564=CARTESIAN_POINT('',(-0.0627109795608791,0.,0.141381397208144));
#49565=CARTESIAN_POINT('',(-0.0721687836487033,-0.25,0.125));
#49566=CARTESIAN_POINT('',(-0.0721687836487033,0.,0.125));
#49567=CARTESIAN_POINT('',(-0.144337567297406,-0.25,-1.76762539787485E-17));
#49568=CARTESIAN_POINT('Origin',(0.0721687836487032,0.,0.125));
#49569=CARTESIAN_POINT('',(0.0721687836487032,0.,0.125));
#49570=CARTESIAN_POINT('',(0.146084391824352,0.,0.125));
#49571=CARTESIAN_POINT('',(0.0721687836487032,-0.25,0.125));
#49572=CARTESIAN_POINT('',(0.0721687836487032,0.,0.125));
#49573=CARTESIAN_POINT('',(-0.0721687836487033,-0.25,0.125));
#49574=CARTESIAN_POINT('Origin',(0.144337567297406,0.,0.));
#49575=CARTESIAN_POINT('',(0.153795371385231,0.,-0.0163813972081441));
#49576=CARTESIAN_POINT('',(0.0721687836487032,-0.25,0.125));
#49577=CARTESIAN_POINT('Origin',(0.,-0.25,0.));
#49578=CARTESIAN_POINT('Origin',(0.22,0.,0.));
#49579=CARTESIAN_POINT('',(-0.22,-8.67361737988404E-18,-2.69422295812418E-17));
#49580=CARTESIAN_POINT('Origin',(0.,0.,0.));
#49581=CARTESIAN_POINT('Origin',(0.,-0.015,0.));
#49582=CARTESIAN_POINT('',(-0.24505,-0.02505,-3.00099698131059E-17));
#49583=CARTESIAN_POINT('Origin',(0.,-0.02505,0.));
#49584=CARTESIAN_POINT('',(-0.235,-0.015,-2.87791997799628E-17));
#49585=CARTESIAN_POINT('Origin',(0.,-0.3775,0.));
#49586=CARTESIAN_POINT('',(-0.24505,-0.72995,3.00099698131059E-17));
#49587=CARTESIAN_POINT('Origin',(0.,-0.72995,0.));
#49588=CARTESIAN_POINT('',(-0.24505,-0.3775,-3.00099698131059E-17));
#49589=CARTESIAN_POINT('Origin',(0.,-0.7625,0.));
#49590=CARTESIAN_POINT('',(-0.175,-0.8,-2.14313189850787E-17));
#49591=CARTESIAN_POINT('Origin',(0.,-0.8,0.));
#49592=CARTESIAN_POINT('',(-0.2125,-0.7625,-2.60237444818813E-17));
#49593=CARTESIAN_POINT('Origin',(0.,-0.8,0.));
#49594=CARTESIAN_POINT('',(0.,0.,0.));
#49595=CARTESIAN_POINT('',(0.,0.,0.));
#49596=CARTESIAN_POINT('',(0.,0.,0.));
#49597=CARTESIAN_POINT('',(0.,0.,0.));
#49598=CARTESIAN_POINT('',(0.,0.,0.));
#49599=CARTESIAN_POINT('',(0.,0.,0.));
#49600=CARTESIAN_POINT('',(0.,0.,0.));
#49601=CARTESIAN_POINT('',(0.,-8.2,11.4));
#49602=CARTESIAN_POINT('',(0.,8.2,11.4));
#49603=CARTESIAN_POINT('',(0.,-2.,10.));
#49604=CARTESIAN_POINT('',(0.,-1.4,9.65));
#49605=CARTESIAN_POINT('',(0.,0.,0.));
#49606=CARTESIAN_POINT('Origin',(0.3,0.,0.));
#49607=CARTESIAN_POINT('',(0.3,2.2,-1.28));
#49608=CARTESIAN_POINT('',(0.3,2.2,-0.953939201416946));
#49609=CARTESIAN_POINT('',(0.3,2.2,0.));
#49610=CARTESIAN_POINT('',(0.3,-1.,-1.28));
#49611=CARTESIAN_POINT('',(0.3,0.,-1.28));
#49612=CARTESIAN_POINT('',(0.3,-1.,-0.953939201416946));
#49613=CARTESIAN_POINT('',(0.3,-1.,0.));
#49614=CARTESIAN_POINT('',(0.3,0.,-0.953939201416946));
#49615=CARTESIAN_POINT('Origin',(0.3,0.,-1.28));
#49616=CARTESIAN_POINT('',(-0.3,2.2,-1.28));
#49617=CARTESIAN_POINT('',(0.15,2.2,-1.28));
#49618=CARTESIAN_POINT('',(-0.3,-1.,-1.28));
#49619=CARTESIAN_POINT('',(-0.3,0.,-1.28));
#49620=CARTESIAN_POINT('',(0.15,-1.,-1.28));
#49621=CARTESIAN_POINT('Origin',(-0.3,0.,-1.28));
#49622=CARTESIAN_POINT('',(-0.3,2.2,-0.953939201416946));
#49623=CARTESIAN_POINT('',(-0.3,2.2,-0.64));
#49624=CARTESIAN_POINT('',(-0.3,-1.,-0.953939201416946));
#49625=CARTESIAN_POINT('',(-0.3,0.,-0.953939201416946));
#49626=CARTESIAN_POINT('',(-0.3,-1.,-0.64));
#49627=CARTESIAN_POINT('Origin',(0.,-1.,0.));
#49628=CARTESIAN_POINT('',(3.66661143271685,-1.,0.786422660831985));
#49629=CARTESIAN_POINT('',(3.62400312501245,-1.,0.963899035117249));
#49630=CARTESIAN_POINT('Origin',(0.,-1.,0.));
#49631=CARTESIAN_POINT('',(4.01728681790024,-1.,1.22531898815164));
#49632=CARTESIAN_POINT('Ctrl Pts',(3.62400312501245,-1.,0.963899035117249));
#49633=CARTESIAN_POINT('Ctrl Pts',(3.6240482887845,-1.,0.963880158555582));
#49634=CARTESIAN_POINT('Ctrl Pts',(3.62424461507588,-1.,0.963861297423241));
#49635=CARTESIAN_POINT('Ctrl Pts',(3.62489305727662,-1.,0.963957782642844));
#49636=CARTESIAN_POINT('Ctrl Pts',(3.62652618145335,-1.,0.964373850166458));
#49637=CARTESIAN_POINT('Ctrl Pts',(3.62988252139846,-1.,0.965395153165294));
#49638=CARTESIAN_POINT('Ctrl Pts',(3.63492122081143,-1.,0.967052554541386));
#49639=CARTESIAN_POINT('Ctrl Pts',(3.64113946505766,-1.,0.969195124675866));
#49640=CARTESIAN_POINT('Ctrl Pts',(3.64819756447455,-1.,0.971722122061341));
#49641=CARTESIAN_POINT('Ctrl Pts',(3.65571576735126,-1.,0.974519971354849));
#49642=CARTESIAN_POINT('Ctrl Pts',(3.66333049637475,-1.,0.977478312751618));
#49643=CARTESIAN_POINT('Ctrl Pts',(3.67074983340361,-1.,0.980505922458267));
#49644=CARTESIAN_POINT('Ctrl Pts',(3.67782408841715,-1.,0.98355079147042));
#49645=CARTESIAN_POINT('Ctrl Pts',(3.68455317926068,-1.,0.986602639863838));
#49646=CARTESIAN_POINT('Ctrl Pts',(3.69102682138846,-1.,0.989676715398559));
#49647=CARTESIAN_POINT('Ctrl Pts',(3.69738123415662,-1.,0.992802218332011));
#49648=CARTESIAN_POINT('Ctrl Pts',(3.70375282282138,-1.,0.996009819772518));
#49649=CARTESIAN_POINT('Ctrl Pts',(3.71022439713938,-1.,0.999317260756531));
#49650=CARTESIAN_POINT('Ctrl Pts',(3.71680667125118,-1.,1.00272423396822));
#49651=CARTESIAN_POINT('Ctrl Pts',(3.72346803750595,-1.,1.0062200073571));
#49652=CARTESIAN_POINT('Ctrl Pts',(3.73015276704426,-1.,1.00978798539496));
#49653=CARTESIAN_POINT('Ctrl Pts',(3.73680245055734,-1.,1.01341114319903));
#49654=CARTESIAN_POINT('Ctrl Pts',(3.74337942504959,-1.,1.01707794311079));
#49655=CARTESIAN_POINT('Ctrl Pts',(3.74987777155834,-1.,1.02078510487428));
#49656=CARTESIAN_POINT('Ctrl Pts',(3.75631037456194,-1.,1.0245342944466));
#49657=CARTESIAN_POINT('Ctrl Pts',(3.76270122291232,-1.,1.02833014458181));
#49658=CARTESIAN_POINT('Ctrl Pts',(3.76907609832522,-1.,1.0321778660492));
#49659=CARTESIAN_POINT('Ctrl Pts',(3.77545283140445,-1.,1.03608074678013));
#49660=CARTESIAN_POINT('Ctrl Pts',(3.78183535008192,-1.,1.04003862055804));
#49661=CARTESIAN_POINT('Ctrl Pts',(3.78821910787195,-1.,1.04404924374426));
#49662=CARTESIAN_POINT('Ctrl Pts',(3.79459440308793,-1.,1.04810913267641));
#49663=CARTESIAN_POINT('Ctrl Pts',(3.80095039790678,-1.,1.05221457990015));
#49664=CARTESIAN_POINT('Ctrl Pts',(3.80727913637784,-1.,1.05636266918643));
#49665=CARTESIAN_POINT('Ctrl Pts',(3.81357866117485,-1.,1.06055206187298));
#49666=CARTESIAN_POINT('Ctrl Pts',(3.81985083953012,-1.,1.06478244038931));
#49667=CARTESIAN_POINT('Ctrl Pts',(3.82609989967278,-1.,1.0690541318036));
#49668=CARTESIAN_POINT('Ctrl Pts',(3.83233071195145,-1.,1.0733676663346));
#49669=CARTESIAN_POINT('Ctrl Pts',(3.83854714117486,-1.,1.07772335353856));
#49670=CARTESIAN_POINT('Ctrl Pts',(3.84475048030615,-1.,1.08212087917986));
#49671=CARTESIAN_POINT('Ctrl Pts',(3.8509402522269,-1.,1.08655950846377));
#49672=CARTESIAN_POINT('Ctrl Pts',(3.85711487933911,-1.,1.09103825516288));
#49673=CARTESIAN_POINT('Ctrl Pts',(3.86327241021242,-1.,1.09555606505012));
#49674=CARTESIAN_POINT('Ctrl Pts',(3.86941120134872,-1.,1.10011198761203));
#49675=CARTESIAN_POINT('Ctrl Pts',(3.87553067187566,-1.,1.10470536603303));
#49676=CARTESIAN_POINT('Ctrl Pts',(3.88163105531791,-1.,1.10933577224029));
#49677=CARTESIAN_POINT('Ctrl Pts',(3.88771308285229,-1.,1.11400292434447));
#49678=CARTESIAN_POINT('Ctrl Pts',(3.89377768340362,-1.,1.11870660794609));
#49679=CARTESIAN_POINT('Ctrl Pts',(3.89982569749978,-1.,1.12344660099029));
#49680=CARTESIAN_POINT('Ctrl Pts',(3.90585753318622,-1.,1.12822258281518));
#49681=CARTESIAN_POINT('Ctrl Pts',(3.91187321145495,-1.,1.13303414693849));
#49682=CARTESIAN_POINT('Ctrl Pts',(3.91787251936688,-1.,1.13788084225511));
#49683=CARTESIAN_POINT('Ctrl Pts',(3.92385513133937,-1.,1.14276220561575));
#49684=CARTESIAN_POINT('Ctrl Pts',(3.92982073294334,-1.,1.14767779451147));
#49685=CARTESIAN_POINT('Ctrl Pts',(3.9357691705651,-1.,1.15262722716391));
#49686=CARTESIAN_POINT('Ctrl Pts',(3.94170046685542,-1.,1.15761018341061));
#49687=CARTESIAN_POINT('Ctrl Pts',(3.9476147478092,-1.,1.16262637999261));
#49688=CARTESIAN_POINT('Ctrl Pts',(3.95351219510062,-1.,1.16767555244495));
#49689=CARTESIAN_POINT('Ctrl Pts',(3.95939299213164,-1.,1.17275743590327));
#49690=CARTESIAN_POINT('Ctrl Pts',(3.96525726357682,-1.,1.17787174135446));
#49691=CARTESIAN_POINT('Ctrl Pts',(3.9711050516465,-1.,1.18301815039596));
#49692=CARTESIAN_POINT('Ctrl Pts',(3.97693634766926,-1.,1.18819633715285));
#49693=CARTESIAN_POINT('Ctrl Pts',(3.98275111052015,-1.,1.19340598349307));
#49694=CARTESIAN_POINT('Ctrl Pts',(3.98854928957287,-1.,1.19864679609596));
#49695=CARTESIAN_POINT('Ctrl Pts',(3.99433084800649,-1.,1.2039185237544));
#49696=CARTESIAN_POINT('Ctrl Pts',(4.00009577952534,-1.,1.20922097030107));
#49697=CARTESIAN_POINT('Ctrl Pts',(4.00584409524937,-1.,1.21455398918813));
#49698=CARTESIAN_POINT('Ctrl Pts',(4.01042947142681,-1.,1.21884478244983));
#49699=CARTESIAN_POINT('Ctrl Pts',(4.01386104434674,-1.,1.22207656456199));
#49700=CARTESIAN_POINT('Ctrl Pts',(4.0161454457032,-1.,1.22423716681447));
#49701=CARTESIAN_POINT('Ctrl Pts',(4.01728681790024,-1.,1.22531898815164));
#49702=CARTESIAN_POINT('',(3.97027773754922,-1.,1.36999806084573));
#49703=CARTESIAN_POINT('',(4.01728681790024,-1.,1.22531898815164));
#49704=CARTESIAN_POINT('',(3.4984457533445,-1.,1.35032489087101));
#49705=CARTESIAN_POINT('Ctrl Pts',(3.97027773754922,-1.,1.36999806084573));
#49706=CARTESIAN_POINT('Ctrl Pts',(3.9687184694131,-1.,1.37020239094614));
#49707=CARTESIAN_POINT('Ctrl Pts',(3.96560037974645,-1.,1.37060761745635));
#49708=CARTESIAN_POINT('Ctrl Pts',(3.96092458506535,-1.,1.3712051561502));
#49709=CARTESIAN_POINT('Ctrl Pts',(3.95469287280914,-1.,1.37198126432386));
#49710=CARTESIAN_POINT('Ctrl Pts',(3.94690771785133,-1.,1.37291699202807));
#49711=CARTESIAN_POINT('Ctrl Pts',(3.93912709040818,-1.,1.37381821967165));
#49712=CARTESIAN_POINT('Ctrl Pts',(3.93135106761844,-1.,1.37468482215751));
#49713=CARTESIAN_POINT('Ctrl Pts',(3.92357976987672,-1.,1.37551664448242));
#49714=CARTESIAN_POINT('Ctrl Pts',(3.91581337462644,-1.,1.37631350505797));
#49715=CARTESIAN_POINT('Ctrl Pts',(3.90805209523486,-1.,1.3770751963402));
#49716=CARTESIAN_POINT('Ctrl Pts',(3.90029615196727,-1.,1.37780148512792));
#49717=CARTESIAN_POINT('Ctrl Pts',(3.89254574338496,-1.,1.3784921128802));
#49718=CARTESIAN_POINT('Ctrl Pts',(3.88480102249277,-1.,1.37914679719383));
#49719=CARTESIAN_POINT('Ctrl Pts',(3.87706205830532,-1.,1.37976523097073));
#49720=CARTESIAN_POINT('Ctrl Pts',(3.86932885813068,-1.,1.38034709213014));
#49721=CARTESIAN_POINT('Ctrl Pts',(3.86160143043959,-1.,1.3808920599299));
#49722=CARTESIAN_POINT('Ctrl Pts',(3.85387983979481,-1.,1.3813998311505));
#49723=CARTESIAN_POINT('Ctrl Pts',(3.84616425605764,-1.,1.38187013346109));
#49724=CARTESIAN_POINT('Ctrl Pts',(3.83845502790746,-1.,1.38230274828822));
#49725=CARTESIAN_POINT('Ctrl Pts',(3.8307526698229,-1.,1.38269750245138));
#49726=CARTESIAN_POINT('Ctrl Pts',(3.82305771743829,-1.,1.38305421262763));
#49727=CARTESIAN_POINT('Ctrl Pts',(3.81537060817811,-1.,1.38337263902782));
#49728=CARTESIAN_POINT('Ctrl Pts',(3.80769156398411,-1.,1.3836524404622));
#49729=CARTESIAN_POINT('Ctrl Pts',(3.80002044322111,-1.,1.38389311766682));
#49730=CARTESIAN_POINT('Ctrl Pts',(3.79235669640841,-1.,1.38409399694566));
#49731=CARTESIAN_POINT('Ctrl Pts',(3.78469969805082,-1.,1.38425435883756));
#49732=CARTESIAN_POINT('Ctrl Pts',(3.77704902230418,-1.,1.38437354551428));
#49733=CARTESIAN_POINT('Ctrl Pts',(3.76940473185779,-1.,1.38445107339518));
#49734=CARTESIAN_POINT('Ctrl Pts',(3.76176768271367,-1.,1.3844867525335));
#49735=CARTESIAN_POINT('Ctrl Pts',(3.7541397631875,-1.,1.38448077997163));
#49736=CARTESIAN_POINT('Ctrl Pts',(3.74652317167876,-1.,1.38443344984394));
#49737=CARTESIAN_POINT('Ctrl Pts',(3.73891976418104,-1.,1.38434489156458));
#49738=CARTESIAN_POINT('Ctrl Pts',(3.73133035859282,-1.,1.38421479111531));
#49739=CARTESIAN_POINT('Ctrl Pts',(3.72375409358803,-1.,1.3840421342895));
#49740=CARTESIAN_POINT('Ctrl Pts',(3.7161876605181,-1.,1.38382489984586));
#49741=CARTESIAN_POINT('Ctrl Pts',(3.70862680753347,-1.,1.38356065402124));
#49742=CARTESIAN_POINT('Ctrl Pts',(3.701067921679,-1.,1.38324717612865));
#49743=CARTESIAN_POINT('Ctrl Pts',(3.69350967899526,-1.,1.38288311171651));
#49744=CARTESIAN_POINT('Ctrl Pts',(3.68595444983837,-1.,1.38246852827182));
#49745=CARTESIAN_POINT('Ctrl Pts',(3.67841038482414,-1.,1.3820057429062));
#49746=CARTESIAN_POINT('Ctrl Pts',(3.67088843112262,-1.,1.38149812653868));
#49747=CARTESIAN_POINT('Ctrl Pts',(3.66339848520857,-1.,1.38094856333552));
#49748=CARTESIAN_POINT('Ctrl Pts',(3.6559455440439,-1.,1.38035791051213));
#49749=CARTESIAN_POINT('Ctrl Pts',(3.64852652756456,-1.,1.37972372481603));
#49750=CARTESIAN_POINT('Ctrl Pts',(3.64112507791141,-1.,1.37903818567359));
#49751=CARTESIAN_POINT('Ctrl Pts',(3.63371727442486,-1.,1.37829035457339));
#49752=CARTESIAN_POINT('Ctrl Pts',(3.62628098665145,-1.,1.37746987919881));
#49753=CARTESIAN_POINT('Ctrl Pts',(3.6188048116042,-1.,1.37657053403107));
#49754=CARTESIAN_POINT('Ctrl Pts',(3.61129546591064,-1.,1.37559314436634));
#49755=CARTESIAN_POINT('Ctrl Pts',(3.60379020123988,-1.,1.37455051379623));
#49756=CARTESIAN_POINT('Ctrl Pts',(3.59634627869048,-1.,1.37346320103157));
#49757=CARTESIAN_POINT('Ctrl Pts',(3.58901853846365,-1.,1.37235053660976));
#49758=CARTESIAN_POINT('Ctrl Pts',(3.58183885982715,-1.,1.37122241663062));
#49759=CARTESIAN_POINT('Ctrl Pts',(3.57479875549486,-1.,1.37007229485659));
#49760=CARTESIAN_POINT('Ctrl Pts',(3.5678208030466,-1.,1.36886584973389));
#49761=CARTESIAN_POINT('Ctrl Pts',(3.56077662028649,-1.,1.36754771771233));
#49762=CARTESIAN_POINT('Ctrl Pts',(3.55353883995949,-1.,1.3660614545677));
#49763=CARTESIAN_POINT('Ctrl Pts',(3.54602591832973,-1.,1.36436666257598));
#49764=CARTESIAN_POINT('Ctrl Pts',(3.53824396424961,-1.,1.36245507339307));
#49765=CARTESIAN_POINT('Ctrl Pts',(3.530344649616,-1.,1.36037259643734));
#49766=CARTESIAN_POINT('Ctrl Pts',(3.52261776116748,-1.,1.35821701528836));
#49767=CARTESIAN_POINT('Ctrl Pts',(3.51542230699556,-1.,1.35611275237152));
#49768=CARTESIAN_POINT('Ctrl Pts',(3.50913227059999,-1.,1.35419113575956));
#49769=CARTESIAN_POINT('Ctrl Pts',(3.50408168106261,-1.,1.35257032843486));
#49770=CARTESIAN_POINT('Ctrl Pts',(3.5007660381649,-1.,1.35142377279517));
#49771=CARTESIAN_POINT('Ctrl Pts',(3.49920025459723,-1.,1.35080045218587));
#49772=CARTESIAN_POINT('Ctrl Pts',(3.49861894124827,-1.,1.35049736560527));
#49773=CARTESIAN_POINT('Ctrl Pts',(3.49847119623846,-1.,1.35036670892966));
#49774=CARTESIAN_POINT('Ctrl Pts',(3.4984457533445,-1.,1.35032489087101));
#49775=CARTESIAN_POINT('',(3.42859860294378,-1.,1.51895082866166));
#49776=CARTESIAN_POINT('Origin',(0.,-1.,0.));
#49777=CARTESIAN_POINT('',(3.77614523045147,-1.,1.83867539237861));
#49778=CARTESIAN_POINT('Ctrl Pts',(3.42859860294378,-1.,1.51895082866166));
#49779=CARTESIAN_POINT('Ctrl Pts',(3.42864616361967,-1.,1.51893924967231));
#49780=CARTESIAN_POINT('Ctrl Pts',(3.42884302333978,-1.,1.51895133295017));
#49781=CARTESIAN_POINT('Ctrl Pts',(3.42946838852728,-1.,1.51914806898539));
#49782=CARTESIAN_POINT('Ctrl Pts',(3.4310163189349,-1.,1.5198144909343));
#49783=CARTESIAN_POINT('Ctrl Pts',(3.43417156977749,-1.,1.52134826724227));
#49784=CARTESIAN_POINT('Ctrl Pts',(3.43888895974182,-1.,1.52377348950429));
#49785=CARTESIAN_POINT('Ctrl Pts',(3.44469547527,-1.,1.52686242875717));
#49786=CARTESIAN_POINT('Ctrl Pts',(3.45127136828667,-1.,1.530462444618));
#49787=CARTESIAN_POINT('Ctrl Pts',(3.45825932955273,-1.,1.53440195378902));
#49788=CARTESIAN_POINT('Ctrl Pts',(3.46531752207222,-1.,1.53851507915533));
#49789=CARTESIAN_POINT('Ctrl Pts',(3.47217189224576,-1.,1.54266605398152));
#49790=CARTESIAN_POINT('Ctrl Pts',(3.47868272898599,-1.,1.54678009290207));
#49791=CARTESIAN_POINT('Ctrl Pts',(3.48485155928414,-1.,1.55084702970382));
#49792=CARTESIAN_POINT('Ctrl Pts',(3.49076460877317,-1.,1.5548959590107));
#49793=CARTESIAN_POINT('Ctrl Pts',(3.49655185179623,-1.,1.55897703097859));
#49794=CARTESIAN_POINT('Ctrl Pts',(3.50234321621607,-1.,1.56314187758689));
#49795=CARTESIAN_POINT('Ctrl Pts',(3.50821771695427,-1.,1.56742097575041));
#49796=CARTESIAN_POINT('Ctrl Pts',(3.51418598431733,-1.,1.57181569799774));
#49797=CARTESIAN_POINT('Ctrl Pts',(3.52021847865961,-1.,1.5763104998818));
#49798=CARTESIAN_POINT('Ctrl Pts',(3.52626275334899,-1.,1.58088027227856));
#49799=CARTESIAN_POINT('Ctrl Pts',(3.53226378147068,-1.,1.58549906268083));
#49800=CARTESIAN_POINT('Ctrl Pts',(3.53818616861045,-1.,1.59014958368725));
#49801=CARTESIAN_POINT('Ctrl Pts',(3.544024581823,-1.,1.5948276694975));
#49802=CARTESIAN_POINT('Ctrl Pts',(3.54979148634426,-1.,1.59953698113444));
#49803=CARTESIAN_POINT('Ctrl Pts',(3.55550985096117,-1.,1.60428584699848));
#49804=CARTESIAN_POINT('Ctrl Pts',(3.56120432482986,-1.,1.60908344685459));
#49805=CARTESIAN_POINT('Ctrl Pts',(3.56689200468404,-1.,1.61393581747522));
#49806=CARTESIAN_POINT('Ctrl Pts',(3.57257679609826,-1.,1.61884340915412));
#49807=CARTESIAN_POINT('Ctrl Pts',(3.57825455954405,-1.,1.62380329464851));
#49808=CARTESIAN_POINT('Ctrl Pts',(3.5839162577435,-1.,1.62881051550748));
#49809=CARTESIAN_POINT('Ctrl Pts',(3.58955176627876,-1.,1.63385971451259));
#49810=CARTESIAN_POINT('Ctrl Pts',(3.59515368334887,-1.,1.63894676675349));
#49811=CARTESIAN_POINT('Ctrl Pts',(3.6007202851384,-1.,1.6440700438558));
#49812=CARTESIAN_POINT('Ctrl Pts',(3.60625346556992,-1.,1.64922952425833));
#49813=CARTESIAN_POINT('Ctrl Pts',(3.61175734965129,-1.,1.65442619244327));
#49814=CARTESIAN_POINT('Ctrl Pts',(3.61723666482457,-1.,1.65966133399186));
#49815=CARTESIAN_POINT('Ctrl Pts',(3.62269517989104,-1.,1.66493585923853));
#49816=CARTESIAN_POINT('Ctrl Pts',(3.62813422105257,-1.,1.67024966008037));
#49817=CARTESIAN_POINT('Ctrl Pts',(3.63355343201211,-1.,1.67560193613145));
#49818=CARTESIAN_POINT('Ctrl Pts',(3.63895140887443,-1.,1.68099146651577));
#49819=CARTESIAN_POINT('Ctrl Pts',(3.64432638915199,-1.,1.68641690471455));
#49820=CARTESIAN_POINT('Ctrl Pts',(3.64967689827393,-1.,1.691877054817));
#49821=CARTESIAN_POINT('Ctrl Pts',(3.65500246526798,-1.,1.69737117722559));
#49822=CARTESIAN_POINT('Ctrl Pts',(3.6603033877491,-1.,1.70289888566904));
#49823=CARTESIAN_POINT('Ctrl Pts',(3.6655804319893,-1.,1.70846001610983));
#49824=CARTESIAN_POINT('Ctrl Pts',(3.67083454901629,-1.,1.71405450210392));
#49825=CARTESIAN_POINT('Ctrl Pts',(3.67606660374665,-1.,1.71968225581787));
#49826=CARTESIAN_POINT('Ctrl Pts',(3.68127704936472,-1.,1.72534302437003));
#49827=CARTESIAN_POINT('Ctrl Pts',(3.68646597019188,-1.,1.73103640956647));
#49828=CARTESIAN_POINT('Ctrl Pts',(3.69163322647906,-1.,1.73676193254493));
#49829=CARTESIAN_POINT('Ctrl Pts',(3.6967785691046,-1.,1.74251908492589));
#49830=CARTESIAN_POINT('Ctrl Pts',(3.70190175673422,-1.,1.74830738046092));
#49831=CARTESIAN_POINT('Ctrl Pts',(3.70700269736876,-1.,1.75412641804148));
#49832=CARTESIAN_POINT('Ctrl Pts',(3.71208146346454,-1.,1.75997588499021));
#49833=CARTESIAN_POINT('Ctrl Pts',(3.71713822377675,-1.,1.76585552124549));
#49834=CARTESIAN_POINT('Ctrl Pts',(3.72217319911429,-1.,1.77176509401846));
#49835=CARTESIAN_POINT('Ctrl Pts',(3.72718661205504,-1.,1.77770437039606));
#49836=CARTESIAN_POINT('Ctrl Pts',(3.73217863095022,-1.,1.78367308442682));
#49837=CARTESIAN_POINT('Ctrl Pts',(3.73714934729962,-1.,1.78967092823139));
#49838=CARTESIAN_POINT('Ctrl Pts',(3.74209880351667,-1.,1.79569757859041));
#49839=CARTESIAN_POINT('Ctrl Pts',(3.74702700874954,-1.,1.80175271485519));
#49840=CARTESIAN_POINT('Ctrl Pts',(3.75193395888069,-1.,1.80783603939662));
#49841=CARTESIAN_POINT('Ctrl Pts',(3.75681965683995,-1.,1.81394729834032));
#49842=CARTESIAN_POINT('Ctrl Pts',(3.76168412709652,-1.,1.82008629694924));
#49843=CARTESIAN_POINT('Ctrl Pts',(3.76652740355856,-1.,1.82625289221933));
#49844=CARTESIAN_POINT('Ctrl Pts',(3.77038509819777,-1.,1.83120816956515));
#49845=CARTESIAN_POINT('Ctrl Pts',(3.77326886065484,-1.,1.83493697935064));
#49846=CARTESIAN_POINT('Ctrl Pts',(3.77518714458232,-1.,1.83742834010821));
#49847=CARTESIAN_POINT('Ctrl Pts',(3.77614523045147,-1.,1.83867539237861));
#49848=CARTESIAN_POINT('',(3.70708211654725,-1.,1.97421938526992));
#49849=CARTESIAN_POINT('',(3.77614523045147,-1.,1.83867539237861));
#49850=CARTESIAN_POINT('',(3.24413672884902,-1.,1.88097764062542));
#49851=CARTESIAN_POINT('Ctrl Pts',(3.70708211654725,-1.,1.97421938526992));
#49852=CARTESIAN_POINT('Ctrl Pts',(3.7055100813194,-1.,1.974177276451));
#49853=CARTESIAN_POINT('Ctrl Pts',(3.70236698911837,-1.,1.97408973726149));
#49854=CARTESIAN_POINT('Ctrl Pts',(3.69765528558292,-1.,1.97394846382289));
#49855=CARTESIAN_POINT('Ctrl Pts',(3.69137888597855,-1.,1.97374016224397));
#49856=CARTESIAN_POINT('Ctrl Pts',(3.68354319913416,-1.,1.97344650303631));
#49857=CARTESIAN_POINT('Ctrl Pts',(3.67571738106175,-1.,1.97311947678035));
#49858=CARTESIAN_POINT('Ctrl Pts',(3.66790152751984,-1.,1.9727589719863));
#49859=CARTESIAN_POINT('Ctrl Pts',(3.66009578166865,-1.,1.97236485439317));
#49860=CARTESIAN_POINT('Ctrl Pts',(3.65230034717364,-1.,1.97193697240645));
#49861=CARTESIAN_POINT('Ctrl Pts',(3.64451546724221,-1.,1.97147515441539));
#49862=CARTESIAN_POINT('Ctrl Pts',(3.63674139590853,-1.,1.97097920454698));
#49863=CARTESIAN_POINT('Ctrl Pts',(3.62897836973397,-1.,1.97044889850518));
#49864=CARTESIAN_POINT('Ctrl Pts',(3.62122658401722,-1.,1.96988398129888));
#49865=CARTESIAN_POINT('Ctrl Pts',(3.61348615496393,-1.,1.96928416040712));
#49866=CARTESIAN_POINT('Ctrl Pts',(3.60575714017676,-1.,1.96864911885775));
#49867=CARTESIAN_POINT('Ctrl Pts',(3.59803959819725,-1.,1.96797854118257));
#49868=CARTESIAN_POINT('Ctrl Pts',(3.5903336402273,-1.,1.96727213799507));
#49869=CARTESIAN_POINT('Ctrl Pts',(3.58263947663884,-1.,1.9665296668894));
#49870=CARTESIAN_POINT('Ctrl Pts',(3.57495748601088,-1.,1.96575096652857));
#49871=CARTESIAN_POINT('Ctrl Pts',(3.56728820357933,-1.,1.96493594634643));
#49872=CARTESIAN_POINT('Ctrl Pts',(3.55963218706201,-1.,1.96408450906868));
#49873=CARTESIAN_POINT('Ctrl Pts',(3.55198990600929,-1.,1.96319648628667));
#49874=CARTESIAN_POINT('Ctrl Pts',(3.54436163300425,-1.,1.96227157573058));
#49875=CARTESIAN_POINT('Ctrl Pts',(3.53674730625759,-1.,1.96130926212661));
#49876=CARTESIAN_POINT('Ctrl Pts',(3.52914648844289,-1.,1.96030879411534));
#49877=CARTESIAN_POINT('Ctrl Pts',(3.52155867431438,-1.,1.95926936324436));
#49878=CARTESIAN_POINT('Ctrl Pts',(3.51398354617772,-1.,1.95819025316768));
#49879=CARTESIAN_POINT('Ctrl Pts',(3.50642124159913,-1.,1.95707099606514));
#49880=CARTESIAN_POINT('Ctrl Pts',(3.49887263575602,-1.,1.9559115382367));
#49881=CARTESIAN_POINT('Ctrl Pts',(3.49133956289154,-1.,1.95471236969653));
#49882=CARTESIAN_POINT('Ctrl Pts',(3.48382414832648,-1.,1.95347412486316));
#49883=CARTESIAN_POINT('Ctrl Pts',(3.47632820495926,-1.,1.95219722189878));
#49884=CARTESIAN_POINT('Ctrl Pts',(3.4688525897419,-1.,1.95088147859876));
#49885=CARTESIAN_POINT('Ctrl Pts',(3.46139661060959,-1.,1.94952575850196));
#49886=CARTESIAN_POINT('Ctrl Pts',(3.45395731584051,-1.,1.94812754766524));
#49887=CARTESIAN_POINT('Ctrl Pts',(3.44653088665685,-1.,1.94668377715332));
#49888=CARTESIAN_POINT('Ctrl Pts',(3.43911410197693,-1.,1.94519168842883));
#49889=CARTESIAN_POINT('Ctrl Pts',(3.43170586602436,-1.,1.94364973660285));
#49890=CARTESIAN_POINT('Ctrl Pts',(3.42430850941497,-1.,1.94205835913692));
#49891=CARTESIAN_POINT('Ctrl Pts',(3.41692971994082,-1.,1.94042111965237));
#49892=CARTESIAN_POINT('Ctrl Pts',(3.40957978266622,-1.,1.93874306008132));
#49893=CARTESIAN_POINT('Ctrl Pts',(3.40226802104093,-1.,1.93702857723089));
#49894=CARTESIAN_POINT('Ctrl Pts',(3.39499923640789,-1.,1.93527929945982));
#49895=CARTESIAN_POINT('Ctrl Pts',(3.38777076883267,-1.,1.93349233176794));
#49896=CARTESIAN_POINT('Ctrl Pts',(3.38056768525577,-1.,1.93165739093292));
#49897=CARTESIAN_POINT('Ctrl Pts',(3.37336807068078,-1.,1.92975993109897));
#49898=CARTESIAN_POINT('Ctrl Pts',(3.36615168657597,-1.,1.92778626543803));
#49899=CARTESIAN_POINT('Ctrl Pts',(3.35890824422976,-1.,1.92572846125763));
#49900=CARTESIAN_POINT('Ctrl Pts',(3.35164424847206,-1.,1.92358838440518));
#49901=CARTESIAN_POINT('Ctrl Pts',(3.34439448941915,-1.,1.92138450828378));
#49902=CARTESIAN_POINT('Ctrl Pts',(3.33721230709948,-1.,1.91914609610173));
#49903=CARTESIAN_POINT('Ctrl Pts',(3.33014884257812,-1.,1.91690081930297));
#49904=CARTESIAN_POINT('Ctrl Pts',(3.32323403454507,-1.,1.91466343916612));
#49905=CARTESIAN_POINT('Ctrl Pts',(3.31646052426395,-1.,1.91242616234459));
#49906=CARTESIAN_POINT('Ctrl Pts',(3.30975721158694,-1.,1.91014297830502));
#49907=CARTESIAN_POINT('Ctrl Pts',(3.30300595568341,-1.,1.90773912171424));
#49908=CARTESIAN_POINT('Ctrl Pts',(3.29608978722258,-1.,1.9051389186417));
#49909=CARTESIAN_POINT('Ctrl Pts',(3.28893448600364,-1.,1.9022897124757));
#49910=CARTESIAN_POINT('Ctrl Pts',(3.28154737912287,-1.,1.89918429230425));
#49911=CARTESIAN_POINT('Ctrl Pts',(3.27407108932908,-1.,1.89589172903662));
#49912=CARTESIAN_POINT('Ctrl Pts',(3.2667765388833,-1.,1.89255393500769));
#49913=CARTESIAN_POINT('Ctrl Pts',(3.2599988519361,-1.,1.88934996203508));
#49914=CARTESIAN_POINT('Ctrl Pts',(3.25408686339298,-1.,1.88646802523372));
#49915=CARTESIAN_POINT('Ctrl Pts',(3.24935200512055,-1.,1.88407708646435));
#49916=CARTESIAN_POINT('Ctrl Pts',(3.24625654410705,-1.,1.88242596600422));
#49917=CARTESIAN_POINT('Ctrl Pts',(3.24480754675942,-1.,1.88156537699118));
#49918=CARTESIAN_POINT('Ctrl Pts',(3.24428080352952,-1.,1.88117508446657));
#49919=CARTESIAN_POINT('Ctrl Pts',(3.2441553167131,-1.,1.88102292397987));
#49920=CARTESIAN_POINT('Ctrl Pts',(3.24413672884902,-1.,1.88097764062542));
#49921=CARTESIAN_POINT('',(3.14877060440425,-1.,2.03660101169564));
#49922=CARTESIAN_POINT('Origin',(0.,-1.,0.));
#49923=CARTESIAN_POINT('',(3.44202241512147,-1.,2.40675750623143));
#49924=CARTESIAN_POINT('Ctrl Pts',(3.14877060440425,-1.,2.03660101169564));
#49925=CARTESIAN_POINT('Ctrl Pts',(3.1488193908823,-1.,2.03659701539175));
#49926=CARTESIAN_POINT('Ctrl Pts',(3.14901193669147,-1.,2.03663974554941));
#49927=CARTESIAN_POINT('Ctrl Pts',(3.14959882629936,-1.,2.03693188810614));
#49928=CARTESIAN_POINT('Ctrl Pts',(3.15102344775396,-1.,2.03783225496023));
#49929=CARTESIAN_POINT('Ctrl Pts',(3.1538999167466,-1.,2.03984073791432));
#49930=CARTESIAN_POINT('Ctrl Pts',(3.15817983946525,-1.,2.04297406404132));
#49931=CARTESIAN_POINT('Ctrl Pts',(3.16343165059235,-1.,2.0469333124766));
#49932=CARTESIAN_POINT('Ctrl Pts',(3.16936341689859,-1.,2.05151770247452));
#49933=CARTESIAN_POINT('Ctrl Pts',(3.17564906975592,-1.,2.05650186773279));
#49934=CARTESIAN_POINT('Ctrl Pts',(3.18197692964677,-1.,2.06166849827143));
#49935=CARTESIAN_POINT('Ctrl Pts',(3.18809755562297,-1.,2.06684062744065));
#49936=CARTESIAN_POINT('Ctrl Pts',(3.19388465568113,-1.,2.07192253497765));
#49937=CARTESIAN_POINT('Ctrl Pts',(3.19934132835879,-1.,2.0769044187063));
#49938=CARTESIAN_POINT('Ctrl Pts',(3.20454818630635,-1.,2.08182850370816));
#49939=CARTESIAN_POINT('Ctrl Pts',(3.20962575845433,-1.,2.08676465517435));
#49940=CARTESIAN_POINT('Ctrl Pts',(3.2146942960168,-1.,2.0917841946046));
#49941=CARTESIAN_POINT('Ctrl Pts',(3.21982707347067,-1.,2.09692958434933));
#49942=CARTESIAN_POINT('Ctrl Pts',(3.22503437553496,-1.,2.10220384298534));
#49943=CARTESIAN_POINT('Ctrl Pts',(3.23028945793334,-1.,2.1075869964248));
#49944=CARTESIAN_POINT('Ctrl Pts',(3.23554444767115,-1.,2.11304604021784));
#49945=CARTESIAN_POINT('Ctrl Pts',(3.24074905517282,-1.,2.11854673326972));
#49946=CARTESIAN_POINT('Ctrl Pts',(3.24587102613347,-1.,2.12406646410943));
#49947=CARTESIAN_POINT('Ctrl Pts',(3.25090574493994,-1.,2.1296002839681));
#49948=CARTESIAN_POINT('Ctrl Pts',(3.25586495065027,-1.,2.13515375878786));
#49949=CARTESIAN_POINT('Ctrl Pts',(3.26077002641868,-1.,2.14073870754258));
#49950=CARTESIAN_POINT('Ctrl Pts',(3.26564388189764,-1.,2.14636805295663));
#49951=CARTESIAN_POINT('Ctrl Pts',(3.27050245897244,-1.,2.15205043199818));
#49952=CARTESIAN_POINT('Ctrl Pts',(3.27534954469206,-1.,2.15778690038359));
#49953=CARTESIAN_POINT('Ctrl Pts',(3.28018150841414,-1.,2.16357391934434));
#49954=CARTESIAN_POINT('Ctrl Pts',(3.2849901997973,-1.,2.16940517773459));
#49955=CARTESIAN_POINT('Ctrl Pts',(3.28976645712566,-1.,2.17527380048422));
#49956=CARTESIAN_POINT('Ctrl Pts',(3.29450361500484,-1.,2.18117455557062));
#49957=CARTESIAN_POINT('Ctrl Pts',(3.29920022557635,-1.,2.18710556500325));
#49958=CARTESIAN_POINT('Ctrl Pts',(3.30385816281831,-1.,2.19306710376112));
#49959=CARTESIAN_POINT('Ctrl Pts',(3.30848134694596,-1.,2.19906078949925));
#49960=CARTESIAN_POINT('Ctrl Pts',(3.3130742460895,-1.,2.20508863150608));
#49961=CARTESIAN_POINT('Ctrl Pts',(3.31764044024231,-1.,2.21115211847872));
#49962=CARTESIAN_POINT('Ctrl Pts',(3.32218125618955,-1.,2.21725135110889));
#49963=CARTESIAN_POINT('Ctrl Pts',(3.32669646722871,-1.,2.22338548312759));
#49964=CARTESIAN_POINT('Ctrl Pts',(3.33118487773593,-1.,2.22955308907221));
#49965=CARTESIAN_POINT('Ctrl Pts',(3.33564495756478,-1.,2.2357525632881));
#49966=CARTESIAN_POINT('Ctrl Pts',(3.34007543738044,-1.,2.24198249391437));
#49967=CARTESIAN_POINT('Ctrl Pts',(3.34447596770768,-1.,2.24824207678288));
#49968=CARTESIAN_POINT('Ctrl Pts',(3.34884690292342,-1.,2.25453097693524));
#49969=CARTESIAN_POINT('Ctrl Pts',(3.35318902552676,-1.,2.26084915222484));
#49970=CARTESIAN_POINT('Ctrl Pts',(3.35750328523077,-1.,2.26719668579921));
#49971=CARTESIAN_POINT('Ctrl Pts',(3.36179055004369,-1.,2.27357362620902));
#49972=CARTESIAN_POINT('Ctrl Pts',(3.36605130712978,-1.,2.27997979457968));
#49973=CARTESIAN_POINT('Ctrl Pts',(3.37028570206357,-1.,2.28641481081045));
#49974=CARTESIAN_POINT('Ctrl Pts',(3.37449367172707,-1.,2.2928781800731));
#49975=CARTESIAN_POINT('Ctrl Pts',(3.37867504959382,-1.,2.29936936127588));
#49976=CARTESIAN_POINT('Ctrl Pts',(3.38282967336676,-1.,2.30588783640389));
#49977=CARTESIAN_POINT('Ctrl Pts',(3.38695751492659,-1.,2.31243319489505));
#49978=CARTESIAN_POINT('Ctrl Pts',(3.39105869475112,-1.,2.31900513925627));
#49979=CARTESIAN_POINT('Ctrl Pts',(3.39513342020045,-1.,2.32560343902683));
#49980=CARTESIAN_POINT('Ctrl Pts',(3.39918194578115,-1.,2.33222789882601));
#49981=CARTESIAN_POINT('Ctrl Pts',(3.40320452776646,-1.,2.33887832342715));
#49982=CARTESIAN_POINT('Ctrl Pts',(3.40720137403888,-1.,2.34555447648901));
#49983=CARTESIAN_POINT('Ctrl Pts',(3.41117262313464,-1.,2.35225606823649));
#49984=CARTESIAN_POINT('Ctrl Pts',(3.4151183675076,-1.,2.35898278606449));
#49985=CARTESIAN_POINT('Ctrl Pts',(3.41903866635384,-1.,2.36573431470314));
#49986=CARTESIAN_POINT('Ctrl Pts',(3.42293356216595,-1.,2.37251035954351));
#49987=CARTESIAN_POINT('Ctrl Pts',(3.42680309755241,-1.,2.37931067029517));
#49988=CARTESIAN_POINT('Ctrl Pts',(3.43064732714472,-1.,2.38613505844641));
#49989=CARTESIAN_POINT('Ctrl Pts',(3.43446630680436,-1.,2.39298338805823));
#49990=CARTESIAN_POINT('Ctrl Pts',(3.43750133066036,-1.,2.39848113411429));
#49991=CARTESIAN_POINT('Ctrl Pts',(3.43976627485223,-1.,2.40261515590099));
#49992=CARTESIAN_POINT('Ctrl Pts',(3.44127120683402,-1.,2.40537592959345));
#49993=CARTESIAN_POINT('Ctrl Pts',(3.44202241512147,-1.,2.40675750623143));
#49994=CARTESIAN_POINT('',(3.35260583073571,-1.,2.52982887637028));
#49995=CARTESIAN_POINT('',(3.44202241512147,-1.,2.40675750623143));
#49996=CARTESIAN_POINT('',(2.90994629141676,-1.,2.36531447826074));
#49997=CARTESIAN_POINT('Ctrl Pts',(3.35260583073571,-1.,2.52982887637028));
#49998=CARTESIAN_POINT('Ctrl Pts',(3.35105973714071,-1.,2.5295413654909));
#49999=CARTESIAN_POINT('Ctrl Pts',(3.34796903576663,-1.,2.52896321610703));
#50000=CARTESIAN_POINT('Ctrl Pts',(3.34333744115511,-1.,2.52808660915689));
#50001=CARTESIAN_POINT('Ctrl Pts',(3.33717089999103,-1.,2.52689902690158));
#50002=CARTESIAN_POINT('Ctrl Pts',(3.32947762187533,-1.,2.52538321164634));
#50003=CARTESIAN_POINT('Ctrl Pts',(3.32179931078699,-1.,2.5238359839626));
#50004=CARTESIAN_POINT('Ctrl Pts',(3.31413607874645,-1.,2.52225724871313));
#50005=CARTESIAN_POINT('Ctrl Pts',(3.30648808815442,-1.,2.52064689568511));
#50006=CARTESIAN_POINT('Ctrl Pts',(3.29885556388352,-1.,2.51900480701069));
#50007=CARTESIAN_POINT('Ctrl Pts',(3.2912387729927,-1.,2.51733085123797));
#50008=CARTESIAN_POINT('Ctrl Pts',(3.28363799702982,-1.,2.51562487464514));
#50009=CARTESIAN_POINT('Ctrl Pts',(3.27605350473142,-1.,2.513886692704));
#50010=CARTESIAN_POINT('Ctrl Pts',(3.26848552888115,-1.,2.51211608411423));
#50011=CARTESIAN_POINT('Ctrl Pts',(3.26093423001434,-1.,2.51031277813486));
#50012=CARTESIAN_POINT('Ctrl Pts',(3.25339971460982,-1.,2.50847647070723));
#50013=CARTESIAN_POINT('Ctrl Pts',(3.24588208983849,-1.,2.506606859405));
#50014=CARTESIAN_POINT('Ctrl Pts',(3.23838151080319,-1.,2.5047036758003));
#50015=CARTESIAN_POINT('Ctrl Pts',(3.23089822320646,-1.,2.50276671338111));
#50016=CARTESIAN_POINT('Ctrl Pts',(3.22343262620503,-1.,2.50079587201958));
#50017=CARTESIAN_POINT('Ctrl Pts',(3.21598526261286,-1.,2.4987911459939));
#50018=CARTESIAN_POINT('Ctrl Pts',(3.20855669849836,-1.,2.4967525264737));
#50019=CARTESIAN_POINT('Ctrl Pts',(3.20114742397588,-1.,2.49467992057755));
#50020=CARTESIAN_POINT('Ctrl Pts',(3.19375775555798,-1.,2.49257307239848));
#50021=CARTESIAN_POINT('Ctrl Pts',(3.18638771282266,-1.,2.49043146334059));
#50022=CARTESIAN_POINT('Ctrl Pts',(3.17903698136622,-1.,2.48825428288201));
#50023=CARTESIAN_POINT('Ctrl Pts',(3.17170518863313,-1.,2.48604065348587));
#50024=CARTESIAN_POINT('Ctrl Pts',(3.16439213290161,-1.,2.48378981792725));
#50025=CARTESIAN_POINT('Ctrl Pts',(3.15709802322739,-1.,2.48150133566571));
#50026=CARTESIAN_POINT('Ctrl Pts',(3.14982373241352,-1.,2.47917529057029));
#50027=CARTESIAN_POINT('Ctrl Pts',(3.1425709954655,-1.,2.47681245356109));
#50028=CARTESIAN_POINT('Ctrl Pts',(3.13534181229295,-1.,2.47441378371932));
#50029=CARTESIAN_POINT('Ctrl Pts',(3.12813790805952,-1.,2.47197997765871));
#50030=CARTESIAN_POINT('Ctrl Pts',(3.12096015766983,-1.,2.46951098947469));
#50031=CARTESIAN_POINT('Ctrl Pts',(3.11380805536122,-1.,2.46700558843506));
#50032=CARTESIAN_POINT('Ctrl Pts',(3.1066790790198,-1.,2.46446082979646));
#50033=CARTESIAN_POINT('Ctrl Pts',(3.09956993697052,-1.,2.46187308501884));
#50034=CARTESIAN_POINT('Ctrl Pts',(3.09247787931887,-1.,2.4592391256388));
#50035=CARTESIAN_POINT('Ctrl Pts',(3.08540206545315,-1.,2.45655725437039));
#50036=CARTESIAN_POINT('Ctrl Pts',(3.07834472886139,-1.,2.4538282678779));
#50037=CARTESIAN_POINT('Ctrl Pts',(3.07131290521297,-1.,2.45105688854422));
#50038=CARTESIAN_POINT('Ctrl Pts',(3.06431596421405,-1.,2.44824970516544));
#50039=CARTESIAN_POINT('Ctrl Pts',(3.05736242671506,-1.,2.44541251892556));
#50040=CARTESIAN_POINT('Ctrl Pts',(3.05045678021504,-1.,2.44254768923105));
#50041=CARTESIAN_POINT('Ctrl Pts',(3.04359685040555,-1.,2.43965194061857));
#50042=CARTESIAN_POINT('Ctrl Pts',(3.03676949672821,-1.,2.43671278042414));
#50043=CARTESIAN_POINT('Ctrl Pts',(3.02995534946978,-1.,2.43371241361488));
#50044=CARTESIAN_POINT('Ctrl Pts',(3.02313656036004,-1.,2.43063415586637));
#50045=CARTESIAN_POINT('Ctrl Pts',(3.01630420830504,-1.,2.42746856264168));
#50046=CARTESIAN_POINT('Ctrl Pts',(3.00946442616658,-1.,2.42421849439613));
#50047=CARTESIAN_POINT('Ctrl Pts',(3.00264868585996,-1.,2.42090763946779));
#50048=CARTESIAN_POINT('Ctrl Pts',(2.99590509293503,-1.,2.41757324500514));
#50049=CARTESIAN_POINT('Ctrl Pts',(2.98927983005796,-1.,2.41425064199586));
#50050=CARTESIAN_POINT('Ctrl Pts',(2.98280015815107,-1.,2.41095909342571));
#50051=CARTESIAN_POINT('Ctrl Pts',(2.97646002822422,-1.,2.40768975073713));
#50052=CARTESIAN_POINT('Ctrl Pts',(2.9701964131236,-1.,2.40438604734919));
#50053=CARTESIAN_POINT('Ctrl Pts',(2.96390432240312,-1.,2.4009556571164));
#50054=CARTESIAN_POINT('Ctrl Pts',(2.95748006482942,-1.,2.39730553974517));
#50055=CARTESIAN_POINT('Ctrl Pts',(2.95085857128439,-1.,2.39337207631667));
#50056=CARTESIAN_POINT('Ctrl Pts',(2.94404820669076,-1.,2.38914929090759));
#50057=CARTESIAN_POINT('Ctrl Pts',(2.93717903280391,-1.,2.38472771516311));
#50058=CARTESIAN_POINT('Ctrl Pts',(2.93049643640206,-1.,2.38028989582073));
#50059=CARTESIAN_POINT('Ctrl Pts',(2.92430340582608,-1.,2.3760651052403));
#50060=CARTESIAN_POINT('Ctrl Pts',(2.91891503791411,-1.,2.37229381109821));
#50061=CARTESIAN_POINT('Ctrl Pts',(2.9146124988314,-1.,2.36919161373173));
#50062=CARTESIAN_POINT('Ctrl Pts',(2.91181344022548,-1.,2.36707658451664));
#50063=CARTESIAN_POINT('Ctrl Pts',(2.91051690822156,-1.,2.36599991765749));
#50064=CARTESIAN_POINT('Ctrl Pts',(2.91005770527719,-1.,2.36553202948613));
#50065=CARTESIAN_POINT('Ctrl Pts',(2.90995756655606,-1.,2.36536211188453));
#50066=CARTESIAN_POINT('Ctrl Pts',(2.90994629141676,-1.,2.36531447826074));
#50067=CARTESIAN_POINT('',(2.79140942341378,-1.,2.50410331873042));
#50068=CARTESIAN_POINT('Origin',(0.,-1.,0.));
#50069=CARTESIAN_POINT('',(3.02314558451372,-1.,2.91557726271063));
#50070=CARTESIAN_POINT('Ctrl Pts',(2.79140942341378,-1.,2.50410331873043));
#50071=CARTESIAN_POINT('Ctrl Pts',(2.79145823440899,-1.,2.50410700351427));
#50072=CARTESIAN_POINT('Ctrl Pts',(2.79164172519039,-1.,2.50417932839343));
#50073=CARTESIAN_POINT('Ctrl Pts',(2.79217568804874,-1.,2.50455968395235));
#50074=CARTESIAN_POINT('Ctrl Pts',(2.79344192164204,-1.,2.50567182569153));
#50075=CARTESIAN_POINT('Ctrl Pts',(2.7959687805717,-1.,2.50810555977564));
#50076=CARTESIAN_POINT('Ctrl Pts',(2.79970585014308,-1.,2.51186983687947));
#50077=CARTESIAN_POINT('Ctrl Pts',(2.80427363984939,-1.,2.51660190466067));
#50078=CARTESIAN_POINT('Ctrl Pts',(2.80941521967234,-1.,2.52205778589922));
#50079=CARTESIAN_POINT('Ctrl Pts',(2.8148437904867,-1.,2.52796388055457));
#50080=CARTESIAN_POINT('Ctrl Pts',(2.82028550483744,-1.,2.53405679667463));
#50081=CARTESIAN_POINT('Ctrl Pts',(2.82552167649157,-1.,2.54012272520141));
#50082=CARTESIAN_POINT('Ctrl Pts',(2.83044254225794,-1.,2.54604736792542));
#50083=CARTESIAN_POINT('Ctrl Pts',(2.83505269592412,-1.,2.55182152806964));
#50084=CARTESIAN_POINT('Ctrl Pts',(2.83942515220699,-1.,2.55749952145165));
#50085=CARTESIAN_POINT('Ctrl Pts',(2.84366802680211,-1.,2.56316920798489));
#50086=CARTESIAN_POINT('Ctrl Pts',(2.84788893329091,-1.,2.56891984251743));
#50087=CARTESIAN_POINT('Ctrl Pts',(2.85215360144482,-1.,2.57480482727128));
#50088=CARTESIAN_POINT('Ctrl Pts',(2.85647171715147,-1.,2.58082875254407));
#50089=CARTESIAN_POINT('Ctrl Pts',(2.86081999003668,-1.,2.5869677064356));
#50090=CARTESIAN_POINT('Ctrl Pts',(2.86515629953528,-1.,2.59318160184921));
#50091=CARTESIAN_POINT('Ctrl Pts',(2.86943633170712,-1.,2.59942875223202));
#50092=CARTESIAN_POINT('Ctrl Pts',(2.87363176656475,-1.,2.6056817788128));
#50093=CARTESIAN_POINT('Ctrl Pts',(2.87773881947885,-1.,2.61193507170928));
#50094=CARTESIAN_POINT('Ctrl Pts',(2.88176821427502,-1.,2.61819596473087));
#50095=CARTESIAN_POINT('Ctrl Pts',(2.88573922195049,-1.,2.62447947640253));
#50096=CARTESIAN_POINT('Ctrl Pts',(2.88967244854243,-1.,2.63080195420771));
#50097=CARTESIAN_POINT('Ctrl Pts',(2.89358228854557,-1.,2.63717442263944));
#50098=CARTESIAN_POINT('Ctrl Pts',(2.89747231723361,-1.,2.64359851684146));
#50099=CARTESIAN_POINT('Ctrl Pts',(2.90133950224879,-1.,2.65007017365576));
#50100=CARTESIAN_POINT('Ctrl Pts',(2.90517678087467,-1.,2.65658188464287));
#50101=CARTESIAN_POINT('Ctrl Pts',(2.90897617968921,-1.,2.66312542616809));
#50102=CARTESIAN_POINT('Ctrl Pts',(2.91273193382876,-1.,2.66969458792627));
#50103=CARTESIAN_POINT('Ctrl Pts',(2.91644290704281,-1.,2.67628728855309));
#50104=CARTESIAN_POINT('Ctrl Pts',(2.92011090722152,-1.,2.68290409279689));
#50105=CARTESIAN_POINT('Ctrl Pts',(2.92373955325876,-1.,2.68954721165342));
#50106=CARTESIAN_POINT('Ctrl Pts',(2.92733294395268,-1.,2.69621932864302));
#50107=CARTESIAN_POINT('Ctrl Pts',(2.93089438233746,-1.,2.70292247416881));
#50108=CARTESIAN_POINT('Ctrl Pts',(2.93442516311167,-1.,2.70965695523776));
#50109=CARTESIAN_POINT('Ctrl Pts',(2.93792519474955,-1.,2.71642190053575));
#50110=CARTESIAN_POINT('Ctrl Pts',(2.94139351933882,-1.,2.72321571511322));
#50111=CARTESIAN_POINT('Ctrl Pts',(2.94482887675139,-1.,2.73003657371613));
#50112=CARTESIAN_POINT('Ctrl Pts',(2.94823023414381,-1.,2.73688288329825));
#50113=CARTESIAN_POINT('Ctrl Pts',(2.95159737214304,-1.,2.7437537949221));
#50114=CARTESIAN_POINT('Ctrl Pts',(2.95493069316211,-1.,2.75064903318996));
#50115=CARTESIAN_POINT('Ctrl Pts',(2.9582309766594,-1.,2.75756867888393));
#50116=CARTESIAN_POINT('Ctrl Pts',(2.96149914764832,-1.,2.76451296269571));
#50117=CARTESIAN_POINT('Ctrl Pts',(2.96473605585548,-1.,2.77148206836464));
#50118=CARTESIAN_POINT('Ctrl Pts',(2.9679422104295,-1.,2.77847589542767));
#50119=CARTESIAN_POINT('Ctrl Pts',(2.97111781461349,-1.,2.78549409123657));
#50120=CARTESIAN_POINT('Ctrl Pts',(2.97426288347475,-1.,2.79253615718147));
#50121=CARTESIAN_POINT('Ctrl Pts',(2.97737733718242,-1.,2.79960153278186));
#50122=CARTESIAN_POINT('Ctrl Pts',(2.98046109647299,-1.,2.80668968101162));
#50123=CARTESIAN_POINT('Ctrl Pts',(2.9835141977994,-1.,2.81380019196454));
#50124=CARTESIAN_POINT('Ctrl Pts',(2.98653680669434,-1.,2.82093279065704));
#50125=CARTESIAN_POINT('Ctrl Pts',(2.98952916401699,-1.,2.82808728190402));
#50126=CARTESIAN_POINT('Ctrl Pts',(2.99249155170479,-1.,2.83526351254383));
#50127=CARTESIAN_POINT('Ctrl Pts',(2.995424253416,-1.,2.84246132984334));
#50128=CARTESIAN_POINT('Ctrl Pts',(2.99832751144566,-1.,2.84968053289104));
#50129=CARTESIAN_POINT('Ctrl Pts',(3.0012015079552,-1.,2.85692085715129));
#50130=CARTESIAN_POINT('Ctrl Pts',(3.00404638316245,-1.,2.86418200833065));
#50131=CARTESIAN_POINT('Ctrl Pts',(3.00686224485374,-1.,2.87146368430104));
#50132=CARTESIAN_POINT('Ctrl Pts',(3.0096491810855,-1.,2.87876560072799));
#50133=CARTESIAN_POINT('Ctrl Pts',(3.01240727309568,-1.,2.88608751706796));
#50134=CARTESIAN_POINT('Ctrl Pts',(3.01513660433291,-1.,2.8934292556764));
#50135=CARTESIAN_POINT('Ctrl Pts',(3.01783725123646,-1.,2.90079069102661));
#50136=CARTESIAN_POINT('Ctrl Pts',(3.01997487194926,-1.,2.90669553303902));
#50137=CARTESIAN_POINT('Ctrl Pts',(3.02156522743299,-1.,2.91113297349052));
#50138=CARTESIAN_POINT('Ctrl Pts',(3.02261975104912,-1.,2.91409518070707));
#50139=CARTESIAN_POINT('Ctrl Pts',(3.02314558451372,-1.,2.91557726271063));
#50140=CARTESIAN_POINT('',(2.91557726271063,-1.,3.02314558451372));
#50141=CARTESIAN_POINT('',(3.02314558451372,-1.,2.91557726271063));
#50142=CARTESIAN_POINT('',(2.50410331873176,-1.,2.79140942341258));
#50143=CARTESIAN_POINT('Ctrl Pts',(2.91557726271063,-1.,3.02314558451372));
#50144=CARTESIAN_POINT('Ctrl Pts',(2.91409518070399,-1.,3.02261975104593));
#50145=CARTESIAN_POINT('Ctrl Pts',(2.91113297348212,-1.,3.02156522742431));
#50146=CARTESIAN_POINT('Ctrl Pts',(2.90669553302526,-1.,3.01997487193503));
#50147=CARTESIAN_POINT('Ctrl Pts',(2.9007906910105,-1.,3.01783725121981));
#50148=CARTESIAN_POINT('Ctrl Pts',(2.89342925566321,-1.,3.01513660431928));
#50149=CARTESIAN_POINT('Ctrl Pts',(2.8860875170608,-1.,3.01240727308829));
#50150=CARTESIAN_POINT('Ctrl Pts',(2.87876560072727,-1.,3.00964918108476));
#50151=CARTESIAN_POINT('Ctrl Pts',(2.87146368430501,-1.,3.00686224485784));
#50152=CARTESIAN_POINT('Ctrl Pts',(2.86418200833667,-1.,3.00404638316867));
#50153=CARTESIAN_POINT('Ctrl Pts',(2.85692085715685,-1.,3.00120150796095));
#50154=CARTESIAN_POINT('Ctrl Pts',(2.84968053289451,-1.,2.99832751144925));
#50155=CARTESIAN_POINT('Ctrl Pts',(2.84246132984415,-1.,2.99542425341685));
#50156=CARTESIAN_POINT('Ctrl Pts',(2.83526351254248,-1.,2.9924915517034));
#50157=CARTESIAN_POINT('Ctrl Pts',(2.82808728190157,-1.,2.98952916401446));
#50158=CARTESIAN_POINT('Ctrl Pts',(2.82093279065457,-1.,2.9865368066918));
#50159=CARTESIAN_POINT('Ctrl Pts',(2.81380019196286,-1.,2.98351419779767));
#50160=CARTESIAN_POINT('Ctrl Pts',(2.80668968101106,-1.,2.98046109647241));
#50161=CARTESIAN_POINT('Ctrl Pts',(2.7996015327823,-1.,2.97737733718287));
#50162=CARTESIAN_POINT('Ctrl Pts',(2.79253615718248,-1.,2.9742628834758));
#50163=CARTESIAN_POINT('Ctrl Pts',(2.78549409123769,-1.,2.97111781461465));
#50164=CARTESIAN_POINT('Ctrl Pts',(2.7784758954285,-1.,2.96794221043036));
#50165=CARTESIAN_POINT('Ctrl Pts',(2.77148206836498,-1.,2.96473605585583));
#50166=CARTESIAN_POINT('Ctrl Pts',(2.76451296269557,-1.,2.96149914764818));
#50167=CARTESIAN_POINT('Ctrl Pts',(2.7575686788835,-1.,2.95823097665896));
#50168=CARTESIAN_POINT('Ctrl Pts',(2.75064903318947,-1.,2.95493069316161));
#50169=CARTESIAN_POINT('Ctrl Pts',(2.74375379492172,-1.,2.95159737214266));
#50170=CARTESIAN_POINT('Ctrl Pts',(2.73688288329808,-1.,2.94823023414364));
#50171=CARTESIAN_POINT('Ctrl Pts',(2.73003657371616,-1.,2.94482887675143));
#50172=CARTESIAN_POINT('Ctrl Pts',(2.72321571511337,-1.,2.94139351933897));
#50173=CARTESIAN_POINT('Ctrl Pts',(2.71642190053592,-1.,2.93792519474972));
#50174=CARTESIAN_POINT('Ctrl Pts',(2.70965695523787,-1.,2.93442516311179));
#50175=CARTESIAN_POINT('Ctrl Pts',(2.70292247416885,-1.,2.9308943823375));
#50176=CARTESIAN_POINT('Ctrl Pts',(2.69621932864301,-1.,2.92733294395267));
#50177=CARTESIAN_POINT('Ctrl Pts',(2.68954721165339,-1.,2.92373955325875));
#50178=CARTESIAN_POINT('Ctrl Pts',(2.68290409279688,-1.,2.92011090722152));
#50179=CARTESIAN_POINT('Ctrl Pts',(2.67628728855312,-1.,2.91644290704285));
#50180=CARTESIAN_POINT('Ctrl Pts',(2.66969458792631,-1.,2.91273193382882));
#50181=CARTESIAN_POINT('Ctrl Pts',(2.6631254261681,-1.,2.90897617968923));
#50182=CARTESIAN_POINT('Ctrl Pts',(2.65658188464282,-1.,2.90517678087461));
#50183=CARTESIAN_POINT('Ctrl Pts',(2.65007017365564,-1.,2.90133950224867));
#50184=CARTESIAN_POINT('Ctrl Pts',(2.64359851684131,-1.,2.89747231723345));
#50185=CARTESIAN_POINT('Ctrl Pts',(2.63717442263932,-1.,2.89358228854544));
#50186=CARTESIAN_POINT('Ctrl Pts',(2.63080195420767,-1.,2.88967244854239));
#50187=CARTESIAN_POINT('Ctrl Pts',(2.62447947640262,-1.,2.88573922195059));
#50188=CARTESIAN_POINT('Ctrl Pts',(2.61819596473108,-1.,2.88176821427525));
#50189=CARTESIAN_POINT('Ctrl Pts',(2.61193507170955,-1.,2.87773881947916));
#50190=CARTESIAN_POINT('Ctrl Pts',(2.60568177881303,-1.,2.87363176656501));
#50191=CARTESIAN_POINT('Ctrl Pts',(2.5994287522321,-1.,2.86943633170722));
#50192=CARTESIAN_POINT('Ctrl Pts',(2.59318160184908,-1.,2.86515629953513));
#50193=CARTESIAN_POINT('Ctrl Pts',(2.58696770643524,-1.,2.86081999003629));
#50194=CARTESIAN_POINT('Ctrl Pts',(2.58082875254357,-1.,2.85647171715092));
#50195=CARTESIAN_POINT('Ctrl Pts',(2.57480482727081,-1.,2.85215360144431));
#50196=CARTESIAN_POINT('Ctrl Pts',(2.56891984251721,-1.,2.84788893329067));
#50197=CARTESIAN_POINT('Ctrl Pts',(2.56316920798513,-1.,2.84366802680237));
#50198=CARTESIAN_POINT('Ctrl Pts',(2.55749952145241,-1.,2.83942515220782));
#50199=CARTESIAN_POINT('Ctrl Pts',(2.55182152807077,-1.,2.83505269592536));
#50200=CARTESIAN_POINT('Ctrl Pts',(2.54604736792655,-1.,2.83044254225917));
#50201=CARTESIAN_POINT('Ctrl Pts',(2.54012272520199,-1.,2.8255216764922));
#50202=CARTESIAN_POINT('Ctrl Pts',(2.53405679667412,-1.,2.82028550483689));
#50203=CARTESIAN_POINT('Ctrl Pts',(2.52796388055278,-1.,2.81484379048475));
#50204=CARTESIAN_POINT('Ctrl Pts',(2.52205778589653,-1.,2.80941521966941));
#50205=CARTESIAN_POINT('Ctrl Pts',(2.51660190465805,-1.,2.80427363984653));
#50206=CARTESIAN_POINT('Ctrl Pts',(2.51186983687818,-1.,2.79970585014168));
#50207=CARTESIAN_POINT('Ctrl Pts',(2.5081055597767,-1.,2.79596878057287));
#50208=CARTESIAN_POINT('Ctrl Pts',(2.50567182569081,-1.,2.79344192164147));
#50209=CARTESIAN_POINT('Ctrl Pts',(2.50455968395146,-1.,2.79217568804755));
#50210=CARTESIAN_POINT('Ctrl Pts',(2.50417932839313,-1.,2.79164172518905));
#50211=CARTESIAN_POINT('Ctrl Pts',(2.50410700351493,-1.,2.79145823440781));
#50212=CARTESIAN_POINT('Ctrl Pts',(2.50410331873176,-1.,2.79140942341258));
#50213=CARTESIAN_POINT('',(2.36531447826213,-1.,2.90994629141563));
#50214=CARTESIAN_POINT('Origin',(0.,-1.,0.));
#50215=CARTESIAN_POINT('',(2.52982887637028,-1.,3.35260583073571));
#50216=CARTESIAN_POINT('Ctrl Pts',(2.36531447826213,-1.,2.90994629141563));
#50217=CARTESIAN_POINT('Ctrl Pts',(2.3653621118858,-1.,2.90995756655559));
#50218=CARTESIAN_POINT('Ctrl Pts',(2.36553202948741,-1.,2.9100577052777));
#50219=CARTESIAN_POINT('Ctrl Pts',(2.36599991765853,-1.,2.91051690822262));
#50220=CARTESIAN_POINT('Ctrl Pts',(2.36707658451709,-1.,2.91181344022628));
#50221=CARTESIAN_POINT('Ctrl Pts',(2.36919161373074,-1.,2.91461249883016));
#50222=CARTESIAN_POINT('Ctrl Pts',(2.37229381109939,-1.,2.9189150379156));
#50223=CARTESIAN_POINT('Ctrl Pts',(2.37606510524271,-1.,2.92430340582912));
#50224=CARTESIAN_POINT('Ctrl Pts',(2.3802898958232,-1.,2.93049643640517));
#50225=CARTESIAN_POINT('Ctrl Pts',(2.38472771516476,-1.,2.93717903280599));
#50226=CARTESIAN_POINT('Ctrl Pts',(2.38914929090806,-1.,2.94404820669135));
#50227=CARTESIAN_POINT('Ctrl Pts',(2.39337207631613,-1.,2.95085857128372));
#50228=CARTESIAN_POINT('Ctrl Pts',(2.39730553974412,-1.,2.95748006482811));
#50229=CARTESIAN_POINT('Ctrl Pts',(2.40095565711535,-1.,2.96390432240181));
#50230=CARTESIAN_POINT('Ctrl Pts',(2.40438604734848,-1.,2.97019641312272));
#50231=CARTESIAN_POINT('Ctrl Pts',(2.40768975073691,-1.,2.97646002822395));
#50232=CARTESIAN_POINT('Ctrl Pts',(2.41095909342591,-1.,2.98280015815132));
#50233=CARTESIAN_POINT('Ctrl Pts',(2.4142506419963,-1.,2.98927983005851));
#50234=CARTESIAN_POINT('Ctrl Pts',(2.4175732450056,-1.,2.99590509293561));
#50235=CARTESIAN_POINT('Ctrl Pts',(2.42090763946812,-1.,3.00264868586038));
#50236=CARTESIAN_POINT('Ctrl Pts',(2.42421849439625,-1.,3.00946442616674));
#50237=CARTESIAN_POINT('Ctrl Pts',(2.4274685626416,-1.,3.01630420830494));
#50238=CARTESIAN_POINT('Ctrl Pts',(2.43063415586615,-1.,3.02313656035977));
#50239=CARTESIAN_POINT('Ctrl Pts',(2.43371241361462,-1.,3.02995534946946));
#50240=CARTESIAN_POINT('Ctrl Pts',(2.43671278042394,-1.,3.03676949672797));
#50241=CARTESIAN_POINT('Ctrl Pts',(2.43965194061849,-1.,3.04359685040545));
#50242=CARTESIAN_POINT('Ctrl Pts',(2.44254768923109,-1.,3.05045678021509));
#50243=CARTESIAN_POINT('Ctrl Pts',(2.44541251892568,-1.,3.05736242671521));
#50244=CARTESIAN_POINT('Ctrl Pts',(2.44824970516557,-1.,3.06431596421422));
#50245=CARTESIAN_POINT('Ctrl Pts',(2.45105688854432,-1.,3.0713129052131));
#50246=CARTESIAN_POINT('Ctrl Pts',(2.45382826787795,-1.,3.07834472886145));
#50247=CARTESIAN_POINT('Ctrl Pts',(2.45655725437037,-1.,3.08540206545313));
#50248=CARTESIAN_POINT('Ctrl Pts',(2.45923912563875,-1.,3.09247787931881));
#50249=CARTESIAN_POINT('Ctrl Pts',(2.4618730850188,-1.,3.09956993697048));
#50250=CARTESIAN_POINT('Ctrl Pts',(2.46446082979645,-1.,3.10667907901981));
#50251=CARTESIAN_POINT('Ctrl Pts',(2.46700558843507,-1.,3.11380805536124));
#50252=CARTESIAN_POINT('Ctrl Pts',(2.4695109894747,-1.,3.12096015766984));
#50253=CARTESIAN_POINT('Ctrl Pts',(2.47197997765868,-1.,3.12813790805948));
#50254=CARTESIAN_POINT('Ctrl Pts',(2.47441378371923,-1.,3.13534181229282));
#50255=CARTESIAN_POINT('Ctrl Pts',(2.47681245356095,-1.,3.14257099546531));
#50256=CARTESIAN_POINT('Ctrl Pts',(2.47917529057016,-1.,3.14982373241335));
#50257=CARTESIAN_POINT('Ctrl Pts',(2.48150133566568,-1.,3.15709802322735));
#50258=CARTESIAN_POINT('Ctrl Pts',(2.48378981792739,-1.,3.16439213290181));
#50259=CARTESIAN_POINT('Ctrl Pts',(2.48604065348619,-1.,3.17170518863357));
#50260=CARTESIAN_POINT('Ctrl Pts',(2.48825428288242,-1.,3.17903698136679));
#50261=CARTESIAN_POINT('Ctrl Pts',(2.49043146334095,-1.,3.18638771282315));
#50262=CARTESIAN_POINT('Ctrl Pts',(2.4925730723986,-1.,3.19375775555814));
#50263=CARTESIAN_POINT('Ctrl Pts',(2.49467992057726,-1.,3.20114742397549));
#50264=CARTESIAN_POINT('Ctrl Pts',(2.49675252647298,-1.,3.2085566984974));
#50265=CARTESIAN_POINT('Ctrl Pts',(2.49879114599293,-1.,3.21598526261157));
#50266=CARTESIAN_POINT('Ctrl Pts',(2.5007958720187,-1.,3.22343262620387));
#50267=CARTESIAN_POINT('Ctrl Pts',(2.50276671338074,-1.,3.23089822320596));
#50268=CARTESIAN_POINT('Ctrl Pts',(2.50470367580078,-1.,3.23838151080383));
#50269=CARTESIAN_POINT('Ctrl Pts',(2.50660685940645,-1.,3.24588208984042));
#50270=CARTESIAN_POINT('Ctrl Pts',(2.50847647070936,-1.,3.25339971461265));
#50271=CARTESIAN_POINT('Ctrl Pts',(2.51031277813697,-1.,3.26093423001716));
#50272=CARTESIAN_POINT('Ctrl Pts',(2.51211608411539,-1.,3.26848552888271));
#50273=CARTESIAN_POINT('Ctrl Pts',(2.51388669270329,-1.,3.27605350473048));
#50274=CARTESIAN_POINT('Ctrl Pts',(2.51562487464214,-1.,3.28363799702583));
#50275=CARTESIAN_POINT('Ctrl Pts',(2.51733085123316,-1.,3.2912387729863));
#50276=CARTESIAN_POINT('Ctrl Pts',(2.51900480700548,-1.,3.29885556387661));
#50277=CARTESIAN_POINT('Ctrl Pts',(2.52064689568167,-1.,3.30648808814986));
#50278=CARTESIAN_POINT('Ctrl Pts',(2.52225724871375,-1.,3.31413607874727));
#50279=CARTESIAN_POINT('Ctrl Pts',(2.52383598396878,-1.,3.32179931079521));
#50280=CARTESIAN_POINT('Ctrl Pts',(2.52538321165774,-1.,3.32947762189049));
#50281=CARTESIAN_POINT('Ctrl Pts',(2.52689902691551,-1.,3.33717090000955));
#50282=CARTESIAN_POINT('Ctrl Pts',(2.52808660916879,-1.,3.34333744117093));
#50283=CARTESIAN_POINT('Ctrl Pts',(2.5289632161143,-1.,3.34796903577628));
#50284=CARTESIAN_POINT('Ctrl Pts',(2.52954136549357,-1.,3.35105973714426));
#50285=CARTESIAN_POINT('Ctrl Pts',(2.52982887637028,-1.,3.35260583073571));
#50286=CARTESIAN_POINT('',(2.40675750623143,-1.,3.44202241512147));
#50287=CARTESIAN_POINT('',(2.52982887637028,-1.,3.35260583073571));
#50288=CARTESIAN_POINT('',(2.03660101169714,-1.,3.14877060440328));
#50289=CARTESIAN_POINT('Ctrl Pts',(2.40675750623143,-1.,3.44202241512147));
#50290=CARTESIAN_POINT('Ctrl Pts',(2.4053759295909,-1.,3.44127120683039));
#50291=CARTESIAN_POINT('Ctrl Pts',(2.40261515589405,-1.,3.43976627484234));
#50292=CARTESIAN_POINT('Ctrl Pts',(2.39848113410292,-1.,3.43750133064416));
#50293=CARTESIAN_POINT('Ctrl Pts',(2.39298338804493,-1.,3.4344663067854));
#50294=CARTESIAN_POINT('Ctrl Pts',(2.38613505843552,-1.,3.4306473271292));
#50295=CARTESIAN_POINT('Ctrl Pts',(2.37931067028926,-1.,3.42680309754399));
#50296=CARTESIAN_POINT('Ctrl Pts',(2.37251035954292,-1.,3.42293356216511));
#50297=CARTESIAN_POINT('Ctrl Pts',(2.36573431470642,-1.,3.41903866635852));
#50298=CARTESIAN_POINT('Ctrl Pts',(2.35898278606946,-1.,3.41511836751469));
#50299=CARTESIAN_POINT('Ctrl Pts',(2.35225606824109,-1.,3.41117262314119));
#50300=CARTESIAN_POINT('Ctrl Pts',(2.34555447649188,-1.,3.40720137404297));
#50301=CARTESIAN_POINT('Ctrl Pts',(2.33887832342782,-1.,3.40320452776743));
#50302=CARTESIAN_POINT('Ctrl Pts',(2.33222789882489,-1.,3.39918194577956));
#50303=CARTESIAN_POINT('Ctrl Pts',(2.3256034390248,-1.,3.39513342019756));
#50304=CARTESIAN_POINT('Ctrl Pts',(2.31900513925424,-1.,3.39105869474822));
#50305=CARTESIAN_POINT('Ctrl Pts',(2.31243319489367,-1.,3.38695751492462));
#50306=CARTESIAN_POINT('Ctrl Pts',(2.30588783640343,-1.,3.3828296733661));
#50307=CARTESIAN_POINT('Ctrl Pts',(2.29936936127624,-1.,3.37867504959433));
#50308=CARTESIAN_POINT('Ctrl Pts',(2.29287818007393,-1.,3.37449367172826));
#50309=CARTESIAN_POINT('Ctrl Pts',(2.28641481081137,-1.,3.37028570206488));
#50310=CARTESIAN_POINT('Ctrl Pts',(2.27997979458037,-1.,3.36605130713076));
#50311=CARTESIAN_POINT('Ctrl Pts',(2.2735736262093,-1.,3.36179055004409));
#50312=CARTESIAN_POINT('Ctrl Pts',(2.26719668579909,-1.,3.35750328523061));
#50313=CARTESIAN_POINT('Ctrl Pts',(2.26084915222449,-1.,3.35318902552626));
#50314=CARTESIAN_POINT('Ctrl Pts',(2.25453097693483,-1.,3.34884690292285));
#50315=CARTESIAN_POINT('Ctrl Pts',(2.24824207678256,-1.,3.34447596770723));
#50316=CARTESIAN_POINT('Ctrl Pts',(2.24198249391422,-1.,3.34007543738025));
#50317=CARTESIAN_POINT('Ctrl Pts',(2.23575256328812,-1.,3.33564495756482));
#50318=CARTESIAN_POINT('Ctrl Pts',(2.22955308907233,-1.,3.33118487773611));
#50319=CARTESIAN_POINT('Ctrl Pts',(2.22338548312772,-1.,3.3266964672289));
#50320=CARTESIAN_POINT('Ctrl Pts',(2.21725135110898,-1.,3.32218125618968));
#50321=CARTESIAN_POINT('Ctrl Pts',(2.21115211847875,-1.,3.31764044024235));
#50322=CARTESIAN_POINT('Ctrl Pts',(2.20508863150607,-1.,3.31307424608949));
#50323=CARTESIAN_POINT('Ctrl Pts',(2.19906078949922,-1.,3.30848134694595));
#50324=CARTESIAN_POINT('Ctrl Pts',(2.19306710376111,-1.,3.30385816281831));
#50325=CARTESIAN_POINT('Ctrl Pts',(2.18710556500327,-1.,3.29920022557639));
#50326=CARTESIAN_POINT('Ctrl Pts',(2.18117455557065,-1.,3.2945036150049));
#50327=CARTESIAN_POINT('Ctrl Pts',(2.17527380048423,-1.,3.28976645712568));
#50328=CARTESIAN_POINT('Ctrl Pts',(2.16940517773455,-1.,3.28499019979724));
#50329=CARTESIAN_POINT('Ctrl Pts',(2.16357391934425,-1.,3.280181508414));
#50330=CARTESIAN_POINT('Ctrl Pts',(2.15778690038347,-1.,3.27534954469187));
#50331=CARTESIAN_POINT('Ctrl Pts',(2.15205043199808,-1.,3.27050245897228));
#50332=CARTESIAN_POINT('Ctrl Pts',(2.1463680529566,-1.,3.26564388189759));
#50333=CARTESIAN_POINT('Ctrl Pts',(2.14073870754264,-1.,3.26077002641879));
#50334=CARTESIAN_POINT('Ctrl Pts',(2.13515375878803,-1.,3.25586495065054));
#50335=CARTESIAN_POINT('Ctrl Pts',(2.12960028396832,-1.,3.25090574494028));
#50336=CARTESIAN_POINT('Ctrl Pts',(2.12406646410962,-1.,3.24587102613376));
#50337=CARTESIAN_POINT('Ctrl Pts',(2.11854673326979,-1.,3.24074905517293));
#50338=CARTESIAN_POINT('Ctrl Pts',(2.11304604021773,-1.,3.23554444767099));
#50339=CARTESIAN_POINT('Ctrl Pts',(2.10758699642451,-1.,3.23028945793289));
#50340=CARTESIAN_POINT('Ctrl Pts',(2.10220384298492,-1.,3.22503437553434));
#50341=CARTESIAN_POINT('Ctrl Pts',(2.09692958434895,-1.,3.21982707347009));
#50342=CARTESIAN_POINT('Ctrl Pts',(2.09178419460443,-1.,3.21469429601654));
#50343=CARTESIAN_POINT('Ctrl Pts',(2.08676465517455,-1.,3.20962575845463));
#50344=CARTESIAN_POINT('Ctrl Pts',(2.08182850370878,-1.,3.2045481863073));
#50345=CARTESIAN_POINT('Ctrl Pts',(2.07690441870722,-1.,3.19934132836019));
#50346=CARTESIAN_POINT('Ctrl Pts',(2.07192253497857,-1.,3.19388465568252));
#50347=CARTESIAN_POINT('Ctrl Pts',(2.06684062744112,-1.,3.18809755562368));
#50348=CARTESIAN_POINT('Ctrl Pts',(2.06166849827101,-1.,3.18197692964614));
#50349=CARTESIAN_POINT('Ctrl Pts',(2.05650186773132,-1.,3.17564906975371));
#50350=CARTESIAN_POINT('Ctrl Pts',(2.05151770247233,-1.,3.16936341689527));
#50351=CARTESIAN_POINT('Ctrl Pts',(2.04693331247446,-1.,3.16343165058912));
#50352=CARTESIAN_POINT('Ctrl Pts',(2.04297406404027,-1.,3.15817983946367));
#50353=CARTESIAN_POINT('Ctrl Pts',(2.03984073791519,-1.,3.15389991674792));
#50354=CARTESIAN_POINT('Ctrl Pts',(2.03783225495961,-1.,3.15102344775328));
#50355=CARTESIAN_POINT('Ctrl Pts',(2.03693188810544,-1.,3.14959882629805));
#50356=CARTESIAN_POINT('Ctrl Pts',(2.03663974554932,-1.,3.1490119366901));
#50357=CARTESIAN_POINT('Ctrl Pts',(2.03659701539259,-1.,3.14881939088124));
#50358=CARTESIAN_POINT('Ctrl Pts',(2.03660101169714,-1.,3.14877060440328));
#50359=CARTESIAN_POINT('',(1.88097764062697,-1.,3.24413672884812));
#50360=CARTESIAN_POINT('Origin',(0.,-1.,0.));
#50361=CARTESIAN_POINT('',(1.97421938526992,-1.,3.70708211654725));
#50362=CARTESIAN_POINT('Ctrl Pts',(1.88097764062697,-1.,3.24413672884812));
#50363=CARTESIAN_POINT('Ctrl Pts',(1.8810229239812,-1.,3.24415531671284));
#50364=CARTESIAN_POINT('Ctrl Pts',(1.88117508446775,-1.,3.24428080353022));
#50365=CARTESIAN_POINT('Ctrl Pts',(1.88156537699203,-1.,3.24480754676064));
#50366=CARTESIAN_POINT('Ctrl Pts',(1.88242596600454,-1.,3.2462565441079));
#50367=CARTESIAN_POINT('Ctrl Pts',(1.88407708646357,-1.,3.24935200511918));
#50368=CARTESIAN_POINT('Ctrl Pts',(1.88646802523466,-1.,3.25408686339463));
#50369=CARTESIAN_POINT('Ctrl Pts',(1.88934996203698,-1.,3.25999885193947));
#50370=CARTESIAN_POINT('Ctrl Pts',(1.89255393500965,-1.,3.26677653888676));
#50371=CARTESIAN_POINT('Ctrl Pts',(1.89589172903793,-1.,3.27407108933139));
#50372=CARTESIAN_POINT('Ctrl Pts',(1.89918429230462,-1.,3.28154737912352));
#50373=CARTESIAN_POINT('Ctrl Pts',(1.90228971247527,-1.,3.2889344860029));
#50374=CARTESIAN_POINT('Ctrl Pts',(1.90513891864087,-1.,3.29608978722113));
#50375=CARTESIAN_POINT('Ctrl Pts',(1.90773912171341,-1.,3.30300595568195));
#50376=CARTESIAN_POINT('Ctrl Pts',(1.91014297830446,-1.,3.30975721158596));
#50377=CARTESIAN_POINT('Ctrl Pts',(1.91242616234442,-1.,3.31646052426364));
#50378=CARTESIAN_POINT('Ctrl Pts',(1.91466343916627,-1.,3.32323403454535));
#50379=CARTESIAN_POINT('Ctrl Pts',(1.91690081930331,-1.,3.33014884257873));
#50380=CARTESIAN_POINT('Ctrl Pts',(1.9191460961021,-1.,3.33721230710012));
#50381=CARTESIAN_POINT('Ctrl Pts',(1.92138450828404,-1.,3.34439448941961));
#50382=CARTESIAN_POINT('Ctrl Pts',(1.92358838440528,-1.,3.35164424847223));
#50383=CARTESIAN_POINT('Ctrl Pts',(1.92572846125756,-1.,3.35890824422965));
#50384=CARTESIAN_POINT('Ctrl Pts',(1.92778626543786,-1.,3.36615168657567));
#50385=CARTESIAN_POINT('Ctrl Pts',(1.92975993109877,-1.,3.37336807068043));
#50386=CARTESIAN_POINT('Ctrl Pts',(1.93165739093276,-1.,3.3805676852555));
#50387=CARTESIAN_POINT('Ctrl Pts',(1.93349233176788,-1.,3.38777076883256));
#50388=CARTESIAN_POINT('Ctrl Pts',(1.93527929945985,-1.,3.39499923640795));
#50389=CARTESIAN_POINT('Ctrl Pts',(1.93702857723098,-1.,3.40226802104109));
#50390=CARTESIAN_POINT('Ctrl Pts',(1.93874306008143,-1.,3.40957978266642));
#50391=CARTESIAN_POINT('Ctrl Pts',(1.94042111965246,-1.,3.41692971994096));
#50392=CARTESIAN_POINT('Ctrl Pts',(1.94205835913696,-1.,3.42430850941503));
#50393=CARTESIAN_POINT('Ctrl Pts',(1.94364973660284,-1.,3.43170586602434));
#50394=CARTESIAN_POINT('Ctrl Pts',(1.94519168842879,-1.,3.43911410197687));
#50395=CARTESIAN_POINT('Ctrl Pts',(1.94668377715329,-1.,3.44653088665681));
#50396=CARTESIAN_POINT('Ctrl Pts',(1.94812754766524,-1.,3.45395731584051));
#50397=CARTESIAN_POINT('Ctrl Pts',(1.94952575850197,-1.,3.46139661060962));
#50398=CARTESIAN_POINT('Ctrl Pts',(1.95088147859876,-1.,3.46885258974191));
#50399=CARTESIAN_POINT('Ctrl Pts',(1.95219722189876,-1.,3.47632820495921));
#50400=CARTESIAN_POINT('Ctrl Pts',(1.95347412486308,-1.,3.48382414832634));
#50401=CARTESIAN_POINT('Ctrl Pts',(1.95471236969643,-1.,3.49133956289133));
#50402=CARTESIAN_POINT('Ctrl Pts',(1.95591153823661,-1.,3.49887263575583));
#50403=CARTESIAN_POINT('Ctrl Pts',(1.95707099606511,-1.,3.50642124159909));
#50404=CARTESIAN_POINT('Ctrl Pts',(1.95819025316779,-1.,3.51398354617794));
#50405=CARTESIAN_POINT('Ctrl Pts',(1.95926936324461,-1.,3.52155867431486));
#50406=CARTESIAN_POINT('Ctrl Pts',(1.96030879411566,-1.,3.52914648844351));
#50407=CARTESIAN_POINT('Ctrl Pts',(1.96130926212689,-1.,3.53674730625813));
#50408=CARTESIAN_POINT('Ctrl Pts',(1.96227157573067,-1.,3.54436163300443));
#50409=CARTESIAN_POINT('Ctrl Pts',(1.96319648628644,-1.,3.55198990600886));
#50410=CARTESIAN_POINT('Ctrl Pts',(1.96408450906812,-1.,3.55963218706096));
#50411=CARTESIAN_POINT('Ctrl Pts',(1.96493594634567,-1.,3.56728820357791));
#50412=CARTESIAN_POINT('Ctrl Pts',(1.96575096652789,-1.,3.57495748600959));
#50413=CARTESIAN_POINT('Ctrl Pts',(1.96652966688911,-1.,3.58263947663829));
#50414=CARTESIAN_POINT('Ctrl Pts',(1.96727213799544,-1.,3.59033364022801));
#50415=CARTESIAN_POINT('Ctrl Pts',(1.96797854118369,-1.,3.59803959819938));
#50416=CARTESIAN_POINT('Ctrl Pts',(1.9686491188594,-1.,3.60575714017989));
#50417=CARTESIAN_POINT('Ctrl Pts',(1.96928416040877,-1.,3.61348615496704));
#50418=CARTESIAN_POINT('Ctrl Pts',(1.96988398129978,-1.,3.62122658401893));
#50419=CARTESIAN_POINT('Ctrl Pts',(1.97044889850463,-1.,3.62897836973293));
#50420=CARTESIAN_POINT('Ctrl Pts',(1.97097920454464,-1.,3.63674139590412));
#50421=CARTESIAN_POINT('Ctrl Pts',(1.97147515441164,-1.,3.64451546723514));
#50422=CARTESIAN_POINT('Ctrl Pts',(1.97193697240239,-1.,3.652300347166));
#50423=CARTESIAN_POINT('Ctrl Pts',(1.9723648543905,-1.,3.6600957816636));
#50424=CARTESIAN_POINT('Ctrl Pts',(1.97275897198678,-1.,3.66790152752075));
#50425=CARTESIAN_POINT('Ctrl Pts',(1.97311947678516,-1.,3.67571738107084));
#50426=CARTESIAN_POINT('Ctrl Pts',(1.97344650304519,-1.,3.68354319915092));
#50427=CARTESIAN_POINT('Ctrl Pts',(1.97374016225483,-1.,3.69137888599902));
#50428=CARTESIAN_POINT('Ctrl Pts',(1.97394846383216,-1.,3.6976552856004));
#50429=CARTESIAN_POINT('Ctrl Pts',(1.97408973726715,-1.,3.70236698912904));
#50430=CARTESIAN_POINT('Ctrl Pts',(1.97417727645308,-1.,3.70551008132332));
#50431=CARTESIAN_POINT('Ctrl Pts',(1.97421938526992,-1.,3.70708211654725));
#50432=CARTESIAN_POINT('',(1.8386753923786,-1.,3.77614523045147));
#50433=CARTESIAN_POINT('',(1.97421938526992,-1.,3.70708211654725));
#50434=CARTESIAN_POINT('',(1.5189508286633,-1.,3.42859860294306));
#50435=CARTESIAN_POINT('Ctrl Pts',(1.8386753923786,-1.,3.77614523045147));
#50436=CARTESIAN_POINT('Ctrl Pts',(1.83742834010626,-1.,3.77518714457833));
#50437=CARTESIAN_POINT('Ctrl Pts',(1.83493697934534,-1.,3.77326886064398));
#50438=CARTESIAN_POINT('Ctrl Pts',(1.83120816955645,-1.,3.77038509817999));
#50439=CARTESIAN_POINT('Ctrl Pts',(1.82625289220915,-1.,3.76652740353775));
#50440=CARTESIAN_POINT('Ctrl Pts',(1.82008629694091,-1.,3.76168412707948));
#50441=CARTESIAN_POINT('Ctrl Pts',(1.8139472983358,-1.,3.75681965683071));
#50442=CARTESIAN_POINT('Ctrl Pts',(1.80783603939617,-1.,3.75193395887977));
#50443=CARTESIAN_POINT('Ctrl Pts',(1.8017527148577,-1.,3.74702700875467));
#50444=CARTESIAN_POINT('Ctrl Pts',(1.79569757859422,-1.,3.74209880352445));
#50445=CARTESIAN_POINT('Ctrl Pts',(1.78967092823491,-1.,3.73714934730681));
#50446=CARTESIAN_POINT('Ctrl Pts',(1.78367308442901,-1.,3.7321786309547));
#50447=CARTESIAN_POINT('Ctrl Pts',(1.77770437039658,-1.,3.72718661205609));
#50448=CARTESIAN_POINT('Ctrl Pts',(1.77176509401761,-1.,3.72217319911254));
#50449=CARTESIAN_POINT('Ctrl Pts',(1.76585552124394,-1.,3.71713822377359));
#50450=CARTESIAN_POINT('Ctrl Pts',(1.75997588498865,-1.,3.71208146346136));
#50451=CARTESIAN_POINT('Ctrl Pts',(1.75412641804042,-1.,3.70700269736659));
#50452=CARTESIAN_POINT('Ctrl Pts',(1.74830738046057,-1.,3.7019017567335));
#50453=CARTESIAN_POINT('Ctrl Pts',(1.74251908492617,-1.,3.69677856910517));
#50454=CARTESIAN_POINT('Ctrl Pts',(1.73676193254557,-1.,3.69163322648036));
#50455=CARTESIAN_POINT('Ctrl Pts',(1.73103640956717,-1.,3.68646597019332));
#50456=CARTESIAN_POINT('Ctrl Pts',(1.72534302437056,-1.,3.68127704936579));
#50457=CARTESIAN_POINT('Ctrl Pts',(1.71968225581808,-1.,3.67606660374709));
#50458=CARTESIAN_POINT('Ctrl Pts',(1.71405450210383,-1.,3.67083454901611));
#50459=CARTESIAN_POINT('Ctrl Pts',(1.70846001610956,-1.,3.66558043198876));
#50460=CARTESIAN_POINT('Ctrl Pts',(1.70289888566873,-1.,3.66030338774847));
#50461=CARTESIAN_POINT('Ctrl Pts',(1.69737117722534,-1.,3.65500246526749));
#50462=CARTESIAN_POINT('Ctrl Pts',(1.69187705481689,-1.,3.64967689827371));
#50463=CARTESIAN_POINT('Ctrl Pts',(1.68641690471457,-1.,3.64432638915203));
#50464=CARTESIAN_POINT('Ctrl Pts',(1.68099146651586,-1.,3.63895140887462));
#50465=CARTESIAN_POINT('Ctrl Pts',(1.67560193613156,-1.,3.63355343201232));
#50466=CARTESIAN_POINT('Ctrl Pts',(1.67024966008044,-1.,3.62813422105271));
#50467=CARTESIAN_POINT('Ctrl Pts',(1.66493585923855,-1.,3.62269517989109));
#50468=CARTESIAN_POINT('Ctrl Pts',(1.65966133399186,-1.,3.61723666482456));
#50469=CARTESIAN_POINT('Ctrl Pts',(1.65442619244325,-1.,3.61175734965127));
#50470=CARTESIAN_POINT('Ctrl Pts',(1.64922952425832,-1.,3.60625346556992));
#50471=CARTESIAN_POINT('Ctrl Pts',(1.64407004385582,-1.,3.60072028513845));
#50472=CARTESIAN_POINT('Ctrl Pts',(1.63894676675352,-1.,3.59515368334893));
#50473=CARTESIAN_POINT('Ctrl Pts',(1.6338597145126,-1.,3.58955176627879));
#50474=CARTESIAN_POINT('Ctrl Pts',(1.62881051550745,-1.,3.58391625774343));
#50475=CARTESIAN_POINT('Ctrl Pts',(1.62380329464844,-1.,3.5782545595439));
#50476=CARTESIAN_POINT('Ctrl Pts',(1.61884340915404,-1.,3.57257679609806));
#50477=CARTESIAN_POINT('Ctrl Pts',(1.61393581747514,-1.,3.56689200468387));
#50478=CARTESIAN_POINT('Ctrl Pts',(1.60908344685457,-1.,3.5612043248298));
#50479=CARTESIAN_POINT('Ctrl Pts',(1.60428584699853,-1.,3.55550985096129));
#50480=CARTESIAN_POINT('Ctrl Pts',(1.59953698113457,-1.,3.54979148634454));
#50481=CARTESIAN_POINT('Ctrl Pts',(1.59482766949766,-1.,3.54402458182337));
#50482=CARTESIAN_POINT('Ctrl Pts',(1.59014958368739,-1.,3.53818616861077));
#50483=CARTESIAN_POINT('Ctrl Pts',(1.58549906268088,-1.,3.5322637814708));
#50484=CARTESIAN_POINT('Ctrl Pts',(1.58088027227848,-1.,3.52626275334881));
#50485=CARTESIAN_POINT('Ctrl Pts',(1.57631049988158,-1.,3.52021847865912));
#50486=CARTESIAN_POINT('Ctrl Pts',(1.57181569799743,-1.,3.51418598431665));
#50487=CARTESIAN_POINT('Ctrl Pts',(1.56742097575012,-1.,3.50821771695363));
#50488=CARTESIAN_POINT('Ctrl Pts',(1.56314187758675,-1.,3.50234321621578));
#50489=CARTESIAN_POINT('Ctrl Pts',(1.55897703097874,-1.,3.49655185179655));
#50490=CARTESIAN_POINT('Ctrl Pts',(1.55489595901116,-1.,3.4907646087742));
#50491=CARTESIAN_POINT('Ctrl Pts',(1.55084702970452,-1.,3.48485155928567));
#50492=CARTESIAN_POINT('Ctrl Pts',(1.54678009290276,-1.,3.47868272898751));
#50493=CARTESIAN_POINT('Ctrl Pts',(1.54266605398187,-1.,3.47217189224653));
#50494=CARTESIAN_POINT('Ctrl Pts',(1.53851507915502,-1.,3.46531752207153));
#50495=CARTESIAN_POINT('Ctrl Pts',(1.53440195378792,-1.,3.45825932955032));
#50496=CARTESIAN_POINT('Ctrl Pts',(1.53046244461635,-1.,3.45127136828305));
#50497=CARTESIAN_POINT('Ctrl Pts',(1.52686242875556,-1.,3.44469547526647));
#50498=CARTESIAN_POINT('Ctrl Pts',(1.5237734895035,-1.,3.4388889597401));
#50499=CARTESIAN_POINT('Ctrl Pts',(1.52134826724292,-1.,3.43417156977893));
#50500=CARTESIAN_POINT('Ctrl Pts',(1.5198144909338,-1.,3.43101631893414));
#50501=CARTESIAN_POINT('Ctrl Pts',(1.51914806898491,-1.,3.42946838852587));
#50502=CARTESIAN_POINT('Ctrl Pts',(1.5189513329503,-1.,3.42884302333841));
#50503=CARTESIAN_POINT('Ctrl Pts',(1.51893924967331,-1.,3.42864616361875));
#50504=CARTESIAN_POINT('Ctrl Pts',(1.5189508286633,-1.,3.42859860294306));
#50505=CARTESIAN_POINT('',(1.35032489087269,-1.,3.49844575334386));
#50506=CARTESIAN_POINT('Origin',(0.,-1.,0.));
#50507=CARTESIAN_POINT('',(1.36999806084572,-1.,3.97027773754922));
#50508=CARTESIAN_POINT('Ctrl Pts',(1.35032489087269,-1.,3.49844575334386));
#50509=CARTESIAN_POINT('Ctrl Pts',(1.35036670893102,-1.,3.49847119623841));
#50510=CARTESIAN_POINT('Ctrl Pts',(1.35049736560633,-1.,3.49861894124915));
#50511=CARTESIAN_POINT('Ctrl Pts',(1.35080045218652,-1.,3.49920025459856));
#50512=CARTESIAN_POINT('Ctrl Pts',(1.35142377279535,-1.,3.5007660381658));
#50513=CARTESIAN_POINT('Ctrl Pts',(1.3525703284343,-1.,3.50408168106113));
#50514=CARTESIAN_POINT('Ctrl Pts',(1.35419113576022,-1.,3.50913227060177));
#50515=CARTESIAN_POINT('Ctrl Pts',(1.35611275237288,-1.,3.51542230699919));
#50516=CARTESIAN_POINT('Ctrl Pts',(1.35821701528975,-1.,3.52261776117121));
#50517=CARTESIAN_POINT('Ctrl Pts',(1.36037259643827,-1.,3.53034464961849));
#50518=CARTESIAN_POINT('Ctrl Pts',(1.36245507339334,-1.,3.53824396425032));
#50519=CARTESIAN_POINT('Ctrl Pts',(1.36436666257567,-1.,3.54602591832893));
#50520=CARTESIAN_POINT('Ctrl Pts',(1.36606145456711,-1.,3.55353883995793));
#50521=CARTESIAN_POINT('Ctrl Pts',(1.36754771771174,-1.,3.56077662028492));
#50522=CARTESIAN_POINT('Ctrl Pts',(1.36886584973349,-1.,3.56782080304554));
#50523=CARTESIAN_POINT('Ctrl Pts',(1.37007229485646,-1.,3.57479875549453));
#50524=CARTESIAN_POINT('Ctrl Pts',(1.37122241663073,-1.,3.58183885982745));
#50525=CARTESIAN_POINT('Ctrl Pts',(1.37235053661,-1.,3.5890185384643));
#50526=CARTESIAN_POINT('Ctrl Pts',(1.37346320103184,-1.,3.59634627869117));
#50527=CARTESIAN_POINT('Ctrl Pts',(1.37455051379642,-1.,3.60379020124038));
#50528=CARTESIAN_POINT('Ctrl Pts',(1.37559314436641,-1.,3.61129546591082));
#50529=CARTESIAN_POINT('Ctrl Pts',(1.37657053403102,-1.,3.61880481160408));
#50530=CARTESIAN_POINT('Ctrl Pts',(1.37746987919868,-1.,3.62628098665112));
#50531=CARTESIAN_POINT('Ctrl Pts',(1.37829035457324,-1.,3.63371727442448));
#50532=CARTESIAN_POINT('Ctrl Pts',(1.37903818567347,-1.,3.64112507791112));
#50533=CARTESIAN_POINT('Ctrl Pts',(1.37972372481598,-1.,3.64852652756444));
#50534=CARTESIAN_POINT('Ctrl Pts',(1.38035791051215,-1.,3.65594554404396));
#50535=CARTESIAN_POINT('Ctrl Pts',(1.38094856333558,-1.,3.66339848520874));
#50536=CARTESIAN_POINT('Ctrl Pts',(1.38149812653876,-1.,3.67088843112282));
#50537=CARTESIAN_POINT('Ctrl Pts',(1.38200574290626,-1.,3.6784103848243));
#50538=CARTESIAN_POINT('Ctrl Pts',(1.38246852827185,-1.,3.68595444983844));
#50539=CARTESIAN_POINT('Ctrl Pts',(1.38288311171649,-1.,3.69350967899523));
#50540=CARTESIAN_POINT('Ctrl Pts',(1.38324717612862,-1.,3.70106792167894));
#50541=CARTESIAN_POINT('Ctrl Pts',(1.38356065402122,-1.,3.70862680753343));
#50542=CARTESIAN_POINT('Ctrl Pts',(1.38382489984585,-1.,3.7161876605181));
#50543=CARTESIAN_POINT('Ctrl Pts',(1.3840421342895,-1.,3.72375409358805));
#50544=CARTESIAN_POINT('Ctrl Pts',(1.38421479111531,-1.,3.73133035859283));
#50545=CARTESIAN_POINT('Ctrl Pts',(1.38434489156456,-1.,3.73891976418099));
#50546=CARTESIAN_POINT('Ctrl Pts',(1.38443344984389,-1.,3.7465231716786));
#50547=CARTESIAN_POINT('Ctrl Pts',(1.38448077997155,-1.,3.75413976318727));
#50548=CARTESIAN_POINT('Ctrl Pts',(1.38448675253343,-1.,3.76176768271347));
#50549=CARTESIAN_POINT('Ctrl Pts',(1.38445107339517,-1.,3.76940473185775));
#50550=CARTESIAN_POINT('Ctrl Pts',(1.38437354551435,-1.,3.77704902230441));
#50551=CARTESIAN_POINT('Ctrl Pts',(1.38425435883773,-1.,3.78469969805134));
#50552=CARTESIAN_POINT('Ctrl Pts',(1.38409399694588,-1.,3.79235669640907));
#50553=CARTESIAN_POINT('Ctrl Pts',(1.38389311766701,-1.,3.80002044322169));
#50554=CARTESIAN_POINT('Ctrl Pts',(1.38365244046226,-1.,3.80769156398429));
#50555=CARTESIAN_POINT('Ctrl Pts',(1.38337263902766,-1.,3.81537060817765));
#50556=CARTESIAN_POINT('Ctrl Pts',(1.38305421262724,-1.,3.82305771743715));
#50557=CARTESIAN_POINT('Ctrl Pts',(1.38269750245086,-1.,3.83075266982138));
#50558=CARTESIAN_POINT('Ctrl Pts',(1.38230274828774,-1.,3.83845502790609));
#50559=CARTESIAN_POINT('Ctrl Pts',(1.38187013346089,-1.,3.84616425605705));
#50560=CARTESIAN_POINT('Ctrl Pts',(1.38139983115075,-1.,3.85387983979557));
#50561=CARTESIAN_POINT('Ctrl Pts',(1.38089205993067,-1.,3.86160143044187));
#50562=CARTESIAN_POINT('Ctrl Pts',(1.38034709213129,-1.,3.86932885813403));
#50563=CARTESIAN_POINT('Ctrl Pts',(1.37976523097187,-1.,3.87706205830865));
#50564=CARTESIAN_POINT('Ctrl Pts',(1.37914679719446,-1.,3.88480102249461));
#50565=CARTESIAN_POINT('Ctrl Pts',(1.37849211287981,-1.,3.89254574338385));
#50566=CARTESIAN_POINT('Ctrl Pts',(1.3778014851263,-1.,3.90029615196255));
#50567=CARTESIAN_POINT('Ctrl Pts',(1.3770751963376,-1.,3.90805209522729));
#50568=CARTESIAN_POINT('Ctrl Pts',(1.37631350505516,-1.,3.91581337461825));
#50569=CARTESIAN_POINT('Ctrl Pts',(1.37551664448057,-1.,3.92357976987132));
#50570=CARTESIAN_POINT('Ctrl Pts',(1.37468482215784,-1.,3.93135106761941));
#50571=CARTESIAN_POINT('Ctrl Pts',(1.37381821967499,-1.,3.93912709041791));
#50572=CARTESIAN_POINT('Ctrl Pts',(1.37291699203423,-1.,3.94690771786926));
#50573=CARTESIAN_POINT('Ctrl Pts',(1.37198126433139,-1.,3.95469287283105));
#50574=CARTESIAN_POINT('Ctrl Pts',(1.37120515615663,-1.,3.96092458508407));
#50575=CARTESIAN_POINT('Ctrl Pts',(1.37060761746027,-1.,3.96560037975788));
#50576=CARTESIAN_POINT('Ctrl Pts',(1.37020239094758,-1.,3.9687184694173));
#50577=CARTESIAN_POINT('Ctrl Pts',(1.36999806084572,-1.,3.97027773754922));
#50578=CARTESIAN_POINT('',(1.22531898815164,-1.,4.01728681790024));
#50579=CARTESIAN_POINT('',(1.36999806084572,-1.,3.97027773754922));
#50580=CARTESIAN_POINT('',(0.963899035118985,-1.,3.62400312501199));
#50581=CARTESIAN_POINT('Ctrl Pts',(1.22531898815164,-1.,4.01728681790024));
#50582=CARTESIAN_POINT('Ctrl Pts',(1.22423716681317,-1.,4.01614544569895));
#50583=CARTESIAN_POINT('Ctrl Pts',(1.22207656455845,-1.,4.01386104433519));
#50584=CARTESIAN_POINT('Ctrl Pts',(1.21884478244403,-1.,4.01042947140789));
#50585=CARTESIAN_POINT('Ctrl Pts',(1.21455398918133,-1.,4.00584409522722));
#50586=CARTESIAN_POINT('Ctrl Pts',(1.20922097029551,-1.,4.00009577950721));
#50587=CARTESIAN_POINT('Ctrl Pts',(1.20391852375138,-1.,3.99433084799666));
#50588=CARTESIAN_POINT('Ctrl Pts',(1.19864679609566,-1.,3.98854928957189));
#50589=CARTESIAN_POINT('Ctrl Pts',(1.19340598349475,-1.,3.98275111052561));
#50590=CARTESIAN_POINT('Ctrl Pts',(1.18819633715539,-1.,3.97693634767754));
#50591=CARTESIAN_POINT('Ctrl Pts',(1.18301815039831,-1.,3.97110505165415));
#50592=CARTESIAN_POINT('Ctrl Pts',(1.17787174135592,-1.,3.96525726358159));
#50593=CARTESIAN_POINT('Ctrl Pts',(1.17275743590361,-1.,3.95939299213276));
#50594=CARTESIAN_POINT('Ctrl Pts',(1.16767555244438,-1.,3.95351219509876));
#50595=CARTESIAN_POINT('Ctrl Pts',(1.16262637999157,-1.,3.94761474780583));
#50596=CARTESIAN_POINT('Ctrl Pts',(1.15761018340956,-1.,3.94170046685203));
#50597=CARTESIAN_POINT('Ctrl Pts',(1.1526272271632,-1.,3.9357691705628));
#50598=CARTESIAN_POINT('Ctrl Pts',(1.14767779451123,-1.,3.92982073294257));
#50599=CARTESIAN_POINT('Ctrl Pts',(1.14276220561593,-1.,3.92385513133997));
#50600=CARTESIAN_POINT('Ctrl Pts',(1.13788084225554,-1.,3.91787251936827));
#50601=CARTESIAN_POINT('Ctrl Pts',(1.13303414693896,-1.,3.91187321145649));
#50602=CARTESIAN_POINT('Ctrl Pts',(1.12822258281553,-1.,3.90585753318737));
#50603=CARTESIAN_POINT('Ctrl Pts',(1.12344660099043,-1.,3.89982569750025));
#50604=CARTESIAN_POINT('Ctrl Pts',(1.11870660794603,-1.,3.89377768340344));
#50605=CARTESIAN_POINT('Ctrl Pts',(1.11400292434429,-1.,3.88771308285171));
#50606=CARTESIAN_POINT('Ctrl Pts',(1.10933577224008,-1.,3.88163105531724));
#50607=CARTESIAN_POINT('Ctrl Pts',(1.10470536603287,-1.,3.87553067187514));
#50608=CARTESIAN_POINT('Ctrl Pts',(1.10011198761195,-1.,3.86941120134849));
#50609=CARTESIAN_POINT('Ctrl Pts',(1.09555606505013,-1.,3.86327241021247));
#50610=CARTESIAN_POINT('Ctrl Pts',(1.09103825516294,-1.,3.85711487933931));
#50611=CARTESIAN_POINT('Ctrl Pts',(1.08655950846384,-1.,3.85094025222713));
#50612=CARTESIAN_POINT('Ctrl Pts',(1.08212087917991,-1.,3.8447504803063));
#50613=CARTESIAN_POINT('Ctrl Pts',(1.07772335353858,-1.,3.83854714117491));
#50614=CARTESIAN_POINT('Ctrl Pts',(1.07336766633459,-1.,3.83233071195144));
#50615=CARTESIAN_POINT('Ctrl Pts',(1.06905413180359,-1.,3.82609989967276));
#50616=CARTESIAN_POINT('Ctrl Pts',(1.0647824403893,-1.,3.81985083953012));
#50617=CARTESIAN_POINT('Ctrl Pts',(1.06055206187299,-1.,3.8135786611749));
#50618=CARTESIAN_POINT('Ctrl Pts',(1.05636266918644,-1.,3.80727913637791));
#50619=CARTESIAN_POINT('Ctrl Pts',(1.05221457990016,-1.,3.80095039790681));
#50620=CARTESIAN_POINT('Ctrl Pts',(1.04810913267639,-1.,3.79459440308786));
#50621=CARTESIAN_POINT('Ctrl Pts',(1.04404924374422,-1.,3.78821910787179));
#50622=CARTESIAN_POINT('Ctrl Pts',(1.04003862055798,-1.,3.7818353500817));
#50623=CARTESIAN_POINT('Ctrl Pts',(1.03608074678008,-1.,3.77545283140427));
#50624=CARTESIAN_POINT('Ctrl Pts',(1.03217786604919,-1.,3.76907609832516));
#50625=CARTESIAN_POINT('Ctrl Pts',(1.02833014458184,-1.,3.76270122291245));
#50626=CARTESIAN_POINT('Ctrl Pts',(1.02453429444668,-1.,3.75631037456224));
#50627=CARTESIAN_POINT('Ctrl Pts',(1.02078510487439,-1.,3.74987777155873));
#50628=CARTESIAN_POINT('Ctrl Pts',(1.01707794311088,-1.,3.74337942504993));
#50629=CARTESIAN_POINT('Ctrl Pts',(1.01341114319906,-1.,3.73680245055747));
#50630=CARTESIAN_POINT('Ctrl Pts',(1.00978798539491,-1.,3.73015276704407));
#50631=CARTESIAN_POINT('Ctrl Pts',(1.00622000735696,-1.,3.72346803750544));
#50632=CARTESIAN_POINT('Ctrl Pts',(1.00272423396802,-1.,3.71680667125047));
#50633=CARTESIAN_POINT('Ctrl Pts',(0.999317260756344,-1.,3.7102243971387));
#50634=CARTESIAN_POINT('Ctrl Pts',(0.996009819772431,-1.,3.70375282282107));
#50635=CARTESIAN_POINT('Ctrl Pts',(0.992802218332103,-1.,3.69738123415696));
#50636=CARTESIAN_POINT('Ctrl Pts',(0.989676715398858,-1.,3.69102682138955));
#50637=CARTESIAN_POINT('Ctrl Pts',(0.986602639864285,-1.,3.6845531792623));
#50638=CARTESIAN_POINT('Ctrl Pts',(0.983550791470864,-1.,3.67782408841876));
#50639=CARTESIAN_POINT('Ctrl Pts',(0.980505922458494,-1.,3.67074983340444));
#50640=CARTESIAN_POINT('Ctrl Pts',(0.977478312751416,-1.,3.66333049637403));
#50641=CARTESIAN_POINT('Ctrl Pts',(0.974519971354138,-1.,3.6557157673487));
#50642=CARTESIAN_POINT('Ctrl Pts',(0.971722122060277,-1.,3.64819756447072));
#50643=CARTESIAN_POINT('Ctrl Pts',(0.969195124674828,-1.,3.64113946505393));
#50644=CARTESIAN_POINT('Ctrl Pts',(0.967052554540877,-1.,3.6349212208096));
#50645=CARTESIAN_POINT('Ctrl Pts',(0.965395153165715,-1.,3.62988252139998));
#50646=CARTESIAN_POINT('Ctrl Pts',(0.964373850166081,-1.,3.62652618145252));
#50647=CARTESIAN_POINT('Ctrl Pts',(0.963957782642589,-1.,3.62489305727516));
#50648=CARTESIAN_POINT('Ctrl Pts',(0.963861297423578,-1.,3.62424461507455));
#50649=CARTESIAN_POINT('Ctrl Pts',(0.963880158556713,-1.,3.62404828878374));
#50650=CARTESIAN_POINT('Ctrl Pts',(0.963899035118985,-1.,3.62400312501199));
#50651=CARTESIAN_POINT('',(0.786422660833742,-1.,3.66661143271648));
#50652=CARTESIAN_POINT('Origin',(0.,-1.,0.));
#50653=CARTESIAN_POINT('',(0.732042837400619,-1.,4.13571194405636));
#50654=CARTESIAN_POINT('Ctrl Pts',(0.786422660833742,-1.,3.66661143271648));
#50655=CARTESIAN_POINT('Ctrl Pts',(0.786459983896781,-1.,3.66664310415236));
#50656=CARTESIAN_POINT('Ctrl Pts',(0.786565919559889,-1.,3.66680946938396));
#50657=CARTESIAN_POINT('Ctrl Pts',(0.786774337198499,-1.,3.66743103898844));
#50658=CARTESIAN_POINT('Ctrl Pts',(0.787145041181588,-1.,3.66907505398769));
#50659=CARTESIAN_POINT('Ctrl Pts',(0.787758799995426,-1.,3.672529236635));
#50660=CARTESIAN_POINT('Ctrl Pts',(0.788569566220662,-1.,3.67777119516438));
#50661=CARTESIAN_POINT('Ctrl Pts',(0.789483546065158,-1.,3.68428439784285));
#50662=CARTESIAN_POINT('Ctrl Pts',(0.790436284989579,-1.,3.69172044327754));
#50663=CARTESIAN_POINT('Ctrl Pts',(0.791356575696508,-1.,3.69968940808982));
#50664=CARTESIAN_POINT('Ctrl Pts',(0.792177688845967,-1.,3.70781724021879));
#50665=CARTESIAN_POINT('Ctrl Pts',(0.792848377370115,-1.,3.7158024239604));
#50666=CARTESIAN_POINT('Ctrl Pts',(0.79334702378387,-1.,3.7234879729357));
#50667=CARTESIAN_POINT('Ctrl Pts',(0.793682750269347,-1.,3.7308691469564));
#50668=CARTESIAN_POINT('Ctrl Pts',(0.79388270093679,-1.,3.73803280541576));
#50669=CARTESIAN_POINT('Ctrl Pts',(0.79398270045988,-1.,3.74511357728827));
#50670=CARTESIAN_POINT('Ctrl Pts',(0.79401734737144,-1.,3.75224692493895));
#50671=CARTESIAN_POINT('Ctrl Pts',(0.794008429135046,-1.,3.75951468666325));
#50672=CARTESIAN_POINT('Ctrl Pts',(0.793961083689141,-1.,3.76692626931184));
#50673=CARTESIAN_POINT('Ctrl Pts',(0.793870523787515,-1.,3.77444863801264));
#50674=CARTESIAN_POINT('Ctrl Pts',(0.793726235781339,-1.,3.78202460377617));
#50675=CARTESIAN_POINT('Ctrl Pts',(0.793516871680965,-1.,3.78959439439222));
#50676=CARTESIAN_POINT('Ctrl Pts',(0.7932356129732,-1.,3.79711921389862));
#50677=CARTESIAN_POINT('Ctrl Pts',(0.792882695234692,-1.,3.80459229925598));
#50678=CARTESIAN_POINT('Ctrl Pts',(0.792462483517568,-1.,3.81202588694726));
#50679=CARTESIAN_POINT('Ctrl Pts',(0.791981740718606,-1.,3.81944345442237));
#50680=CARTESIAN_POINT('Ctrl Pts',(0.791447528662381,-1.,3.82687033899799));
#50681=CARTESIAN_POINT('Ctrl Pts',(0.790865012705339,-1.,3.83432392054804));
#50682=CARTESIAN_POINT('Ctrl Pts',(0.790236124191289,-1.,3.84180762342476));
#50683=CARTESIAN_POINT('Ctrl Pts',(0.789560798155618,-1.,3.8493163780891));
#50684=CARTESIAN_POINT('Ctrl Pts',(0.788837734090688,-1.,3.85683995872536));
#50685=CARTESIAN_POINT('Ctrl Pts',(0.78806531509377,-1.,3.86436702561342));
#50686=CARTESIAN_POINT('Ctrl Pts',(0.78724252761798,-1.,3.87188916600905));
#50687=CARTESIAN_POINT('Ctrl Pts',(0.786369675812591,-1.,3.87940402818186));
#50688=CARTESIAN_POINT('Ctrl Pts',(0.785447890340723,-1.,3.88691313167399));
#50689=CARTESIAN_POINT('Ctrl Pts',(0.784478799358335,-1.,3.89442039235105));
#50690=CARTESIAN_POINT('Ctrl Pts',(0.783464141529082,-1.,3.90193039043971));
#50691=CARTESIAN_POINT('Ctrl Pts',(0.782405395622758,-1.,3.90944671004536));
#50692=CARTESIAN_POINT('Ctrl Pts',(0.781303428618343,-1.,3.9169703605466));
#50693=CARTESIAN_POINT('Ctrl Pts',(0.780158678615506,-1.,3.92450058323799));
#50694=CARTESIAN_POINT('Ctrl Pts',(0.778971308134786,-1.,3.93203552473153));
#50695=CARTESIAN_POINT('Ctrl Pts',(0.777741370568549,-1.,3.93957296768098));
#50696=CARTESIAN_POINT('Ctrl Pts',(0.776468966697959,-1.,3.94711101619471));
#50697=CARTESIAN_POINT('Ctrl Pts',(0.775154418039441,-1.,3.95464885452364));
#50698=CARTESIAN_POINT('Ctrl Pts',(0.773798212026682,-1.,3.96218649639876));
#50699=CARTESIAN_POINT('Ctrl Pts',(0.772400931772238,-1.,3.96972446532832));
#50700=CARTESIAN_POINT('Ctrl Pts',(0.770963190030503,-1.,3.97726349165507));
#50701=CARTESIAN_POINT('Ctrl Pts',(0.769485566245459,-1.,3.98480422348403));
#50702=CARTESIAN_POINT('Ctrl Pts',(0.767968531377707,-1.,3.99234687880892));
#50703=CARTESIAN_POINT('Ctrl Pts',(0.766412457135785,-1.,3.99989129179464));
#50704=CARTESIAN_POINT('Ctrl Pts',(0.764817648784946,-1.,4.00743706791366));
#50705=CARTESIAN_POINT('Ctrl Pts',(0.763184371182826,-1.,4.01498370680434));
#50706=CARTESIAN_POINT('Ctrl Pts',(0.761512875859941,-1.,4.02253072741347));
#50707=CARTESIAN_POINT('Ctrl Pts',(0.759803433244165,-1.,4.0300778195465));
#50708=CARTESIAN_POINT('Ctrl Pts',(0.758056338885553,-1.,4.03762485803468));
#50709=CARTESIAN_POINT('Ctrl Pts',(0.756271902370186,-1.,4.04517182654344));
#50710=CARTESIAN_POINT('Ctrl Pts',(0.754450441816411,-1.,4.05271876688106));
#50711=CARTESIAN_POINT('Ctrl Pts',(0.752592276482868,-1.,4.06026572221399));
#50712=CARTESIAN_POINT('Ctrl Pts',(0.750697720483175,-1.,4.06781267241886));
#50713=CARTESIAN_POINT('Ctrl Pts',(0.748767076679176,-1.,4.07535951055363));
#50714=CARTESIAN_POINT('Ctrl Pts',(0.746800631490821,-1.,4.08290608094789));
#50715=CARTESIAN_POINT('Ctrl Pts',(0.744798649705513,-1.,4.09045220253011));
#50716=CARTESIAN_POINT('Ctrl Pts',(0.742761369690017,-1.,4.09799769702712));
#50717=CARTESIAN_POINT('Ctrl Pts',(0.740688998555151,-1.,4.1055424175856));
#50718=CARTESIAN_POINT('Ctrl Pts',(0.738581708229118,-1.,4.11308626953795));
#50719=CARTESIAN_POINT('Ctrl Pts',(0.736439634335347,-1.,4.12062919626082));
#50720=CARTESIAN_POINT('Ctrl Pts',(0.734698226767512,-1.,4.12666277572794));
#50721=CARTESIAN_POINT('Ctrl Pts',(0.733376589325634,-1.,4.13118752796397));
#50722=CARTESIAN_POINT('Ctrl Pts',(0.732488575135925,-1.,4.13420383737278));
#50723=CARTESIAN_POINT('Ctrl Pts',(0.732042837400619,-1.,4.13571194405636));
#50724=CARTESIAN_POINT('',(0.581791163835814,-1.,4.15950947128175));
#50725=CARTESIAN_POINT('',(0.732042837400619,-1.,4.13571194405636));
#50726=CARTESIAN_POINT('',(0.385112848332549,-1.,3.73017266276632));
#50727=CARTESIAN_POINT('Ctrl Pts',(0.581791163835814,-1.,4.15950947128175));
#50728=CARTESIAN_POINT('Ctrl Pts',(0.580901211462913,-1.,4.15821291712391));
#50729=CARTESIAN_POINT('Ctrl Pts',(0.579124568912543,-1.,4.15561864787379));
#50730=CARTESIAN_POINT('Ctrl Pts',(0.576469391673916,-1.,4.1517237611974));
#50731=CARTESIAN_POINT('Ctrl Pts',(0.572948736066276,-1.,4.14652361065787));
#50732=CARTESIAN_POINT('Ctrl Pts',(0.568580610187115,-1.,4.14001179828669));
#50733=CARTESIAN_POINT('Ctrl Pts',(0.564245279535705,-1.,4.13348835726086));
#50734=CARTESIAN_POINT('Ctrl Pts',(0.559942890594628,-1.,4.12695329951859));
#50735=CARTESIAN_POINT('Ctrl Pts',(0.555673636130778,-1.,4.1204066619623));
#50736=CARTESIAN_POINT('Ctrl Pts',(0.551437758498246,-1.,4.11384852025578));
#50737=CARTESIAN_POINT('Ctrl Pts',(0.547235539486759,-1.,4.1072789702877));
#50738=CARTESIAN_POINT('Ctrl Pts',(0.543067286878457,-1.,4.10069810244473));
#50739=CARTESIAN_POINT('Ctrl Pts',(0.53893332117992,-1.,4.09410597627116));
#50740=CARTESIAN_POINT('Ctrl Pts',(0.534833963476999,-1.,4.08750259988693));
#50741=CARTESIAN_POINT('Ctrl Pts',(0.530769518728075,-1.,4.08088789536488));
#50742=CARTESIAN_POINT('Ctrl Pts',(0.526740277226999,-1.,4.07426172299496));
#50743=CARTESIAN_POINT('Ctrl Pts',(0.522746528602767,-1.,4.06762394471075));
#50744=CARTESIAN_POINT('Ctrl Pts',(0.518788572336809,-1.,4.06097448037934));
#50745=CARTESIAN_POINT('Ctrl Pts',(0.514866728193103,-1.,4.05431335771261));
#50746=CARTESIAN_POINT('Ctrl Pts',(0.510981349219173,-1.,4.04764078815591));
#50747=CARTESIAN_POINT('Ctrl Pts',(0.507132823288361,-1.,4.04095715149074));
#50748=CARTESIAN_POINT('Ctrl Pts',(0.503321556915513,-1.,4.0342628417439));
#50749=CARTESIAN_POINT('Ctrl Pts',(0.499547962340889,-1.,4.0275581398015));
#50750=CARTESIAN_POINT('Ctrl Pts',(0.495812444326222,-1.,4.02084308851813));
#50751=CARTESIAN_POINT('Ctrl Pts',(0.49211538341793,-1.,4.01411733503486));
#50752=CARTESIAN_POINT('Ctrl Pts',(0.48845713042453,-1.,4.0073800839092));
#50753=CARTESIAN_POINT('Ctrl Pts',(0.484838042421754,-1.,4.00063045119234));
#50754=CARTESIAN_POINT('Ctrl Pts',(0.481258512209637,-1.,3.99386775880655));
#50755=CARTESIAN_POINT('Ctrl Pts',(0.477718999122033,-1.,3.98709184306743));
#50756=CARTESIAN_POINT('Ctrl Pts',(0.474220061019542,-1.,3.9803033804443));
#50757=CARTESIAN_POINT('Ctrl Pts',(0.470762379613477,-1.,3.97350414289415));
#50758=CARTESIAN_POINT('Ctrl Pts',(0.467346690880671,-1.,3.96669622273946));
#50759=CARTESIAN_POINT('Ctrl Pts',(0.463973722115744,-1.,3.95988133243543));
#50760=CARTESIAN_POINT('Ctrl Pts',(0.460644124429119,-1.,3.95306005817363));
#50761=CARTESIAN_POINT('Ctrl Pts',(0.457358410451673,-1.,3.94623117206675));
#50762=CARTESIAN_POINT('Ctrl Pts',(0.454116879027575,-1.,3.93939080846298));
#50763=CARTESIAN_POINT('Ctrl Pts',(0.450919768356346,-1.,3.93253407403128));
#50764=CARTESIAN_POINT('Ctrl Pts',(0.447767416837296,-1.,3.92565674143424));
#50765=CARTESIAN_POINT('Ctrl Pts',(0.444660430230592,-1.,3.91875701610721));
#50766=CARTESIAN_POINT('Ctrl Pts',(0.441599824524047,-1.,3.91183704069146));
#50767=CARTESIAN_POINT('Ctrl Pts',(0.438587235458233,-1.,3.90490512938546));
#50768=CARTESIAN_POINT('Ctrl Pts',(0.435624629433505,-1.,3.8979725665544));
#50769=CARTESIAN_POINT('Ctrl Pts',(0.432713929544439,-1.,3.89104947940592));
#50770=CARTESIAN_POINT('Ctrl Pts',(0.429856640579733,-1.,3.88414070943334));
#50771=CARTESIAN_POINT('Ctrl Pts',(0.427053541173469,-1.,3.87724240306609));
#50772=CARTESIAN_POINT('Ctrl Pts',(0.424304173195142,-1.,3.87033643487882));
#50773=CARTESIAN_POINT('Ctrl Pts',(0.421607423177575,-1.,3.86339652542749));
#50774=CARTESIAN_POINT('Ctrl Pts',(0.418962468086809,-1.,3.85639825648031));
#50775=CARTESIAN_POINT('Ctrl Pts',(0.41636967805292,-1.,3.8493286415751));
#50776=CARTESIAN_POINT('Ctrl Pts',(0.413831367016726,-1.,3.84219403994742));
#50777=CARTESIAN_POINT('Ctrl Pts',(0.411353038798459,-1.,3.83503345578645));
#50778=CARTESIAN_POINT('Ctrl Pts',(0.408942371447376,-1.,3.82790724256397));
#50779=CARTESIAN_POINT('Ctrl Pts',(0.406607038258906,-1.,3.82087303913741));
#50780=CARTESIAN_POINT('Ctrl Pts',(0.404352694628236,-1.,3.81396374287762));
#50781=CARTESIAN_POINT('Ctrl Pts',(0.402181320148474,-1.,3.80716881962763));
#50782=CARTESIAN_POINT('Ctrl Pts',(0.400088346504726,-1.,3.80040370384659));
#50783=CARTESIAN_POINT('Ctrl Pts',(0.398064818684158,-1.,3.79352887163457));
#50784=CARTESIAN_POINT('Ctrl Pts',(0.396103205335028,-1.,3.78640521279479));
#50785=CARTESIAN_POINT('Ctrl Pts',(0.394202481011595,-1.,3.77894173114368));
#50786=CARTESIAN_POINT('Ctrl Pts',(0.392372786223346,-1.,3.77114011595892));
#50787=CARTESIAN_POINT('Ctrl Pts',(0.390642072979258,-1.,3.76315635032993));
#50788=CARTESIAN_POINT('Ctrl Pts',(0.38905477589825,-1.,3.75529302894757));
#50789=CARTESIAN_POINT('Ctrl Pts',(0.387663020050396,-1.,3.74792651696269));
#50790=CARTESIAN_POINT('Ctrl Pts',(0.386519576222035,-1.,3.74144965781088));
#50791=CARTESIAN_POINT('Ctrl Pts',(0.385670806454744,-1.,3.73621371845475));
#50792=CARTESIAN_POINT('Ctrl Pts',(0.385187124633964,-1.,3.73273893363318));
#50793=CARTESIAN_POINT('Ctrl Pts',(0.385031656499141,-1.,3.73106082862399));
#50794=CARTESIAN_POINT('Ctrl Pts',(0.385037797882046,-1.,3.73040527620929));
#50795=CARTESIAN_POINT('Ctrl Pts',(0.385087139001608,-1.,3.73021431755218));
#50796=CARTESIAN_POINT('Ctrl Pts',(0.385112848332549,-1.,3.73017266276632));
#50797=CARTESIAN_POINT('',(0.203156094897895,-1.,3.74449296982994));
#50798=CARTESIAN_POINT('Origin',(0.,-1.,0.));
#50799=CARTESIAN_POINT('',(0.0760622897878233,-1.,4.19931119685982));
#50800=CARTESIAN_POINT('Ctrl Pts',(0.203156094897895,-1.,3.74449296982994));
#50801=CARTESIAN_POINT('Ctrl Pts',(0.203188003947964,-1.,3.74453008995129));
#50802=CARTESIAN_POINT('Ctrl Pts',(0.203266610111263,-1.,3.74471097893961));
#50803=CARTESIAN_POINT('Ctrl Pts',(0.203375226874331,-1.,3.74535749969262));
#50804=CARTESIAN_POINT('Ctrl Pts',(0.203484186269314,-1.,3.74703926501843));
#50805=CARTESIAN_POINT('Ctrl Pts',(0.203550035479096,-1.,3.75054693397716));
#50806=CARTESIAN_POINT('Ctrl Pts',(0.203530796848403,-1.,3.75585118707924));
#50807=CARTESIAN_POINT('Ctrl Pts',(0.203414634707646,-1.,3.76242717937273));
#50808=CARTESIAN_POINT('Ctrl Pts',(0.203192390045337,-1.,3.76992071595267));
#50809=CARTESIAN_POINT('Ctrl Pts',(0.202854729699196,-1.,3.77793553476879));
#50810=CARTESIAN_POINT('Ctrl Pts',(0.202394260512192,-1.,3.78609175019317));
#50811=CARTESIAN_POINT('Ctrl Pts',(0.201807533800798,-1.,3.79408354187274));
#50812=CARTESIAN_POINT('Ctrl Pts',(0.201097756307251,-1.,3.80175247447171));
#50813=CARTESIAN_POINT('Ctrl Pts',(0.200274679433289,-1.,3.80909529318501));
#50814=CARTESIAN_POINT('Ctrl Pts',(0.199351525297396,-1.,3.81620203429702));
#50815=CARTESIAN_POINT('Ctrl Pts',(0.198342616900469,-1.,3.82321127348981));
#50816=CARTESIAN_POINT('Ctrl Pts',(0.197260935827375,-1.,3.83026221776488));
#50817=CARTESIAN_POINT('Ctrl Pts',(0.196115198971889,-1.,3.83743910616265));
#50818=CARTESIAN_POINT('Ctrl Pts',(0.194909009460254,-1.,3.84475203347052));
#50819=CARTESIAN_POINT('Ctrl Pts',(0.193642806777747,-1.,3.85216762264019));
#50820=CARTESIAN_POINT('Ctrl Pts',(0.192315153044979,-1.,3.85962774407652));
#50821=CARTESIAN_POINT('Ctrl Pts',(0.190924190418612,-1.,3.8670715862477));
#50822=CARTESIAN_POINT('Ctrl Pts',(0.189469253358254,-1.,3.87445976418377));
#50823=CARTESIAN_POINT('Ctrl Pts',(0.187951632512663,-1.,3.88178563496187));
#50824=CARTESIAN_POINT('Ctrl Pts',(0.186373724985263,-1.,3.88906196725817));
#50825=CARTESIAN_POINT('Ctrl Pts',(0.184738537728034,-1.,3.89631300742633));
#50826=CARTESIAN_POINT('Ctrl Pts',(0.183049081993193,-1.,3.90356488555138));
#50827=CARTESIAN_POINT('Ctrl Pts',(0.181307740731795,-1.,3.91083557557193));
#50828=CARTESIAN_POINT('Ctrl Pts',(0.179515885822894,-1.,3.91812876180948));
#50829=CARTESIAN_POINT('Ctrl Pts',(0.177674246152328,-1.,3.92543942697672));
#50830=CARTESIAN_POINT('Ctrl Pts',(0.175783136893872,-1.,3.93275726771049));
#50831=CARTESIAN_POINT('Ctrl Pts',(0.173842734974607,-1.,3.94007083096214));
#50832=CARTESIAN_POINT('Ctrl Pts',(0.171853355369232,-1.,3.94737164900861));
#50833=CARTESIAN_POINT('Ctrl Pts',(0.16981566637413,-1.,3.95465744665263));
#50834=CARTESIAN_POINT('Ctrl Pts',(0.167730547023312,-1.,3.96192990160296));
#50835=CARTESIAN_POINT('Ctrl Pts',(0.165598992851097,-1.,3.9691931362141));
#50836=CARTESIAN_POINT('Ctrl Pts',(0.163422004609998,-1.,3.97645194630944));
#50837=CARTESIAN_POINT('Ctrl Pts',(0.161200482186087,-1.,3.98371010319866));
#50838=CARTESIAN_POINT('Ctrl Pts',(0.158935123982796,-1.,3.99096873945862));
#50839=CARTESIAN_POINT('Ctrl Pts',(0.156626481393735,-1.,3.99822717425869));
#50840=CARTESIAN_POINT('Ctrl Pts',(0.154275004872309,-1.,4.00548360245297));
#50841=CARTESIAN_POINT('Ctrl Pts',(0.151881094022909,-1.,4.01273584234684));
#50842=CARTESIAN_POINT('Ctrl Pts',(0.149445144968707,-1.,4.01998203715588));
#50843=CARTESIAN_POINT('Ctrl Pts',(0.146967602878998,-1.,4.02722143147048));
#50844=CARTESIAN_POINT('Ctrl Pts',(0.144448947038352,-1.,4.03445411510403));
#50845=CARTESIAN_POINT('Ctrl Pts',(0.141889671485507,-1.,4.04168069633842));
#50846=CARTESIAN_POINT('Ctrl Pts',(0.139290267180059,-1.,4.04890199238056));
#50847=CARTESIAN_POINT('Ctrl Pts',(0.136651205046111,-1.,4.05611873400122));
#50848=CARTESIAN_POINT('Ctrl Pts',(0.133972916144225,-1.,4.06333121018476));
#50849=CARTESIAN_POINT('Ctrl Pts',(0.131255793548914,-1.,4.07053931528579));
#50850=CARTESIAN_POINT('Ctrl Pts',(0.128500200484813,-1.,4.07774270738809));
#50851=CARTESIAN_POINT('Ctrl Pts',(0.125706476822529,-1.,4.08494093372315));
#50852=CARTESIAN_POINT('Ctrl Pts',(0.122874946249119,-1.,4.09213355850836));
#50853=CARTESIAN_POINT('Ctrl Pts',(0.120005924388162,-1.,4.09932031767243));
#50854=CARTESIAN_POINT('Ctrl Pts',(0.117099722731704,-1.,4.10650113382187));
#50855=CARTESIAN_POINT('Ctrl Pts',(0.114156649609601,-1.,4.11367603925313));
#50856=CARTESIAN_POINT('Ctrl Pts',(0.111177012683377,-1.,4.12084512502444));
#50857=CARTESIAN_POINT('Ctrl Pts',(0.10816112052835,-1.,4.12800848371386));
#50858=CARTESIAN_POINT('Ctrl Pts',(0.105109286538864,-1.,4.13516614458396));
#50859=CARTESIAN_POINT('Ctrl Pts',(0.102021826577453,-1.,4.14231804938737));
#50860=CARTESIAN_POINT('Ctrl Pts',(0.0988990478899809,-1.,4.1494640891762));
#50861=CARTESIAN_POINT('Ctrl Pts',(0.0957412403297065,-1.,4.15660412653006));
#50862=CARTESIAN_POINT('Ctrl Pts',(0.0925486672167687,-1.,4.16373802265942));
#50863=CARTESIAN_POINT('Ctrl Pts',(0.0893215560850325,-1.,4.17086566491823));
#50864=CARTESIAN_POINT('Ctrl Pts',(0.0860600915552512,-1.,4.17798698669991));
#50865=CARTESIAN_POINT('Ctrl Pts',(0.0827644164389507,-1.,4.1851019532944));
#50866=CARTESIAN_POINT('Ctrl Pts',(0.08010058871176,-1.,4.19078883322483));
#50867=CARTESIAN_POINT('Ctrl Pts',(0.0780873956244399,-1.,4.19505112860624));
#50868=CARTESIAN_POINT('Ctrl Pts',(0.0767384596142192,-1.,4.19789138621624));
#50869=CARTESIAN_POINT('Ctrl Pts',(0.0760622897878233,-1.,4.19931119685982));
#50870=CARTESIAN_POINT('',(-0.0760622897878249,-1.,4.19931119685982));
#50871=CARTESIAN_POINT('',(0.0760622897878233,-1.,4.19931119685982));
#50872=CARTESIAN_POINT('',(-0.203156094896101,-1.,3.74449296983004));
#50873=CARTESIAN_POINT('Ctrl Pts',(-0.0760622897878249,-1.,4.19931119685982));
#50874=CARTESIAN_POINT('Ctrl Pts',(-0.0767384596141467,-1.,4.1978913862118));
#50875=CARTESIAN_POINT('Ctrl Pts',(-0.07808739562424,-1.,4.19505112859416));
#50876=CARTESIAN_POINT('Ctrl Pts',(-0.0801005887114322,-1.,4.19078883320504));
#50877=CARTESIAN_POINT('Ctrl Pts',(-0.0827644164385681,-1.,4.18510195327123));
#50878=CARTESIAN_POINT('Ctrl Pts',(-0.0860600915549399,-1.,4.17798698668094));
#50879=CARTESIAN_POINT('Ctrl Pts',(-0.0893215560848652,-1.,4.17086566490794));
#50880=CARTESIAN_POINT('Ctrl Pts',(-0.0925486672167534,-1.,4.16373802265839));
#50881=CARTESIAN_POINT('Ctrl Pts',(-0.0957412403298009,-1.,4.15660412653577));
#50882=CARTESIAN_POINT('Ctrl Pts',(-0.0988990478901228,-1.,4.14946408918485));
#50883=CARTESIAN_POINT('Ctrl Pts',(-0.102021826577584,-1.,4.14231804939538));
#50884=CARTESIAN_POINT('Ctrl Pts',(-0.105109286538945,-1.,4.13516614458895));
#50885=CARTESIAN_POINT('Ctrl Pts',(-0.10816112052837,-1.,4.12800848371504));
#50886=CARTESIAN_POINT('Ctrl Pts',(-0.111177012683347,-1.,4.1208451250225));
#50887=CARTESIAN_POINT('Ctrl Pts',(-0.114156649609546,-1.,4.11367603924961));
#50888=CARTESIAN_POINT('Ctrl Pts',(-0.117099722731648,-1.,4.10650113381833));
#50889=CARTESIAN_POINT('Ctrl Pts',(-0.120005924388124,-1.,4.09932031767002));
#50890=CARTESIAN_POINT('Ctrl Pts',(-0.122874946249107,-1.,4.09213355850756));
#50891=CARTESIAN_POINT('Ctrl Pts',(-0.12570647682254,-1.,4.08494093372377));
#50892=CARTESIAN_POINT('Ctrl Pts',(-0.128500200484838,-1.,4.07774270738954));
#50893=CARTESIAN_POINT('Ctrl Pts',(-0.131255793548941,-1.,4.0705393152874));
#50894=CARTESIAN_POINT('Ctrl Pts',(-0.133972916144245,-1.,4.06333121018596));
#50895=CARTESIAN_POINT('Ctrl Pts',(-0.136651205046119,-1.,4.05611873400172));
#50896=CARTESIAN_POINT('Ctrl Pts',(-0.139290267180057,-1.,4.04890199238036));
#50897=CARTESIAN_POINT('Ctrl Pts',(-0.1418896714855,-1.,4.04168069633781));
#50898=CARTESIAN_POINT('Ctrl Pts',(-0.144448947038345,-1.,4.03445411510333));
#50899=CARTESIAN_POINT('Ctrl Pts',(-0.146967602878994,-1.,4.02722143146994));
#50900=CARTESIAN_POINT('Ctrl Pts',(-0.149445144968707,-1.,4.01998203715564));
#50901=CARTESIAN_POINT('Ctrl Pts',(-0.151881094022911,-1.,4.01273584234689));
#50902=CARTESIAN_POINT('Ctrl Pts',(-0.154275004872311,-1.,4.00548360245319));
#50903=CARTESIAN_POINT('Ctrl Pts',(-0.156626481393734,-1.,3.99822717425893));
#50904=CARTESIAN_POINT('Ctrl Pts',(-0.158935123982793,-1.,3.99096873945878));
#50905=CARTESIAN_POINT('Ctrl Pts',(-0.161200482186085,-1.,3.98371010319872));
#50906=CARTESIAN_POINT('Ctrl Pts',(-0.163422004609999,-1.,3.97645194630943));
#50907=CARTESIAN_POINT('Ctrl Pts',(-0.165598992851102,-1.,3.96919313621407));
#50908=CARTESIAN_POINT('Ctrl Pts',(-0.16773054702332,-1.,3.96192990160296));
#50909=CARTESIAN_POINT('Ctrl Pts',(-0.169815666374139,-1.,3.95465744665268));
#50910=CARTESIAN_POINT('Ctrl Pts',(-0.17185335536924,-1.,3.94737164900868));
#50911=CARTESIAN_POINT('Ctrl Pts',(-0.17384273497461,-1.,3.94007083096217));
#50912=CARTESIAN_POINT('Ctrl Pts',(-0.175783136893868,-1.,3.93275726771042));
#50913=CARTESIAN_POINT('Ctrl Pts',(-0.177674246152318,-1.,3.92543942697655));
#50914=CARTESIAN_POINT('Ctrl Pts',(-0.179515885822882,-1.,3.91812876180926));
#50915=CARTESIAN_POINT('Ctrl Pts',(-0.181307740731786,-1.,3.91083557557175));
#50916=CARTESIAN_POINT('Ctrl Pts',(-0.183049081993191,-1.,3.90356488555132));
#50917=CARTESIAN_POINT('Ctrl Pts',(-0.184738537728043,-1.,3.89631300742646));
#50918=CARTESIAN_POINT('Ctrl Pts',(-0.186373724985281,-1.,3.88906196725848));
#50919=CARTESIAN_POINT('Ctrl Pts',(-0.187951632512685,-1.,3.88178563496228));
#50920=CARTESIAN_POINT('Ctrl Pts',(-0.189469253358273,-1.,3.87445976418412));
#50921=CARTESIAN_POINT('Ctrl Pts',(-0.19092419041862,-1.,3.86707158624783));
#50922=CARTESIAN_POINT('Ctrl Pts',(-0.192315153044971,-1.,3.85962774407633));
#50923=CARTESIAN_POINT('Ctrl Pts',(-0.193642806777723,-1.,3.85216762263966));
#50924=CARTESIAN_POINT('Ctrl Pts',(-0.194909009460221,-1.,3.84475203346977));
#50925=CARTESIAN_POINT('Ctrl Pts',(-0.196115198971859,-1.,3.83743910616195));
#50926=CARTESIAN_POINT('Ctrl Pts',(-0.197260935827362,-1.,3.83026221776456));
#50927=CARTESIAN_POINT('Ctrl Pts',(-0.198342616900487,-1.,3.82321127349016));
#50928=CARTESIAN_POINT('Ctrl Pts',(-0.199351525297447,-1.,3.81620203429815));
#50929=CARTESIAN_POINT('Ctrl Pts',(-0.200274679433365,-1.,3.80909529318669));
#50930=CARTESIAN_POINT('Ctrl Pts',(-0.201097756307326,-1.,3.80175247447337));
#50931=CARTESIAN_POINT('Ctrl Pts',(-0.201807533800837,-1.,3.7940835418736));
#50932=CARTESIAN_POINT('Ctrl Pts',(-0.20239426051216,-1.,3.78609175019242));
#50933=CARTESIAN_POINT('Ctrl Pts',(-0.202854729699081,-1.,3.77793553476614));
#50934=CARTESIAN_POINT('Ctrl Pts',(-0.203192390045165,-1.,3.7699207159487));
#50935=CARTESIAN_POINT('Ctrl Pts',(-0.203414634707479,-1.,3.76242717936885));
#50936=CARTESIAN_POINT('Ctrl Pts',(-0.203530796848322,-1.,3.75585118707734));
#50937=CARTESIAN_POINT('Ctrl Pts',(-0.203550035479166,-1.,3.75054693397875));
#50938=CARTESIAN_POINT('Ctrl Pts',(-0.203484186269415,-1.,3.74703926501752));
#50939=CARTESIAN_POINT('Ctrl Pts',(-0.203375226874122,-1.,3.74535749969115));
#50940=CARTESIAN_POINT('Ctrl Pts',(-0.203266610110531,-1.,3.74471097893845));
#50941=CARTESIAN_POINT('Ctrl Pts',(-0.203188003946657,-1.,3.74453008995092));
#50942=CARTESIAN_POINT('Ctrl Pts',(-0.203156094896101,-1.,3.74449296983004));
#50943=CARTESIAN_POINT('',(-0.385112848330762,-1.,3.73017266276651));
#50944=CARTESIAN_POINT('Origin',(0.,-1.,0.));
#50945=CARTESIAN_POINT('',(-0.581791163835815,-1.,4.15950947128175));
#50946=CARTESIAN_POINT('Ctrl Pts',(-0.385112848330762,-1.,3.73017266276651));
#50947=CARTESIAN_POINT('Ctrl Pts',(-0.385087139000375,-1.,3.73021431755274));
#50948=CARTESIAN_POINT('Ctrl Pts',(-0.385037797881504,-1.,3.73040527621055));
#50949=CARTESIAN_POINT('Ctrl Pts',(-0.385031656499164,-1.,3.73106082862548));
#50950=CARTESIAN_POINT('Ctrl Pts',(-0.385187124634206,-1.,3.73273893363406));
#50951=CARTESIAN_POINT('Ctrl Pts',(-0.385670806454566,-1.,3.73621371845318));
#50952=CARTESIAN_POINT('Ctrl Pts',(-0.386519576222251,-1.,3.74144965781276));
#50953=CARTESIAN_POINT('Ctrl Pts',(-0.387663020050836,-1.,3.74792651696654));
#50954=CARTESIAN_POINT('Ctrl Pts',(-0.389054775898702,-1.,3.75529302895152));
#50955=CARTESIAN_POINT('Ctrl Pts',(-0.39064207297956,-1.,3.76315635033257));
#50956=CARTESIAN_POINT('Ctrl Pts',(-0.392372786223433,-1.,3.77114011595967));
#50957=CARTESIAN_POINT('Ctrl Pts',(-0.394202481011499,-1.,3.77894173114283));
#50958=CARTESIAN_POINT('Ctrl Pts',(-0.396103205334841,-1.,3.78640521279313));
#50959=CARTESIAN_POINT('Ctrl Pts',(-0.39806481868397,-1.,3.7935288716329));
#50960=CARTESIAN_POINT('Ctrl Pts',(-0.4000883465046,-1.,3.80040370384546));
#50961=CARTESIAN_POINT('Ctrl Pts',(-0.402181320148436,-1.,3.80716881962728));
#50962=CARTESIAN_POINT('Ctrl Pts',(-0.404352694628273,-1.,3.81396374287793));
#50963=CARTESIAN_POINT('Ctrl Pts',(-0.406607038258985,-1.,3.8208730391381));
#50964=CARTESIAN_POINT('Ctrl Pts',(-0.40894237144746,-1.,3.82790724256471));
#50965=CARTESIAN_POINT('Ctrl Pts',(-0.411353038798519,-1.,3.83503345578698));
#50966=CARTESIAN_POINT('Ctrl Pts',(-0.413831367016748,-1.,3.84219403994762));
#50967=CARTESIAN_POINT('Ctrl Pts',(-0.416369678052907,-1.,3.84932864157497));
#50968=CARTESIAN_POINT('Ctrl Pts',(-0.418962468086773,-1.,3.85639825647996));
#50969=CARTESIAN_POINT('Ctrl Pts',(-0.421607423177534,-1.,3.86339652542709));
#50970=CARTESIAN_POINT('Ctrl Pts',(-0.424304173195111,-1.,3.87033643487851));
#50971=CARTESIAN_POINT('Ctrl Pts',(-0.427053541173457,-1.,3.87724240306597));
#50972=CARTESIAN_POINT('Ctrl Pts',(-0.429856640579741,-1.,3.88414070943341));
#50973=CARTESIAN_POINT('Ctrl Pts',(-0.432713929544458,-1.,3.89104947940611));
#50974=CARTESIAN_POINT('Ctrl Pts',(-0.435624629433528,-1.,3.89797256655462));
#50975=CARTESIAN_POINT('Ctrl Pts',(-0.43858723545825,-1.,3.90490512938563));
#50976=CARTESIAN_POINT('Ctrl Pts',(-0.441599824524054,-1.,3.91183704069153));
#50977=CARTESIAN_POINT('Ctrl Pts',(-0.444660430230591,-1.,3.91875701610719));
#50978=CARTESIAN_POINT('Ctrl Pts',(-0.447767416837293,-1.,3.92565674143416));
#50979=CARTESIAN_POINT('Ctrl Pts',(-0.450919768356348,-1.,3.93253407403123));
#50980=CARTESIAN_POINT('Ctrl Pts',(-0.454116879027584,-1.,3.93939080846298));
#50981=CARTESIAN_POINT('Ctrl Pts',(-0.457358410451683,-1.,3.94623117206678));
#50982=CARTESIAN_POINT('Ctrl Pts',(-0.460644124429121,-1.,3.95306005817364));
#50983=CARTESIAN_POINT('Ctrl Pts',(-0.463973722115733,-1.,3.95988133243538));
#50984=CARTESIAN_POINT('Ctrl Pts',(-0.467346690880643,-1.,3.9666962227393));
#50985=CARTESIAN_POINT('Ctrl Pts',(-0.470762379613439,-1.,3.97350414289392));
#50986=CARTESIAN_POINT('Ctrl Pts',(-0.47422006101951,-1.,3.98030338044409));
#50987=CARTESIAN_POINT('Ctrl Pts',(-0.477718999122027,-1.,3.98709184306738));
#50988=CARTESIAN_POINT('Ctrl Pts',(-0.481258512209675,-1.,3.99386775880679));
#50989=CARTESIAN_POINT('Ctrl Pts',(-0.484838042421835,-1.,4.00063045119288));
#50990=CARTESIAN_POINT('Ctrl Pts',(-0.488457130424633,-1.,4.0073800839099));
#50991=CARTESIAN_POINT('Ctrl Pts',(-0.492115383418018,-1.,4.01411733503546));
#50992=CARTESIAN_POINT('Ctrl Pts',(-0.495812444326251,-1.,4.02084308851832));
#50993=CARTESIAN_POINT('Ctrl Pts',(-0.499547962340821,-1.,4.02755813980101));
#50994=CARTESIAN_POINT('Ctrl Pts',(-0.503321556915346,-1.,4.03426284174272));
#50995=CARTESIAN_POINT('Ctrl Pts',(-0.507132823288136,-1.,4.04095715148915));
#50996=CARTESIAN_POINT('Ctrl Pts',(-0.51098134921897,-1.,4.04764078815447));
#50997=CARTESIAN_POINT('Ctrl Pts',(-0.514866728193017,-1.,4.05431335771199));
#50998=CARTESIAN_POINT('Ctrl Pts',(-0.518788572336924,-1.,4.06097448038013));
#50999=CARTESIAN_POINT('Ctrl Pts',(-0.522746528603107,-1.,4.06762394471314));
#51000=CARTESIAN_POINT('Ctrl Pts',(-0.526740277227498,-1.,4.07426172299847));
#51001=CARTESIAN_POINT('Ctrl Pts',(-0.530769518728571,-1.,4.08088789536836));
#51002=CARTESIAN_POINT('Ctrl Pts',(-0.534833963477273,-1.,4.08750259988885));
#51003=CARTESIAN_POINT('Ctrl Pts',(-0.538933321179756,-1.,4.09410597627));
#51004=CARTESIAN_POINT('Ctrl Pts',(-0.543067286877757,-1.,4.10069810243979));
#51005=CARTESIAN_POINT('Ctrl Pts',(-0.547235539485637,-1.,4.10727897027977));
#51006=CARTESIAN_POINT('Ctrl Pts',(-0.551437758497033,-1.,4.11384852024721));
#51007=CARTESIAN_POINT('Ctrl Pts',(-0.555673636129977,-1.,4.12040666195664));
#51008=CARTESIAN_POINT('Ctrl Pts',(-0.559942890594774,-1.,4.12695329951961));
#51009=CARTESIAN_POINT('Ctrl Pts',(-0.564245279537149,-1.,4.13348835727104));
#51010=CARTESIAN_POINT('Ctrl Pts',(-0.568580610189775,-1.,4.14001179830547));
#51011=CARTESIAN_POINT('Ctrl Pts',(-0.572948736069522,-1.,4.14652361068081));
#51012=CARTESIAN_POINT('Ctrl Pts',(-0.576469391676688,-1.,4.151723761217));
#51013=CARTESIAN_POINT('Ctrl Pts',(-0.579124568914235,-1.,4.15561864788576));
#51014=CARTESIAN_POINT('Ctrl Pts',(-0.580901211463535,-1.,4.1582129171283));
#51015=CARTESIAN_POINT('Ctrl Pts',(-0.581791163835815,-1.,4.15950947128175));
#51016=CARTESIAN_POINT('',(-0.73204283740062,-1.,4.13571194405636));
#51017=CARTESIAN_POINT('',(-0.581791163835815,-1.,4.15950947128175));
#51018=CARTESIAN_POINT('',(-0.786422660831985,-1.,3.66661143271685));
#51019=CARTESIAN_POINT('Ctrl Pts',(-0.73204283740062,-1.,4.13571194405636));
#51020=CARTESIAN_POINT('Ctrl Pts',(-0.73248857513516,-1.,4.1342038373684));
#51021=CARTESIAN_POINT('Ctrl Pts',(-0.733376589323546,-1.,4.13118752795207));
#51022=CARTESIAN_POINT('Ctrl Pts',(-0.734698226764092,-1.,4.12666277570844));
#51023=CARTESIAN_POINT('Ctrl Pts',(-0.736439634331345,-1.,4.120629196238));
#51024=CARTESIAN_POINT('Ctrl Pts',(-0.738581708225844,-1.,4.11308626951927));
#51025=CARTESIAN_POINT('Ctrl Pts',(-0.740688998553377,-1.,4.10554241757547));
#51026=CARTESIAN_POINT('Ctrl Pts',(-0.742761369689841,-1.,4.09799769702611));
#51027=CARTESIAN_POINT('Ctrl Pts',(-0.7447986497065,-1.,4.09045220253573));
#51028=CARTESIAN_POINT('Ctrl Pts',(-0.746800631492315,-1.,4.08290608095642));
#51029=CARTESIAN_POINT('Ctrl Pts',(-0.748767076680557,-1.,4.07535951056152));
#51030=CARTESIAN_POINT('Ctrl Pts',(-0.750697720484036,-1.,4.06781267242378));
#51031=CARTESIAN_POINT('Ctrl Pts',(-0.752592276483072,-1.,4.06026572221515));
#51032=CARTESIAN_POINT('Ctrl Pts',(-0.754450441816078,-1.,4.05271876687915));
#51033=CARTESIAN_POINT('Ctrl Pts',(-0.756271902369581,-1.,4.04517182653997));
#51034=CARTESIAN_POINT('Ctrl Pts',(-0.758056338884944,-1.,4.03762485803119));
#51035=CARTESIAN_POINT('Ctrl Pts',(-0.759803433243752,-1.,4.03007781954412));
#51036=CARTESIAN_POINT('Ctrl Pts',(-0.761512875859804,-1.,4.02253072741268));
#51037=CARTESIAN_POINT('Ctrl Pts',(-0.763184371182935,-1.,4.01498370680496));
#51038=CARTESIAN_POINT('Ctrl Pts',(-0.764817648785198,-1.,4.00743706791509));
#51039=CARTESIAN_POINT('Ctrl Pts',(-0.766412457136064,-1.,3.99989129179622));
#51040=CARTESIAN_POINT('Ctrl Pts',(-0.767968531377915,-1.,3.9923468788101));
#51041=CARTESIAN_POINT('Ctrl Pts',(-0.769485566245544,-1.,3.98480422348451));
#51042=CARTESIAN_POINT('Ctrl Pts',(-0.770963190030471,-1.,3.97726349165488));
#51043=CARTESIAN_POINT('Ctrl Pts',(-0.772400931772136,-1.,3.96972446532772));
#51044=CARTESIAN_POINT('Ctrl Pts',(-0.773798212026566,-1.,3.96218649639807));
#51045=CARTESIAN_POINT('Ctrl Pts',(-0.775154418039352,-1.,3.9546488545231));
#51046=CARTESIAN_POINT('Ctrl Pts',(-0.776468966697921,-1.,3.94711101619447));
#51047=CARTESIAN_POINT('Ctrl Pts',(-0.777741370568559,-1.,3.93957296768103));
#51048=CARTESIAN_POINT('Ctrl Pts',(-0.778971308134821,-1.,3.93203552473174));
#51049=CARTESIAN_POINT('Ctrl Pts',(-0.780158678615543,-1.,3.92450058323823));
#51050=CARTESIAN_POINT('Ctrl Pts',(-0.781303428618367,-1.,3.91697036054676));
#51051=CARTESIAN_POINT('Ctrl Pts',(-0.782405395622764,-1.,3.90944671004542));
#51052=CARTESIAN_POINT('Ctrl Pts',(-0.783464141529081,-1.,3.9019303904397));
#51053=CARTESIAN_POINT('Ctrl Pts',(-0.784478799358336,-1.,3.89442039235103));
#51054=CARTESIAN_POINT('Ctrl Pts',(-0.78544789034073,-1.,3.88691313167398));
#51055=CARTESIAN_POINT('Ctrl Pts',(-0.786369675812609,-1.,3.8794040281819));
#51056=CARTESIAN_POINT('Ctrl Pts',(-0.787242527617999,-1.,3.87188916600912));
#51057=CARTESIAN_POINT('Ctrl Pts',(-0.788065315093778,-1.,3.86436702561345));
#51058=CARTESIAN_POINT('Ctrl Pts',(-0.788837734090672,-1.,3.85683995872529));
#51059=CARTESIAN_POINT('Ctrl Pts',(-0.789560798155582,-1.,3.84931637808894));
#51060=CARTESIAN_POINT('Ctrl Pts',(-0.790236124191242,-1.,3.84180762342454));
#51061=CARTESIAN_POINT('Ctrl Pts',(-0.790865012705301,-1.,3.83432392054786));
#51062=CARTESIAN_POINT('Ctrl Pts',(-0.791447528662369,-1.,3.82687033899792));
#51063=CARTESIAN_POINT('Ctrl Pts',(-0.791981740718635,-1.,3.81944345442249));
#51064=CARTESIAN_POINT('Ctrl Pts',(-0.792462483517634,-1.,3.81202588694756));
#51065=CARTESIAN_POINT('Ctrl Pts',(-0.792882695234778,-1.,3.80459229925637));
#51066=CARTESIAN_POINT('Ctrl Pts',(-0.793235612973273,-1.,3.79711921389897));
#51067=CARTESIAN_POINT('Ctrl Pts',(-0.793516871680993,-1.,3.78959439439235));
#51068=CARTESIAN_POINT('Ctrl Pts',(-0.7937262357813,-1.,3.78202460377598));
#51069=CARTESIAN_POINT('Ctrl Pts',(-0.793870523787408,-1.,3.77444863801212));
#51070=CARTESIAN_POINT('Ctrl Pts',(-0.793961083688992,-1.,3.76692626931111));
#51071=CARTESIAN_POINT('Ctrl Pts',(-0.794008429134907,-1.,3.75951468666257));
#51072=CARTESIAN_POINT('Ctrl Pts',(-0.794017347371377,-1.,3.75224692493864));
#51073=CARTESIAN_POINT('Ctrl Pts',(-0.793982700459952,-1.,3.74511357728861));
#51074=CARTESIAN_POINT('Ctrl Pts',(-0.793882700937017,-1.,3.73803280541687));
#51075=CARTESIAN_POINT('Ctrl Pts',(-0.793682750269684,-1.,3.73086914695805));
#51076=CARTESIAN_POINT('Ctrl Pts',(-0.793347023784205,-1.,3.72348797293734));
#51077=CARTESIAN_POINT('Ctrl Pts',(-0.792848377370287,-1.,3.71580242396124));
#51078=CARTESIAN_POINT('Ctrl Pts',(-0.792177688845818,-1.,3.70781724021806));
#51079=CARTESIAN_POINT('Ctrl Pts',(-0.79135657569598,-1.,3.69968940808721));
#51080=CARTESIAN_POINT('Ctrl Pts',(-0.790436284988788,-1.,3.69172044327364));
#51081=CARTESIAN_POINT('Ctrl Pts',(-0.789483546064387,-1.,3.68428439783905));
#51082=CARTESIAN_POINT('Ctrl Pts',(-0.788569566220285,-1.,3.67777119516252));
#51083=CARTESIAN_POINT('Ctrl Pts',(-0.787758799995743,-1.,3.67252923663655));
#51084=CARTESIAN_POINT('Ctrl Pts',(-0.787145041181546,-1.,3.66907505398677));
#51085=CARTESIAN_POINT('Ctrl Pts',(-0.786774337198062,-1.,3.66743103898702));
#51086=CARTESIAN_POINT('Ctrl Pts',(-0.786565919558984,-1.,3.66680946938292));
#51087=CARTESIAN_POINT('Ctrl Pts',(-0.786459983895432,-1.,3.6666431041522));
#51088=CARTESIAN_POINT('Ctrl Pts',(-0.786422660831985,-1.,3.66661143271685));
#51089=CARTESIAN_POINT('',(-0.963899035117249,-1.,3.62400312501245));
#51090=CARTESIAN_POINT('Origin',(0.,-1.,0.));
#51091=CARTESIAN_POINT('',(-1.22531898815164,-1.,4.01728681790024));
#51092=CARTESIAN_POINT('Ctrl Pts',(-0.963899035117249,-1.,3.62400312501245));
#51093=CARTESIAN_POINT('Ctrl Pts',(-0.963880158555582,-1.,3.6240482887845));
#51094=CARTESIAN_POINT('Ctrl Pts',(-0.963861297423241,-1.,3.62424461507588));
#51095=CARTESIAN_POINT('Ctrl Pts',(-0.963957782642843,-1.,3.62489305727662));
#51096=CARTESIAN_POINT('Ctrl Pts',(-0.964373850166458,-1.,3.62652618145335));
#51097=CARTESIAN_POINT('Ctrl Pts',(-0.965395153165293,-1.,3.62988252139846));
#51098=CARTESIAN_POINT('Ctrl Pts',(-0.967052554541386,-1.,3.63492122081143));
#51099=CARTESIAN_POINT('Ctrl Pts',(-0.969195124675866,-1.,3.64113946505766));
#51100=CARTESIAN_POINT('Ctrl Pts',(-0.971722122061341,-1.,3.64819756447455));
#51101=CARTESIAN_POINT('Ctrl Pts',(-0.974519971354848,-1.,3.65571576735126));
#51102=CARTESIAN_POINT('Ctrl Pts',(-0.977478312751618,-1.,3.66333049637475));
#51103=CARTESIAN_POINT('Ctrl Pts',(-0.980505922458267,-1.,3.67074983340361));
#51104=CARTESIAN_POINT('Ctrl Pts',(-0.983550791470419,-1.,3.67782408841715));
#51105=CARTESIAN_POINT('Ctrl Pts',(-0.986602639863838,-1.,3.68455317926068));
#51106=CARTESIAN_POINT('Ctrl Pts',(-0.989676715398558,-1.,3.69102682138846));
#51107=CARTESIAN_POINT('Ctrl Pts',(-0.99280221833201,-1.,3.69738123415662));
#51108=CARTESIAN_POINT('Ctrl Pts',(-0.996009819772518,-1.,3.70375282282138));
#51109=CARTESIAN_POINT('Ctrl Pts',(-0.999317260756531,-1.,3.71022439713938));
#51110=CARTESIAN_POINT('Ctrl Pts',(-1.00272423396822,-1.,3.71680667125118));
#51111=CARTESIAN_POINT('Ctrl Pts',(-1.0062200073571,-1.,3.72346803750595));
#51112=CARTESIAN_POINT('Ctrl Pts',(-1.00978798539496,-1.,3.73015276704426));
#51113=CARTESIAN_POINT('Ctrl Pts',(-1.01341114319903,-1.,3.73680245055734));
#51114=CARTESIAN_POINT('Ctrl Pts',(-1.01707794311079,-1.,3.74337942504959));
#51115=CARTESIAN_POINT('Ctrl Pts',(-1.02078510487428,-1.,3.74987777155834));
#51116=CARTESIAN_POINT('Ctrl Pts',(-1.0245342944466,-1.,3.75631037456194));
#51117=CARTESIAN_POINT('Ctrl Pts',(-1.02833014458181,-1.,3.76270122291232));
#51118=CARTESIAN_POINT('Ctrl Pts',(-1.0321778660492,-1.,3.76907609832522));
#51119=CARTESIAN_POINT('Ctrl Pts',(-1.03608074678013,-1.,3.77545283140445));
#51120=CARTESIAN_POINT('Ctrl Pts',(-1.04003862055804,-1.,3.78183535008192));
#51121=CARTESIAN_POINT('Ctrl Pts',(-1.04404924374426,-1.,3.78821910787195));
#51122=CARTESIAN_POINT('Ctrl Pts',(-1.04810913267641,-1.,3.79459440308793));
#51123=CARTESIAN_POINT('Ctrl Pts',(-1.05221457990015,-1.,3.80095039790678));
#51124=CARTESIAN_POINT('Ctrl Pts',(-1.05636266918643,-1.,3.80727913637784));
#51125=CARTESIAN_POINT('Ctrl Pts',(-1.06055206187298,-1.,3.81357866117485));
#51126=CARTESIAN_POINT('Ctrl Pts',(-1.06478244038931,-1.,3.81985083953012));
#51127=CARTESIAN_POINT('Ctrl Pts',(-1.0690541318036,-1.,3.82609989967278));
#51128=CARTESIAN_POINT('Ctrl Pts',(-1.0733676663346,-1.,3.83233071195145));
#51129=CARTESIAN_POINT('Ctrl Pts',(-1.07772335353856,-1.,3.83854714117486));
#51130=CARTESIAN_POINT('Ctrl Pts',(-1.08212087917986,-1.,3.84475048030615));
#51131=CARTESIAN_POINT('Ctrl Pts',(-1.08655950846377,-1.,3.8509402522269));
#51132=CARTESIAN_POINT('Ctrl Pts',(-1.09103825516288,-1.,3.85711487933911));
#51133=CARTESIAN_POINT('Ctrl Pts',(-1.09555606505012,-1.,3.86327241021242));
#51134=CARTESIAN_POINT('Ctrl Pts',(-1.10011198761202,-1.,3.86941120134872));
#51135=CARTESIAN_POINT('Ctrl Pts',(-1.10470536603303,-1.,3.87553067187566));
#51136=CARTESIAN_POINT('Ctrl Pts',(-1.10933577224029,-1.,3.88163105531791));
#51137=CARTESIAN_POINT('Ctrl Pts',(-1.11400292434447,-1.,3.88771308285229));
#51138=CARTESIAN_POINT('Ctrl Pts',(-1.11870660794609,-1.,3.89377768340362));
#51139=CARTESIAN_POINT('Ctrl Pts',(-1.12344660099029,-1.,3.89982569749978));
#51140=CARTESIAN_POINT('Ctrl Pts',(-1.12822258281518,-1.,3.90585753318622));
#51141=CARTESIAN_POINT('Ctrl Pts',(-1.13303414693849,-1.,3.91187321145495));
#51142=CARTESIAN_POINT('Ctrl Pts',(-1.13788084225511,-1.,3.91787251936688));
#51143=CARTESIAN_POINT('Ctrl Pts',(-1.14276220561575,-1.,3.92385513133937));
#51144=CARTESIAN_POINT('Ctrl Pts',(-1.14767779451147,-1.,3.92982073294334));
#51145=CARTESIAN_POINT('Ctrl Pts',(-1.15262722716391,-1.,3.9357691705651));
#51146=CARTESIAN_POINT('Ctrl Pts',(-1.1576101834106,-1.,3.94170046685542));
#51147=CARTESIAN_POINT('Ctrl Pts',(-1.16262637999261,-1.,3.9476147478092));
#51148=CARTESIAN_POINT('Ctrl Pts',(-1.16767555244495,-1.,3.95351219510062));
#51149=CARTESIAN_POINT('Ctrl Pts',(-1.17275743590327,-1.,3.95939299213164));
#51150=CARTESIAN_POINT('Ctrl Pts',(-1.17787174135445,-1.,3.96525726357682));
#51151=CARTESIAN_POINT('Ctrl Pts',(-1.18301815039596,-1.,3.9711050516465));
#51152=CARTESIAN_POINT('Ctrl Pts',(-1.18819633715285,-1.,3.97693634766926));
#51153=CARTESIAN_POINT('Ctrl Pts',(-1.19340598349307,-1.,3.98275111052015));
#51154=CARTESIAN_POINT('Ctrl Pts',(-1.19864679609596,-1.,3.98854928957287));
#51155=CARTESIAN_POINT('Ctrl Pts',(-1.2039185237544,-1.,3.99433084800649));
#51156=CARTESIAN_POINT('Ctrl Pts',(-1.20922097030107,-1.,4.00009577952534));
#51157=CARTESIAN_POINT('Ctrl Pts',(-1.21455398918813,-1.,4.00584409524937));
#51158=CARTESIAN_POINT('Ctrl Pts',(-1.21884478244983,-1.,4.01042947142681));
#51159=CARTESIAN_POINT('Ctrl Pts',(-1.22207656456199,-1.,4.01386104434674));
#51160=CARTESIAN_POINT('Ctrl Pts',(-1.22423716681447,-1.,4.0161454457032));
#51161=CARTESIAN_POINT('Ctrl Pts',(-1.22531898815164,-1.,4.01728681790024));
#51162=CARTESIAN_POINT('',(-1.36999806084572,-1.,3.97027773754922));
#51163=CARTESIAN_POINT('',(-1.22531898815164,-1.,4.01728681790024));
#51164=CARTESIAN_POINT('',(-1.35032489087101,-1.,3.4984457533445));
#51165=CARTESIAN_POINT('Ctrl Pts',(-1.36999806084572,-1.,3.97027773754922));
#51166=CARTESIAN_POINT('Ctrl Pts',(-1.37020239094614,-1.,3.9687184694131));
#51167=CARTESIAN_POINT('Ctrl Pts',(-1.37060761745635,-1.,3.96560037974645));
#51168=CARTESIAN_POINT('Ctrl Pts',(-1.3712051561502,-1.,3.96092458506535));
#51169=CARTESIAN_POINT('Ctrl Pts',(-1.37198126432386,-1.,3.95469287280914));
#51170=CARTESIAN_POINT('Ctrl Pts',(-1.37291699202807,-1.,3.94690771785133));
#51171=CARTESIAN_POINT('Ctrl Pts',(-1.37381821967165,-1.,3.93912709040818));
#51172=CARTESIAN_POINT('Ctrl Pts',(-1.37468482215751,-1.,3.93135106761844));
#51173=CARTESIAN_POINT('Ctrl Pts',(-1.37551664448242,-1.,3.92357976987672));
#51174=CARTESIAN_POINT('Ctrl Pts',(-1.37631350505797,-1.,3.91581337462644));
#51175=CARTESIAN_POINT('Ctrl Pts',(-1.3770751963402,-1.,3.90805209523486));
#51176=CARTESIAN_POINT('Ctrl Pts',(-1.37780148512792,-1.,3.90029615196727));
#51177=CARTESIAN_POINT('Ctrl Pts',(-1.3784921128802,-1.,3.89254574338496));
#51178=CARTESIAN_POINT('Ctrl Pts',(-1.37914679719383,-1.,3.88480102249277));
#51179=CARTESIAN_POINT('Ctrl Pts',(-1.37976523097073,-1.,3.87706205830532));
#51180=CARTESIAN_POINT('Ctrl Pts',(-1.38034709213014,-1.,3.86932885813068));
#51181=CARTESIAN_POINT('Ctrl Pts',(-1.38089205992989,-1.,3.86160143043959));
#51182=CARTESIAN_POINT('Ctrl Pts',(-1.38139983115049,-1.,3.85387983979481));
#51183=CARTESIAN_POINT('Ctrl Pts',(-1.38187013346109,-1.,3.84616425605764));
#51184=CARTESIAN_POINT('Ctrl Pts',(-1.38230274828822,-1.,3.83845502790746));
#51185=CARTESIAN_POINT('Ctrl Pts',(-1.38269750245138,-1.,3.8307526698229));
#51186=CARTESIAN_POINT('Ctrl Pts',(-1.38305421262763,-1.,3.82305771743829));
#51187=CARTESIAN_POINT('Ctrl Pts',(-1.38337263902782,-1.,3.81537060817811));
#51188=CARTESIAN_POINT('Ctrl Pts',(-1.3836524404622,-1.,3.80769156398411));
#51189=CARTESIAN_POINT('Ctrl Pts',(-1.38389311766682,-1.,3.80002044322111));
#51190=CARTESIAN_POINT('Ctrl Pts',(-1.38409399694566,-1.,3.79235669640841));
#51191=CARTESIAN_POINT('Ctrl Pts',(-1.38425435883756,-1.,3.78469969805082));
#51192=CARTESIAN_POINT('Ctrl Pts',(-1.38437354551428,-1.,3.77704902230418));
#51193=CARTESIAN_POINT('Ctrl Pts',(-1.38445107339518,-1.,3.76940473185779));
#51194=CARTESIAN_POINT('Ctrl Pts',(-1.3844867525335,-1.,3.76176768271367));
#51195=CARTESIAN_POINT('Ctrl Pts',(-1.38448077997163,-1.,3.7541397631875));
#51196=CARTESIAN_POINT('Ctrl Pts',(-1.38443344984394,-1.,3.74652317167876));
#51197=CARTESIAN_POINT('Ctrl Pts',(-1.38434489156458,-1.,3.73891976418104));
#51198=CARTESIAN_POINT('Ctrl Pts',(-1.38421479111531,-1.,3.73133035859282));
#51199=CARTESIAN_POINT('Ctrl Pts',(-1.3840421342895,-1.,3.72375409358803));
#51200=CARTESIAN_POINT('Ctrl Pts',(-1.38382489984586,-1.,3.7161876605181));
#51201=CARTESIAN_POINT('Ctrl Pts',(-1.38356065402124,-1.,3.70862680753347));
#51202=CARTESIAN_POINT('Ctrl Pts',(-1.38324717612865,-1.,3.701067921679));
#51203=CARTESIAN_POINT('Ctrl Pts',(-1.38288311171651,-1.,3.69350967899526));
#51204=CARTESIAN_POINT('Ctrl Pts',(-1.38246852827182,-1.,3.68595444983837));
#51205=CARTESIAN_POINT('Ctrl Pts',(-1.3820057429062,-1.,3.67841038482414));
#51206=CARTESIAN_POINT('Ctrl Pts',(-1.38149812653868,-1.,3.67088843112262));
#51207=CARTESIAN_POINT('Ctrl Pts',(-1.38094856333552,-1.,3.66339848520857));
#51208=CARTESIAN_POINT('Ctrl Pts',(-1.38035791051213,-1.,3.6559455440439));
#51209=CARTESIAN_POINT('Ctrl Pts',(-1.37972372481603,-1.,3.64852652756456));
#51210=CARTESIAN_POINT('Ctrl Pts',(-1.37903818567359,-1.,3.64112507791141));
#51211=CARTESIAN_POINT('Ctrl Pts',(-1.37829035457339,-1.,3.63371727442486));
#51212=CARTESIAN_POINT('Ctrl Pts',(-1.37746987919881,-1.,3.62628098665145));
#51213=CARTESIAN_POINT('Ctrl Pts',(-1.37657053403107,-1.,3.6188048116042));
#51214=CARTESIAN_POINT('Ctrl Pts',(-1.37559314436634,-1.,3.61129546591064));
#51215=CARTESIAN_POINT('Ctrl Pts',(-1.37455051379623,-1.,3.60379020123988));
#51216=CARTESIAN_POINT('Ctrl Pts',(-1.37346320103157,-1.,3.59634627869048));
#51217=CARTESIAN_POINT('Ctrl Pts',(-1.37235053660976,-1.,3.58901853846365));
#51218=CARTESIAN_POINT('Ctrl Pts',(-1.37122241663062,-1.,3.58183885982715));
#51219=CARTESIAN_POINT('Ctrl Pts',(-1.37007229485659,-1.,3.57479875549486));
#51220=CARTESIAN_POINT('Ctrl Pts',(-1.36886584973389,-1.,3.5678208030466));
#51221=CARTESIAN_POINT('Ctrl Pts',(-1.36754771771233,-1.,3.56077662028649));
#51222=CARTESIAN_POINT('Ctrl Pts',(-1.3660614545677,-1.,3.55353883995949));
#51223=CARTESIAN_POINT('Ctrl Pts',(-1.36436666257598,-1.,3.54602591832973));
#51224=CARTESIAN_POINT('Ctrl Pts',(-1.36245507339307,-1.,3.53824396424961));
#51225=CARTESIAN_POINT('Ctrl Pts',(-1.36037259643734,-1.,3.530344649616));
#51226=CARTESIAN_POINT('Ctrl Pts',(-1.35821701528836,-1.,3.52261776116748));
#51227=CARTESIAN_POINT('Ctrl Pts',(-1.35611275237152,-1.,3.51542230699556));
#51228=CARTESIAN_POINT('Ctrl Pts',(-1.35419113575956,-1.,3.50913227059999));
#51229=CARTESIAN_POINT('Ctrl Pts',(-1.35257032843486,-1.,3.50408168106261));
#51230=CARTESIAN_POINT('Ctrl Pts',(-1.35142377279517,-1.,3.5007660381649));
#51231=CARTESIAN_POINT('Ctrl Pts',(-1.35080045218587,-1.,3.49920025459723));
#51232=CARTESIAN_POINT('Ctrl Pts',(-1.35049736560527,-1.,3.49861894124827));
#51233=CARTESIAN_POINT('Ctrl Pts',(-1.35036670892966,-1.,3.49847119623846));
#51234=CARTESIAN_POINT('Ctrl Pts',(-1.35032489087101,-1.,3.4984457533445));
#51235=CARTESIAN_POINT('',(-1.51895082866166,-1.,3.42859860294378));
#51236=CARTESIAN_POINT('Origin',(0.,-1.,0.));
#51237=CARTESIAN_POINT('',(-1.83867539237861,-1.,3.77614523045147));
#51238=CARTESIAN_POINT('Ctrl Pts',(-1.51895082866166,-1.,3.42859860294378));
#51239=CARTESIAN_POINT('Ctrl Pts',(-1.51893924967231,-1.,3.42864616361967));
#51240=CARTESIAN_POINT('Ctrl Pts',(-1.51895133295017,-1.,3.42884302333978));
#51241=CARTESIAN_POINT('Ctrl Pts',(-1.51914806898539,-1.,3.42946838852728));
#51242=CARTESIAN_POINT('Ctrl Pts',(-1.5198144909343,-1.,3.4310163189349));
#51243=CARTESIAN_POINT('Ctrl Pts',(-1.52134826724227,-1.,3.43417156977749));
#51244=CARTESIAN_POINT('Ctrl Pts',(-1.52377348950429,-1.,3.43888895974182));
#51245=CARTESIAN_POINT('Ctrl Pts',(-1.52686242875717,-1.,3.44469547527));
#51246=CARTESIAN_POINT('Ctrl Pts',(-1.530462444618,-1.,3.45127136828667));
#51247=CARTESIAN_POINT('Ctrl Pts',(-1.53440195378902,-1.,3.45825932955273));
#51248=CARTESIAN_POINT('Ctrl Pts',(-1.53851507915533,-1.,3.46531752207222));
#51249=CARTESIAN_POINT('Ctrl Pts',(-1.54266605398152,-1.,3.47217189224576));
#51250=CARTESIAN_POINT('Ctrl Pts',(-1.54678009290207,-1.,3.47868272898599));
#51251=CARTESIAN_POINT('Ctrl Pts',(-1.55084702970382,-1.,3.48485155928414));
#51252=CARTESIAN_POINT('Ctrl Pts',(-1.5548959590107,-1.,3.49076460877317));
#51253=CARTESIAN_POINT('Ctrl Pts',(-1.55897703097859,-1.,3.49655185179623));
#51254=CARTESIAN_POINT('Ctrl Pts',(-1.56314187758689,-1.,3.50234321621607));
#51255=CARTESIAN_POINT('Ctrl Pts',(-1.56742097575041,-1.,3.50821771695427));
#51256=CARTESIAN_POINT('Ctrl Pts',(-1.57181569799774,-1.,3.51418598431733));
#51257=CARTESIAN_POINT('Ctrl Pts',(-1.5763104998818,-1.,3.52021847865961));
#51258=CARTESIAN_POINT('Ctrl Pts',(-1.58088027227856,-1.,3.52626275334899));
#51259=CARTESIAN_POINT('Ctrl Pts',(-1.58549906268083,-1.,3.53226378147068));
#51260=CARTESIAN_POINT('Ctrl Pts',(-1.59014958368725,-1.,3.53818616861045));
#51261=CARTESIAN_POINT('Ctrl Pts',(-1.5948276694975,-1.,3.544024581823));
#51262=CARTESIAN_POINT('Ctrl Pts',(-1.59953698113444,-1.,3.54979148634426));
#51263=CARTESIAN_POINT('Ctrl Pts',(-1.60428584699848,-1.,3.55550985096117));
#51264=CARTESIAN_POINT('Ctrl Pts',(-1.60908344685459,-1.,3.56120432482986));
#51265=CARTESIAN_POINT('Ctrl Pts',(-1.61393581747522,-1.,3.56689200468404));
#51266=CARTESIAN_POINT('Ctrl Pts',(-1.61884340915412,-1.,3.57257679609826));
#51267=CARTESIAN_POINT('Ctrl Pts',(-1.62380329464851,-1.,3.57825455954405));
#51268=CARTESIAN_POINT('Ctrl Pts',(-1.62881051550748,-1.,3.5839162577435));
#51269=CARTESIAN_POINT('Ctrl Pts',(-1.63385971451259,-1.,3.58955176627876));
#51270=CARTESIAN_POINT('Ctrl Pts',(-1.63894676675349,-1.,3.59515368334887));
#51271=CARTESIAN_POINT('Ctrl Pts',(-1.6440700438558,-1.,3.6007202851384));
#51272=CARTESIAN_POINT('Ctrl Pts',(-1.64922952425833,-1.,3.60625346556992));
#51273=CARTESIAN_POINT('Ctrl Pts',(-1.65442619244327,-1.,3.61175734965129));
#51274=CARTESIAN_POINT('Ctrl Pts',(-1.65966133399186,-1.,3.61723666482457));
#51275=CARTESIAN_POINT('Ctrl Pts',(-1.66493585923853,-1.,3.62269517989104));
#51276=CARTESIAN_POINT('Ctrl Pts',(-1.67024966008037,-1.,3.62813422105257));
#51277=CARTESIAN_POINT('Ctrl Pts',(-1.67560193613145,-1.,3.63355343201211));
#51278=CARTESIAN_POINT('Ctrl Pts',(-1.68099146651577,-1.,3.63895140887443));
#51279=CARTESIAN_POINT('Ctrl Pts',(-1.68641690471455,-1.,3.64432638915199));
#51280=CARTESIAN_POINT('Ctrl Pts',(-1.691877054817,-1.,3.64967689827393));
#51281=CARTESIAN_POINT('Ctrl Pts',(-1.69737117722559,-1.,3.65500246526798));
#51282=CARTESIAN_POINT('Ctrl Pts',(-1.70289888566904,-1.,3.6603033877491));
#51283=CARTESIAN_POINT('Ctrl Pts',(-1.70846001610983,-1.,3.6655804319893));
#51284=CARTESIAN_POINT('Ctrl Pts',(-1.71405450210392,-1.,3.67083454901629));
#51285=CARTESIAN_POINT('Ctrl Pts',(-1.71968225581787,-1.,3.67606660374665));
#51286=CARTESIAN_POINT('Ctrl Pts',(-1.72534302437003,-1.,3.68127704936472));
#51287=CARTESIAN_POINT('Ctrl Pts',(-1.73103640956647,-1.,3.68646597019188));
#51288=CARTESIAN_POINT('Ctrl Pts',(-1.73676193254493,-1.,3.69163322647906));
#51289=CARTESIAN_POINT('Ctrl Pts',(-1.74251908492589,-1.,3.6967785691046));
#51290=CARTESIAN_POINT('Ctrl Pts',(-1.74830738046092,-1.,3.70190175673422));
#51291=CARTESIAN_POINT('Ctrl Pts',(-1.75412641804148,-1.,3.70700269736876));
#51292=CARTESIAN_POINT('Ctrl Pts',(-1.75997588499021,-1.,3.71208146346454));
#51293=CARTESIAN_POINT('Ctrl Pts',(-1.76585552124549,-1.,3.71713822377675));
#51294=CARTESIAN_POINT('Ctrl Pts',(-1.77176509401846,-1.,3.72217319911429));
#51295=CARTESIAN_POINT('Ctrl Pts',(-1.77770437039606,-1.,3.72718661205504));
#51296=CARTESIAN_POINT('Ctrl Pts',(-1.78367308442682,-1.,3.73217863095022));
#51297=CARTESIAN_POINT('Ctrl Pts',(-1.78967092823139,-1.,3.73714934729962));
#51298=CARTESIAN_POINT('Ctrl Pts',(-1.79569757859041,-1.,3.74209880351667));
#51299=CARTESIAN_POINT('Ctrl Pts',(-1.80175271485519,-1.,3.74702700874954));
#51300=CARTESIAN_POINT('Ctrl Pts',(-1.80783603939662,-1.,3.75193395888069));
#51301=CARTESIAN_POINT('Ctrl Pts',(-1.81394729834032,-1.,3.75681965683995));
#51302=CARTESIAN_POINT('Ctrl Pts',(-1.82008629694924,-1.,3.76168412709652));
#51303=CARTESIAN_POINT('Ctrl Pts',(-1.82625289221933,-1.,3.76652740355856));
#51304=CARTESIAN_POINT('Ctrl Pts',(-1.83120816956515,-1.,3.77038509819777));
#51305=CARTESIAN_POINT('Ctrl Pts',(-1.83493697935064,-1.,3.77326886065484));
#51306=CARTESIAN_POINT('Ctrl Pts',(-1.83742834010821,-1.,3.77518714458232));
#51307=CARTESIAN_POINT('Ctrl Pts',(-1.83867539237861,-1.,3.77614523045147));
#51308=CARTESIAN_POINT('',(-1.97421938526992,-1.,3.70708211654725));
#51309=CARTESIAN_POINT('',(-1.83867539237861,-1.,3.77614523045147));
#51310=CARTESIAN_POINT('',(-1.88097764062542,-1.,3.24413672884902));
#51311=CARTESIAN_POINT('Ctrl Pts',(-1.97421938526992,-1.,3.70708211654725));
#51312=CARTESIAN_POINT('Ctrl Pts',(-1.974177276451,-1.,3.7055100813194));
#51313=CARTESIAN_POINT('Ctrl Pts',(-1.97408973726149,-1.,3.70236698911837));
#51314=CARTESIAN_POINT('Ctrl Pts',(-1.97394846382289,-1.,3.69765528558292));
#51315=CARTESIAN_POINT('Ctrl Pts',(-1.97374016224397,-1.,3.69137888597855));
#51316=CARTESIAN_POINT('Ctrl Pts',(-1.97344650303631,-1.,3.68354319913416));
#51317=CARTESIAN_POINT('Ctrl Pts',(-1.97311947678035,-1.,3.67571738106175));
#51318=CARTESIAN_POINT('Ctrl Pts',(-1.9727589719863,-1.,3.66790152751984));
#51319=CARTESIAN_POINT('Ctrl Pts',(-1.97236485439317,-1.,3.66009578166865));
#51320=CARTESIAN_POINT('Ctrl Pts',(-1.97193697240645,-1.,3.65230034717364));
#51321=CARTESIAN_POINT('Ctrl Pts',(-1.97147515441539,-1.,3.64451546724221));
#51322=CARTESIAN_POINT('Ctrl Pts',(-1.97097920454698,-1.,3.63674139590853));
#51323=CARTESIAN_POINT('Ctrl Pts',(-1.97044889850518,-1.,3.62897836973397));
#51324=CARTESIAN_POINT('Ctrl Pts',(-1.96988398129888,-1.,3.62122658401722));
#51325=CARTESIAN_POINT('Ctrl Pts',(-1.96928416040712,-1.,3.61348615496393));
#51326=CARTESIAN_POINT('Ctrl Pts',(-1.96864911885775,-1.,3.60575714017676));
#51327=CARTESIAN_POINT('Ctrl Pts',(-1.96797854118257,-1.,3.59803959819725));
#51328=CARTESIAN_POINT('Ctrl Pts',(-1.96727213799507,-1.,3.5903336402273));
#51329=CARTESIAN_POINT('Ctrl Pts',(-1.9665296668894,-1.,3.58263947663884));
#51330=CARTESIAN_POINT('Ctrl Pts',(-1.96575096652857,-1.,3.57495748601088));
#51331=CARTESIAN_POINT('Ctrl Pts',(-1.96493594634643,-1.,3.56728820357933));
#51332=CARTESIAN_POINT('Ctrl Pts',(-1.96408450906868,-1.,3.55963218706201));
#51333=CARTESIAN_POINT('Ctrl Pts',(-1.96319648628667,-1.,3.55198990600929));
#51334=CARTESIAN_POINT('Ctrl Pts',(-1.96227157573058,-1.,3.54436163300425));
#51335=CARTESIAN_POINT('Ctrl Pts',(-1.96130926212661,-1.,3.53674730625759));
#51336=CARTESIAN_POINT('Ctrl Pts',(-1.96030879411534,-1.,3.52914648844289));
#51337=CARTESIAN_POINT('Ctrl Pts',(-1.95926936324436,-1.,3.52155867431438));
#51338=CARTESIAN_POINT('Ctrl Pts',(-1.95819025316768,-1.,3.51398354617772));
#51339=CARTESIAN_POINT('Ctrl Pts',(-1.95707099606514,-1.,3.50642124159913));
#51340=CARTESIAN_POINT('Ctrl Pts',(-1.9559115382367,-1.,3.49887263575602));
#51341=CARTESIAN_POINT('Ctrl Pts',(-1.95471236969653,-1.,3.49133956289154));
#51342=CARTESIAN_POINT('Ctrl Pts',(-1.95347412486316,-1.,3.48382414832648));
#51343=CARTESIAN_POINT('Ctrl Pts',(-1.95219722189878,-1.,3.47632820495926));
#51344=CARTESIAN_POINT('Ctrl Pts',(-1.95088147859876,-1.,3.4688525897419));
#51345=CARTESIAN_POINT('Ctrl Pts',(-1.94952575850196,-1.,3.46139661060959));
#51346=CARTESIAN_POINT('Ctrl Pts',(-1.94812754766524,-1.,3.45395731584051));
#51347=CARTESIAN_POINT('Ctrl Pts',(-1.94668377715332,-1.,3.44653088665685));
#51348=CARTESIAN_POINT('Ctrl Pts',(-1.94519168842883,-1.,3.43911410197693));
#51349=CARTESIAN_POINT('Ctrl Pts',(-1.94364973660285,-1.,3.43170586602436));
#51350=CARTESIAN_POINT('Ctrl Pts',(-1.94205835913692,-1.,3.42430850941497));
#51351=CARTESIAN_POINT('Ctrl Pts',(-1.94042111965237,-1.,3.41692971994082));
#51352=CARTESIAN_POINT('Ctrl Pts',(-1.93874306008132,-1.,3.40957978266622));
#51353=CARTESIAN_POINT('Ctrl Pts',(-1.93702857723089,-1.,3.40226802104093));
#51354=CARTESIAN_POINT('Ctrl Pts',(-1.93527929945982,-1.,3.39499923640789));
#51355=CARTESIAN_POINT('Ctrl Pts',(-1.93349233176794,-1.,3.38777076883267));
#51356=CARTESIAN_POINT('Ctrl Pts',(-1.93165739093292,-1.,3.38056768525577));
#51357=CARTESIAN_POINT('Ctrl Pts',(-1.92975993109897,-1.,3.37336807068078));
#51358=CARTESIAN_POINT('Ctrl Pts',(-1.92778626543803,-1.,3.36615168657597));
#51359=CARTESIAN_POINT('Ctrl Pts',(-1.92572846125763,-1.,3.35890824422976));
#51360=CARTESIAN_POINT('Ctrl Pts',(-1.92358838440518,-1.,3.35164424847206));
#51361=CARTESIAN_POINT('Ctrl Pts',(-1.92138450828378,-1.,3.34439448941915));
#51362=CARTESIAN_POINT('Ctrl Pts',(-1.91914609610173,-1.,3.33721230709948));
#51363=CARTESIAN_POINT('Ctrl Pts',(-1.91690081930297,-1.,3.33014884257812));
#51364=CARTESIAN_POINT('Ctrl Pts',(-1.91466343916612,-1.,3.32323403454507));
#51365=CARTESIAN_POINT('Ctrl Pts',(-1.91242616234459,-1.,3.31646052426395));
#51366=CARTESIAN_POINT('Ctrl Pts',(-1.91014297830502,-1.,3.30975721158694));
#51367=CARTESIAN_POINT('Ctrl Pts',(-1.90773912171424,-1.,3.30300595568341));
#51368=CARTESIAN_POINT('Ctrl Pts',(-1.9051389186417,-1.,3.29608978722258));
#51369=CARTESIAN_POINT('Ctrl Pts',(-1.9022897124757,-1.,3.28893448600364));
#51370=CARTESIAN_POINT('Ctrl Pts',(-1.89918429230425,-1.,3.28154737912287));
#51371=CARTESIAN_POINT('Ctrl Pts',(-1.89589172903662,-1.,3.27407108932908));
#51372=CARTESIAN_POINT('Ctrl Pts',(-1.89255393500769,-1.,3.2667765388833));
#51373=CARTESIAN_POINT('Ctrl Pts',(-1.88934996203508,-1.,3.2599988519361));
#51374=CARTESIAN_POINT('Ctrl Pts',(-1.88646802523372,-1.,3.25408686339298));
#51375=CARTESIAN_POINT('Ctrl Pts',(-1.88407708646435,-1.,3.24935200512055));
#51376=CARTESIAN_POINT('Ctrl Pts',(-1.88242596600422,-1.,3.24625654410705));
#51377=CARTESIAN_POINT('Ctrl Pts',(-1.88156537699118,-1.,3.24480754675942));
#51378=CARTESIAN_POINT('Ctrl Pts',(-1.88117508446657,-1.,3.24428080352952));
#51379=CARTESIAN_POINT('Ctrl Pts',(-1.88102292397987,-1.,3.2441553167131));
#51380=CARTESIAN_POINT('Ctrl Pts',(-1.88097764062542,-1.,3.24413672884902));
#51381=CARTESIAN_POINT('',(-2.03660101169564,-1.,3.14877060440425));
#51382=CARTESIAN_POINT('Origin',(0.,-1.,0.));
#51383=CARTESIAN_POINT('',(-2.40675750623143,-1.,3.44202241512147));
#51384=CARTESIAN_POINT('Ctrl Pts',(-2.03660101169564,-1.,3.14877060440425));
#51385=CARTESIAN_POINT('Ctrl Pts',(-2.03659701539175,-1.,3.1488193908823));
#51386=CARTESIAN_POINT('Ctrl Pts',(-2.03663974554941,-1.,3.14901193669147));
#51387=CARTESIAN_POINT('Ctrl Pts',(-2.03693188810614,-1.,3.14959882629936));
#51388=CARTESIAN_POINT('Ctrl Pts',(-2.03783225496023,-1.,3.15102344775396));
#51389=CARTESIAN_POINT('Ctrl Pts',(-2.03984073791432,-1.,3.1538999167466));
#51390=CARTESIAN_POINT('Ctrl Pts',(-2.04297406404132,-1.,3.15817983946525));
#51391=CARTESIAN_POINT('Ctrl Pts',(-2.0469333124766,-1.,3.16343165059235));
#51392=CARTESIAN_POINT('Ctrl Pts',(-2.05151770247452,-1.,3.16936341689859));
#51393=CARTESIAN_POINT('Ctrl Pts',(-2.05650186773279,-1.,3.17564906975592));
#51394=CARTESIAN_POINT('Ctrl Pts',(-2.06166849827143,-1.,3.18197692964677));
#51395=CARTESIAN_POINT('Ctrl Pts',(-2.06684062744065,-1.,3.18809755562297));
#51396=CARTESIAN_POINT('Ctrl Pts',(-2.07192253497765,-1.,3.19388465568113));
#51397=CARTESIAN_POINT('Ctrl Pts',(-2.0769044187063,-1.,3.19934132835879));
#51398=CARTESIAN_POINT('Ctrl Pts',(-2.08182850370816,-1.,3.20454818630635));
#51399=CARTESIAN_POINT('Ctrl Pts',(-2.08676465517435,-1.,3.20962575845433));
#51400=CARTESIAN_POINT('Ctrl Pts',(-2.0917841946046,-1.,3.2146942960168));
#51401=CARTESIAN_POINT('Ctrl Pts',(-2.09692958434933,-1.,3.21982707347067));
#51402=CARTESIAN_POINT('Ctrl Pts',(-2.10220384298533,-1.,3.22503437553496));
#51403=CARTESIAN_POINT('Ctrl Pts',(-2.1075869964248,-1.,3.23028945793334));
#51404=CARTESIAN_POINT('Ctrl Pts',(-2.11304604021784,-1.,3.23554444767115));
#51405=CARTESIAN_POINT('Ctrl Pts',(-2.11854673326972,-1.,3.24074905517282));
#51406=CARTESIAN_POINT('Ctrl Pts',(-2.12406646410943,-1.,3.24587102613347));
#51407=CARTESIAN_POINT('Ctrl Pts',(-2.1296002839681,-1.,3.25090574493994));
#51408=CARTESIAN_POINT('Ctrl Pts',(-2.13515375878786,-1.,3.25586495065027));
#51409=CARTESIAN_POINT('Ctrl Pts',(-2.14073870754257,-1.,3.26077002641868));
#51410=CARTESIAN_POINT('Ctrl Pts',(-2.14636805295663,-1.,3.26564388189764));
#51411=CARTESIAN_POINT('Ctrl Pts',(-2.15205043199818,-1.,3.27050245897244));
#51412=CARTESIAN_POINT('Ctrl Pts',(-2.15778690038359,-1.,3.27534954469206));
#51413=CARTESIAN_POINT('Ctrl Pts',(-2.16357391934434,-1.,3.28018150841414));
#51414=CARTESIAN_POINT('Ctrl Pts',(-2.16940517773459,-1.,3.2849901997973));
#51415=CARTESIAN_POINT('Ctrl Pts',(-2.17527380048422,-1.,3.28976645712566));
#51416=CARTESIAN_POINT('Ctrl Pts',(-2.18117455557062,-1.,3.29450361500484));
#51417=CARTESIAN_POINT('Ctrl Pts',(-2.18710556500325,-1.,3.29920022557635));
#51418=CARTESIAN_POINT('Ctrl Pts',(-2.19306710376112,-1.,3.30385816281831));
#51419=CARTESIAN_POINT('Ctrl Pts',(-2.19906078949924,-1.,3.30848134694596));
#51420=CARTESIAN_POINT('Ctrl Pts',(-2.20508863150608,-1.,3.3130742460895));
#51421=CARTESIAN_POINT('Ctrl Pts',(-2.21115211847872,-1.,3.31764044024231));
#51422=CARTESIAN_POINT('Ctrl Pts',(-2.21725135110889,-1.,3.32218125618955));
#51423=CARTESIAN_POINT('Ctrl Pts',(-2.22338548312758,-1.,3.32669646722871));
#51424=CARTESIAN_POINT('Ctrl Pts',(-2.22955308907221,-1.,3.33118487773593));
#51425=CARTESIAN_POINT('Ctrl Pts',(-2.2357525632881,-1.,3.33564495756478));
#51426=CARTESIAN_POINT('Ctrl Pts',(-2.24198249391437,-1.,3.34007543738044));
#51427=CARTESIAN_POINT('Ctrl Pts',(-2.24824207678288,-1.,3.34447596770768));
#51428=CARTESIAN_POINT('Ctrl Pts',(-2.25453097693524,-1.,3.34884690292342));
#51429=CARTESIAN_POINT('Ctrl Pts',(-2.26084915222484,-1.,3.35318902552676));
#51430=CARTESIAN_POINT('Ctrl Pts',(-2.26719668579921,-1.,3.35750328523077));
#51431=CARTESIAN_POINT('Ctrl Pts',(-2.27357362620902,-1.,3.36179055004369));
#51432=CARTESIAN_POINT('Ctrl Pts',(-2.27997979457968,-1.,3.36605130712978));
#51433=CARTESIAN_POINT('Ctrl Pts',(-2.28641481081045,-1.,3.37028570206357));
#51434=CARTESIAN_POINT('Ctrl Pts',(-2.2928781800731,-1.,3.37449367172707));
#51435=CARTESIAN_POINT('Ctrl Pts',(-2.29936936127588,-1.,3.37867504959382));
#51436=CARTESIAN_POINT('Ctrl Pts',(-2.30588783640389,-1.,3.38282967336676));
#51437=CARTESIAN_POINT('Ctrl Pts',(-2.31243319489505,-1.,3.38695751492659));
#51438=CARTESIAN_POINT('Ctrl Pts',(-2.31900513925627,-1.,3.39105869475112));
#51439=CARTESIAN_POINT('Ctrl Pts',(-2.32560343902683,-1.,3.39513342020045));
#51440=CARTESIAN_POINT('Ctrl Pts',(-2.33222789882601,-1.,3.39918194578115));
#51441=CARTESIAN_POINT('Ctrl Pts',(-2.33887832342715,-1.,3.40320452776646));
#51442=CARTESIAN_POINT('Ctrl Pts',(-2.34555447648901,-1.,3.40720137403888));
#51443=CARTESIAN_POINT('Ctrl Pts',(-2.35225606823649,-1.,3.41117262313464));
#51444=CARTESIAN_POINT('Ctrl Pts',(-2.35898278606449,-1.,3.4151183675076));
#51445=CARTESIAN_POINT('Ctrl Pts',(-2.36573431470314,-1.,3.41903866635384));
#51446=CARTESIAN_POINT('Ctrl Pts',(-2.37251035954351,-1.,3.42293356216595));
#51447=CARTESIAN_POINT('Ctrl Pts',(-2.37931067029517,-1.,3.42680309755241));
#51448=CARTESIAN_POINT('Ctrl Pts',(-2.38613505844641,-1.,3.43064732714472));
#51449=CARTESIAN_POINT('Ctrl Pts',(-2.39298338805823,-1.,3.43446630680436));
#51450=CARTESIAN_POINT('Ctrl Pts',(-2.39848113411429,-1.,3.43750133066036));
#51451=CARTESIAN_POINT('Ctrl Pts',(-2.40261515590099,-1.,3.43976627485223));
#51452=CARTESIAN_POINT('Ctrl Pts',(-2.40537592959345,-1.,3.44127120683402));
#51453=CARTESIAN_POINT('Ctrl Pts',(-2.40675750623143,-1.,3.44202241512147));
#51454=CARTESIAN_POINT('',(-2.52982887637028,-1.,3.35260583073571));
#51455=CARTESIAN_POINT('',(-2.40675750623143,-1.,3.44202241512147));
#51456=CARTESIAN_POINT('',(-2.36531447826073,-1.,2.90994629141676));
#51457=CARTESIAN_POINT('Ctrl Pts',(-2.52982887637028,-1.,3.35260583073571));
#51458=CARTESIAN_POINT('Ctrl Pts',(-2.5295413654909,-1.,3.35105973714071));
#51459=CARTESIAN_POINT('Ctrl Pts',(-2.52896321610703,-1.,3.34796903576663));
#51460=CARTESIAN_POINT('Ctrl Pts',(-2.52808660915689,-1.,3.34333744115511));
#51461=CARTESIAN_POINT('Ctrl Pts',(-2.52689902690158,-1.,3.33717089999103));
#51462=CARTESIAN_POINT('Ctrl Pts',(-2.52538321164634,-1.,3.32947762187533));
#51463=CARTESIAN_POINT('Ctrl Pts',(-2.5238359839626,-1.,3.32179931078699));
#51464=CARTESIAN_POINT('Ctrl Pts',(-2.52225724871313,-1.,3.31413607874645));
#51465=CARTESIAN_POINT('Ctrl Pts',(-2.52064689568511,-1.,3.30648808815442));
#51466=CARTESIAN_POINT('Ctrl Pts',(-2.51900480701069,-1.,3.29885556388352));
#51467=CARTESIAN_POINT('Ctrl Pts',(-2.51733085123797,-1.,3.2912387729927));
#51468=CARTESIAN_POINT('Ctrl Pts',(-2.51562487464514,-1.,3.28363799702982));
#51469=CARTESIAN_POINT('Ctrl Pts',(-2.513886692704,-1.,3.27605350473142));
#51470=CARTESIAN_POINT('Ctrl Pts',(-2.51211608411423,-1.,3.26848552888115));
#51471=CARTESIAN_POINT('Ctrl Pts',(-2.51031277813486,-1.,3.26093423001434));
#51472=CARTESIAN_POINT('Ctrl Pts',(-2.50847647070723,-1.,3.25339971460982));
#51473=CARTESIAN_POINT('Ctrl Pts',(-2.506606859405,-1.,3.24588208983849));
#51474=CARTESIAN_POINT('Ctrl Pts',(-2.5047036758003,-1.,3.23838151080319));
#51475=CARTESIAN_POINT('Ctrl Pts',(-2.50276671338111,-1.,3.23089822320646));
#51476=CARTESIAN_POINT('Ctrl Pts',(-2.50079587201957,-1.,3.22343262620503));
#51477=CARTESIAN_POINT('Ctrl Pts',(-2.4987911459939,-1.,3.21598526261286));
#51478=CARTESIAN_POINT('Ctrl Pts',(-2.4967525264737,-1.,3.20855669849836));
#51479=CARTESIAN_POINT('Ctrl Pts',(-2.49467992057755,-1.,3.20114742397588));
#51480=CARTESIAN_POINT('Ctrl Pts',(-2.49257307239848,-1.,3.19375775555798));
#51481=CARTESIAN_POINT('Ctrl Pts',(-2.49043146334059,-1.,3.18638771282266));
#51482=CARTESIAN_POINT('Ctrl Pts',(-2.48825428288201,-1.,3.17903698136622));
#51483=CARTESIAN_POINT('Ctrl Pts',(-2.48604065348587,-1.,3.17170518863313));
#51484=CARTESIAN_POINT('Ctrl Pts',(-2.48378981792725,-1.,3.16439213290161));
#51485=CARTESIAN_POINT('Ctrl Pts',(-2.48150133566571,-1.,3.15709802322739));
#51486=CARTESIAN_POINT('Ctrl Pts',(-2.47917529057029,-1.,3.14982373241352));
#51487=CARTESIAN_POINT('Ctrl Pts',(-2.47681245356109,-1.,3.1425709954655));
#51488=CARTESIAN_POINT('Ctrl Pts',(-2.47441378371932,-1.,3.13534181229295));
#51489=CARTESIAN_POINT('Ctrl Pts',(-2.47197997765871,-1.,3.12813790805952));
#51490=CARTESIAN_POINT('Ctrl Pts',(-2.46951098947469,-1.,3.12096015766983));
#51491=CARTESIAN_POINT('Ctrl Pts',(-2.46700558843506,-1.,3.11380805536122));
#51492=CARTESIAN_POINT('Ctrl Pts',(-2.46446082979646,-1.,3.1066790790198));
#51493=CARTESIAN_POINT('Ctrl Pts',(-2.46187308501884,-1.,3.09956993697052));
#51494=CARTESIAN_POINT('Ctrl Pts',(-2.4592391256388,-1.,3.09247787931887));
#51495=CARTESIAN_POINT('Ctrl Pts',(-2.45655725437039,-1.,3.08540206545315));
#51496=CARTESIAN_POINT('Ctrl Pts',(-2.4538282678779,-1.,3.07834472886139));
#51497=CARTESIAN_POINT('Ctrl Pts',(-2.45105688854422,-1.,3.07131290521297));
#51498=CARTESIAN_POINT('Ctrl Pts',(-2.44824970516544,-1.,3.06431596421405));
#51499=CARTESIAN_POINT('Ctrl Pts',(-2.44541251892556,-1.,3.05736242671506));
#51500=CARTESIAN_POINT('Ctrl Pts',(-2.44254768923105,-1.,3.05045678021504));
#51501=CARTESIAN_POINT('Ctrl Pts',(-2.43965194061857,-1.,3.04359685040555));
#51502=CARTESIAN_POINT('Ctrl Pts',(-2.43671278042414,-1.,3.03676949672821));
#51503=CARTESIAN_POINT('Ctrl Pts',(-2.43371241361488,-1.,3.02995534946978));
#51504=CARTESIAN_POINT('Ctrl Pts',(-2.43063415586637,-1.,3.02313656036004));
#51505=CARTESIAN_POINT('Ctrl Pts',(-2.42746856264168,-1.,3.01630420830504));
#51506=CARTESIAN_POINT('Ctrl Pts',(-2.42421849439613,-1.,3.00946442616658));
#51507=CARTESIAN_POINT('Ctrl Pts',(-2.42090763946779,-1.,3.00264868585996));
#51508=CARTESIAN_POINT('Ctrl Pts',(-2.41757324500514,-1.,2.99590509293503));
#51509=CARTESIAN_POINT('Ctrl Pts',(-2.41425064199586,-1.,2.98927983005796));
#51510=CARTESIAN_POINT('Ctrl Pts',(-2.41095909342571,-1.,2.98280015815107));
#51511=CARTESIAN_POINT('Ctrl Pts',(-2.40768975073713,-1.,2.97646002822422));
#51512=CARTESIAN_POINT('Ctrl Pts',(-2.40438604734919,-1.,2.9701964131236));
#51513=CARTESIAN_POINT('Ctrl Pts',(-2.4009556571164,-1.,2.96390432240312));
#51514=CARTESIAN_POINT('Ctrl Pts',(-2.39730553974517,-1.,2.95748006482942));
#51515=CARTESIAN_POINT('Ctrl Pts',(-2.39337207631667,-1.,2.95085857128439));
#51516=CARTESIAN_POINT('Ctrl Pts',(-2.38914929090759,-1.,2.94404820669076));
#51517=CARTESIAN_POINT('Ctrl Pts',(-2.38472771516311,-1.,2.93717903280391));
#51518=CARTESIAN_POINT('Ctrl Pts',(-2.38028989582073,-1.,2.93049643640206));
#51519=CARTESIAN_POINT('Ctrl Pts',(-2.3760651052403,-1.,2.92430340582608));
#51520=CARTESIAN_POINT('Ctrl Pts',(-2.37229381109821,-1.,2.91891503791411));
#51521=CARTESIAN_POINT('Ctrl Pts',(-2.36919161373173,-1.,2.9146124988314));
#51522=CARTESIAN_POINT('Ctrl Pts',(-2.36707658451664,-1.,2.91181344022549));
#51523=CARTESIAN_POINT('Ctrl Pts',(-2.36599991765749,-1.,2.91051690822156));
#51524=CARTESIAN_POINT('Ctrl Pts',(-2.36553202948613,-1.,2.91005770527719));
#51525=CARTESIAN_POINT('Ctrl Pts',(-2.36536211188453,-1.,2.90995756655606));
#51526=CARTESIAN_POINT('Ctrl Pts',(-2.36531447826074,-1.,2.90994629141676));
#51527=CARTESIAN_POINT('',(-2.50410331873042,-1.,2.79140942341378));
#51528=CARTESIAN_POINT('Origin',(0.,-1.,0.));
#51529=CARTESIAN_POINT('',(-2.91557726271063,-1.,3.02314558451372));
#51530=CARTESIAN_POINT('Ctrl Pts',(-2.50410331873042,-1.,2.79140942341378));
#51531=CARTESIAN_POINT('Ctrl Pts',(-2.50410700351426,-1.,2.79145823440899));
#51532=CARTESIAN_POINT('Ctrl Pts',(-2.50417932839343,-1.,2.79164172519039));
#51533=CARTESIAN_POINT('Ctrl Pts',(-2.50455968395235,-1.,2.79217568804874));
#51534=CARTESIAN_POINT('Ctrl Pts',(-2.50567182569153,-1.,2.79344192164204));
#51535=CARTESIAN_POINT('Ctrl Pts',(-2.50810555977564,-1.,2.7959687805717));
#51536=CARTESIAN_POINT('Ctrl Pts',(-2.51186983687947,-1.,2.79970585014308));
#51537=CARTESIAN_POINT('Ctrl Pts',(-2.51660190466067,-1.,2.80427363984939));
#51538=CARTESIAN_POINT('Ctrl Pts',(-2.52205778589922,-1.,2.80941521967234));
#51539=CARTESIAN_POINT('Ctrl Pts',(-2.52796388055457,-1.,2.8148437904867));
#51540=CARTESIAN_POINT('Ctrl Pts',(-2.53405679667463,-1.,2.82028550483744));
#51541=CARTESIAN_POINT('Ctrl Pts',(-2.54012272520141,-1.,2.82552167649157));
#51542=CARTESIAN_POINT('Ctrl Pts',(-2.54604736792542,-1.,2.83044254225794));
#51543=CARTESIAN_POINT('Ctrl Pts',(-2.55182152806964,-1.,2.83505269592412));
#51544=CARTESIAN_POINT('Ctrl Pts',(-2.55749952145165,-1.,2.83942515220699));
#51545=CARTESIAN_POINT('Ctrl Pts',(-2.56316920798489,-1.,2.84366802680211));
#51546=CARTESIAN_POINT('Ctrl Pts',(-2.56891984251743,-1.,2.84788893329091));
#51547=CARTESIAN_POINT('Ctrl Pts',(-2.57480482727128,-1.,2.85215360144483));
#51548=CARTESIAN_POINT('Ctrl Pts',(-2.58082875254407,-1.,2.85647171715147));
#51549=CARTESIAN_POINT('Ctrl Pts',(-2.5869677064356,-1.,2.86081999003668));
#51550=CARTESIAN_POINT('Ctrl Pts',(-2.59318160184921,-1.,2.86515629953528));
#51551=CARTESIAN_POINT('Ctrl Pts',(-2.59942875223202,-1.,2.86943633170712));
#51552=CARTESIAN_POINT('Ctrl Pts',(-2.6056817788128,-1.,2.87363176656475));
#51553=CARTESIAN_POINT('Ctrl Pts',(-2.61193507170928,-1.,2.87773881947885));
#51554=CARTESIAN_POINT('Ctrl Pts',(-2.61819596473087,-1.,2.88176821427502));
#51555=CARTESIAN_POINT('Ctrl Pts',(-2.62447947640253,-1.,2.88573922195049));
#51556=CARTESIAN_POINT('Ctrl Pts',(-2.63080195420771,-1.,2.88967244854243));
#51557=CARTESIAN_POINT('Ctrl Pts',(-2.63717442263944,-1.,2.89358228854557));
#51558=CARTESIAN_POINT('Ctrl Pts',(-2.64359851684146,-1.,2.89747231723361));
#51559=CARTESIAN_POINT('Ctrl Pts',(-2.65007017365576,-1.,2.90133950224879));
#51560=CARTESIAN_POINT('Ctrl Pts',(-2.65658188464287,-1.,2.90517678087467));
#51561=CARTESIAN_POINT('Ctrl Pts',(-2.66312542616809,-1.,2.90897617968921));
#51562=CARTESIAN_POINT('Ctrl Pts',(-2.66969458792627,-1.,2.91273193382876));
#51563=CARTESIAN_POINT('Ctrl Pts',(-2.67628728855309,-1.,2.91644290704281));
#51564=CARTESIAN_POINT('Ctrl Pts',(-2.68290409279689,-1.,2.92011090722152));
#51565=CARTESIAN_POINT('Ctrl Pts',(-2.68954721165342,-1.,2.92373955325876));
#51566=CARTESIAN_POINT('Ctrl Pts',(-2.69621932864302,-1.,2.92733294395268));
#51567=CARTESIAN_POINT('Ctrl Pts',(-2.70292247416881,-1.,2.93089438233746));
#51568=CARTESIAN_POINT('Ctrl Pts',(-2.70965695523776,-1.,2.93442516311168));
#51569=CARTESIAN_POINT('Ctrl Pts',(-2.71642190053575,-1.,2.93792519474955));
#51570=CARTESIAN_POINT('Ctrl Pts',(-2.72321571511322,-1.,2.94139351933882));
#51571=CARTESIAN_POINT('Ctrl Pts',(-2.73003657371613,-1.,2.94482887675139));
#51572=CARTESIAN_POINT('Ctrl Pts',(-2.73688288329825,-1.,2.94823023414381));
#51573=CARTESIAN_POINT('Ctrl Pts',(-2.7437537949221,-1.,2.95159737214305));
#51574=CARTESIAN_POINT('Ctrl Pts',(-2.75064903318996,-1.,2.95493069316211));
#51575=CARTESIAN_POINT('Ctrl Pts',(-2.75756867888393,-1.,2.9582309766594));
#51576=CARTESIAN_POINT('Ctrl Pts',(-2.76451296269571,-1.,2.96149914764832));
#51577=CARTESIAN_POINT('Ctrl Pts',(-2.77148206836464,-1.,2.96473605585548));
#51578=CARTESIAN_POINT('Ctrl Pts',(-2.77847589542767,-1.,2.9679422104295));
#51579=CARTESIAN_POINT('Ctrl Pts',(-2.78549409123657,-1.,2.97111781461349));
#51580=CARTESIAN_POINT('Ctrl Pts',(-2.79253615718147,-1.,2.97426288347475));
#51581=CARTESIAN_POINT('Ctrl Pts',(-2.79960153278186,-1.,2.97737733718242));
#51582=CARTESIAN_POINT('Ctrl Pts',(-2.80668968101162,-1.,2.98046109647299));
#51583=CARTESIAN_POINT('Ctrl Pts',(-2.81380019196454,-1.,2.9835141977994));
#51584=CARTESIAN_POINT('Ctrl Pts',(-2.82093279065704,-1.,2.98653680669434));
#51585=CARTESIAN_POINT('Ctrl Pts',(-2.82808728190402,-1.,2.98952916401699));
#51586=CARTESIAN_POINT('Ctrl Pts',(-2.83526351254383,-1.,2.99249155170479));
#51587=CARTESIAN_POINT('Ctrl Pts',(-2.84246132984334,-1.,2.995424253416));
#51588=CARTESIAN_POINT('Ctrl Pts',(-2.84968053289104,-1.,2.99832751144566));
#51589=CARTESIAN_POINT('Ctrl Pts',(-2.85692085715129,-1.,3.0012015079552));
#51590=CARTESIAN_POINT('Ctrl Pts',(-2.86418200833065,-1.,3.00404638316245));
#51591=CARTESIAN_POINT('Ctrl Pts',(-2.87146368430104,-1.,3.00686224485374));
#51592=CARTESIAN_POINT('Ctrl Pts',(-2.87876560072799,-1.,3.0096491810855));
#51593=CARTESIAN_POINT('Ctrl Pts',(-2.88608751706796,-1.,3.01240727309568));
#51594=CARTESIAN_POINT('Ctrl Pts',(-2.8934292556764,-1.,3.01513660433291));
#51595=CARTESIAN_POINT('Ctrl Pts',(-2.90079069102661,-1.,3.01783725123646));
#51596=CARTESIAN_POINT('Ctrl Pts',(-2.90669553303902,-1.,3.01997487194926));
#51597=CARTESIAN_POINT('Ctrl Pts',(-2.91113297349052,-1.,3.02156522743299));
#51598=CARTESIAN_POINT('Ctrl Pts',(-2.91409518070707,-1.,3.02261975104912));
#51599=CARTESIAN_POINT('Ctrl Pts',(-2.91557726271063,-1.,3.02314558451372));
#51600=CARTESIAN_POINT('',(-3.02314558451372,-1.,2.91557726271063));
#51601=CARTESIAN_POINT('',(-2.91557726271063,-1.,3.02314558451372));
#51602=CARTESIAN_POINT('',(-2.79140942341258,-1.,2.50410331873176));
#51603=CARTESIAN_POINT('Ctrl Pts',(-3.02314558451372,-1.,2.91557726271063));
#51604=CARTESIAN_POINT('Ctrl Pts',(-3.02261975104593,-1.,2.91409518070399));
#51605=CARTESIAN_POINT('Ctrl Pts',(-3.02156522742431,-1.,2.91113297348212));
#51606=CARTESIAN_POINT('Ctrl Pts',(-3.01997487193503,-1.,2.90669553302526));
#51607=CARTESIAN_POINT('Ctrl Pts',(-3.01783725121981,-1.,2.9007906910105));
#51608=CARTESIAN_POINT('Ctrl Pts',(-3.01513660431928,-1.,2.89342925566321));
#51609=CARTESIAN_POINT('Ctrl Pts',(-3.01240727308829,-1.,2.8860875170608));
#51610=CARTESIAN_POINT('Ctrl Pts',(-3.00964918108476,-1.,2.87876560072727));
#51611=CARTESIAN_POINT('Ctrl Pts',(-3.00686224485784,-1.,2.87146368430502));
#51612=CARTESIAN_POINT('Ctrl Pts',(-3.00404638316867,-1.,2.86418200833667));
#51613=CARTESIAN_POINT('Ctrl Pts',(-3.00120150796095,-1.,2.85692085715686));
#51614=CARTESIAN_POINT('Ctrl Pts',(-2.99832751144925,-1.,2.84968053289451));
#51615=CARTESIAN_POINT('Ctrl Pts',(-2.99542425341685,-1.,2.84246132984415));
#51616=CARTESIAN_POINT('Ctrl Pts',(-2.9924915517034,-1.,2.83526351254248));
#51617=CARTESIAN_POINT('Ctrl Pts',(-2.98952916401446,-1.,2.82808728190157));
#51618=CARTESIAN_POINT('Ctrl Pts',(-2.9865368066918,-1.,2.82093279065457));
#51619=CARTESIAN_POINT('Ctrl Pts',(-2.98351419779767,-1.,2.81380019196286));
#51620=CARTESIAN_POINT('Ctrl Pts',(-2.98046109647241,-1.,2.80668968101106));
#51621=CARTESIAN_POINT('Ctrl Pts',(-2.97737733718287,-1.,2.7996015327823));
#51622=CARTESIAN_POINT('Ctrl Pts',(-2.9742628834758,-1.,2.79253615718248));
#51623=CARTESIAN_POINT('Ctrl Pts',(-2.97111781461465,-1.,2.78549409123769));
#51624=CARTESIAN_POINT('Ctrl Pts',(-2.96794221043036,-1.,2.7784758954285));
#51625=CARTESIAN_POINT('Ctrl Pts',(-2.96473605585583,-1.,2.77148206836498));
#51626=CARTESIAN_POINT('Ctrl Pts',(-2.96149914764818,-1.,2.76451296269557));
#51627=CARTESIAN_POINT('Ctrl Pts',(-2.95823097665896,-1.,2.7575686788835));
#51628=CARTESIAN_POINT('Ctrl Pts',(-2.95493069316161,-1.,2.75064903318947));
#51629=CARTESIAN_POINT('Ctrl Pts',(-2.95159737214266,-1.,2.74375379492172));
#51630=CARTESIAN_POINT('Ctrl Pts',(-2.94823023414364,-1.,2.73688288329808));
#51631=CARTESIAN_POINT('Ctrl Pts',(-2.94482887675143,-1.,2.73003657371617));
#51632=CARTESIAN_POINT('Ctrl Pts',(-2.94139351933897,-1.,2.72321571511337));
#51633=CARTESIAN_POINT('Ctrl Pts',(-2.93792519474972,-1.,2.71642190053592));
#51634=CARTESIAN_POINT('Ctrl Pts',(-2.93442516311179,-1.,2.70965695523787));
#51635=CARTESIAN_POINT('Ctrl Pts',(-2.9308943823375,-1.,2.70292247416885));
#51636=CARTESIAN_POINT('Ctrl Pts',(-2.92733294395267,-1.,2.69621932864301));
#51637=CARTESIAN_POINT('Ctrl Pts',(-2.92373955325875,-1.,2.68954721165339));
#51638=CARTESIAN_POINT('Ctrl Pts',(-2.92011090722152,-1.,2.68290409279688));
#51639=CARTESIAN_POINT('Ctrl Pts',(-2.91644290704285,-1.,2.67628728855312));
#51640=CARTESIAN_POINT('Ctrl Pts',(-2.91273193382882,-1.,2.66969458792631));
#51641=CARTESIAN_POINT('Ctrl Pts',(-2.90897617968923,-1.,2.6631254261681));
#51642=CARTESIAN_POINT('Ctrl Pts',(-2.90517678087461,-1.,2.65658188464282));
#51643=CARTESIAN_POINT('Ctrl Pts',(-2.90133950224867,-1.,2.65007017365564));
#51644=CARTESIAN_POINT('Ctrl Pts',(-2.89747231723345,-1.,2.64359851684131));
#51645=CARTESIAN_POINT('Ctrl Pts',(-2.89358228854544,-1.,2.63717442263932));
#51646=CARTESIAN_POINT('Ctrl Pts',(-2.88967244854239,-1.,2.63080195420767));
#51647=CARTESIAN_POINT('Ctrl Pts',(-2.88573922195059,-1.,2.62447947640262));
#51648=CARTESIAN_POINT('Ctrl Pts',(-2.88176821427525,-1.,2.61819596473108));
#51649=CARTESIAN_POINT('Ctrl Pts',(-2.87773881947916,-1.,2.61193507170955));
#51650=CARTESIAN_POINT('Ctrl Pts',(-2.87363176656501,-1.,2.60568177881303));
#51651=CARTESIAN_POINT('Ctrl Pts',(-2.86943633170722,-1.,2.5994287522321));
#51652=CARTESIAN_POINT('Ctrl Pts',(-2.86515629953513,-1.,2.59318160184908));
#51653=CARTESIAN_POINT('Ctrl Pts',(-2.86081999003629,-1.,2.58696770643524));
#51654=CARTESIAN_POINT('Ctrl Pts',(-2.85647171715092,-1.,2.58082875254357));
#51655=CARTESIAN_POINT('Ctrl Pts',(-2.85215360144431,-1.,2.57480482727081));
#51656=CARTESIAN_POINT('Ctrl Pts',(-2.84788893329067,-1.,2.56891984251721));
#51657=CARTESIAN_POINT('Ctrl Pts',(-2.84366802680237,-1.,2.56316920798513));
#51658=CARTESIAN_POINT('Ctrl Pts',(-2.83942515220782,-1.,2.55749952145241));
#51659=CARTESIAN_POINT('Ctrl Pts',(-2.83505269592536,-1.,2.55182152807077));
#51660=CARTESIAN_POINT('Ctrl Pts',(-2.83044254225917,-1.,2.54604736792655));
#51661=CARTESIAN_POINT('Ctrl Pts',(-2.8255216764922,-1.,2.54012272520199));
#51662=CARTESIAN_POINT('Ctrl Pts',(-2.82028550483689,-1.,2.53405679667412));
#51663=CARTESIAN_POINT('Ctrl Pts',(-2.81484379048475,-1.,2.52796388055278));
#51664=CARTESIAN_POINT('Ctrl Pts',(-2.80941521966941,-1.,2.52205778589653));
#51665=CARTESIAN_POINT('Ctrl Pts',(-2.80427363984653,-1.,2.51660190465805));
#51666=CARTESIAN_POINT('Ctrl Pts',(-2.79970585014168,-1.,2.51186983687818));
#51667=CARTESIAN_POINT('Ctrl Pts',(-2.79596878057287,-1.,2.50810555977671));
#51668=CARTESIAN_POINT('Ctrl Pts',(-2.79344192164147,-1.,2.50567182569081));
#51669=CARTESIAN_POINT('Ctrl Pts',(-2.79217568804755,-1.,2.50455968395146));
#51670=CARTESIAN_POINT('Ctrl Pts',(-2.79164172518905,-1.,2.50417932839313));
#51671=CARTESIAN_POINT('Ctrl Pts',(-2.79145823440781,-1.,2.50410700351493));
#51672=CARTESIAN_POINT('Ctrl Pts',(-2.79140942341258,-1.,2.50410331873176));
#51673=CARTESIAN_POINT('',(-2.90994629141562,-1.,2.36531447826213));
#51674=CARTESIAN_POINT('Origin',(0.,-1.,0.));
#51675=CARTESIAN_POINT('',(-3.35260583073571,-1.,2.52982887637028));
#51676=CARTESIAN_POINT('Ctrl Pts',(-2.90994629141562,-1.,2.36531447826213));
#51677=CARTESIAN_POINT('Ctrl Pts',(-2.90995756655558,-1.,2.3653621118858));
#51678=CARTESIAN_POINT('Ctrl Pts',(-2.9100577052777,-1.,2.36553202948741));
#51679=CARTESIAN_POINT('Ctrl Pts',(-2.91051690822262,-1.,2.36599991765853));
#51680=CARTESIAN_POINT('Ctrl Pts',(-2.91181344022628,-1.,2.36707658451709));
#51681=CARTESIAN_POINT('Ctrl Pts',(-2.91461249883016,-1.,2.36919161373074));
#51682=CARTESIAN_POINT('Ctrl Pts',(-2.9189150379156,-1.,2.37229381109939));
#51683=CARTESIAN_POINT('Ctrl Pts',(-2.92430340582912,-1.,2.37606510524271));
#51684=CARTESIAN_POINT('Ctrl Pts',(-2.93049643640517,-1.,2.3802898958232));
#51685=CARTESIAN_POINT('Ctrl Pts',(-2.93717903280599,-1.,2.38472771516476));
#51686=CARTESIAN_POINT('Ctrl Pts',(-2.94404820669135,-1.,2.38914929090806));
#51687=CARTESIAN_POINT('Ctrl Pts',(-2.95085857128372,-1.,2.39337207631613));
#51688=CARTESIAN_POINT('Ctrl Pts',(-2.95748006482811,-1.,2.39730553974412));
#51689=CARTESIAN_POINT('Ctrl Pts',(-2.96390432240181,-1.,2.40095565711535));
#51690=CARTESIAN_POINT('Ctrl Pts',(-2.97019641312272,-1.,2.40438604734848));
#51691=CARTESIAN_POINT('Ctrl Pts',(-2.97646002822395,-1.,2.40768975073691));
#51692=CARTESIAN_POINT('Ctrl Pts',(-2.98280015815132,-1.,2.41095909342591));
#51693=CARTESIAN_POINT('Ctrl Pts',(-2.98927983005851,-1.,2.4142506419963));
#51694=CARTESIAN_POINT('Ctrl Pts',(-2.99590509293561,-1.,2.4175732450056));
#51695=CARTESIAN_POINT('Ctrl Pts',(-3.00264868586038,-1.,2.42090763946812));
#51696=CARTESIAN_POINT('Ctrl Pts',(-3.00946442616674,-1.,2.42421849439625));
#51697=CARTESIAN_POINT('Ctrl Pts',(-3.01630420830494,-1.,2.4274685626416));
#51698=CARTESIAN_POINT('Ctrl Pts',(-3.02313656035977,-1.,2.43063415586615));
#51699=CARTESIAN_POINT('Ctrl Pts',(-3.02995534946946,-1.,2.43371241361462));
#51700=CARTESIAN_POINT('Ctrl Pts',(-3.03676949672797,-1.,2.43671278042394));
#51701=CARTESIAN_POINT('Ctrl Pts',(-3.04359685040545,-1.,2.43965194061849));
#51702=CARTESIAN_POINT('Ctrl Pts',(-3.05045678021509,-1.,2.44254768923109));
#51703=CARTESIAN_POINT('Ctrl Pts',(-3.05736242671521,-1.,2.44541251892568));
#51704=CARTESIAN_POINT('Ctrl Pts',(-3.06431596421422,-1.,2.44824970516558));
#51705=CARTESIAN_POINT('Ctrl Pts',(-3.0713129052131,-1.,2.45105688854432));
#51706=CARTESIAN_POINT('Ctrl Pts',(-3.07834472886145,-1.,2.45382826787795));
#51707=CARTESIAN_POINT('Ctrl Pts',(-3.08540206545313,-1.,2.45655725437037));
#51708=CARTESIAN_POINT('Ctrl Pts',(-3.09247787931881,-1.,2.45923912563875));
#51709=CARTESIAN_POINT('Ctrl Pts',(-3.09956993697048,-1.,2.4618730850188));
#51710=CARTESIAN_POINT('Ctrl Pts',(-3.10667907901981,-1.,2.46446082979645));
#51711=CARTESIAN_POINT('Ctrl Pts',(-3.11380805536124,-1.,2.46700558843507));
#51712=CARTESIAN_POINT('Ctrl Pts',(-3.12096015766984,-1.,2.4695109894747));
#51713=CARTESIAN_POINT('Ctrl Pts',(-3.12813790805948,-1.,2.47197997765868));
#51714=CARTESIAN_POINT('Ctrl Pts',(-3.13534181229282,-1.,2.47441378371923));
#51715=CARTESIAN_POINT('Ctrl Pts',(-3.14257099546531,-1.,2.47681245356095));
#51716=CARTESIAN_POINT('Ctrl Pts',(-3.14982373241335,-1.,2.47917529057016));
#51717=CARTESIAN_POINT('Ctrl Pts',(-3.15709802322735,-1.,2.48150133566568));
#51718=CARTESIAN_POINT('Ctrl Pts',(-3.16439213290181,-1.,2.48378981792739));
#51719=CARTESIAN_POINT('Ctrl Pts',(-3.17170518863357,-1.,2.48604065348619));
#51720=CARTESIAN_POINT('Ctrl Pts',(-3.17903698136679,-1.,2.48825428288243));
#51721=CARTESIAN_POINT('Ctrl Pts',(-3.18638771282315,-1.,2.49043146334095));
#51722=CARTESIAN_POINT('Ctrl Pts',(-3.19375775555814,-1.,2.4925730723986));
#51723=CARTESIAN_POINT('Ctrl Pts',(-3.20114742397549,-1.,2.49467992057726));
#51724=CARTESIAN_POINT('Ctrl Pts',(-3.2085566984974,-1.,2.49675252647298));
#51725=CARTESIAN_POINT('Ctrl Pts',(-3.21598526261157,-1.,2.49879114599293));
#51726=CARTESIAN_POINT('Ctrl Pts',(-3.22343262620387,-1.,2.5007958720187));
#51727=CARTESIAN_POINT('Ctrl Pts',(-3.23089822320596,-1.,2.50276671338074));
#51728=CARTESIAN_POINT('Ctrl Pts',(-3.23838151080383,-1.,2.50470367580078));
#51729=CARTESIAN_POINT('Ctrl Pts',(-3.24588208984042,-1.,2.50660685940645));
#51730=CARTESIAN_POINT('Ctrl Pts',(-3.25339971461265,-1.,2.50847647070936));
#51731=CARTESIAN_POINT('Ctrl Pts',(-3.26093423001716,-1.,2.51031277813697));
#51732=CARTESIAN_POINT('Ctrl Pts',(-3.26848552888271,-1.,2.51211608411539));
#51733=CARTESIAN_POINT('Ctrl Pts',(-3.27605350473048,-1.,2.51388669270329));
#51734=CARTESIAN_POINT('Ctrl Pts',(-3.28363799702583,-1.,2.51562487464215));
#51735=CARTESIAN_POINT('Ctrl Pts',(-3.2912387729863,-1.,2.51733085123316));
#51736=CARTESIAN_POINT('Ctrl Pts',(-3.29885556387661,-1.,2.51900480700548));
#51737=CARTESIAN_POINT('Ctrl Pts',(-3.30648808814986,-1.,2.52064689568167));
#51738=CARTESIAN_POINT('Ctrl Pts',(-3.31413607874727,-1.,2.52225724871375));
#51739=CARTESIAN_POINT('Ctrl Pts',(-3.32179931079521,-1.,2.52383598396878));
#51740=CARTESIAN_POINT('Ctrl Pts',(-3.32947762189049,-1.,2.52538321165774));
#51741=CARTESIAN_POINT('Ctrl Pts',(-3.33717090000955,-1.,2.52689902691551));
#51742=CARTESIAN_POINT('Ctrl Pts',(-3.34333744117093,-1.,2.52808660916879));
#51743=CARTESIAN_POINT('Ctrl Pts',(-3.34796903577628,-1.,2.5289632161143));
#51744=CARTESIAN_POINT('Ctrl Pts',(-3.35105973714426,-1.,2.52954136549357));
#51745=CARTESIAN_POINT('Ctrl Pts',(-3.35260583073571,-1.,2.52982887637028));
#51746=CARTESIAN_POINT('',(-3.44202241512147,-1.,2.40675750623143));
#51747=CARTESIAN_POINT('',(-3.35260583073571,-1.,2.52982887637028));
#51748=CARTESIAN_POINT('',(-3.14877060440327,-1.,2.03660101169715));
#51749=CARTESIAN_POINT('Ctrl Pts',(-3.44202241512147,-1.,2.40675750623143));
#51750=CARTESIAN_POINT('Ctrl Pts',(-3.44127120683039,-1.,2.4053759295909));
#51751=CARTESIAN_POINT('Ctrl Pts',(-3.43976627484234,-1.,2.40261515589405));
#51752=CARTESIAN_POINT('Ctrl Pts',(-3.43750133064416,-1.,2.39848113410292));
#51753=CARTESIAN_POINT('Ctrl Pts',(-3.4344663067854,-1.,2.39298338804493));
#51754=CARTESIAN_POINT('Ctrl Pts',(-3.4306473271292,-1.,2.38613505843552));
#51755=CARTESIAN_POINT('Ctrl Pts',(-3.42680309754399,-1.,2.37931067028926));
#51756=CARTESIAN_POINT('Ctrl Pts',(-3.42293356216511,-1.,2.37251035954292));
#51757=CARTESIAN_POINT('Ctrl Pts',(-3.41903866635852,-1.,2.36573431470642));
#51758=CARTESIAN_POINT('Ctrl Pts',(-3.41511836751469,-1.,2.35898278606946));
#51759=CARTESIAN_POINT('Ctrl Pts',(-3.41117262314119,-1.,2.35225606824109));
#51760=CARTESIAN_POINT('Ctrl Pts',(-3.40720137404297,-1.,2.34555447649188));
#51761=CARTESIAN_POINT('Ctrl Pts',(-3.40320452776743,-1.,2.33887832342782));
#51762=CARTESIAN_POINT('Ctrl Pts',(-3.39918194577956,-1.,2.33222789882489));
#51763=CARTESIAN_POINT('Ctrl Pts',(-3.39513342019756,-1.,2.3256034390248));
#51764=CARTESIAN_POINT('Ctrl Pts',(-3.39105869474822,-1.,2.31900513925424));
#51765=CARTESIAN_POINT('Ctrl Pts',(-3.38695751492462,-1.,2.31243319489367));
#51766=CARTESIAN_POINT('Ctrl Pts',(-3.3828296733661,-1.,2.30588783640343));
#51767=CARTESIAN_POINT('Ctrl Pts',(-3.37867504959433,-1.,2.29936936127624));
#51768=CARTESIAN_POINT('Ctrl Pts',(-3.37449367172826,-1.,2.29287818007393));
#51769=CARTESIAN_POINT('Ctrl Pts',(-3.37028570206488,-1.,2.28641481081137));
#51770=CARTESIAN_POINT('Ctrl Pts',(-3.36605130713076,-1.,2.27997979458037));
#51771=CARTESIAN_POINT('Ctrl Pts',(-3.36179055004409,-1.,2.2735736262093));
#51772=CARTESIAN_POINT('Ctrl Pts',(-3.35750328523061,-1.,2.2671966857991));
#51773=CARTESIAN_POINT('Ctrl Pts',(-3.35318902552626,-1.,2.26084915222449));
#51774=CARTESIAN_POINT('Ctrl Pts',(-3.34884690292285,-1.,2.25453097693483));
#51775=CARTESIAN_POINT('Ctrl Pts',(-3.34447596770723,-1.,2.24824207678256));
#51776=CARTESIAN_POINT('Ctrl Pts',(-3.34007543738025,-1.,2.24198249391422));
#51777=CARTESIAN_POINT('Ctrl Pts',(-3.33564495756482,-1.,2.23575256328812));
#51778=CARTESIAN_POINT('Ctrl Pts',(-3.33118487773611,-1.,2.22955308907233));
#51779=CARTESIAN_POINT('Ctrl Pts',(-3.3266964672289,-1.,2.22338548312772));
#51780=CARTESIAN_POINT('Ctrl Pts',(-3.32218125618968,-1.,2.21725135110898));
#51781=CARTESIAN_POINT('Ctrl Pts',(-3.31764044024235,-1.,2.21115211847875));
#51782=CARTESIAN_POINT('Ctrl Pts',(-3.31307424608949,-1.,2.20508863150607));
#51783=CARTESIAN_POINT('Ctrl Pts',(-3.30848134694595,-1.,2.19906078949923));
#51784=CARTESIAN_POINT('Ctrl Pts',(-3.30385816281831,-1.,2.19306710376111));
#51785=CARTESIAN_POINT('Ctrl Pts',(-3.29920022557639,-1.,2.18710556500327));
#51786=CARTESIAN_POINT('Ctrl Pts',(-3.2945036150049,-1.,2.18117455557065));
#51787=CARTESIAN_POINT('Ctrl Pts',(-3.28976645712568,-1.,2.17527380048423));
#51788=CARTESIAN_POINT('Ctrl Pts',(-3.28499019979724,-1.,2.16940517773455));
#51789=CARTESIAN_POINT('Ctrl Pts',(-3.280181508414,-1.,2.16357391934425));
#51790=CARTESIAN_POINT('Ctrl Pts',(-3.27534954469187,-1.,2.15778690038347));
#51791=CARTESIAN_POINT('Ctrl Pts',(-3.27050245897228,-1.,2.15205043199808));
#51792=CARTESIAN_POINT('Ctrl Pts',(-3.26564388189759,-1.,2.1463680529566));
#51793=CARTESIAN_POINT('Ctrl Pts',(-3.26077002641879,-1.,2.14073870754264));
#51794=CARTESIAN_POINT('Ctrl Pts',(-3.25586495065054,-1.,2.13515375878803));
#51795=CARTESIAN_POINT('Ctrl Pts',(-3.25090574494028,-1.,2.12960028396832));
#51796=CARTESIAN_POINT('Ctrl Pts',(-3.24587102613376,-1.,2.12406646410962));
#51797=CARTESIAN_POINT('Ctrl Pts',(-3.24074905517293,-1.,2.11854673326979));
#51798=CARTESIAN_POINT('Ctrl Pts',(-3.23554444767099,-1.,2.11304604021773));
#51799=CARTESIAN_POINT('Ctrl Pts',(-3.23028945793289,-1.,2.10758699642451));
#51800=CARTESIAN_POINT('Ctrl Pts',(-3.22503437553434,-1.,2.10220384298492));
#51801=CARTESIAN_POINT('Ctrl Pts',(-3.21982707347009,-1.,2.09692958434895));
#51802=CARTESIAN_POINT('Ctrl Pts',(-3.21469429601654,-1.,2.09178419460443));
#51803=CARTESIAN_POINT('Ctrl Pts',(-3.20962575845463,-1.,2.08676465517455));
#51804=CARTESIAN_POINT('Ctrl Pts',(-3.2045481863073,-1.,2.08182850370878));
#51805=CARTESIAN_POINT('Ctrl Pts',(-3.19934132836019,-1.,2.07690441870722));
#51806=CARTESIAN_POINT('Ctrl Pts',(-3.19388465568252,-1.,2.07192253497857));
#51807=CARTESIAN_POINT('Ctrl Pts',(-3.18809755562368,-1.,2.06684062744112));
#51808=CARTESIAN_POINT('Ctrl Pts',(-3.18197692964614,-1.,2.06166849827101));
#51809=CARTESIAN_POINT('Ctrl Pts',(-3.17564906975371,-1.,2.05650186773132));
#51810=CARTESIAN_POINT('Ctrl Pts',(-3.16936341689527,-1.,2.05151770247233));
#51811=CARTESIAN_POINT('Ctrl Pts',(-3.16343165058912,-1.,2.04693331247446));
#51812=CARTESIAN_POINT('Ctrl Pts',(-3.15817983946367,-1.,2.04297406404027));
#51813=CARTESIAN_POINT('Ctrl Pts',(-3.15389991674792,-1.,2.03984073791519));
#51814=CARTESIAN_POINT('Ctrl Pts',(-3.15102344775328,-1.,2.03783225495961));
#51815=CARTESIAN_POINT('Ctrl Pts',(-3.14959882629805,-1.,2.03693188810544));
#51816=CARTESIAN_POINT('Ctrl Pts',(-3.1490119366901,-1.,2.03663974554932));
#51817=CARTESIAN_POINT('Ctrl Pts',(-3.14881939088124,-1.,2.03659701539259));
#51818=CARTESIAN_POINT('Ctrl Pts',(-3.14877060440328,-1.,2.03660101169715));
#51819=CARTESIAN_POINT('',(-3.24413672884812,-1.,1.88097764062697));
#51820=CARTESIAN_POINT('Origin',(0.,-1.,0.));
#51821=CARTESIAN_POINT('',(-3.70708211654725,-1.,1.97421938526992));
#51822=CARTESIAN_POINT('Ctrl Pts',(-3.24413672884812,-1.,1.88097764062697));
#51823=CARTESIAN_POINT('Ctrl Pts',(-3.24415531671284,-1.,1.8810229239812));
#51824=CARTESIAN_POINT('Ctrl Pts',(-3.24428080353022,-1.,1.88117508446775));
#51825=CARTESIAN_POINT('Ctrl Pts',(-3.24480754676064,-1.,1.88156537699203));
#51826=CARTESIAN_POINT('Ctrl Pts',(-3.2462565441079,-1.,1.88242596600454));
#51827=CARTESIAN_POINT('Ctrl Pts',(-3.24935200511918,-1.,1.88407708646357));
#51828=CARTESIAN_POINT('Ctrl Pts',(-3.25408686339463,-1.,1.88646802523466));
#51829=CARTESIAN_POINT('Ctrl Pts',(-3.25999885193947,-1.,1.88934996203698));
#51830=CARTESIAN_POINT('Ctrl Pts',(-3.26677653888676,-1.,1.89255393500965));
#51831=CARTESIAN_POINT('Ctrl Pts',(-3.27407108933139,-1.,1.89589172903793));
#51832=CARTESIAN_POINT('Ctrl Pts',(-3.28154737912352,-1.,1.89918429230462));
#51833=CARTESIAN_POINT('Ctrl Pts',(-3.2889344860029,-1.,1.90228971247527));
#51834=CARTESIAN_POINT('Ctrl Pts',(-3.29608978722113,-1.,1.90513891864087));
#51835=CARTESIAN_POINT('Ctrl Pts',(-3.30300595568195,-1.,1.90773912171341));
#51836=CARTESIAN_POINT('Ctrl Pts',(-3.30975721158596,-1.,1.91014297830446));
#51837=CARTESIAN_POINT('Ctrl Pts',(-3.31646052426364,-1.,1.91242616234442));
#51838=CARTESIAN_POINT('Ctrl Pts',(-3.32323403454535,-1.,1.91466343916628));
#51839=CARTESIAN_POINT('Ctrl Pts',(-3.33014884257873,-1.,1.91690081930331));
#51840=CARTESIAN_POINT('Ctrl Pts',(-3.33721230710012,-1.,1.9191460961021));
#51841=CARTESIAN_POINT('Ctrl Pts',(-3.34439448941961,-1.,1.92138450828404));
#51842=CARTESIAN_POINT('Ctrl Pts',(-3.35164424847223,-1.,1.92358838440528));
#51843=CARTESIAN_POINT('Ctrl Pts',(-3.35890824422965,-1.,1.92572846125756));
#51844=CARTESIAN_POINT('Ctrl Pts',(-3.36615168657567,-1.,1.92778626543786));
#51845=CARTESIAN_POINT('Ctrl Pts',(-3.37336807068043,-1.,1.92975993109877));
#51846=CARTESIAN_POINT('Ctrl Pts',(-3.3805676852555,-1.,1.93165739093276));
#51847=CARTESIAN_POINT('Ctrl Pts',(-3.38777076883256,-1.,1.93349233176788));
#51848=CARTESIAN_POINT('Ctrl Pts',(-3.39499923640795,-1.,1.93527929945985));
#51849=CARTESIAN_POINT('Ctrl Pts',(-3.40226802104109,-1.,1.93702857723098));
#51850=CARTESIAN_POINT('Ctrl Pts',(-3.40957978266642,-1.,1.93874306008143));
#51851=CARTESIAN_POINT('Ctrl Pts',(-3.41692971994096,-1.,1.94042111965246));
#51852=CARTESIAN_POINT('Ctrl Pts',(-3.42430850941503,-1.,1.94205835913696));
#51853=CARTESIAN_POINT('Ctrl Pts',(-3.43170586602434,-1.,1.94364973660284));
#51854=CARTESIAN_POINT('Ctrl Pts',(-3.43911410197687,-1.,1.94519168842879));
#51855=CARTESIAN_POINT('Ctrl Pts',(-3.44653088665681,-1.,1.94668377715329));
#51856=CARTESIAN_POINT('Ctrl Pts',(-3.45395731584051,-1.,1.94812754766524));
#51857=CARTESIAN_POINT('Ctrl Pts',(-3.46139661060962,-1.,1.94952575850197));
#51858=CARTESIAN_POINT('Ctrl Pts',(-3.46885258974191,-1.,1.95088147859876));
#51859=CARTESIAN_POINT('Ctrl Pts',(-3.47632820495921,-1.,1.95219722189876));
#51860=CARTESIAN_POINT('Ctrl Pts',(-3.48382414832634,-1.,1.95347412486308));
#51861=CARTESIAN_POINT('Ctrl Pts',(-3.49133956289133,-1.,1.95471236969643));
#51862=CARTESIAN_POINT('Ctrl Pts',(-3.49887263575583,-1.,1.95591153823661));
#51863=CARTESIAN_POINT('Ctrl Pts',(-3.50642124159909,-1.,1.95707099606511));
#51864=CARTESIAN_POINT('Ctrl Pts',(-3.51398354617794,-1.,1.95819025316779));
#51865=CARTESIAN_POINT('Ctrl Pts',(-3.52155867431486,-1.,1.95926936324461));
#51866=CARTESIAN_POINT('Ctrl Pts',(-3.52914648844351,-1.,1.96030879411566));
#51867=CARTESIAN_POINT('Ctrl Pts',(-3.53674730625813,-1.,1.96130926212689));
#51868=CARTESIAN_POINT('Ctrl Pts',(-3.54436163300443,-1.,1.96227157573067));
#51869=CARTESIAN_POINT('Ctrl Pts',(-3.55198990600886,-1.,1.96319648628644));
#51870=CARTESIAN_POINT('Ctrl Pts',(-3.55963218706096,-1.,1.96408450906812));
#51871=CARTESIAN_POINT('Ctrl Pts',(-3.56728820357791,-1.,1.96493594634567));
#51872=CARTESIAN_POINT('Ctrl Pts',(-3.57495748600959,-1.,1.96575096652789));
#51873=CARTESIAN_POINT('Ctrl Pts',(-3.58263947663829,-1.,1.96652966688911));
#51874=CARTESIAN_POINT('Ctrl Pts',(-3.59033364022801,-1.,1.96727213799544));
#51875=CARTESIAN_POINT('Ctrl Pts',(-3.59803959819938,-1.,1.96797854118369));
#51876=CARTESIAN_POINT('Ctrl Pts',(-3.60575714017989,-1.,1.9686491188594));
#51877=CARTESIAN_POINT('Ctrl Pts',(-3.61348615496704,-1.,1.96928416040877));
#51878=CARTESIAN_POINT('Ctrl Pts',(-3.62122658401893,-1.,1.96988398129978));
#51879=CARTESIAN_POINT('Ctrl Pts',(-3.62897836973293,-1.,1.97044889850463));
#51880=CARTESIAN_POINT('Ctrl Pts',(-3.63674139590412,-1.,1.97097920454464));
#51881=CARTESIAN_POINT('Ctrl Pts',(-3.64451546723514,-1.,1.97147515441164));
#51882=CARTESIAN_POINT('Ctrl Pts',(-3.652300347166,-1.,1.9719369724024));
#51883=CARTESIAN_POINT('Ctrl Pts',(-3.6600957816636,-1.,1.9723648543905));
#51884=CARTESIAN_POINT('Ctrl Pts',(-3.66790152752075,-1.,1.97275897198678));
#51885=CARTESIAN_POINT('Ctrl Pts',(-3.67571738107084,-1.,1.97311947678516));
#51886=CARTESIAN_POINT('Ctrl Pts',(-3.68354319915092,-1.,1.97344650304519));
#51887=CARTESIAN_POINT('Ctrl Pts',(-3.69137888599902,-1.,1.97374016225483));
#51888=CARTESIAN_POINT('Ctrl Pts',(-3.6976552856004,-1.,1.97394846383216));
#51889=CARTESIAN_POINT('Ctrl Pts',(-3.70236698912904,-1.,1.97408973726715));
#51890=CARTESIAN_POINT('Ctrl Pts',(-3.70551008132332,-1.,1.97417727645308));
#51891=CARTESIAN_POINT('Ctrl Pts',(-3.70708211654725,-1.,1.97421938526992));
#51892=CARTESIAN_POINT('',(-3.77614523045147,-1.,1.8386753923786));
#51893=CARTESIAN_POINT('',(-3.70708211654725,-1.,1.97421938526992));
#51894=CARTESIAN_POINT('',(-3.42859860294306,-1.,1.5189508286633));
#51895=CARTESIAN_POINT('Ctrl Pts',(-3.77614523045147,-1.,1.8386753923786));
#51896=CARTESIAN_POINT('Ctrl Pts',(-3.77518714457833,-1.,1.83742834010626));
#51897=CARTESIAN_POINT('Ctrl Pts',(-3.77326886064398,-1.,1.83493697934534));
#51898=CARTESIAN_POINT('Ctrl Pts',(-3.77038509817999,-1.,1.83120816955645));
#51899=CARTESIAN_POINT('Ctrl Pts',(-3.76652740353775,-1.,1.82625289220915));
#51900=CARTESIAN_POINT('Ctrl Pts',(-3.76168412707948,-1.,1.82008629694091));
#51901=CARTESIAN_POINT('Ctrl Pts',(-3.75681965683071,-1.,1.8139472983358));
#51902=CARTESIAN_POINT('Ctrl Pts',(-3.75193395887977,-1.,1.80783603939617));
#51903=CARTESIAN_POINT('Ctrl Pts',(-3.74702700875467,-1.,1.8017527148577));
#51904=CARTESIAN_POINT('Ctrl Pts',(-3.74209880352445,-1.,1.79569757859422));
#51905=CARTESIAN_POINT('Ctrl Pts',(-3.73714934730681,-1.,1.78967092823491));
#51906=CARTESIAN_POINT('Ctrl Pts',(-3.7321786309547,-1.,1.78367308442901));
#51907=CARTESIAN_POINT('Ctrl Pts',(-3.72718661205609,-1.,1.77770437039658));
#51908=CARTESIAN_POINT('Ctrl Pts',(-3.72217319911254,-1.,1.77176509401761));
#51909=CARTESIAN_POINT('Ctrl Pts',(-3.71713822377359,-1.,1.76585552124394));
#51910=CARTESIAN_POINT('Ctrl Pts',(-3.71208146346136,-1.,1.75997588498865));
#51911=CARTESIAN_POINT('Ctrl Pts',(-3.70700269736659,-1.,1.75412641804042));
#51912=CARTESIAN_POINT('Ctrl Pts',(-3.7019017567335,-1.,1.74830738046057));
#51913=CARTESIAN_POINT('Ctrl Pts',(-3.69677856910517,-1.,1.74251908492617));
#51914=CARTESIAN_POINT('Ctrl Pts',(-3.69163322648036,-1.,1.73676193254557));
#51915=CARTESIAN_POINT('Ctrl Pts',(-3.68646597019332,-1.,1.73103640956717));
#51916=CARTESIAN_POINT('Ctrl Pts',(-3.68127704936579,-1.,1.72534302437056));
#51917=CARTESIAN_POINT('Ctrl Pts',(-3.67606660374709,-1.,1.71968225581808));
#51918=CARTESIAN_POINT('Ctrl Pts',(-3.67083454901611,-1.,1.71405450210383));
#51919=CARTESIAN_POINT('Ctrl Pts',(-3.66558043198876,-1.,1.70846001610956));
#51920=CARTESIAN_POINT('Ctrl Pts',(-3.66030338774847,-1.,1.70289888566873));
#51921=CARTESIAN_POINT('Ctrl Pts',(-3.65500246526749,-1.,1.69737117722534));
#51922=CARTESIAN_POINT('Ctrl Pts',(-3.64967689827371,-1.,1.69187705481689));
#51923=CARTESIAN_POINT('Ctrl Pts',(-3.64432638915203,-1.,1.68641690471457));
#51924=CARTESIAN_POINT('Ctrl Pts',(-3.63895140887462,-1.,1.68099146651586));
#51925=CARTESIAN_POINT('Ctrl Pts',(-3.63355343201232,-1.,1.67560193613156));
#51926=CARTESIAN_POINT('Ctrl Pts',(-3.62813422105271,-1.,1.67024966008045));
#51927=CARTESIAN_POINT('Ctrl Pts',(-3.62269517989109,-1.,1.66493585923855));
#51928=CARTESIAN_POINT('Ctrl Pts',(-3.61723666482456,-1.,1.65966133399186));
#51929=CARTESIAN_POINT('Ctrl Pts',(-3.61175734965127,-1.,1.65442619244325));
#51930=CARTESIAN_POINT('Ctrl Pts',(-3.60625346556992,-1.,1.64922952425832));
#51931=CARTESIAN_POINT('Ctrl Pts',(-3.60072028513845,-1.,1.64407004385582));
#51932=CARTESIAN_POINT('Ctrl Pts',(-3.59515368334893,-1.,1.63894676675352));
#51933=CARTESIAN_POINT('Ctrl Pts',(-3.58955176627879,-1.,1.6338597145126));
#51934=CARTESIAN_POINT('Ctrl Pts',(-3.58391625774343,-1.,1.62881051550745));
#51935=CARTESIAN_POINT('Ctrl Pts',(-3.5782545595439,-1.,1.62380329464844));
#51936=CARTESIAN_POINT('Ctrl Pts',(-3.57257679609806,-1.,1.61884340915404));
#51937=CARTESIAN_POINT('Ctrl Pts',(-3.56689200468387,-1.,1.61393581747514));
#51938=CARTESIAN_POINT('Ctrl Pts',(-3.5612043248298,-1.,1.60908344685457));
#51939=CARTESIAN_POINT('Ctrl Pts',(-3.55550985096129,-1.,1.60428584699853));
#51940=CARTESIAN_POINT('Ctrl Pts',(-3.54979148634454,-1.,1.59953698113457));
#51941=CARTESIAN_POINT('Ctrl Pts',(-3.54402458182337,-1.,1.59482766949766));
#51942=CARTESIAN_POINT('Ctrl Pts',(-3.53818616861077,-1.,1.59014958368739));
#51943=CARTESIAN_POINT('Ctrl Pts',(-3.5322637814708,-1.,1.58549906268088));
#51944=CARTESIAN_POINT('Ctrl Pts',(-3.52626275334881,-1.,1.58088027227848));
#51945=CARTESIAN_POINT('Ctrl Pts',(-3.52021847865912,-1.,1.57631049988158));
#51946=CARTESIAN_POINT('Ctrl Pts',(-3.51418598431665,-1.,1.57181569799743));
#51947=CARTESIAN_POINT('Ctrl Pts',(-3.50821771695363,-1.,1.56742097575012));
#51948=CARTESIAN_POINT('Ctrl Pts',(-3.50234321621578,-1.,1.56314187758675));
#51949=CARTESIAN_POINT('Ctrl Pts',(-3.49655185179655,-1.,1.55897703097874));
#51950=CARTESIAN_POINT('Ctrl Pts',(-3.4907646087742,-1.,1.55489595901116));
#51951=CARTESIAN_POINT('Ctrl Pts',(-3.48485155928567,-1.,1.55084702970452));
#51952=CARTESIAN_POINT('Ctrl Pts',(-3.47868272898751,-1.,1.54678009290276));
#51953=CARTESIAN_POINT('Ctrl Pts',(-3.47217189224653,-1.,1.54266605398187));
#51954=CARTESIAN_POINT('Ctrl Pts',(-3.46531752207153,-1.,1.53851507915502));
#51955=CARTESIAN_POINT('Ctrl Pts',(-3.45825932955032,-1.,1.53440195378792));
#51956=CARTESIAN_POINT('Ctrl Pts',(-3.45127136828305,-1.,1.53046244461635));
#51957=CARTESIAN_POINT('Ctrl Pts',(-3.44469547526647,-1.,1.52686242875556));
#51958=CARTESIAN_POINT('Ctrl Pts',(-3.4388889597401,-1.,1.5237734895035));
#51959=CARTESIAN_POINT('Ctrl Pts',(-3.43417156977893,-1.,1.52134826724292));
#51960=CARTESIAN_POINT('Ctrl Pts',(-3.43101631893414,-1.,1.5198144909338));
#51961=CARTESIAN_POINT('Ctrl Pts',(-3.42946838852587,-1.,1.51914806898491));
#51962=CARTESIAN_POINT('Ctrl Pts',(-3.42884302333841,-1.,1.5189513329503));
#51963=CARTESIAN_POINT('Ctrl Pts',(-3.42864616361875,-1.,1.51893924967331));
#51964=CARTESIAN_POINT('Ctrl Pts',(-3.42859860294306,-1.,1.5189508286633));
#51965=CARTESIAN_POINT('',(-3.49844575334386,-1.,1.35032489087269));
#51966=CARTESIAN_POINT('Origin',(0.,-1.,0.));
#51967=CARTESIAN_POINT('',(-3.97027773754922,-1.,1.36999806084572));
#51968=CARTESIAN_POINT('Ctrl Pts',(-3.49844575334386,-1.,1.35032489087269));
#51969=CARTESIAN_POINT('Ctrl Pts',(-3.49847119623841,-1.,1.35036670893102));
#51970=CARTESIAN_POINT('Ctrl Pts',(-3.49861894124915,-1.,1.35049736560633));
#51971=CARTESIAN_POINT('Ctrl Pts',(-3.49920025459856,-1.,1.35080045218652));
#51972=CARTESIAN_POINT('Ctrl Pts',(-3.5007660381658,-1.,1.35142377279535));
#51973=CARTESIAN_POINT('Ctrl Pts',(-3.50408168106113,-1.,1.3525703284343));
#51974=CARTESIAN_POINT('Ctrl Pts',(-3.50913227060177,-1.,1.35419113576022));
#51975=CARTESIAN_POINT('Ctrl Pts',(-3.51542230699919,-1.,1.35611275237288));
#51976=CARTESIAN_POINT('Ctrl Pts',(-3.52261776117121,-1.,1.35821701528975));
#51977=CARTESIAN_POINT('Ctrl Pts',(-3.53034464961849,-1.,1.36037259643827));
#51978=CARTESIAN_POINT('Ctrl Pts',(-3.53824396425032,-1.,1.36245507339334));
#51979=CARTESIAN_POINT('Ctrl Pts',(-3.54602591832893,-1.,1.36436666257567));
#51980=CARTESIAN_POINT('Ctrl Pts',(-3.55353883995793,-1.,1.36606145456711));
#51981=CARTESIAN_POINT('Ctrl Pts',(-3.56077662028492,-1.,1.36754771771174));
#51982=CARTESIAN_POINT('Ctrl Pts',(-3.56782080304554,-1.,1.36886584973349));
#51983=CARTESIAN_POINT('Ctrl Pts',(-3.57479875549453,-1.,1.37007229485646));
#51984=CARTESIAN_POINT('Ctrl Pts',(-3.58183885982745,-1.,1.37122241663073));
#51985=CARTESIAN_POINT('Ctrl Pts',(-3.5890185384643,-1.,1.37235053661));
#51986=CARTESIAN_POINT('Ctrl Pts',(-3.59634627869117,-1.,1.37346320103184));
#51987=CARTESIAN_POINT('Ctrl Pts',(-3.60379020124038,-1.,1.37455051379642));
#51988=CARTESIAN_POINT('Ctrl Pts',(-3.61129546591082,-1.,1.37559314436641));
#51989=CARTESIAN_POINT('Ctrl Pts',(-3.61880481160408,-1.,1.37657053403102));
#51990=CARTESIAN_POINT('Ctrl Pts',(-3.62628098665112,-1.,1.37746987919868));
#51991=CARTESIAN_POINT('Ctrl Pts',(-3.63371727442448,-1.,1.37829035457324));
#51992=CARTESIAN_POINT('Ctrl Pts',(-3.64112507791112,-1.,1.37903818567347));
#51993=CARTESIAN_POINT('Ctrl Pts',(-3.64852652756444,-1.,1.37972372481598));
#51994=CARTESIAN_POINT('Ctrl Pts',(-3.65594554404396,-1.,1.38035791051215));
#51995=CARTESIAN_POINT('Ctrl Pts',(-3.66339848520874,-1.,1.38094856333558));
#51996=CARTESIAN_POINT('Ctrl Pts',(-3.67088843112282,-1.,1.38149812653876));
#51997=CARTESIAN_POINT('Ctrl Pts',(-3.6784103848243,-1.,1.38200574290626));
#51998=CARTESIAN_POINT('Ctrl Pts',(-3.68595444983844,-1.,1.38246852827185));
#51999=CARTESIAN_POINT('Ctrl Pts',(-3.69350967899523,-1.,1.38288311171649));
#52000=CARTESIAN_POINT('Ctrl Pts',(-3.70106792167894,-1.,1.38324717612862));
#52001=CARTESIAN_POINT('Ctrl Pts',(-3.70862680753343,-1.,1.38356065402122));
#52002=CARTESIAN_POINT('Ctrl Pts',(-3.7161876605181,-1.,1.38382489984585));
#52003=CARTESIAN_POINT('Ctrl Pts',(-3.72375409358805,-1.,1.3840421342895));
#52004=CARTESIAN_POINT('Ctrl Pts',(-3.73133035859283,-1.,1.38421479111531));
#52005=CARTESIAN_POINT('Ctrl Pts',(-3.73891976418099,-1.,1.38434489156456));
#52006=CARTESIAN_POINT('Ctrl Pts',(-3.7465231716786,-1.,1.38443344984389));
#52007=CARTESIAN_POINT('Ctrl Pts',(-3.75413976318727,-1.,1.38448077997155));
#52008=CARTESIAN_POINT('Ctrl Pts',(-3.76176768271347,-1.,1.38448675253343));
#52009=CARTESIAN_POINT('Ctrl Pts',(-3.76940473185775,-1.,1.38445107339517));
#52010=CARTESIAN_POINT('Ctrl Pts',(-3.77704902230441,-1.,1.38437354551435));
#52011=CARTESIAN_POINT('Ctrl Pts',(-3.78469969805134,-1.,1.38425435883773));
#52012=CARTESIAN_POINT('Ctrl Pts',(-3.79235669640907,-1.,1.38409399694588));
#52013=CARTESIAN_POINT('Ctrl Pts',(-3.80002044322169,-1.,1.38389311766701));
#52014=CARTESIAN_POINT('Ctrl Pts',(-3.80769156398429,-1.,1.38365244046226));
#52015=CARTESIAN_POINT('Ctrl Pts',(-3.81537060817765,-1.,1.38337263902766));
#52016=CARTESIAN_POINT('Ctrl Pts',(-3.82305771743715,-1.,1.38305421262724));
#52017=CARTESIAN_POINT('Ctrl Pts',(-3.83075266982138,-1.,1.38269750245086));
#52018=CARTESIAN_POINT('Ctrl Pts',(-3.83845502790609,-1.,1.38230274828774));
#52019=CARTESIAN_POINT('Ctrl Pts',(-3.84616425605705,-1.,1.38187013346089));
#52020=CARTESIAN_POINT('Ctrl Pts',(-3.85387983979557,-1.,1.38139983115075));
#52021=CARTESIAN_POINT('Ctrl Pts',(-3.86160143044187,-1.,1.38089205993067));
#52022=CARTESIAN_POINT('Ctrl Pts',(-3.86932885813403,-1.,1.38034709213129));
#52023=CARTESIAN_POINT('Ctrl Pts',(-3.87706205830865,-1.,1.37976523097187));
#52024=CARTESIAN_POINT('Ctrl Pts',(-3.88480102249461,-1.,1.37914679719446));
#52025=CARTESIAN_POINT('Ctrl Pts',(-3.89254574338385,-1.,1.37849211287981));
#52026=CARTESIAN_POINT('Ctrl Pts',(-3.90029615196255,-1.,1.3778014851263));
#52027=CARTESIAN_POINT('Ctrl Pts',(-3.90805209522729,-1.,1.3770751963376));
#52028=CARTESIAN_POINT('Ctrl Pts',(-3.91581337461825,-1.,1.37631350505516));
#52029=CARTESIAN_POINT('Ctrl Pts',(-3.92357976987132,-1.,1.37551664448057));
#52030=CARTESIAN_POINT('Ctrl Pts',(-3.93135106761941,-1.,1.37468482215784));
#52031=CARTESIAN_POINT('Ctrl Pts',(-3.93912709041791,-1.,1.37381821967499));
#52032=CARTESIAN_POINT('Ctrl Pts',(-3.94690771786926,-1.,1.37291699203423));
#52033=CARTESIAN_POINT('Ctrl Pts',(-3.95469287283105,-1.,1.37198126433139));
#52034=CARTESIAN_POINT('Ctrl Pts',(-3.96092458508407,-1.,1.37120515615663));
#52035=CARTESIAN_POINT('Ctrl Pts',(-3.96560037975788,-1.,1.37060761746027));
#52036=CARTESIAN_POINT('Ctrl Pts',(-3.9687184694173,-1.,1.37020239094758));
#52037=CARTESIAN_POINT('Ctrl Pts',(-3.97027773754922,-1.,1.36999806084572));
#52038=CARTESIAN_POINT('',(-4.01728681790024,-1.,1.22531898815164));
#52039=CARTESIAN_POINT('',(-3.97027773754922,-1.,1.36999806084572));
#52040=CARTESIAN_POINT('',(-3.62400312501199,-1.,0.963899035118985));
#52041=CARTESIAN_POINT('Ctrl Pts',(-4.01728681790024,-1.,1.22531898815164));
#52042=CARTESIAN_POINT('Ctrl Pts',(-4.01614544569895,-1.,1.22423716681317));
#52043=CARTESIAN_POINT('Ctrl Pts',(-4.01386104433519,-1.,1.22207656455845));
#52044=CARTESIAN_POINT('Ctrl Pts',(-4.01042947140789,-1.,1.21884478244403));
#52045=CARTESIAN_POINT('Ctrl Pts',(-4.00584409522722,-1.,1.21455398918133));
#52046=CARTESIAN_POINT('Ctrl Pts',(-4.00009577950721,-1.,1.20922097029551));
#52047=CARTESIAN_POINT('Ctrl Pts',(-3.99433084799666,-1.,1.20391852375139));
#52048=CARTESIAN_POINT('Ctrl Pts',(-3.98854928957189,-1.,1.19864679609566));
#52049=CARTESIAN_POINT('Ctrl Pts',(-3.98275111052561,-1.,1.19340598349475));
#52050=CARTESIAN_POINT('Ctrl Pts',(-3.97693634767754,-1.,1.18819633715539));
#52051=CARTESIAN_POINT('Ctrl Pts',(-3.97110505165415,-1.,1.18301815039831));
#52052=CARTESIAN_POINT('Ctrl Pts',(-3.96525726358159,-1.,1.17787174135592));
#52053=CARTESIAN_POINT('Ctrl Pts',(-3.95939299213276,-1.,1.17275743590361));
#52054=CARTESIAN_POINT('Ctrl Pts',(-3.95351219509876,-1.,1.16767555244438));
#52055=CARTESIAN_POINT('Ctrl Pts',(-3.94761474780583,-1.,1.16262637999157));
#52056=CARTESIAN_POINT('Ctrl Pts',(-3.94170046685203,-1.,1.15761018340956));
#52057=CARTESIAN_POINT('Ctrl Pts',(-3.9357691705628,-1.,1.1526272271632));
#52058=CARTESIAN_POINT('Ctrl Pts',(-3.92982073294257,-1.,1.14767779451123));
#52059=CARTESIAN_POINT('Ctrl Pts',(-3.92385513133997,-1.,1.14276220561593));
#52060=CARTESIAN_POINT('Ctrl Pts',(-3.91787251936827,-1.,1.13788084225554));
#52061=CARTESIAN_POINT('Ctrl Pts',(-3.91187321145649,-1.,1.13303414693896));
#52062=CARTESIAN_POINT('Ctrl Pts',(-3.90585753318737,-1.,1.12822258281553));
#52063=CARTESIAN_POINT('Ctrl Pts',(-3.89982569750025,-1.,1.12344660099043));
#52064=CARTESIAN_POINT('Ctrl Pts',(-3.89377768340344,-1.,1.11870660794603));
#52065=CARTESIAN_POINT('Ctrl Pts',(-3.88771308285171,-1.,1.11400292434429));
#52066=CARTESIAN_POINT('Ctrl Pts',(-3.88163105531724,-1.,1.10933577224008));
#52067=CARTESIAN_POINT('Ctrl Pts',(-3.87553067187514,-1.,1.10470536603287));
#52068=CARTESIAN_POINT('Ctrl Pts',(-3.86941120134849,-1.,1.10011198761195));
#52069=CARTESIAN_POINT('Ctrl Pts',(-3.86327241021247,-1.,1.09555606505013));
#52070=CARTESIAN_POINT('Ctrl Pts',(-3.85711487933931,-1.,1.09103825516294));
#52071=CARTESIAN_POINT('Ctrl Pts',(-3.85094025222713,-1.,1.08655950846384));
#52072=CARTESIAN_POINT('Ctrl Pts',(-3.8447504803063,-1.,1.08212087917991));
#52073=CARTESIAN_POINT('Ctrl Pts',(-3.83854714117491,-1.,1.07772335353858));
#52074=CARTESIAN_POINT('Ctrl Pts',(-3.83233071195144,-1.,1.07336766633459));
#52075=CARTESIAN_POINT('Ctrl Pts',(-3.82609989967276,-1.,1.06905413180359));
#52076=CARTESIAN_POINT('Ctrl Pts',(-3.81985083953012,-1.,1.0647824403893));
#52077=CARTESIAN_POINT('Ctrl Pts',(-3.8135786611749,-1.,1.06055206187299));
#52078=CARTESIAN_POINT('Ctrl Pts',(-3.80727913637791,-1.,1.05636266918644));
#52079=CARTESIAN_POINT('Ctrl Pts',(-3.80095039790681,-1.,1.05221457990016));
#52080=CARTESIAN_POINT('Ctrl Pts',(-3.79459440308786,-1.,1.04810913267639));
#52081=CARTESIAN_POINT('Ctrl Pts',(-3.78821910787179,-1.,1.04404924374422));
#52082=CARTESIAN_POINT('Ctrl Pts',(-3.7818353500817,-1.,1.04003862055798));
#52083=CARTESIAN_POINT('Ctrl Pts',(-3.77545283140427,-1.,1.03608074678008));
#52084=CARTESIAN_POINT('Ctrl Pts',(-3.76907609832516,-1.,1.03217786604919));
#52085=CARTESIAN_POINT('Ctrl Pts',(-3.76270122291245,-1.,1.02833014458184));
#52086=CARTESIAN_POINT('Ctrl Pts',(-3.75631037456224,-1.,1.02453429444668));
#52087=CARTESIAN_POINT('Ctrl Pts',(-3.74987777155873,-1.,1.02078510487439));
#52088=CARTESIAN_POINT('Ctrl Pts',(-3.74337942504993,-1.,1.01707794311088));
#52089=CARTESIAN_POINT('Ctrl Pts',(-3.73680245055747,-1.,1.01341114319906));
#52090=CARTESIAN_POINT('Ctrl Pts',(-3.73015276704407,-1.,1.00978798539491));
#52091=CARTESIAN_POINT('Ctrl Pts',(-3.72346803750544,-1.,1.00622000735696));
#52092=CARTESIAN_POINT('Ctrl Pts',(-3.71680667125047,-1.,1.00272423396802));
#52093=CARTESIAN_POINT('Ctrl Pts',(-3.7102243971387,-1.,0.999317260756344));
#52094=CARTESIAN_POINT('Ctrl Pts',(-3.70375282282107,-1.,0.996009819772431));
#52095=CARTESIAN_POINT('Ctrl Pts',(-3.69738123415696,-1.,0.992802218332103));
#52096=CARTESIAN_POINT('Ctrl Pts',(-3.69102682138955,-1.,0.989676715398858));
#52097=CARTESIAN_POINT('Ctrl Pts',(-3.6845531792623,-1.,0.986602639864285));
#52098=CARTESIAN_POINT('Ctrl Pts',(-3.67782408841876,-1.,0.983550791470864));
#52099=CARTESIAN_POINT('Ctrl Pts',(-3.67074983340444,-1.,0.980505922458494));
#52100=CARTESIAN_POINT('Ctrl Pts',(-3.66333049637403,-1.,0.977478312751416));
#52101=CARTESIAN_POINT('Ctrl Pts',(-3.6557157673487,-1.,0.974519971354138));
#52102=CARTESIAN_POINT('Ctrl Pts',(-3.64819756447072,-1.,0.971722122060277));
#52103=CARTESIAN_POINT('Ctrl Pts',(-3.64113946505393,-1.,0.969195124674829));
#52104=CARTESIAN_POINT('Ctrl Pts',(-3.6349212208096,-1.,0.967052554540877));
#52105=CARTESIAN_POINT('Ctrl Pts',(-3.62988252139998,-1.,0.965395153165716));
#52106=CARTESIAN_POINT('Ctrl Pts',(-3.62652618145252,-1.,0.964373850166081));
#52107=CARTESIAN_POINT('Ctrl Pts',(-3.62489305727516,-1.,0.963957782642589));
#52108=CARTESIAN_POINT('Ctrl Pts',(-3.62424461507455,-1.,0.963861297423579));
#52109=CARTESIAN_POINT('Ctrl Pts',(-3.62404828878375,-1.,0.963880158556713));
#52110=CARTESIAN_POINT('Ctrl Pts',(-3.62400312501199,-1.,0.963899035118985));
#52111=CARTESIAN_POINT('',(-3.66661143271648,-1.,0.786422660833743));
#52112=CARTESIAN_POINT('Origin',(0.,-1.,0.));
#52113=CARTESIAN_POINT('',(-4.13571194405636,-1.,0.732042837400619));
#52114=CARTESIAN_POINT('Ctrl Pts',(-3.66661143271648,-1.,0.786422660833743));
#52115=CARTESIAN_POINT('Ctrl Pts',(-3.66664310415236,-1.,0.786459983896781));
#52116=CARTESIAN_POINT('Ctrl Pts',(-3.66680946938396,-1.,0.78656591955989));
#52117=CARTESIAN_POINT('Ctrl Pts',(-3.66743103898844,-1.,0.786774337198499));
#52118=CARTESIAN_POINT('Ctrl Pts',(-3.66907505398769,-1.,0.787145041181588));
#52119=CARTESIAN_POINT('Ctrl Pts',(-3.672529236635,-1.,0.787758799995426));
#52120=CARTESIAN_POINT('Ctrl Pts',(-3.67777119516438,-1.,0.788569566220662));
#52121=CARTESIAN_POINT('Ctrl Pts',(-3.68428439784285,-1.,0.789483546065158));
#52122=CARTESIAN_POINT('Ctrl Pts',(-3.69172044327754,-1.,0.79043628498958));
#52123=CARTESIAN_POINT('Ctrl Pts',(-3.69968940808982,-1.,0.791356575696509));
#52124=CARTESIAN_POINT('Ctrl Pts',(-3.70781724021879,-1.,0.792177688845967));
#52125=CARTESIAN_POINT('Ctrl Pts',(-3.7158024239604,-1.,0.792848377370115));
#52126=CARTESIAN_POINT('Ctrl Pts',(-3.7234879729357,-1.,0.79334702378387));
#52127=CARTESIAN_POINT('Ctrl Pts',(-3.7308691469564,-1.,0.793682750269347));
#52128=CARTESIAN_POINT('Ctrl Pts',(-3.73803280541576,-1.,0.79388270093679));
#52129=CARTESIAN_POINT('Ctrl Pts',(-3.74511357728827,-1.,0.79398270045988));
#52130=CARTESIAN_POINT('Ctrl Pts',(-3.75224692493895,-1.,0.79401734737144));
#52131=CARTESIAN_POINT('Ctrl Pts',(-3.75951468666325,-1.,0.794008429135047));
#52132=CARTESIAN_POINT('Ctrl Pts',(-3.76692626931184,-1.,0.793961083689141));
#52133=CARTESIAN_POINT('Ctrl Pts',(-3.77444863801264,-1.,0.793870523787515));
#52134=CARTESIAN_POINT('Ctrl Pts',(-3.78202460377617,-1.,0.793726235781339));
#52135=CARTESIAN_POINT('Ctrl Pts',(-3.78959439439222,-1.,0.793516871680966));
#52136=CARTESIAN_POINT('Ctrl Pts',(-3.79711921389862,-1.,0.7932356129732));
#52137=CARTESIAN_POINT('Ctrl Pts',(-3.80459229925598,-1.,0.792882695234693));
#52138=CARTESIAN_POINT('Ctrl Pts',(-3.81202588694726,-1.,0.792462483517568));
#52139=CARTESIAN_POINT('Ctrl Pts',(-3.81944345442237,-1.,0.791981740718606));
#52140=CARTESIAN_POINT('Ctrl Pts',(-3.82687033899799,-1.,0.791447528662381));
#52141=CARTESIAN_POINT('Ctrl Pts',(-3.83432392054804,-1.,0.79086501270534));
#52142=CARTESIAN_POINT('Ctrl Pts',(-3.84180762342476,-1.,0.790236124191289));
#52143=CARTESIAN_POINT('Ctrl Pts',(-3.8493163780891,-1.,0.789560798155618));
#52144=CARTESIAN_POINT('Ctrl Pts',(-3.85683995872536,-1.,0.788837734090688));
#52145=CARTESIAN_POINT('Ctrl Pts',(-3.86436702561342,-1.,0.788065315093771));
#52146=CARTESIAN_POINT('Ctrl Pts',(-3.87188916600905,-1.,0.78724252761798));
#52147=CARTESIAN_POINT('Ctrl Pts',(-3.87940402818186,-1.,0.786369675812592));
#52148=CARTESIAN_POINT('Ctrl Pts',(-3.88691313167399,-1.,0.785447890340723));
#52149=CARTESIAN_POINT('Ctrl Pts',(-3.89442039235105,-1.,0.784478799358335));
#52150=CARTESIAN_POINT('Ctrl Pts',(-3.90193039043971,-1.,0.783464141529082));
#52151=CARTESIAN_POINT('Ctrl Pts',(-3.90944671004536,-1.,0.782405395622758));
#52152=CARTESIAN_POINT('Ctrl Pts',(-3.9169703605466,-1.,0.781303428618343));
#52153=CARTESIAN_POINT('Ctrl Pts',(-3.92450058323799,-1.,0.780158678615506));
#52154=CARTESIAN_POINT('Ctrl Pts',(-3.93203552473153,-1.,0.778971308134786));
#52155=CARTESIAN_POINT('Ctrl Pts',(-3.93957296768098,-1.,0.777741370568549));
#52156=CARTESIAN_POINT('Ctrl Pts',(-3.94711101619471,-1.,0.77646896669796));
#52157=CARTESIAN_POINT('Ctrl Pts',(-3.95464885452364,-1.,0.775154418039441));
#52158=CARTESIAN_POINT('Ctrl Pts',(-3.96218649639876,-1.,0.773798212026682));
#52159=CARTESIAN_POINT('Ctrl Pts',(-3.96972446532832,-1.,0.772400931772238));
#52160=CARTESIAN_POINT('Ctrl Pts',(-3.97726349165507,-1.,0.770963190030503));
#52161=CARTESIAN_POINT('Ctrl Pts',(-3.98480422348403,-1.,0.769485566245459));
#52162=CARTESIAN_POINT('Ctrl Pts',(-3.99234687880892,-1.,0.767968531377708));
#52163=CARTESIAN_POINT('Ctrl Pts',(-3.99989129179464,-1.,0.766412457135785));
#52164=CARTESIAN_POINT('Ctrl Pts',(-4.00743706791366,-1.,0.764817648784946));
#52165=CARTESIAN_POINT('Ctrl Pts',(-4.01498370680434,-1.,0.763184371182826));
#52166=CARTESIAN_POINT('Ctrl Pts',(-4.02253072741347,-1.,0.761512875859941));
#52167=CARTESIAN_POINT('Ctrl Pts',(-4.0300778195465,-1.,0.759803433244166));
#52168=CARTESIAN_POINT('Ctrl Pts',(-4.03762485803468,-1.,0.758056338885553));
#52169=CARTESIAN_POINT('Ctrl Pts',(-4.04517182654344,-1.,0.756271902370186));
#52170=CARTESIAN_POINT('Ctrl Pts',(-4.05271876688106,-1.,0.754450441816411));
#52171=CARTESIAN_POINT('Ctrl Pts',(-4.06026572221399,-1.,0.752592276482869));
#52172=CARTESIAN_POINT('Ctrl Pts',(-4.06781267241886,-1.,0.750697720483175));
#52173=CARTESIAN_POINT('Ctrl Pts',(-4.07535951055363,-1.,0.748767076679177));
#52174=CARTESIAN_POINT('Ctrl Pts',(-4.08290608094789,-1.,0.746800631490821));
#52175=CARTESIAN_POINT('Ctrl Pts',(-4.09045220253011,-1.,0.744798649705514));
#52176=CARTESIAN_POINT('Ctrl Pts',(-4.09799769702712,-1.,0.742761369690017));
#52177=CARTESIAN_POINT('Ctrl Pts',(-4.1055424175856,-1.,0.740688998555151));
#52178=CARTESIAN_POINT('Ctrl Pts',(-4.11308626953795,-1.,0.738581708229118));
#52179=CARTESIAN_POINT('Ctrl Pts',(-4.12062919626082,-1.,0.736439634335347));
#52180=CARTESIAN_POINT('Ctrl Pts',(-4.12666277572794,-1.,0.734698226767512));
#52181=CARTESIAN_POINT('Ctrl Pts',(-4.13118752796397,-1.,0.733376589325634));
#52182=CARTESIAN_POINT('Ctrl Pts',(-4.13420383737278,-1.,0.732488575135926));
#52183=CARTESIAN_POINT('Ctrl Pts',(-4.13571194405636,-1.,0.732042837400619));
#52184=CARTESIAN_POINT('',(-4.15950947128175,-1.,0.581791163835814));
#52185=CARTESIAN_POINT('',(-4.13571194405636,-1.,0.732042837400619));
#52186=CARTESIAN_POINT('',(-3.73017266276632,-1.,0.385112848332549));
#52187=CARTESIAN_POINT('Ctrl Pts',(-4.15950947128175,-1.,0.581791163835814));
#52188=CARTESIAN_POINT('Ctrl Pts',(-4.15821291712391,-1.,0.580901211462913));
#52189=CARTESIAN_POINT('Ctrl Pts',(-4.15561864787379,-1.,0.579124568912543));
#52190=CARTESIAN_POINT('Ctrl Pts',(-4.1517237611974,-1.,0.576469391673916));
#52191=CARTESIAN_POINT('Ctrl Pts',(-4.14652361065787,-1.,0.572948736066276));
#52192=CARTESIAN_POINT('Ctrl Pts',(-4.14001179828669,-1.,0.568580610187116));
#52193=CARTESIAN_POINT('Ctrl Pts',(-4.13348835726086,-1.,0.564245279535705));
#52194=CARTESIAN_POINT('Ctrl Pts',(-4.12695329951859,-1.,0.559942890594628));
#52195=CARTESIAN_POINT('Ctrl Pts',(-4.1204066619623,-1.,0.555673636130778));
#52196=CARTESIAN_POINT('Ctrl Pts',(-4.11384852025578,-1.,0.551437758498246));
#52197=CARTESIAN_POINT('Ctrl Pts',(-4.1072789702877,-1.,0.547235539486759));
#52198=CARTESIAN_POINT('Ctrl Pts',(-4.10069810244473,-1.,0.543067286878457));
#52199=CARTESIAN_POINT('Ctrl Pts',(-4.09410597627116,-1.,0.53893332117992));
#52200=CARTESIAN_POINT('Ctrl Pts',(-4.08750259988693,-1.,0.534833963476999));
#52201=CARTESIAN_POINT('Ctrl Pts',(-4.08088789536488,-1.,0.530769518728075));
#52202=CARTESIAN_POINT('Ctrl Pts',(-4.07426172299496,-1.,0.526740277226999));
#52203=CARTESIAN_POINT('Ctrl Pts',(-4.06762394471075,-1.,0.522746528602767));
#52204=CARTESIAN_POINT('Ctrl Pts',(-4.06097448037934,-1.,0.518788572336809));
#52205=CARTESIAN_POINT('Ctrl Pts',(-4.05431335771261,-1.,0.514866728193104));
#52206=CARTESIAN_POINT('Ctrl Pts',(-4.04764078815591,-1.,0.510981349219173));
#52207=CARTESIAN_POINT('Ctrl Pts',(-4.04095715149074,-1.,0.507132823288361));
#52208=CARTESIAN_POINT('Ctrl Pts',(-4.0342628417439,-1.,0.503321556915513));
#52209=CARTESIAN_POINT('Ctrl Pts',(-4.0275581398015,-1.,0.499547962340889));
#52210=CARTESIAN_POINT('Ctrl Pts',(-4.02084308851813,-1.,0.495812444326223));
#52211=CARTESIAN_POINT('Ctrl Pts',(-4.01411733503486,-1.,0.49211538341793));
#52212=CARTESIAN_POINT('Ctrl Pts',(-4.0073800839092,-1.,0.48845713042453));
#52213=CARTESIAN_POINT('Ctrl Pts',(-4.00063045119234,-1.,0.484838042421754));
#52214=CARTESIAN_POINT('Ctrl Pts',(-3.99386775880655,-1.,0.481258512209638));
#52215=CARTESIAN_POINT('Ctrl Pts',(-3.98709184306743,-1.,0.477718999122033));
#52216=CARTESIAN_POINT('Ctrl Pts',(-3.9803033804443,-1.,0.474220061019542));
#52217=CARTESIAN_POINT('Ctrl Pts',(-3.97350414289415,-1.,0.470762379613477));
#52218=CARTESIAN_POINT('Ctrl Pts',(-3.96669622273946,-1.,0.467346690880671));
#52219=CARTESIAN_POINT('Ctrl Pts',(-3.95988133243543,-1.,0.463973722115744));
#52220=CARTESIAN_POINT('Ctrl Pts',(-3.95306005817363,-1.,0.460644124429119));
#52221=CARTESIAN_POINT('Ctrl Pts',(-3.94623117206675,-1.,0.457358410451674));
#52222=CARTESIAN_POINT('Ctrl Pts',(-3.93939080846298,-1.,0.454116879027576));
#52223=CARTESIAN_POINT('Ctrl Pts',(-3.93253407403128,-1.,0.450919768356347));
#52224=CARTESIAN_POINT('Ctrl Pts',(-3.92565674143424,-1.,0.447767416837296));
#52225=CARTESIAN_POINT('Ctrl Pts',(-3.91875701610721,-1.,0.444660430230592));
#52226=CARTESIAN_POINT('Ctrl Pts',(-3.91183704069146,-1.,0.441599824524047));
#52227=CARTESIAN_POINT('Ctrl Pts',(-3.90490512938546,-1.,0.438587235458233));
#52228=CARTESIAN_POINT('Ctrl Pts',(-3.8979725665544,-1.,0.435624629433505));
#52229=CARTESIAN_POINT('Ctrl Pts',(-3.89104947940592,-1.,0.432713929544439));
#52230=CARTESIAN_POINT('Ctrl Pts',(-3.88414070943334,-1.,0.429856640579733));
#52231=CARTESIAN_POINT('Ctrl Pts',(-3.87724240306609,-1.,0.427053541173469));
#52232=CARTESIAN_POINT('Ctrl Pts',(-3.87033643487882,-1.,0.424304173195142));
#52233=CARTESIAN_POINT('Ctrl Pts',(-3.86339652542749,-1.,0.421607423177575));
#52234=CARTESIAN_POINT('Ctrl Pts',(-3.85639825648031,-1.,0.418962468086809));
#52235=CARTESIAN_POINT('Ctrl Pts',(-3.8493286415751,-1.,0.41636967805292));
#52236=CARTESIAN_POINT('Ctrl Pts',(-3.84219403994742,-1.,0.413831367016726));
#52237=CARTESIAN_POINT('Ctrl Pts',(-3.83503345578645,-1.,0.411353038798459));
#52238=CARTESIAN_POINT('Ctrl Pts',(-3.82790724256397,-1.,0.408942371447377));
#52239=CARTESIAN_POINT('Ctrl Pts',(-3.82087303913741,-1.,0.406607038258906));
#52240=CARTESIAN_POINT('Ctrl Pts',(-3.81396374287762,-1.,0.404352694628236));
#52241=CARTESIAN_POINT('Ctrl Pts',(-3.80716881962763,-1.,0.402181320148474));
#52242=CARTESIAN_POINT('Ctrl Pts',(-3.80040370384659,-1.,0.400088346504726));
#52243=CARTESIAN_POINT('Ctrl Pts',(-3.79352887163457,-1.,0.398064818684158));
#52244=CARTESIAN_POINT('Ctrl Pts',(-3.78640521279479,-1.,0.396103205335028));
#52245=CARTESIAN_POINT('Ctrl Pts',(-3.77894173114368,-1.,0.394202481011595));
#52246=CARTESIAN_POINT('Ctrl Pts',(-3.77114011595892,-1.,0.392372786223346));
#52247=CARTESIAN_POINT('Ctrl Pts',(-3.76315635032993,-1.,0.390642072979259));
#52248=CARTESIAN_POINT('Ctrl Pts',(-3.75529302894757,-1.,0.389054775898251));
#52249=CARTESIAN_POINT('Ctrl Pts',(-3.74792651696269,-1.,0.387663020050396));
#52250=CARTESIAN_POINT('Ctrl Pts',(-3.74144965781088,-1.,0.386519576222035));
#52251=CARTESIAN_POINT('Ctrl Pts',(-3.73621371845475,-1.,0.385670806454744));
#52252=CARTESIAN_POINT('Ctrl Pts',(-3.73273893363318,-1.,0.385187124633964));
#52253=CARTESIAN_POINT('Ctrl Pts',(-3.73106082862399,-1.,0.385031656499141));
#52254=CARTESIAN_POINT('Ctrl Pts',(-3.73040527620929,-1.,0.385037797882046));
#52255=CARTESIAN_POINT('Ctrl Pts',(-3.73021431755218,-1.,0.385087139001609));
#52256=CARTESIAN_POINT('Ctrl Pts',(-3.73017266276632,-1.,0.385112848332549));
#52257=CARTESIAN_POINT('',(-3.74449296982994,-1.,0.203156094897895));
#52258=CARTESIAN_POINT('Origin',(0.,-1.,0.));
#52259=CARTESIAN_POINT('',(-4.19931119685982,-1.,0.0760622897878236));
#52260=CARTESIAN_POINT('Ctrl Pts',(-3.74449296982994,-1.,0.203156094897895));
#52261=CARTESIAN_POINT('Ctrl Pts',(-3.74453008995129,-1.,0.203188003947965));
#52262=CARTESIAN_POINT('Ctrl Pts',(-3.74471097893961,-1.,0.203266610111264));
#52263=CARTESIAN_POINT('Ctrl Pts',(-3.74535749969262,-1.,0.203375226874331));
#52264=CARTESIAN_POINT('Ctrl Pts',(-3.74703926501843,-1.,0.203484186269314));
#52265=CARTESIAN_POINT('Ctrl Pts',(-3.75054693397716,-1.,0.203550035479097));
#52266=CARTESIAN_POINT('Ctrl Pts',(-3.75585118707924,-1.,0.203530796848403));
#52267=CARTESIAN_POINT('Ctrl Pts',(-3.76242717937273,-1.,0.203414634707646));
#52268=CARTESIAN_POINT('Ctrl Pts',(-3.76992071595267,-1.,0.203192390045337));
#52269=CARTESIAN_POINT('Ctrl Pts',(-3.77793553476879,-1.,0.202854729699196));
#52270=CARTESIAN_POINT('Ctrl Pts',(-3.78609175019317,-1.,0.202394260512193));
#52271=CARTESIAN_POINT('Ctrl Pts',(-3.79408354187274,-1.,0.201807533800799));
#52272=CARTESIAN_POINT('Ctrl Pts',(-3.80175247447171,-1.,0.201097756307252));
#52273=CARTESIAN_POINT('Ctrl Pts',(-3.80909529318501,-1.,0.20027467943329));
#52274=CARTESIAN_POINT('Ctrl Pts',(-3.81620203429702,-1.,0.199351525297396));
#52275=CARTESIAN_POINT('Ctrl Pts',(-3.82321127348981,-1.,0.19834261690047));
#52276=CARTESIAN_POINT('Ctrl Pts',(-3.83026221776488,-1.,0.197260935827375));
#52277=CARTESIAN_POINT('Ctrl Pts',(-3.83743910616265,-1.,0.196115198971889));
#52278=CARTESIAN_POINT('Ctrl Pts',(-3.84475203347052,-1.,0.194909009460254));
#52279=CARTESIAN_POINT('Ctrl Pts',(-3.85216762264019,-1.,0.193642806777747));
#52280=CARTESIAN_POINT('Ctrl Pts',(-3.85962774407652,-1.,0.192315153044979));
#52281=CARTESIAN_POINT('Ctrl Pts',(-3.8670715862477,-1.,0.190924190418613));
#52282=CARTESIAN_POINT('Ctrl Pts',(-3.87445976418377,-1.,0.189469253358254));
#52283=CARTESIAN_POINT('Ctrl Pts',(-3.88178563496187,-1.,0.187951632512663));
#52284=CARTESIAN_POINT('Ctrl Pts',(-3.88906196725817,-1.,0.186373724985263));
#52285=CARTESIAN_POINT('Ctrl Pts',(-3.89631300742633,-1.,0.184738537728035));
#52286=CARTESIAN_POINT('Ctrl Pts',(-3.90356488555138,-1.,0.183049081993193));
#52287=CARTESIAN_POINT('Ctrl Pts',(-3.91083557557193,-1.,0.181307740731796));
#52288=CARTESIAN_POINT('Ctrl Pts',(-3.91812876180948,-1.,0.179515885822894));
#52289=CARTESIAN_POINT('Ctrl Pts',(-3.92543942697672,-1.,0.177674246152328));
#52290=CARTESIAN_POINT('Ctrl Pts',(-3.93275726771049,-1.,0.175783136893872));
#52291=CARTESIAN_POINT('Ctrl Pts',(-3.94007083096214,-1.,0.173842734974607));
#52292=CARTESIAN_POINT('Ctrl Pts',(-3.94737164900861,-1.,0.171853355369233));
#52293=CARTESIAN_POINT('Ctrl Pts',(-3.95465744665263,-1.,0.16981566637413));
#52294=CARTESIAN_POINT('Ctrl Pts',(-3.96192990160296,-1.,0.167730547023312));
#52295=CARTESIAN_POINT('Ctrl Pts',(-3.9691931362141,-1.,0.165598992851097));
#52296=CARTESIAN_POINT('Ctrl Pts',(-3.97645194630944,-1.,0.163422004609999));
#52297=CARTESIAN_POINT('Ctrl Pts',(-3.98371010319866,-1.,0.161200482186087));
#52298=CARTESIAN_POINT('Ctrl Pts',(-3.99096873945862,-1.,0.158935123982796));
#52299=CARTESIAN_POINT('Ctrl Pts',(-3.99822717425869,-1.,0.156626481393735));
#52300=CARTESIAN_POINT('Ctrl Pts',(-4.00548360245297,-1.,0.15427500487231));
#52301=CARTESIAN_POINT('Ctrl Pts',(-4.01273584234684,-1.,0.151881094022909));
#52302=CARTESIAN_POINT('Ctrl Pts',(-4.01998203715588,-1.,0.149445144968707));
#52303=CARTESIAN_POINT('Ctrl Pts',(-4.02722143147048,-1.,0.146967602878998));
#52304=CARTESIAN_POINT('Ctrl Pts',(-4.03445411510403,-1.,0.144448947038352));
#52305=CARTESIAN_POINT('Ctrl Pts',(-4.04168069633842,-1.,0.141889671485508));
#52306=CARTESIAN_POINT('Ctrl Pts',(-4.04890199238056,-1.,0.139290267180059));
#52307=CARTESIAN_POINT('Ctrl Pts',(-4.05611873400122,-1.,0.136651205046111));
#52308=CARTESIAN_POINT('Ctrl Pts',(-4.06333121018476,-1.,0.133972916144225));
#52309=CARTESIAN_POINT('Ctrl Pts',(-4.07053931528579,-1.,0.131255793548914));
#52310=CARTESIAN_POINT('Ctrl Pts',(-4.07774270738809,-1.,0.128500200484814));
#52311=CARTESIAN_POINT('Ctrl Pts',(-4.08494093372315,-1.,0.125706476822529));
#52312=CARTESIAN_POINT('Ctrl Pts',(-4.09213355850836,-1.,0.122874946249119));
#52313=CARTESIAN_POINT('Ctrl Pts',(-4.09932031767243,-1.,0.120005924388162));
#52314=CARTESIAN_POINT('Ctrl Pts',(-4.10650113382187,-1.,0.117099722731704));
#52315=CARTESIAN_POINT('Ctrl Pts',(-4.11367603925313,-1.,0.114156649609601));
#52316=CARTESIAN_POINT('Ctrl Pts',(-4.12084512502444,-1.,0.111177012683377));
#52317=CARTESIAN_POINT('Ctrl Pts',(-4.12800848371386,-1.,0.10816112052835));
#52318=CARTESIAN_POINT('Ctrl Pts',(-4.13516614458396,-1.,0.105109286538864));
#52319=CARTESIAN_POINT('Ctrl Pts',(-4.14231804938737,-1.,0.102021826577454));
#52320=CARTESIAN_POINT('Ctrl Pts',(-4.1494640891762,-1.,0.0988990478899811));
#52321=CARTESIAN_POINT('Ctrl Pts',(-4.15660412653006,-1.,0.0957412403297067));
#52322=CARTESIAN_POINT('Ctrl Pts',(-4.16373802265942,-1.,0.092548667216769));
#52323=CARTESIAN_POINT('Ctrl Pts',(-4.17086566491823,-1.,0.0893215560850327));
#52324=CARTESIAN_POINT('Ctrl Pts',(-4.17798698669991,-1.,0.0860600915552515));
#52325=CARTESIAN_POINT('Ctrl Pts',(-4.1851019532944,-1.,0.082764416438951));
#52326=CARTESIAN_POINT('Ctrl Pts',(-4.19078883322483,-1.,0.0801005887117603));
#52327=CARTESIAN_POINT('Ctrl Pts',(-4.19505112860624,-1.,0.0780873956244402));
#52328=CARTESIAN_POINT('Ctrl Pts',(-4.19789138621624,-1.,0.0767384596142195));
#52329=CARTESIAN_POINT('Ctrl Pts',(-4.19931119685982,-1.,0.0760622897878236));
#52330=CARTESIAN_POINT('',(-4.19931119685982,-1.,-0.0760622897878246));
#52331=CARTESIAN_POINT('',(-4.19931119685982,-1.,0.0760622897878236));
#52332=CARTESIAN_POINT('',(-3.74449296983004,-1.,-0.203156094896101));
#52333=CARTESIAN_POINT('Ctrl Pts',(-4.19931119685982,-1.,-0.0760622897878246));
#52334=CARTESIAN_POINT('Ctrl Pts',(-4.1978913862118,-1.,-0.0767384596141464));
#52335=CARTESIAN_POINT('Ctrl Pts',(-4.19505112859416,-1.,-0.0780873956242397));
#52336=CARTESIAN_POINT('Ctrl Pts',(-4.19078883320504,-1.,-0.080100588711432));
#52337=CARTESIAN_POINT('Ctrl Pts',(-4.18510195327123,-1.,-0.0827644164385679));
#52338=CARTESIAN_POINT('Ctrl Pts',(-4.17798698668094,-1.,-0.0860600915549397));
#52339=CARTESIAN_POINT('Ctrl Pts',(-4.17086566490794,-1.,-0.0893215560848649));
#52340=CARTESIAN_POINT('Ctrl Pts',(-4.16373802265839,-1.,-0.0925486672167531));
#52341=CARTESIAN_POINT('Ctrl Pts',(-4.15660412653577,-1.,-0.0957412403298007));
#52342=CARTESIAN_POINT('Ctrl Pts',(-4.14946408918485,-1.,-0.0988990478901226));
#52343=CARTESIAN_POINT('Ctrl Pts',(-4.14231804939538,-1.,-0.102021826577584));
#52344=CARTESIAN_POINT('Ctrl Pts',(-4.13516614458895,-1.,-0.105109286538945));
#52345=CARTESIAN_POINT('Ctrl Pts',(-4.12800848371504,-1.,-0.108161120528369));
#52346=CARTESIAN_POINT('Ctrl Pts',(-4.1208451250225,-1.,-0.111177012683347));
#52347=CARTESIAN_POINT('Ctrl Pts',(-4.11367603924961,-1.,-0.114156649609546));
#52348=CARTESIAN_POINT('Ctrl Pts',(-4.10650113381833,-1.,-0.117099722731648));
#52349=CARTESIAN_POINT('Ctrl Pts',(-4.09932031767002,-1.,-0.120005924388124));
#52350=CARTESIAN_POINT('Ctrl Pts',(-4.09213355850756,-1.,-0.122874946249107));
#52351=CARTESIAN_POINT('Ctrl Pts',(-4.08494093372377,-1.,-0.12570647682254));
#52352=CARTESIAN_POINT('Ctrl Pts',(-4.07774270738954,-1.,-0.128500200484838));
#52353=CARTESIAN_POINT('Ctrl Pts',(-4.0705393152874,-1.,-0.13125579354894));
#52354=CARTESIAN_POINT('Ctrl Pts',(-4.06333121018596,-1.,-0.133972916144245));
#52355=CARTESIAN_POINT('Ctrl Pts',(-4.05611873400172,-1.,-0.136651205046119));
#52356=CARTESIAN_POINT('Ctrl Pts',(-4.04890199238036,-1.,-0.139290267180057));
#52357=CARTESIAN_POINT('Ctrl Pts',(-4.04168069633781,-1.,-0.1418896714855));
#52358=CARTESIAN_POINT('Ctrl Pts',(-4.03445411510333,-1.,-0.144448947038345));
#52359=CARTESIAN_POINT('Ctrl Pts',(-4.02722143146994,-1.,-0.146967602878994));
#52360=CARTESIAN_POINT('Ctrl Pts',(-4.01998203715564,-1.,-0.149445144968707));
#52361=CARTESIAN_POINT('Ctrl Pts',(-4.01273584234689,-1.,-0.151881094022911));
#52362=CARTESIAN_POINT('Ctrl Pts',(-4.00548360245319,-1.,-0.154275004872311));
#52363=CARTESIAN_POINT('Ctrl Pts',(-3.99822717425893,-1.,-0.156626481393734));
#52364=CARTESIAN_POINT('Ctrl Pts',(-3.99096873945878,-1.,-0.158935123982793));
#52365=CARTESIAN_POINT('Ctrl Pts',(-3.98371010319872,-1.,-0.161200482186085));
#52366=CARTESIAN_POINT('Ctrl Pts',(-3.97645194630943,-1.,-0.163422004609999));
#52367=CARTESIAN_POINT('Ctrl Pts',(-3.96919313621407,-1.,-0.165598992851102));
#52368=CARTESIAN_POINT('Ctrl Pts',(-3.96192990160296,-1.,-0.167730547023319));
#52369=CARTESIAN_POINT('Ctrl Pts',(-3.95465744665268,-1.,-0.169815666374139));
#52370=CARTESIAN_POINT('Ctrl Pts',(-3.94737164900868,-1.,-0.17185335536924));
#52371=CARTESIAN_POINT('Ctrl Pts',(-3.94007083096217,-1.,-0.17384273497461));
#52372=CARTESIAN_POINT('Ctrl Pts',(-3.93275726771042,-1.,-0.175783136893868));
#52373=CARTESIAN_POINT('Ctrl Pts',(-3.92543942697655,-1.,-0.177674246152317));
#52374=CARTESIAN_POINT('Ctrl Pts',(-3.91812876180926,-1.,-0.179515885822882));
#52375=CARTESIAN_POINT('Ctrl Pts',(-3.91083557557175,-1.,-0.181307740731786));
#52376=CARTESIAN_POINT('Ctrl Pts',(-3.90356488555132,-1.,-0.183049081993191));
#52377=CARTESIAN_POINT('Ctrl Pts',(-3.89631300742646,-1.,-0.184738537728043));
#52378=CARTESIAN_POINT('Ctrl Pts',(-3.88906196725848,-1.,-0.18637372498528));
#52379=CARTESIAN_POINT('Ctrl Pts',(-3.88178563496228,-1.,-0.187951632512685));
#52380=CARTESIAN_POINT('Ctrl Pts',(-3.87445976418412,-1.,-0.189469253358272));
#52381=CARTESIAN_POINT('Ctrl Pts',(-3.86707158624783,-1.,-0.19092419041862));
#52382=CARTESIAN_POINT('Ctrl Pts',(-3.85962774407633,-1.,-0.192315153044971));
#52383=CARTESIAN_POINT('Ctrl Pts',(-3.85216762263966,-1.,-0.193642806777723));
#52384=CARTESIAN_POINT('Ctrl Pts',(-3.84475203346977,-1.,-0.194909009460221));
#52385=CARTESIAN_POINT('Ctrl Pts',(-3.83743910616195,-1.,-0.196115198971859));
#52386=CARTESIAN_POINT('Ctrl Pts',(-3.83026221776456,-1.,-0.197260935827361));
#52387=CARTESIAN_POINT('Ctrl Pts',(-3.82321127349016,-1.,-0.198342616900486));
#52388=CARTESIAN_POINT('Ctrl Pts',(-3.81620203429815,-1.,-0.199351525297447));
#52389=CARTESIAN_POINT('Ctrl Pts',(-3.80909529318669,-1.,-0.200274679433364));
#52390=CARTESIAN_POINT('Ctrl Pts',(-3.80175247447337,-1.,-0.201097756307326));
#52391=CARTESIAN_POINT('Ctrl Pts',(-3.7940835418736,-1.,-0.201807533800837));
#52392=CARTESIAN_POINT('Ctrl Pts',(-3.78609175019242,-1.,-0.20239426051216));
#52393=CARTESIAN_POINT('Ctrl Pts',(-3.77793553476614,-1.,-0.202854729699081));
#52394=CARTESIAN_POINT('Ctrl Pts',(-3.7699207159487,-1.,-0.203192390045164));
#52395=CARTESIAN_POINT('Ctrl Pts',(-3.76242717936885,-1.,-0.203414634707478));
#52396=CARTESIAN_POINT('Ctrl Pts',(-3.75585118707734,-1.,-0.203530796848322));
#52397=CARTESIAN_POINT('Ctrl Pts',(-3.75054693397875,-1.,-0.203550035479166));
#52398=CARTESIAN_POINT('Ctrl Pts',(-3.74703926501752,-1.,-0.203484186269415));
#52399=CARTESIAN_POINT('Ctrl Pts',(-3.74535749969115,-1.,-0.203375226874121));
#52400=CARTESIAN_POINT('Ctrl Pts',(-3.74471097893845,-1.,-0.203266610110531));
#52401=CARTESIAN_POINT('Ctrl Pts',(-3.74453008995092,-1.,-0.203188003946657));
#52402=CARTESIAN_POINT('Ctrl Pts',(-3.74449296983004,-1.,-0.203156094896101));
#52403=CARTESIAN_POINT('',(-3.73017266276651,-1.,-0.385112848330762));
#52404=CARTESIAN_POINT('Origin',(0.,-1.,0.));
#52405=CARTESIAN_POINT('',(-4.15950947128175,-1.,-0.581791163835815));
#52406=CARTESIAN_POINT('Ctrl Pts',(-3.73017266276651,-1.,-0.385112848330762));
#52407=CARTESIAN_POINT('Ctrl Pts',(-3.73021431755274,-1.,-0.385087139000374));
#52408=CARTESIAN_POINT('Ctrl Pts',(-3.73040527621055,-1.,-0.385037797881504));
#52409=CARTESIAN_POINT('Ctrl Pts',(-3.73106082862548,-1.,-0.385031656499164));
#52410=CARTESIAN_POINT('Ctrl Pts',(-3.73273893363406,-1.,-0.385187124634206));
#52411=CARTESIAN_POINT('Ctrl Pts',(-3.73621371845318,-1.,-0.385670806454566));
#52412=CARTESIAN_POINT('Ctrl Pts',(-3.74144965781276,-1.,-0.386519576222251));
#52413=CARTESIAN_POINT('Ctrl Pts',(-3.74792651696654,-1.,-0.387663020050836));
#52414=CARTESIAN_POINT('Ctrl Pts',(-3.75529302895152,-1.,-0.389054775898702));
#52415=CARTESIAN_POINT('Ctrl Pts',(-3.76315635033257,-1.,-0.39064207297956));
#52416=CARTESIAN_POINT('Ctrl Pts',(-3.77114011595967,-1.,-0.392372786223432));
#52417=CARTESIAN_POINT('Ctrl Pts',(-3.77894173114283,-1.,-0.394202481011499));
#52418=CARTESIAN_POINT('Ctrl Pts',(-3.78640521279313,-1.,-0.396103205334841));
#52419=CARTESIAN_POINT('Ctrl Pts',(-3.7935288716329,-1.,-0.398064818683969));
#52420=CARTESIAN_POINT('Ctrl Pts',(-3.80040370384546,-1.,-0.4000883465046));
#52421=CARTESIAN_POINT('Ctrl Pts',(-3.80716881962728,-1.,-0.402181320148436));
#52422=CARTESIAN_POINT('Ctrl Pts',(-3.81396374287793,-1.,-0.404352694628273));
#52423=CARTESIAN_POINT('Ctrl Pts',(-3.8208730391381,-1.,-0.406607038258985));
#52424=CARTESIAN_POINT('Ctrl Pts',(-3.82790724256471,-1.,-0.40894237144746));
#52425=CARTESIAN_POINT('Ctrl Pts',(-3.83503345578698,-1.,-0.411353038798518));
#52426=CARTESIAN_POINT('Ctrl Pts',(-3.84219403994762,-1.,-0.413831367016748));
#52427=CARTESIAN_POINT('Ctrl Pts',(-3.84932864157497,-1.,-0.416369678052907));
#52428=CARTESIAN_POINT('Ctrl Pts',(-3.85639825647996,-1.,-0.418962468086773));
#52429=CARTESIAN_POINT('Ctrl Pts',(-3.86339652542709,-1.,-0.421607423177534));
#52430=CARTESIAN_POINT('Ctrl Pts',(-3.87033643487851,-1.,-0.424304173195111));
#52431=CARTESIAN_POINT('Ctrl Pts',(-3.87724240306597,-1.,-0.427053541173457));
#52432=CARTESIAN_POINT('Ctrl Pts',(-3.88414070943341,-1.,-0.429856640579741));
#52433=CARTESIAN_POINT('Ctrl Pts',(-3.89104947940611,-1.,-0.432713929544458));
#52434=CARTESIAN_POINT('Ctrl Pts',(-3.89797256655462,-1.,-0.435624629433527));
#52435=CARTESIAN_POINT('Ctrl Pts',(-3.90490512938563,-1.,-0.438587235458249));
#52436=CARTESIAN_POINT('Ctrl Pts',(-3.91183704069153,-1.,-0.441599824524054));
#52437=CARTESIAN_POINT('Ctrl Pts',(-3.91875701610719,-1.,-0.444660430230591));
#52438=CARTESIAN_POINT('Ctrl Pts',(-3.92565674143416,-1.,-0.447767416837292));
#52439=CARTESIAN_POINT('Ctrl Pts',(-3.93253407403123,-1.,-0.450919768356348));
#52440=CARTESIAN_POINT('Ctrl Pts',(-3.93939080846298,-1.,-0.454116879027584));
#52441=CARTESIAN_POINT('Ctrl Pts',(-3.94623117206678,-1.,-0.457358410451683));
#52442=CARTESIAN_POINT('Ctrl Pts',(-3.95306005817364,-1.,-0.460644124429121));
#52443=CARTESIAN_POINT('Ctrl Pts',(-3.95988133243538,-1.,-0.463973722115733));
#52444=CARTESIAN_POINT('Ctrl Pts',(-3.9666962227393,-1.,-0.467346690880643));
#52445=CARTESIAN_POINT('Ctrl Pts',(-3.97350414289392,-1.,-0.470762379613439));
#52446=CARTESIAN_POINT('Ctrl Pts',(-3.98030338044409,-1.,-0.47422006101951));
#52447=CARTESIAN_POINT('Ctrl Pts',(-3.98709184306738,-1.,-0.477718999122027));
#52448=CARTESIAN_POINT('Ctrl Pts',(-3.99386775880679,-1.,-0.481258512209675));
#52449=CARTESIAN_POINT('Ctrl Pts',(-4.00063045119288,-1.,-0.484838042421835));
#52450=CARTESIAN_POINT('Ctrl Pts',(-4.0073800839099,-1.,-0.488457130424633));
#52451=CARTESIAN_POINT('Ctrl Pts',(-4.01411733503546,-1.,-0.492115383418018));
#52452=CARTESIAN_POINT('Ctrl Pts',(-4.02084308851832,-1.,-0.495812444326251));
#52453=CARTESIAN_POINT('Ctrl Pts',(-4.02755813980101,-1.,-0.499547962340821));
#52454=CARTESIAN_POINT('Ctrl Pts',(-4.03426284174272,-1.,-0.503321556915346));
#52455=CARTESIAN_POINT('Ctrl Pts',(-4.04095715148915,-1.,-0.507132823288136));
#52456=CARTESIAN_POINT('Ctrl Pts',(-4.04764078815447,-1.,-0.51098134921897));
#52457=CARTESIAN_POINT('Ctrl Pts',(-4.05431335771199,-1.,-0.514866728193017));
#52458=CARTESIAN_POINT('Ctrl Pts',(-4.06097448038013,-1.,-0.518788572336923));
#52459=CARTESIAN_POINT('Ctrl Pts',(-4.06762394471314,-1.,-0.522746528603107));
#52460=CARTESIAN_POINT('Ctrl Pts',(-4.07426172299847,-1.,-0.526740277227498));
#52461=CARTESIAN_POINT('Ctrl Pts',(-4.08088789536836,-1.,-0.530769518728571));
#52462=CARTESIAN_POINT('Ctrl Pts',(-4.08750259988885,-1.,-0.534833963477273));
#52463=CARTESIAN_POINT('Ctrl Pts',(-4.09410597627,-1.,-0.538933321179756));
#52464=CARTESIAN_POINT('Ctrl Pts',(-4.10069810243979,-1.,-0.543067286877757));
#52465=CARTESIAN_POINT('Ctrl Pts',(-4.10727897027977,-1.,-0.547235539485637));
#52466=CARTESIAN_POINT('Ctrl Pts',(-4.11384852024721,-1.,-0.551437758497032));
#52467=CARTESIAN_POINT('Ctrl Pts',(-4.12040666195664,-1.,-0.555673636129977));
#52468=CARTESIAN_POINT('Ctrl Pts',(-4.12695329951961,-1.,-0.559942890594773));
#52469=CARTESIAN_POINT('Ctrl Pts',(-4.13348835727104,-1.,-0.564245279537148));
#52470=CARTESIAN_POINT('Ctrl Pts',(-4.14001179830547,-1.,-0.568580610189774));
#52471=CARTESIAN_POINT('Ctrl Pts',(-4.14652361068081,-1.,-0.572948736069522));
#52472=CARTESIAN_POINT('Ctrl Pts',(-4.151723761217,-1.,-0.576469391676688));
#52473=CARTESIAN_POINT('Ctrl Pts',(-4.15561864788576,-1.,-0.579124568914235));
#52474=CARTESIAN_POINT('Ctrl Pts',(-4.1582129171283,-1.,-0.580901211463535));
#52475=CARTESIAN_POINT('Ctrl Pts',(-4.15950947128175,-1.,-0.581791163835815));
#52476=CARTESIAN_POINT('',(-4.13571194405636,-1.,-0.73204283740062));
#52477=CARTESIAN_POINT('',(-4.15950947128175,-1.,-0.581791163835815));
#52478=CARTESIAN_POINT('',(-3.66661143271685,-1.,-0.786422660831985));
#52479=CARTESIAN_POINT('Ctrl Pts',(-4.13571194405636,-1.,-0.73204283740062));
#52480=CARTESIAN_POINT('Ctrl Pts',(-4.1342038373684,-1.,-0.732488575135159));
#52481=CARTESIAN_POINT('Ctrl Pts',(-4.13118752795207,-1.,-0.733376589323546));
#52482=CARTESIAN_POINT('Ctrl Pts',(-4.12666277570844,-1.,-0.734698226764092));
#52483=CARTESIAN_POINT('Ctrl Pts',(-4.120629196238,-1.,-0.736439634331345));
#52484=CARTESIAN_POINT('Ctrl Pts',(-4.11308626951927,-1.,-0.738581708225844));
#52485=CARTESIAN_POINT('Ctrl Pts',(-4.10554241757547,-1.,-0.740688998553377));
#52486=CARTESIAN_POINT('Ctrl Pts',(-4.09799769702611,-1.,-0.742761369689841));
#52487=CARTESIAN_POINT('Ctrl Pts',(-4.09045220253573,-1.,-0.7447986497065));
#52488=CARTESIAN_POINT('Ctrl Pts',(-4.08290608095642,-1.,-0.746800631492315));
#52489=CARTESIAN_POINT('Ctrl Pts',(-4.07535951056152,-1.,-0.748767076680557));
#52490=CARTESIAN_POINT('Ctrl Pts',(-4.06781267242378,-1.,-0.750697720484036));
#52491=CARTESIAN_POINT('Ctrl Pts',(-4.06026572221515,-1.,-0.752592276483072));
#52492=CARTESIAN_POINT('Ctrl Pts',(-4.05271876687915,-1.,-0.754450441816078));
#52493=CARTESIAN_POINT('Ctrl Pts',(-4.04517182653997,-1.,-0.756271902369581));
#52494=CARTESIAN_POINT('Ctrl Pts',(-4.03762485803119,-1.,-0.758056338884944));
#52495=CARTESIAN_POINT('Ctrl Pts',(-4.03007781954412,-1.,-0.759803433243752));
#52496=CARTESIAN_POINT('Ctrl Pts',(-4.02253072741268,-1.,-0.761512875859804));
#52497=CARTESIAN_POINT('Ctrl Pts',(-4.01498370680496,-1.,-0.763184371182935));
#52498=CARTESIAN_POINT('Ctrl Pts',(-4.00743706791509,-1.,-0.764817648785197));
#52499=CARTESIAN_POINT('Ctrl Pts',(-3.99989129179622,-1.,-0.766412457136064));
#52500=CARTESIAN_POINT('Ctrl Pts',(-3.9923468788101,-1.,-0.767968531377915));
#52501=CARTESIAN_POINT('Ctrl Pts',(-3.98480422348451,-1.,-0.769485566245544));
#52502=CARTESIAN_POINT('Ctrl Pts',(-3.97726349165488,-1.,-0.770963190030471));
#52503=CARTESIAN_POINT('Ctrl Pts',(-3.96972446532772,-1.,-0.772400931772136));
#52504=CARTESIAN_POINT('Ctrl Pts',(-3.96218649639807,-1.,-0.773798212026565));
#52505=CARTESIAN_POINT('Ctrl Pts',(-3.9546488545231,-1.,-0.775154418039351));
#52506=CARTESIAN_POINT('Ctrl Pts',(-3.94711101619447,-1.,-0.776468966697921));
#52507=CARTESIAN_POINT('Ctrl Pts',(-3.93957296768103,-1.,-0.777741370568558));
#52508=CARTESIAN_POINT('Ctrl Pts',(-3.93203552473174,-1.,-0.778971308134821));
#52509=CARTESIAN_POINT('Ctrl Pts',(-3.92450058323823,-1.,-0.780158678615542));
#52510=CARTESIAN_POINT('Ctrl Pts',(-3.91697036054676,-1.,-0.781303428618366));
#52511=CARTESIAN_POINT('Ctrl Pts',(-3.90944671004542,-1.,-0.782405395622764));
#52512=CARTESIAN_POINT('Ctrl Pts',(-3.9019303904397,-1.,-0.783464141529081));
#52513=CARTESIAN_POINT('Ctrl Pts',(-3.89442039235103,-1.,-0.784478799358336));
#52514=CARTESIAN_POINT('Ctrl Pts',(-3.88691313167398,-1.,-0.78544789034073));
#52515=CARTESIAN_POINT('Ctrl Pts',(-3.8794040281819,-1.,-0.786369675812608));
#52516=CARTESIAN_POINT('Ctrl Pts',(-3.87188916600912,-1.,-0.787242527617999));
#52517=CARTESIAN_POINT('Ctrl Pts',(-3.86436702561345,-1.,-0.788065315093777));
#52518=CARTESIAN_POINT('Ctrl Pts',(-3.85683995872529,-1.,-0.788837734090672));
#52519=CARTESIAN_POINT('Ctrl Pts',(-3.84931637808894,-1.,-0.789560798155582));
#52520=CARTESIAN_POINT('Ctrl Pts',(-3.84180762342454,-1.,-0.790236124191242));
#52521=CARTESIAN_POINT('Ctrl Pts',(-3.83432392054786,-1.,-0.790865012705301));
#52522=CARTESIAN_POINT('Ctrl Pts',(-3.82687033899792,-1.,-0.791447528662369));
#52523=CARTESIAN_POINT('Ctrl Pts',(-3.81944345442249,-1.,-0.791981740718635));
#52524=CARTESIAN_POINT('Ctrl Pts',(-3.81202588694756,-1.,-0.792462483517634));
#52525=CARTESIAN_POINT('Ctrl Pts',(-3.80459229925637,-1.,-0.792882695234778));
#52526=CARTESIAN_POINT('Ctrl Pts',(-3.79711921389897,-1.,-0.793235612973273));
#52527=CARTESIAN_POINT('Ctrl Pts',(-3.78959439439235,-1.,-0.793516871680993));
#52528=CARTESIAN_POINT('Ctrl Pts',(-3.78202460377598,-1.,-0.7937262357813));
#52529=CARTESIAN_POINT('Ctrl Pts',(-3.77444863801212,-1.,-0.793870523787408));
#52530=CARTESIAN_POINT('Ctrl Pts',(-3.76692626931111,-1.,-0.793961083688991));
#52531=CARTESIAN_POINT('Ctrl Pts',(-3.75951468666257,-1.,-0.794008429134907));
#52532=CARTESIAN_POINT('Ctrl Pts',(-3.75224692493864,-1.,-0.794017347371377));
#52533=CARTESIAN_POINT('Ctrl Pts',(-3.74511357728861,-1.,-0.793982700459952));
#52534=CARTESIAN_POINT('Ctrl Pts',(-3.73803280541687,-1.,-0.793882700937017));
#52535=CARTESIAN_POINT('Ctrl Pts',(-3.73086914695805,-1.,-0.793682750269684));
#52536=CARTESIAN_POINT('Ctrl Pts',(-3.72348797293734,-1.,-0.793347023784205));
#52537=CARTESIAN_POINT('Ctrl Pts',(-3.71580242396124,-1.,-0.792848377370287));
#52538=CARTESIAN_POINT('Ctrl Pts',(-3.70781724021806,-1.,-0.792177688845818));
#52539=CARTESIAN_POINT('Ctrl Pts',(-3.69968940808721,-1.,-0.79135657569598));
#52540=CARTESIAN_POINT('Ctrl Pts',(-3.69172044327364,-1.,-0.790436284988787));
#52541=CARTESIAN_POINT('Ctrl Pts',(-3.68428439783905,-1.,-0.789483546064387));
#52542=CARTESIAN_POINT('Ctrl Pts',(-3.67777119516252,-1.,-0.788569566220285));
#52543=CARTESIAN_POINT('Ctrl Pts',(-3.67252923663655,-1.,-0.787758799995742));
#52544=CARTESIAN_POINT('Ctrl Pts',(-3.66907505398677,-1.,-0.787145041181545));
#52545=CARTESIAN_POINT('Ctrl Pts',(-3.66743103898702,-1.,-0.786774337198062));
#52546=CARTESIAN_POINT('Ctrl Pts',(-3.66680946938292,-1.,-0.786565919558984));
#52547=CARTESIAN_POINT('Ctrl Pts',(-3.6666431041522,-1.,-0.786459983895432));
#52548=CARTESIAN_POINT('Ctrl Pts',(-3.66661143271685,-1.,-0.786422660831985));
#52549=CARTESIAN_POINT('',(-3.62400312501245,-1.,-0.963899035117249));
#52550=CARTESIAN_POINT('Origin',(0.,-1.,0.));
#52551=CARTESIAN_POINT('',(-4.01728681790024,-1.,-1.22531898815164));
#52552=CARTESIAN_POINT('Ctrl Pts',(-3.62400312501245,-1.,-0.963899035117249));
#52553=CARTESIAN_POINT('Ctrl Pts',(-3.6240482887845,-1.,-0.963880158555582));
#52554=CARTESIAN_POINT('Ctrl Pts',(-3.62424461507588,-1.,-0.963861297423241));
#52555=CARTESIAN_POINT('Ctrl Pts',(-3.62489305727662,-1.,-0.963957782642843));
#52556=CARTESIAN_POINT('Ctrl Pts',(-3.62652618145335,-1.,-0.964373850166457));
#52557=CARTESIAN_POINT('Ctrl Pts',(-3.62988252139846,-1.,-0.965395153165293));
#52558=CARTESIAN_POINT('Ctrl Pts',(-3.63492122081143,-1.,-0.967052554541385));
#52559=CARTESIAN_POINT('Ctrl Pts',(-3.64113946505766,-1.,-0.969195124675865));
#52560=CARTESIAN_POINT('Ctrl Pts',(-3.64819756447455,-1.,-0.971722122061341));
#52561=CARTESIAN_POINT('Ctrl Pts',(-3.65571576735126,-1.,-0.974519971354848));
#52562=CARTESIAN_POINT('Ctrl Pts',(-3.66333049637475,-1.,-0.977478312751618));
#52563=CARTESIAN_POINT('Ctrl Pts',(-3.67074983340361,-1.,-0.980505922458267));
#52564=CARTESIAN_POINT('Ctrl Pts',(-3.67782408841715,-1.,-0.983550791470419));
#52565=CARTESIAN_POINT('Ctrl Pts',(-3.68455317926068,-1.,-0.986602639863837));
#52566=CARTESIAN_POINT('Ctrl Pts',(-3.69102682138846,-1.,-0.989676715398558));
#52567=CARTESIAN_POINT('Ctrl Pts',(-3.69738123415662,-1.,-0.99280221833201));
#52568=CARTESIAN_POINT('Ctrl Pts',(-3.70375282282138,-1.,-0.996009819772518));
#52569=CARTESIAN_POINT('Ctrl Pts',(-3.71022439713938,-1.,-0.99931726075653));
#52570=CARTESIAN_POINT('Ctrl Pts',(-3.71680667125118,-1.,-1.00272423396822));
#52571=CARTESIAN_POINT('Ctrl Pts',(-3.72346803750595,-1.,-1.0062200073571));
#52572=CARTESIAN_POINT('Ctrl Pts',(-3.73015276704426,-1.,-1.00978798539496));
#52573=CARTESIAN_POINT('Ctrl Pts',(-3.73680245055734,-1.,-1.01341114319903));
#52574=CARTESIAN_POINT('Ctrl Pts',(-3.74337942504959,-1.,-1.01707794311079));
#52575=CARTESIAN_POINT('Ctrl Pts',(-3.74987777155834,-1.,-1.02078510487428));
#52576=CARTESIAN_POINT('Ctrl Pts',(-3.75631037456194,-1.,-1.0245342944466));
#52577=CARTESIAN_POINT('Ctrl Pts',(-3.76270122291232,-1.,-1.02833014458181));
#52578=CARTESIAN_POINT('Ctrl Pts',(-3.76907609832522,-1.,-1.0321778660492));
#52579=CARTESIAN_POINT('Ctrl Pts',(-3.77545283140445,-1.,-1.03608074678013));
#52580=CARTESIAN_POINT('Ctrl Pts',(-3.78183535008192,-1.,-1.04003862055804));
#52581=CARTESIAN_POINT('Ctrl Pts',(-3.78821910787195,-1.,-1.04404924374426));
#52582=CARTESIAN_POINT('Ctrl Pts',(-3.79459440308793,-1.,-1.04810913267641));
#52583=CARTESIAN_POINT('Ctrl Pts',(-3.80095039790678,-1.,-1.05221457990015));
#52584=CARTESIAN_POINT('Ctrl Pts',(-3.80727913637784,-1.,-1.05636266918643));
#52585=CARTESIAN_POINT('Ctrl Pts',(-3.81357866117485,-1.,-1.06055206187298));
#52586=CARTESIAN_POINT('Ctrl Pts',(-3.81985083953012,-1.,-1.06478244038931));
#52587=CARTESIAN_POINT('Ctrl Pts',(-3.82609989967278,-1.,-1.0690541318036));
#52588=CARTESIAN_POINT('Ctrl Pts',(-3.83233071195145,-1.,-1.0733676663346));
#52589=CARTESIAN_POINT('Ctrl Pts',(-3.83854714117486,-1.,-1.07772335353856));
#52590=CARTESIAN_POINT('Ctrl Pts',(-3.84475048030615,-1.,-1.08212087917986));
#52591=CARTESIAN_POINT('Ctrl Pts',(-3.8509402522269,-1.,-1.08655950846377));
#52592=CARTESIAN_POINT('Ctrl Pts',(-3.85711487933911,-1.,-1.09103825516288));
#52593=CARTESIAN_POINT('Ctrl Pts',(-3.86327241021242,-1.,-1.09555606505012));
#52594=CARTESIAN_POINT('Ctrl Pts',(-3.86941120134872,-1.,-1.10011198761202));
#52595=CARTESIAN_POINT('Ctrl Pts',(-3.87553067187566,-1.,-1.10470536603303));
#52596=CARTESIAN_POINT('Ctrl Pts',(-3.88163105531791,-1.,-1.10933577224029));
#52597=CARTESIAN_POINT('Ctrl Pts',(-3.88771308285229,-1.,-1.11400292434447));
#52598=CARTESIAN_POINT('Ctrl Pts',(-3.89377768340362,-1.,-1.11870660794609));
#52599=CARTESIAN_POINT('Ctrl Pts',(-3.89982569749978,-1.,-1.12344660099029));
#52600=CARTESIAN_POINT('Ctrl Pts',(-3.90585753318622,-1.,-1.12822258281518));
#52601=CARTESIAN_POINT('Ctrl Pts',(-3.91187321145495,-1.,-1.13303414693849));
#52602=CARTESIAN_POINT('Ctrl Pts',(-3.91787251936688,-1.,-1.13788084225511));
#52603=CARTESIAN_POINT('Ctrl Pts',(-3.92385513133937,-1.,-1.14276220561575));
#52604=CARTESIAN_POINT('Ctrl Pts',(-3.92982073294334,-1.,-1.14767779451147));
#52605=CARTESIAN_POINT('Ctrl Pts',(-3.9357691705651,-1.,-1.1526272271639));
#52606=CARTESIAN_POINT('Ctrl Pts',(-3.94170046685542,-1.,-1.1576101834106));
#52607=CARTESIAN_POINT('Ctrl Pts',(-3.9476147478092,-1.,-1.16262637999261));
#52608=CARTESIAN_POINT('Ctrl Pts',(-3.95351219510062,-1.,-1.16767555244495));
#52609=CARTESIAN_POINT('Ctrl Pts',(-3.95939299213164,-1.,-1.17275743590327));
#52610=CARTESIAN_POINT('Ctrl Pts',(-3.96525726357682,-1.,-1.17787174135445));
#52611=CARTESIAN_POINT('Ctrl Pts',(-3.9711050516465,-1.,-1.18301815039596));
#52612=CARTESIAN_POINT('Ctrl Pts',(-3.97693634766926,-1.,-1.18819633715285));
#52613=CARTESIAN_POINT('Ctrl Pts',(-3.98275111052015,-1.,-1.19340598349307));
#52614=CARTESIAN_POINT('Ctrl Pts',(-3.98854928957287,-1.,-1.19864679609596));
#52615=CARTESIAN_POINT('Ctrl Pts',(-3.99433084800649,-1.,-1.2039185237544));
#52616=CARTESIAN_POINT('Ctrl Pts',(-4.00009577952534,-1.,-1.20922097030107));
#52617=CARTESIAN_POINT('Ctrl Pts',(-4.00584409524937,-1.,-1.21455398918813));
#52618=CARTESIAN_POINT('Ctrl Pts',(-4.01042947142681,-1.,-1.21884478244983));
#52619=CARTESIAN_POINT('Ctrl Pts',(-4.01386104434674,-1.,-1.22207656456199));
#52620=CARTESIAN_POINT('Ctrl Pts',(-4.0161454457032,-1.,-1.22423716681447));
#52621=CARTESIAN_POINT('Ctrl Pts',(-4.01728681790024,-1.,-1.22531898815164));
#52622=CARTESIAN_POINT('',(-3.97027773754922,-1.,-1.36999806084572));
#52623=CARTESIAN_POINT('',(-4.01728681790024,-1.,-1.22531898815164));
#52624=CARTESIAN_POINT('',(-3.4984457533445,-1.,-1.35032489087101));
#52625=CARTESIAN_POINT('Ctrl Pts',(-3.97027773754922,-1.,-1.36999806084572));
#52626=CARTESIAN_POINT('Ctrl Pts',(-3.9687184694131,-1.,-1.37020239094614));
#52627=CARTESIAN_POINT('Ctrl Pts',(-3.96560037974645,-1.,-1.37060761745635));
#52628=CARTESIAN_POINT('Ctrl Pts',(-3.96092458506535,-1.,-1.3712051561502));
#52629=CARTESIAN_POINT('Ctrl Pts',(-3.95469287280914,-1.,-1.37198126432386));
#52630=CARTESIAN_POINT('Ctrl Pts',(-3.94690771785133,-1.,-1.37291699202807));
#52631=CARTESIAN_POINT('Ctrl Pts',(-3.93912709040818,-1.,-1.37381821967165));
#52632=CARTESIAN_POINT('Ctrl Pts',(-3.93135106761844,-1.,-1.37468482215751));
#52633=CARTESIAN_POINT('Ctrl Pts',(-3.92357976987672,-1.,-1.37551664448242));
#52634=CARTESIAN_POINT('Ctrl Pts',(-3.91581337462644,-1.,-1.37631350505797));
#52635=CARTESIAN_POINT('Ctrl Pts',(-3.90805209523486,-1.,-1.3770751963402));
#52636=CARTESIAN_POINT('Ctrl Pts',(-3.90029615196727,-1.,-1.37780148512792));
#52637=CARTESIAN_POINT('Ctrl Pts',(-3.89254574338496,-1.,-1.3784921128802));
#52638=CARTESIAN_POINT('Ctrl Pts',(-3.88480102249277,-1.,-1.37914679719383));
#52639=CARTESIAN_POINT('Ctrl Pts',(-3.87706205830532,-1.,-1.37976523097073));
#52640=CARTESIAN_POINT('Ctrl Pts',(-3.86932885813068,-1.,-1.38034709213014));
#52641=CARTESIAN_POINT('Ctrl Pts',(-3.86160143043959,-1.,-1.38089205992989));
#52642=CARTESIAN_POINT('Ctrl Pts',(-3.85387983979481,-1.,-1.38139983115049));
#52643=CARTESIAN_POINT('Ctrl Pts',(-3.84616425605764,-1.,-1.38187013346109));
#52644=CARTESIAN_POINT('Ctrl Pts',(-3.83845502790746,-1.,-1.38230274828821));
#52645=CARTESIAN_POINT('Ctrl Pts',(-3.8307526698229,-1.,-1.38269750245138));
#52646=CARTESIAN_POINT('Ctrl Pts',(-3.82305771743829,-1.,-1.38305421262763));
#52647=CARTESIAN_POINT('Ctrl Pts',(-3.81537060817811,-1.,-1.38337263902782));
#52648=CARTESIAN_POINT('Ctrl Pts',(-3.80769156398411,-1.,-1.3836524404622));
#52649=CARTESIAN_POINT('Ctrl Pts',(-3.80002044322111,-1.,-1.38389311766682));
#52650=CARTESIAN_POINT('Ctrl Pts',(-3.79235669640841,-1.,-1.38409399694566));
#52651=CARTESIAN_POINT('Ctrl Pts',(-3.78469969805082,-1.,-1.38425435883756));
#52652=CARTESIAN_POINT('Ctrl Pts',(-3.77704902230418,-1.,-1.38437354551428));
#52653=CARTESIAN_POINT('Ctrl Pts',(-3.76940473185779,-1.,-1.38445107339518));
#52654=CARTESIAN_POINT('Ctrl Pts',(-3.76176768271367,-1.,-1.3844867525335));
#52655=CARTESIAN_POINT('Ctrl Pts',(-3.7541397631875,-1.,-1.38448077997163));
#52656=CARTESIAN_POINT('Ctrl Pts',(-3.74652317167876,-1.,-1.38443344984394));
#52657=CARTESIAN_POINT('Ctrl Pts',(-3.73891976418104,-1.,-1.38434489156458));
#52658=CARTESIAN_POINT('Ctrl Pts',(-3.73133035859282,-1.,-1.38421479111531));
#52659=CARTESIAN_POINT('Ctrl Pts',(-3.72375409358803,-1.,-1.3840421342895));
#52660=CARTESIAN_POINT('Ctrl Pts',(-3.7161876605181,-1.,-1.38382489984586));
#52661=CARTESIAN_POINT('Ctrl Pts',(-3.70862680753347,-1.,-1.38356065402124));
#52662=CARTESIAN_POINT('Ctrl Pts',(-3.701067921679,-1.,-1.38324717612865));
#52663=CARTESIAN_POINT('Ctrl Pts',(-3.69350967899526,-1.,-1.3828831117165));
#52664=CARTESIAN_POINT('Ctrl Pts',(-3.68595444983837,-1.,-1.38246852827182));
#52665=CARTESIAN_POINT('Ctrl Pts',(-3.67841038482414,-1.,-1.3820057429062));
#52666=CARTESIAN_POINT('Ctrl Pts',(-3.67088843112262,-1.,-1.38149812653868));
#52667=CARTESIAN_POINT('Ctrl Pts',(-3.66339848520857,-1.,-1.38094856333552));
#52668=CARTESIAN_POINT('Ctrl Pts',(-3.6559455440439,-1.,-1.38035791051212));
#52669=CARTESIAN_POINT('Ctrl Pts',(-3.64852652756456,-1.,-1.37972372481603));
#52670=CARTESIAN_POINT('Ctrl Pts',(-3.64112507791141,-1.,-1.37903818567359));
#52671=CARTESIAN_POINT('Ctrl Pts',(-3.63371727442486,-1.,-1.37829035457339));
#52672=CARTESIAN_POINT('Ctrl Pts',(-3.62628098665145,-1.,-1.37746987919881));
#52673=CARTESIAN_POINT('Ctrl Pts',(-3.6188048116042,-1.,-1.37657053403107));
#52674=CARTESIAN_POINT('Ctrl Pts',(-3.61129546591064,-1.,-1.37559314436634));
#52675=CARTESIAN_POINT('Ctrl Pts',(-3.60379020123988,-1.,-1.37455051379623));
#52676=CARTESIAN_POINT('Ctrl Pts',(-3.59634627869048,-1.,-1.37346320103157));
#52677=CARTESIAN_POINT('Ctrl Pts',(-3.58901853846365,-1.,-1.37235053660976));
#52678=CARTESIAN_POINT('Ctrl Pts',(-3.58183885982715,-1.,-1.37122241663062));
#52679=CARTESIAN_POINT('Ctrl Pts',(-3.57479875549486,-1.,-1.37007229485659));
#52680=CARTESIAN_POINT('Ctrl Pts',(-3.5678208030466,-1.,-1.36886584973389));
#52681=CARTESIAN_POINT('Ctrl Pts',(-3.56077662028649,-1.,-1.36754771771233));
#52682=CARTESIAN_POINT('Ctrl Pts',(-3.55353883995949,-1.,-1.3660614545677));
#52683=CARTESIAN_POINT('Ctrl Pts',(-3.54602591832973,-1.,-1.36436666257597));
#52684=CARTESIAN_POINT('Ctrl Pts',(-3.53824396424961,-1.,-1.36245507339307));
#52685=CARTESIAN_POINT('Ctrl Pts',(-3.530344649616,-1.,-1.36037259643734));
#52686=CARTESIAN_POINT('Ctrl Pts',(-3.52261776116748,-1.,-1.35821701528836));
#52687=CARTESIAN_POINT('Ctrl Pts',(-3.51542230699556,-1.,-1.35611275237152));
#52688=CARTESIAN_POINT('Ctrl Pts',(-3.50913227059999,-1.,-1.35419113575956));
#52689=CARTESIAN_POINT('Ctrl Pts',(-3.50408168106261,-1.,-1.35257032843486));
#52690=CARTESIAN_POINT('Ctrl Pts',(-3.5007660381649,-1.,-1.35142377279517));
#52691=CARTESIAN_POINT('Ctrl Pts',(-3.49920025459723,-1.,-1.35080045218587));
#52692=CARTESIAN_POINT('Ctrl Pts',(-3.49861894124827,-1.,-1.35049736560527));
#52693=CARTESIAN_POINT('Ctrl Pts',(-3.49847119623846,-1.,-1.35036670892966));
#52694=CARTESIAN_POINT('Ctrl Pts',(-3.4984457533445,-1.,-1.35032489087101));
#52695=CARTESIAN_POINT('',(-3.42859860294378,-1.,-1.51895082866166));
#52696=CARTESIAN_POINT('Origin',(0.,-1.,0.));
#52697=CARTESIAN_POINT('',(-3.77614523045147,-1.,-1.83867539237861));
#52698=CARTESIAN_POINT('Ctrl Pts',(-3.42859860294378,-1.,-1.51895082866166));
#52699=CARTESIAN_POINT('Ctrl Pts',(-3.42864616361967,-1.,-1.51893924967231));
#52700=CARTESIAN_POINT('Ctrl Pts',(-3.42884302333978,-1.,-1.51895133295017));
#52701=CARTESIAN_POINT('Ctrl Pts',(-3.42946838852728,-1.,-1.51914806898539));
#52702=CARTESIAN_POINT('Ctrl Pts',(-3.43101631893491,-1.,-1.5198144909343));
#52703=CARTESIAN_POINT('Ctrl Pts',(-3.43417156977749,-1.,-1.52134826724227));
#52704=CARTESIAN_POINT('Ctrl Pts',(-3.43888895974182,-1.,-1.52377348950429));
#52705=CARTESIAN_POINT('Ctrl Pts',(-3.44469547527,-1.,-1.52686242875717));
#52706=CARTESIAN_POINT('Ctrl Pts',(-3.45127136828667,-1.,-1.530462444618));
#52707=CARTESIAN_POINT('Ctrl Pts',(-3.45825932955273,-1.,-1.53440195378902));
#52708=CARTESIAN_POINT('Ctrl Pts',(-3.46531752207222,-1.,-1.53851507915533));
#52709=CARTESIAN_POINT('Ctrl Pts',(-3.47217189224576,-1.,-1.54266605398152));
#52710=CARTESIAN_POINT('Ctrl Pts',(-3.47868272898599,-1.,-1.54678009290206));
#52711=CARTESIAN_POINT('Ctrl Pts',(-3.48485155928414,-1.,-1.55084702970382));
#52712=CARTESIAN_POINT('Ctrl Pts',(-3.49076460877317,-1.,-1.5548959590107));
#52713=CARTESIAN_POINT('Ctrl Pts',(-3.49655185179623,-1.,-1.55897703097859));
#52714=CARTESIAN_POINT('Ctrl Pts',(-3.50234321621607,-1.,-1.56314187758689));
#52715=CARTESIAN_POINT('Ctrl Pts',(-3.50821771695427,-1.,-1.56742097575041));
#52716=CARTESIAN_POINT('Ctrl Pts',(-3.51418598431733,-1.,-1.57181569799774));
#52717=CARTESIAN_POINT('Ctrl Pts',(-3.52021847865961,-1.,-1.5763104998818));
#52718=CARTESIAN_POINT('Ctrl Pts',(-3.52626275334899,-1.,-1.58088027227856));
#52719=CARTESIAN_POINT('Ctrl Pts',(-3.53226378147068,-1.,-1.58549906268083));
#52720=CARTESIAN_POINT('Ctrl Pts',(-3.53818616861045,-1.,-1.59014958368725));
#52721=CARTESIAN_POINT('Ctrl Pts',(-3.544024581823,-1.,-1.5948276694975));
#52722=CARTESIAN_POINT('Ctrl Pts',(-3.54979148634426,-1.,-1.59953698113444));
#52723=CARTESIAN_POINT('Ctrl Pts',(-3.55550985096117,-1.,-1.60428584699848));
#52724=CARTESIAN_POINT('Ctrl Pts',(-3.56120432482986,-1.,-1.60908344685459));
#52725=CARTESIAN_POINT('Ctrl Pts',(-3.56689200468404,-1.,-1.61393581747522));
#52726=CARTESIAN_POINT('Ctrl Pts',(-3.57257679609826,-1.,-1.61884340915412));
#52727=CARTESIAN_POINT('Ctrl Pts',(-3.57825455954405,-1.,-1.62380329464851));
#52728=CARTESIAN_POINT('Ctrl Pts',(-3.5839162577435,-1.,-1.62881051550748));
#52729=CARTESIAN_POINT('Ctrl Pts',(-3.58955176627876,-1.,-1.63385971451259));
#52730=CARTESIAN_POINT('Ctrl Pts',(-3.59515368334887,-1.,-1.63894676675349));
#52731=CARTESIAN_POINT('Ctrl Pts',(-3.6007202851384,-1.,-1.6440700438558));
#52732=CARTESIAN_POINT('Ctrl Pts',(-3.60625346556992,-1.,-1.64922952425833));
#52733=CARTESIAN_POINT('Ctrl Pts',(-3.61175734965129,-1.,-1.65442619244327));
#52734=CARTESIAN_POINT('Ctrl Pts',(-3.61723666482457,-1.,-1.65966133399186));
#52735=CARTESIAN_POINT('Ctrl Pts',(-3.62269517989104,-1.,-1.66493585923853));
#52736=CARTESIAN_POINT('Ctrl Pts',(-3.62813422105257,-1.,-1.67024966008037));
#52737=CARTESIAN_POINT('Ctrl Pts',(-3.63355343201211,-1.,-1.67560193613145));
#52738=CARTESIAN_POINT('Ctrl Pts',(-3.63895140887443,-1.,-1.68099146651577));
#52739=CARTESIAN_POINT('Ctrl Pts',(-3.64432638915199,-1.,-1.68641690471455));
#52740=CARTESIAN_POINT('Ctrl Pts',(-3.64967689827393,-1.,-1.691877054817));
#52741=CARTESIAN_POINT('Ctrl Pts',(-3.65500246526798,-1.,-1.69737117722558));
#52742=CARTESIAN_POINT('Ctrl Pts',(-3.6603033877491,-1.,-1.70289888566904));
#52743=CARTESIAN_POINT('Ctrl Pts',(-3.6655804319893,-1.,-1.70846001610983));
#52744=CARTESIAN_POINT('Ctrl Pts',(-3.67083454901629,-1.,-1.71405450210392));
#52745=CARTESIAN_POINT('Ctrl Pts',(-3.67606660374665,-1.,-1.71968225581787));
#52746=CARTESIAN_POINT('Ctrl Pts',(-3.68127704936472,-1.,-1.72534302437003));
#52747=CARTESIAN_POINT('Ctrl Pts',(-3.68646597019188,-1.,-1.73103640956647));
#52748=CARTESIAN_POINT('Ctrl Pts',(-3.69163322647906,-1.,-1.73676193254493));
#52749=CARTESIAN_POINT('Ctrl Pts',(-3.6967785691046,-1.,-1.74251908492589));
#52750=CARTESIAN_POINT('Ctrl Pts',(-3.70190175673422,-1.,-1.74830738046092));
#52751=CARTESIAN_POINT('Ctrl Pts',(-3.70700269736876,-1.,-1.75412641804148));
#52752=CARTESIAN_POINT('Ctrl Pts',(-3.71208146346454,-1.,-1.75997588499021));
#52753=CARTESIAN_POINT('Ctrl Pts',(-3.71713822377675,-1.,-1.76585552124549));
#52754=CARTESIAN_POINT('Ctrl Pts',(-3.72217319911429,-1.,-1.77176509401846));
#52755=CARTESIAN_POINT('Ctrl Pts',(-3.72718661205504,-1.,-1.77770437039606));
#52756=CARTESIAN_POINT('Ctrl Pts',(-3.73217863095022,-1.,-1.78367308442682));
#52757=CARTESIAN_POINT('Ctrl Pts',(-3.73714934729962,-1.,-1.78967092823139));
#52758=CARTESIAN_POINT('Ctrl Pts',(-3.74209880351667,-1.,-1.79569757859041));
#52759=CARTESIAN_POINT('Ctrl Pts',(-3.74702700874954,-1.,-1.80175271485519));
#52760=CARTESIAN_POINT('Ctrl Pts',(-3.75193395888069,-1.,-1.80783603939662));
#52761=CARTESIAN_POINT('Ctrl Pts',(-3.75681965683995,-1.,-1.81394729834032));
#52762=CARTESIAN_POINT('Ctrl Pts',(-3.76168412709652,-1.,-1.82008629694924));
#52763=CARTESIAN_POINT('Ctrl Pts',(-3.76652740355856,-1.,-1.82625289221933));
#52764=CARTESIAN_POINT('Ctrl Pts',(-3.77038509819777,-1.,-1.83120816956515));
#52765=CARTESIAN_POINT('Ctrl Pts',(-3.77326886065484,-1.,-1.83493697935064));
#52766=CARTESIAN_POINT('Ctrl Pts',(-3.77518714458232,-1.,-1.83742834010821));
#52767=CARTESIAN_POINT('Ctrl Pts',(-3.77614523045147,-1.,-1.83867539237861));
#52768=CARTESIAN_POINT('',(-3.70708211654725,-1.,-1.97421938526992));
#52769=CARTESIAN_POINT('',(-3.77614523045147,-1.,-1.83867539237861));
#52770=CARTESIAN_POINT('',(-3.24413672884902,-1.,-1.88097764062542));
#52771=CARTESIAN_POINT('Ctrl Pts',(-3.70708211654725,-1.,-1.97421938526992));
#52772=CARTESIAN_POINT('Ctrl Pts',(-3.7055100813194,-1.,-1.974177276451));
#52773=CARTESIAN_POINT('Ctrl Pts',(-3.70236698911837,-1.,-1.97408973726149));
#52774=CARTESIAN_POINT('Ctrl Pts',(-3.69765528558292,-1.,-1.97394846382288));
#52775=CARTESIAN_POINT('Ctrl Pts',(-3.69137888597855,-1.,-1.97374016224397));
#52776=CARTESIAN_POINT('Ctrl Pts',(-3.68354319913416,-1.,-1.9734465030363));
#52777=CARTESIAN_POINT('Ctrl Pts',(-3.67571738106175,-1.,-1.97311947678035));
#52778=CARTESIAN_POINT('Ctrl Pts',(-3.66790152751984,-1.,-1.9727589719863));
#52779=CARTESIAN_POINT('Ctrl Pts',(-3.66009578166865,-1.,-1.97236485439317));
#52780=CARTESIAN_POINT('Ctrl Pts',(-3.65230034717364,-1.,-1.97193697240645));
#52781=CARTESIAN_POINT('Ctrl Pts',(-3.64451546724221,-1.,-1.97147515441539));
#52782=CARTESIAN_POINT('Ctrl Pts',(-3.63674139590853,-1.,-1.97097920454698));
#52783=CARTESIAN_POINT('Ctrl Pts',(-3.62897836973397,-1.,-1.97044889850518));
#52784=CARTESIAN_POINT('Ctrl Pts',(-3.62122658401722,-1.,-1.96988398129888));
#52785=CARTESIAN_POINT('Ctrl Pts',(-3.61348615496393,-1.,-1.96928416040712));
#52786=CARTESIAN_POINT('Ctrl Pts',(-3.60575714017676,-1.,-1.96864911885775));
#52787=CARTESIAN_POINT('Ctrl Pts',(-3.59803959819725,-1.,-1.96797854118257));
#52788=CARTESIAN_POINT('Ctrl Pts',(-3.5903336402273,-1.,-1.96727213799507));
#52789=CARTESIAN_POINT('Ctrl Pts',(-3.58263947663884,-1.,-1.9665296668894));
#52790=CARTESIAN_POINT('Ctrl Pts',(-3.57495748601088,-1.,-1.96575096652857));
#52791=CARTESIAN_POINT('Ctrl Pts',(-3.56728820357933,-1.,-1.96493594634643));
#52792=CARTESIAN_POINT('Ctrl Pts',(-3.55963218706201,-1.,-1.96408450906868));
#52793=CARTESIAN_POINT('Ctrl Pts',(-3.55198990600929,-1.,-1.96319648628667));
#52794=CARTESIAN_POINT('Ctrl Pts',(-3.54436163300425,-1.,-1.96227157573058));
#52795=CARTESIAN_POINT('Ctrl Pts',(-3.53674730625759,-1.,-1.96130926212661));
#52796=CARTESIAN_POINT('Ctrl Pts',(-3.52914648844289,-1.,-1.96030879411534));
#52797=CARTESIAN_POINT('Ctrl Pts',(-3.52155867431438,-1.,-1.95926936324436));
#52798=CARTESIAN_POINT('Ctrl Pts',(-3.51398354617772,-1.,-1.95819025316768));
#52799=CARTESIAN_POINT('Ctrl Pts',(-3.50642124159913,-1.,-1.95707099606513));
#52800=CARTESIAN_POINT('Ctrl Pts',(-3.49887263575602,-1.,-1.9559115382367));
#52801=CARTESIAN_POINT('Ctrl Pts',(-3.49133956289154,-1.,-1.95471236969653));
#52802=CARTESIAN_POINT('Ctrl Pts',(-3.48382414832648,-1.,-1.95347412486316));
#52803=CARTESIAN_POINT('Ctrl Pts',(-3.47632820495926,-1.,-1.95219722189878));
#52804=CARTESIAN_POINT('Ctrl Pts',(-3.4688525897419,-1.,-1.95088147859876));
#52805=CARTESIAN_POINT('Ctrl Pts',(-3.46139661060959,-1.,-1.94952575850196));
#52806=CARTESIAN_POINT('Ctrl Pts',(-3.45395731584051,-1.,-1.94812754766524));
#52807=CARTESIAN_POINT('Ctrl Pts',(-3.44653088665685,-1.,-1.94668377715332));
#52808=CARTESIAN_POINT('Ctrl Pts',(-3.43911410197693,-1.,-1.94519168842883));
#52809=CARTESIAN_POINT('Ctrl Pts',(-3.43170586602436,-1.,-1.94364973660285));
#52810=CARTESIAN_POINT('Ctrl Pts',(-3.42430850941497,-1.,-1.94205835913692));
#52811=CARTESIAN_POINT('Ctrl Pts',(-3.41692971994082,-1.,-1.94042111965237));
#52812=CARTESIAN_POINT('Ctrl Pts',(-3.40957978266622,-1.,-1.93874306008132));
#52813=CARTESIAN_POINT('Ctrl Pts',(-3.40226802104093,-1.,-1.93702857723089));
#52814=CARTESIAN_POINT('Ctrl Pts',(-3.39499923640789,-1.,-1.93527929945982));
#52815=CARTESIAN_POINT('Ctrl Pts',(-3.38777076883267,-1.,-1.93349233176794));
#52816=CARTESIAN_POINT('Ctrl Pts',(-3.38056768525577,-1.,-1.93165739093292));
#52817=CARTESIAN_POINT('Ctrl Pts',(-3.37336807068078,-1.,-1.92975993109897));
#52818=CARTESIAN_POINT('Ctrl Pts',(-3.36615168657597,-1.,-1.92778626543803));
#52819=CARTESIAN_POINT('Ctrl Pts',(-3.35890824422976,-1.,-1.92572846125763));
#52820=CARTESIAN_POINT('Ctrl Pts',(-3.35164424847206,-1.,-1.92358838440518));
#52821=CARTESIAN_POINT('Ctrl Pts',(-3.34439448941915,-1.,-1.92138450828378));
#52822=CARTESIAN_POINT('Ctrl Pts',(-3.33721230709948,-1.,-1.91914609610173));
#52823=CARTESIAN_POINT('Ctrl Pts',(-3.33014884257812,-1.,-1.91690081930297));
#52824=CARTESIAN_POINT('Ctrl Pts',(-3.32323403454507,-1.,-1.91466343916612));
#52825=CARTESIAN_POINT('Ctrl Pts',(-3.31646052426395,-1.,-1.91242616234459));
#52826=CARTESIAN_POINT('Ctrl Pts',(-3.30975721158694,-1.,-1.91014297830502));
#52827=CARTESIAN_POINT('Ctrl Pts',(-3.30300595568341,-1.,-1.90773912171424));
#52828=CARTESIAN_POINT('Ctrl Pts',(-3.29608978722258,-1.,-1.9051389186417));
#52829=CARTESIAN_POINT('Ctrl Pts',(-3.28893448600364,-1.,-1.9022897124757));
#52830=CARTESIAN_POINT('Ctrl Pts',(-3.28154737912287,-1.,-1.89918429230424));
#52831=CARTESIAN_POINT('Ctrl Pts',(-3.27407108932908,-1.,-1.89589172903662));
#52832=CARTESIAN_POINT('Ctrl Pts',(-3.2667765388833,-1.,-1.89255393500769));
#52833=CARTESIAN_POINT('Ctrl Pts',(-3.2599988519361,-1.,-1.88934996203508));
#52834=CARTESIAN_POINT('Ctrl Pts',(-3.25408686339298,-1.,-1.88646802523372));
#52835=CARTESIAN_POINT('Ctrl Pts',(-3.24935200512055,-1.,-1.88407708646435));
#52836=CARTESIAN_POINT('Ctrl Pts',(-3.24625654410705,-1.,-1.88242596600422));
#52837=CARTESIAN_POINT('Ctrl Pts',(-3.24480754675942,-1.,-1.88156537699118));
#52838=CARTESIAN_POINT('Ctrl Pts',(-3.24428080352952,-1.,-1.88117508446657));
#52839=CARTESIAN_POINT('Ctrl Pts',(-3.24415531671311,-1.,-1.88102292397987));
#52840=CARTESIAN_POINT('Ctrl Pts',(-3.24413672884902,-1.,-1.88097764062542));
#52841=CARTESIAN_POINT('',(-3.14877060440425,-1.,-2.03660101169564));
#52842=CARTESIAN_POINT('Origin',(0.,-1.,0.));
#52843=CARTESIAN_POINT('',(-3.44202241512147,-1.,-2.40675750623143));
#52844=CARTESIAN_POINT('Ctrl Pts',(-3.14877060440425,-1.,-2.03660101169564));
#52845=CARTESIAN_POINT('Ctrl Pts',(-3.1488193908823,-1.,-2.03659701539175));
#52846=CARTESIAN_POINT('Ctrl Pts',(-3.14901193669147,-1.,-2.03663974554941));
#52847=CARTESIAN_POINT('Ctrl Pts',(-3.14959882629936,-1.,-2.03693188810614));
#52848=CARTESIAN_POINT('Ctrl Pts',(-3.15102344775396,-1.,-2.03783225496023));
#52849=CARTESIAN_POINT('Ctrl Pts',(-3.1538999167466,-1.,-2.03984073791432));
#52850=CARTESIAN_POINT('Ctrl Pts',(-3.15817983946525,-1.,-2.04297406404132));
#52851=CARTESIAN_POINT('Ctrl Pts',(-3.16343165059235,-1.,-2.0469333124766));
#52852=CARTESIAN_POINT('Ctrl Pts',(-3.16936341689859,-1.,-2.05151770247452));
#52853=CARTESIAN_POINT('Ctrl Pts',(-3.17564906975592,-1.,-2.05650186773279));
#52854=CARTESIAN_POINT('Ctrl Pts',(-3.18197692964677,-1.,-2.06166849827143));
#52855=CARTESIAN_POINT('Ctrl Pts',(-3.18809755562297,-1.,-2.06684062744065));
#52856=CARTESIAN_POINT('Ctrl Pts',(-3.19388465568113,-1.,-2.07192253497765));
#52857=CARTESIAN_POINT('Ctrl Pts',(-3.19934132835879,-1.,-2.0769044187063));
#52858=CARTESIAN_POINT('Ctrl Pts',(-3.20454818630635,-1.,-2.08182850370816));
#52859=CARTESIAN_POINT('Ctrl Pts',(-3.20962575845433,-1.,-2.08676465517435));
#52860=CARTESIAN_POINT('Ctrl Pts',(-3.2146942960168,-1.,-2.0917841946046));
#52861=CARTESIAN_POINT('Ctrl Pts',(-3.21982707347067,-1.,-2.09692958434933));
#52862=CARTESIAN_POINT('Ctrl Pts',(-3.22503437553496,-1.,-2.10220384298533));
#52863=CARTESIAN_POINT('Ctrl Pts',(-3.23028945793334,-1.,-2.1075869964248));
#52864=CARTESIAN_POINT('Ctrl Pts',(-3.23554444767115,-1.,-2.11304604021784));
#52865=CARTESIAN_POINT('Ctrl Pts',(-3.24074905517282,-1.,-2.11854673326972));
#52866=CARTESIAN_POINT('Ctrl Pts',(-3.24587102613347,-1.,-2.12406646410943));
#52867=CARTESIAN_POINT('Ctrl Pts',(-3.25090574493994,-1.,-2.1296002839681));
#52868=CARTESIAN_POINT('Ctrl Pts',(-3.25586495065027,-1.,-2.13515375878786));
#52869=CARTESIAN_POINT('Ctrl Pts',(-3.26077002641868,-1.,-2.14073870754257));
#52870=CARTESIAN_POINT('Ctrl Pts',(-3.26564388189764,-1.,-2.14636805295663));
#52871=CARTESIAN_POINT('Ctrl Pts',(-3.27050245897244,-1.,-2.15205043199818));
#52872=CARTESIAN_POINT('Ctrl Pts',(-3.27534954469206,-1.,-2.15778690038359));
#52873=CARTESIAN_POINT('Ctrl Pts',(-3.28018150841414,-1.,-2.16357391934434));
#52874=CARTESIAN_POINT('Ctrl Pts',(-3.2849901997973,-1.,-2.16940517773459));
#52875=CARTESIAN_POINT('Ctrl Pts',(-3.28976645712566,-1.,-2.17527380048422));
#52876=CARTESIAN_POINT('Ctrl Pts',(-3.29450361500484,-1.,-2.18117455557062));
#52877=CARTESIAN_POINT('Ctrl Pts',(-3.29920022557635,-1.,-2.18710556500325));
#52878=CARTESIAN_POINT('Ctrl Pts',(-3.30385816281831,-1.,-2.19306710376112));
#52879=CARTESIAN_POINT('Ctrl Pts',(-3.30848134694596,-1.,-2.19906078949924));
#52880=CARTESIAN_POINT('Ctrl Pts',(-3.3130742460895,-1.,-2.20508863150608));
#52881=CARTESIAN_POINT('Ctrl Pts',(-3.31764044024231,-1.,-2.21115211847872));
#52882=CARTESIAN_POINT('Ctrl Pts',(-3.32218125618955,-1.,-2.21725135110889));
#52883=CARTESIAN_POINT('Ctrl Pts',(-3.32669646722871,-1.,-2.22338548312758));
#52884=CARTESIAN_POINT('Ctrl Pts',(-3.33118487773593,-1.,-2.22955308907221));
#52885=CARTESIAN_POINT('Ctrl Pts',(-3.33564495756478,-1.,-2.2357525632881));
#52886=CARTESIAN_POINT('Ctrl Pts',(-3.34007543738044,-1.,-2.24198249391437));
#52887=CARTESIAN_POINT('Ctrl Pts',(-3.34447596770768,-1.,-2.24824207678288));
#52888=CARTESIAN_POINT('Ctrl Pts',(-3.34884690292342,-1.,-2.25453097693524));
#52889=CARTESIAN_POINT('Ctrl Pts',(-3.35318902552676,-1.,-2.26084915222484));
#52890=CARTESIAN_POINT('Ctrl Pts',(-3.35750328523077,-1.,-2.26719668579921));
#52891=CARTESIAN_POINT('Ctrl Pts',(-3.36179055004369,-1.,-2.27357362620902));
#52892=CARTESIAN_POINT('Ctrl Pts',(-3.36605130712978,-1.,-2.27997979457968));
#52893=CARTESIAN_POINT('Ctrl Pts',(-3.37028570206357,-1.,-2.28641481081045));
#52894=CARTESIAN_POINT('Ctrl Pts',(-3.37449367172707,-1.,-2.2928781800731));
#52895=CARTESIAN_POINT('Ctrl Pts',(-3.37867504959382,-1.,-2.29936936127588));
#52896=CARTESIAN_POINT('Ctrl Pts',(-3.38282967336676,-1.,-2.30588783640389));
#52897=CARTESIAN_POINT('Ctrl Pts',(-3.38695751492659,-1.,-2.31243319489505));
#52898=CARTESIAN_POINT('Ctrl Pts',(-3.39105869475112,-1.,-2.31900513925627));
#52899=CARTESIAN_POINT('Ctrl Pts',(-3.39513342020045,-1.,-2.32560343902683));
#52900=CARTESIAN_POINT('Ctrl Pts',(-3.39918194578115,-1.,-2.33222789882601));
#52901=CARTESIAN_POINT('Ctrl Pts',(-3.40320452776646,-1.,-2.33887832342715));
#52902=CARTESIAN_POINT('Ctrl Pts',(-3.40720137403888,-1.,-2.34555447648901));
#52903=CARTESIAN_POINT('Ctrl Pts',(-3.41117262313464,-1.,-2.35225606823649));
#52904=CARTESIAN_POINT('Ctrl Pts',(-3.4151183675076,-1.,-2.35898278606449));
#52905=CARTESIAN_POINT('Ctrl Pts',(-3.41903866635384,-1.,-2.36573431470314));
#52906=CARTESIAN_POINT('Ctrl Pts',(-3.42293356216595,-1.,-2.37251035954351));
#52907=CARTESIAN_POINT('Ctrl Pts',(-3.42680309755241,-1.,-2.37931067029517));
#52908=CARTESIAN_POINT('Ctrl Pts',(-3.43064732714472,-1.,-2.38613505844641));
#52909=CARTESIAN_POINT('Ctrl Pts',(-3.43446630680436,-1.,-2.39298338805823));
#52910=CARTESIAN_POINT('Ctrl Pts',(-3.43750133066036,-1.,-2.39848113411429));
#52911=CARTESIAN_POINT('Ctrl Pts',(-3.43976627485223,-1.,-2.40261515590099));
#52912=CARTESIAN_POINT('Ctrl Pts',(-3.44127120683402,-1.,-2.40537592959345));
#52913=CARTESIAN_POINT('Ctrl Pts',(-3.44202241512147,-1.,-2.40675750623143));
#52914=CARTESIAN_POINT('',(-3.35260583073571,-1.,-2.52982887637028));
#52915=CARTESIAN_POINT('',(-3.44202241512147,-1.,-2.40675750623143));
#52916=CARTESIAN_POINT('',(-2.90994629141676,-1.,-2.36531447826073));
#52917=CARTESIAN_POINT('Ctrl Pts',(-3.35260583073571,-1.,-2.52982887637028));
#52918=CARTESIAN_POINT('Ctrl Pts',(-3.35105973714071,-1.,-2.5295413654909));
#52919=CARTESIAN_POINT('Ctrl Pts',(-3.34796903576663,-1.,-2.52896321610703));
#52920=CARTESIAN_POINT('Ctrl Pts',(-3.34333744115511,-1.,-2.52808660915689));
#52921=CARTESIAN_POINT('Ctrl Pts',(-3.33717089999103,-1.,-2.52689902690158));
#52922=CARTESIAN_POINT('Ctrl Pts',(-3.32947762187533,-1.,-2.52538321164634));
#52923=CARTESIAN_POINT('Ctrl Pts',(-3.32179931078699,-1.,-2.5238359839626));
#52924=CARTESIAN_POINT('Ctrl Pts',(-3.31413607874645,-1.,-2.52225724871313));
#52925=CARTESIAN_POINT('Ctrl Pts',(-3.30648808815442,-1.,-2.52064689568511));
#52926=CARTESIAN_POINT('Ctrl Pts',(-3.29885556388352,-1.,-2.51900480701069));
#52927=CARTESIAN_POINT('Ctrl Pts',(-3.2912387729927,-1.,-2.51733085123797));
#52928=CARTESIAN_POINT('Ctrl Pts',(-3.28363799702982,-1.,-2.51562487464514));
#52929=CARTESIAN_POINT('Ctrl Pts',(-3.27605350473142,-1.,-2.513886692704));
#52930=CARTESIAN_POINT('Ctrl Pts',(-3.26848552888115,-1.,-2.51211608411423));
#52931=CARTESIAN_POINT('Ctrl Pts',(-3.26093423001434,-1.,-2.51031277813486));
#52932=CARTESIAN_POINT('Ctrl Pts',(-3.25339971460982,-1.,-2.50847647070723));
#52933=CARTESIAN_POINT('Ctrl Pts',(-3.24588208983849,-1.,-2.506606859405));
#52934=CARTESIAN_POINT('Ctrl Pts',(-3.23838151080319,-1.,-2.5047036758003));
#52935=CARTESIAN_POINT('Ctrl Pts',(-3.23089822320646,-1.,-2.50276671338111));
#52936=CARTESIAN_POINT('Ctrl Pts',(-3.22343262620503,-1.,-2.50079587201957));
#52937=CARTESIAN_POINT('Ctrl Pts',(-3.21598526261286,-1.,-2.4987911459939));
#52938=CARTESIAN_POINT('Ctrl Pts',(-3.20855669849836,-1.,-2.4967525264737));
#52939=CARTESIAN_POINT('Ctrl Pts',(-3.20114742397588,-1.,-2.49467992057755));
#52940=CARTESIAN_POINT('Ctrl Pts',(-3.19375775555798,-1.,-2.49257307239848));
#52941=CARTESIAN_POINT('Ctrl Pts',(-3.18638771282266,-1.,-2.49043146334059));
#52942=CARTESIAN_POINT('Ctrl Pts',(-3.17903698136622,-1.,-2.48825428288201));
#52943=CARTESIAN_POINT('Ctrl Pts',(-3.17170518863313,-1.,-2.48604065348587));
#52944=CARTESIAN_POINT('Ctrl Pts',(-3.16439213290161,-1.,-2.48378981792725));
#52945=CARTESIAN_POINT('Ctrl Pts',(-3.15709802322739,-1.,-2.48150133566571));
#52946=CARTESIAN_POINT('Ctrl Pts',(-3.14982373241352,-1.,-2.47917529057029));
#52947=CARTESIAN_POINT('Ctrl Pts',(-3.1425709954655,-1.,-2.47681245356109));
#52948=CARTESIAN_POINT('Ctrl Pts',(-3.13534181229295,-1.,-2.47441378371932));
#52949=CARTESIAN_POINT('Ctrl Pts',(-3.12813790805952,-1.,-2.47197997765871));
#52950=CARTESIAN_POINT('Ctrl Pts',(-3.12096015766983,-1.,-2.46951098947469));
#52951=CARTESIAN_POINT('Ctrl Pts',(-3.11380805536122,-1.,-2.46700558843506));
#52952=CARTESIAN_POINT('Ctrl Pts',(-3.1066790790198,-1.,-2.46446082979646));
#52953=CARTESIAN_POINT('Ctrl Pts',(-3.09956993697052,-1.,-2.46187308501884));
#52954=CARTESIAN_POINT('Ctrl Pts',(-3.09247787931887,-1.,-2.4592391256388));
#52955=CARTESIAN_POINT('Ctrl Pts',(-3.08540206545315,-1.,-2.45655725437039));
#52956=CARTESIAN_POINT('Ctrl Pts',(-3.07834472886139,-1.,-2.4538282678779));
#52957=CARTESIAN_POINT('Ctrl Pts',(-3.07131290521297,-1.,-2.45105688854422));
#52958=CARTESIAN_POINT('Ctrl Pts',(-3.06431596421405,-1.,-2.44824970516544));
#52959=CARTESIAN_POINT('Ctrl Pts',(-3.05736242671506,-1.,-2.44541251892556));
#52960=CARTESIAN_POINT('Ctrl Pts',(-3.05045678021504,-1.,-2.44254768923105));
#52961=CARTESIAN_POINT('Ctrl Pts',(-3.04359685040555,-1.,-2.43965194061857));
#52962=CARTESIAN_POINT('Ctrl Pts',(-3.03676949672821,-1.,-2.43671278042414));
#52963=CARTESIAN_POINT('Ctrl Pts',(-3.02995534946978,-1.,-2.43371241361488));
#52964=CARTESIAN_POINT('Ctrl Pts',(-3.02313656036004,-1.,-2.43063415586637));
#52965=CARTESIAN_POINT('Ctrl Pts',(-3.01630420830504,-1.,-2.42746856264168));
#52966=CARTESIAN_POINT('Ctrl Pts',(-3.00946442616658,-1.,-2.42421849439613));
#52967=CARTESIAN_POINT('Ctrl Pts',(-3.00264868585996,-1.,-2.42090763946779));
#52968=CARTESIAN_POINT('Ctrl Pts',(-2.99590509293503,-1.,-2.41757324500514));
#52969=CARTESIAN_POINT('Ctrl Pts',(-2.98927983005796,-1.,-2.41425064199586));
#52970=CARTESIAN_POINT('Ctrl Pts',(-2.98280015815107,-1.,-2.41095909342571));
#52971=CARTESIAN_POINT('Ctrl Pts',(-2.97646002822422,-1.,-2.40768975073713));
#52972=CARTESIAN_POINT('Ctrl Pts',(-2.9701964131236,-1.,-2.40438604734919));
#52973=CARTESIAN_POINT('Ctrl Pts',(-2.96390432240312,-1.,-2.4009556571164));
#52974=CARTESIAN_POINT('Ctrl Pts',(-2.95748006482942,-1.,-2.39730553974517));
#52975=CARTESIAN_POINT('Ctrl Pts',(-2.95085857128439,-1.,-2.39337207631667));
#52976=CARTESIAN_POINT('Ctrl Pts',(-2.94404820669076,-1.,-2.38914929090759));
#52977=CARTESIAN_POINT('Ctrl Pts',(-2.93717903280391,-1.,-2.38472771516311));
#52978=CARTESIAN_POINT('Ctrl Pts',(-2.93049643640206,-1.,-2.38028989582073));
#52979=CARTESIAN_POINT('Ctrl Pts',(-2.92430340582608,-1.,-2.3760651052403));
#52980=CARTESIAN_POINT('Ctrl Pts',(-2.91891503791411,-1.,-2.37229381109821));
#52981=CARTESIAN_POINT('Ctrl Pts',(-2.9146124988314,-1.,-2.36919161373173));
#52982=CARTESIAN_POINT('Ctrl Pts',(-2.91181344022549,-1.,-2.36707658451664));
#52983=CARTESIAN_POINT('Ctrl Pts',(-2.91051690822156,-1.,-2.36599991765749));
#52984=CARTESIAN_POINT('Ctrl Pts',(-2.91005770527719,-1.,-2.36553202948613));
#52985=CARTESIAN_POINT('Ctrl Pts',(-2.90995756655606,-1.,-2.36536211188453));
#52986=CARTESIAN_POINT('Ctrl Pts',(-2.90994629141676,-1.,-2.36531447826074));
#52987=CARTESIAN_POINT('',(-2.79140942341378,-1.,-2.50410331873042));
#52988=CARTESIAN_POINT('Origin',(0.,-1.,0.));
#52989=CARTESIAN_POINT('',(-3.02314558451372,-1.,-2.91557726271063));
#52990=CARTESIAN_POINT('Ctrl Pts',(-2.79140942341378,-1.,-2.50410331873042));
#52991=CARTESIAN_POINT('Ctrl Pts',(-2.79145823440899,-1.,-2.50410700351426));
#52992=CARTESIAN_POINT('Ctrl Pts',(-2.79164172519039,-1.,-2.50417932839343));
#52993=CARTESIAN_POINT('Ctrl Pts',(-2.79217568804874,-1.,-2.50455968395235));
#52994=CARTESIAN_POINT('Ctrl Pts',(-2.79344192164204,-1.,-2.50567182569153));
#52995=CARTESIAN_POINT('Ctrl Pts',(-2.7959687805717,-1.,-2.50810555977564));
#52996=CARTESIAN_POINT('Ctrl Pts',(-2.79970585014308,-1.,-2.51186983687947));
#52997=CARTESIAN_POINT('Ctrl Pts',(-2.80427363984939,-1.,-2.51660190466067));
#52998=CARTESIAN_POINT('Ctrl Pts',(-2.80941521967234,-1.,-2.52205778589922));
#52999=CARTESIAN_POINT('Ctrl Pts',(-2.8148437904867,-1.,-2.52796388055457));
#53000=CARTESIAN_POINT('Ctrl Pts',(-2.82028550483744,-1.,-2.53405679667463));
#53001=CARTESIAN_POINT('Ctrl Pts',(-2.82552167649157,-1.,-2.54012272520141));
#53002=CARTESIAN_POINT('Ctrl Pts',(-2.83044254225794,-1.,-2.54604736792542));
#53003=CARTESIAN_POINT('Ctrl Pts',(-2.83505269592412,-1.,-2.55182152806964));
#53004=CARTESIAN_POINT('Ctrl Pts',(-2.83942515220699,-1.,-2.55749952145165));
#53005=CARTESIAN_POINT('Ctrl Pts',(-2.84366802680211,-1.,-2.56316920798489));
#53006=CARTESIAN_POINT('Ctrl Pts',(-2.84788893329091,-1.,-2.56891984251743));
#53007=CARTESIAN_POINT('Ctrl Pts',(-2.85215360144483,-1.,-2.57480482727128));
#53008=CARTESIAN_POINT('Ctrl Pts',(-2.85647171715147,-1.,-2.58082875254407));
#53009=CARTESIAN_POINT('Ctrl Pts',(-2.86081999003668,-1.,-2.5869677064356));
#53010=CARTESIAN_POINT('Ctrl Pts',(-2.86515629953528,-1.,-2.59318160184921));
#53011=CARTESIAN_POINT('Ctrl Pts',(-2.86943633170712,-1.,-2.59942875223202));
#53012=CARTESIAN_POINT('Ctrl Pts',(-2.87363176656475,-1.,-2.6056817788128));
#53013=CARTESIAN_POINT('Ctrl Pts',(-2.87773881947885,-1.,-2.61193507170928));
#53014=CARTESIAN_POINT('Ctrl Pts',(-2.88176821427502,-1.,-2.61819596473087));
#53015=CARTESIAN_POINT('Ctrl Pts',(-2.88573922195049,-1.,-2.62447947640253));
#53016=CARTESIAN_POINT('Ctrl Pts',(-2.88967244854243,-1.,-2.63080195420771));
#53017=CARTESIAN_POINT('Ctrl Pts',(-2.89358228854557,-1.,-2.63717442263944));
#53018=CARTESIAN_POINT('Ctrl Pts',(-2.89747231723361,-1.,-2.64359851684146));
#53019=CARTESIAN_POINT('Ctrl Pts',(-2.90133950224879,-1.,-2.65007017365576));
#53020=CARTESIAN_POINT('Ctrl Pts',(-2.90517678087467,-1.,-2.65658188464287));
#53021=CARTESIAN_POINT('Ctrl Pts',(-2.90897617968921,-1.,-2.66312542616808));
#53022=CARTESIAN_POINT('Ctrl Pts',(-2.91273193382876,-1.,-2.66969458792627));
#53023=CARTESIAN_POINT('Ctrl Pts',(-2.91644290704281,-1.,-2.67628728855309));
#53024=CARTESIAN_POINT('Ctrl Pts',(-2.92011090722152,-1.,-2.68290409279689));
#53025=CARTESIAN_POINT('Ctrl Pts',(-2.92373955325876,-1.,-2.68954721165342));
#53026=CARTESIAN_POINT('Ctrl Pts',(-2.92733294395268,-1.,-2.69621932864302));
#53027=CARTESIAN_POINT('Ctrl Pts',(-2.93089438233746,-1.,-2.70292247416881));
#53028=CARTESIAN_POINT('Ctrl Pts',(-2.93442516311168,-1.,-2.70965695523776));
#53029=CARTESIAN_POINT('Ctrl Pts',(-2.93792519474955,-1.,-2.71642190053575));
#53030=CARTESIAN_POINT('Ctrl Pts',(-2.94139351933882,-1.,-2.72321571511322));
#53031=CARTESIAN_POINT('Ctrl Pts',(-2.94482887675139,-1.,-2.73003657371613));
#53032=CARTESIAN_POINT('Ctrl Pts',(-2.94823023414381,-1.,-2.73688288329825));
#53033=CARTESIAN_POINT('Ctrl Pts',(-2.95159737214305,-1.,-2.7437537949221));
#53034=CARTESIAN_POINT('Ctrl Pts',(-2.95493069316211,-1.,-2.75064903318996));
#53035=CARTESIAN_POINT('Ctrl Pts',(-2.9582309766594,-1.,-2.75756867888393));
#53036=CARTESIAN_POINT('Ctrl Pts',(-2.96149914764832,-1.,-2.76451296269571));
#53037=CARTESIAN_POINT('Ctrl Pts',(-2.96473605585548,-1.,-2.77148206836464));
#53038=CARTESIAN_POINT('Ctrl Pts',(-2.9679422104295,-1.,-2.77847589542767));
#53039=CARTESIAN_POINT('Ctrl Pts',(-2.97111781461349,-1.,-2.78549409123657));
#53040=CARTESIAN_POINT('Ctrl Pts',(-2.97426288347475,-1.,-2.79253615718147));
#53041=CARTESIAN_POINT('Ctrl Pts',(-2.97737733718242,-1.,-2.79960153278186));
#53042=CARTESIAN_POINT('Ctrl Pts',(-2.98046109647299,-1.,-2.80668968101162));
#53043=CARTESIAN_POINT('Ctrl Pts',(-2.9835141977994,-1.,-2.81380019196454));
#53044=CARTESIAN_POINT('Ctrl Pts',(-2.98653680669434,-1.,-2.82093279065704));
#53045=CARTESIAN_POINT('Ctrl Pts',(-2.98952916401699,-1.,-2.82808728190402));
#53046=CARTESIAN_POINT('Ctrl Pts',(-2.99249155170479,-1.,-2.83526351254383));
#53047=CARTESIAN_POINT('Ctrl Pts',(-2.995424253416,-1.,-2.84246132984334));
#53048=CARTESIAN_POINT('Ctrl Pts',(-2.99832751144566,-1.,-2.84968053289104));
#53049=CARTESIAN_POINT('Ctrl Pts',(-3.0012015079552,-1.,-2.85692085715129));
#53050=CARTESIAN_POINT('Ctrl Pts',(-3.00404638316245,-1.,-2.86418200833065));
#53051=CARTESIAN_POINT('Ctrl Pts',(-3.00686224485374,-1.,-2.87146368430104));
#53052=CARTESIAN_POINT('Ctrl Pts',(-3.0096491810855,-1.,-2.87876560072799));
#53053=CARTESIAN_POINT('Ctrl Pts',(-3.01240727309568,-1.,-2.88608751706796));
#53054=CARTESIAN_POINT('Ctrl Pts',(-3.01513660433291,-1.,-2.8934292556764));
#53055=CARTESIAN_POINT('Ctrl Pts',(-3.01783725123646,-1.,-2.90079069102661));
#53056=CARTESIAN_POINT('Ctrl Pts',(-3.01997487194926,-1.,-2.90669553303902));
#53057=CARTESIAN_POINT('Ctrl Pts',(-3.02156522743299,-1.,-2.91113297349052));
#53058=CARTESIAN_POINT('Ctrl Pts',(-3.02261975104912,-1.,-2.91409518070707));
#53059=CARTESIAN_POINT('Ctrl Pts',(-3.02314558451372,-1.,-2.91557726271063));
#53060=CARTESIAN_POINT('',(-2.91557726271063,-1.,-3.02314558451372));
#53061=CARTESIAN_POINT('',(-3.02314558451372,-1.,-2.91557726271063));
#53062=CARTESIAN_POINT('',(-2.50410331873176,-1.,-2.79140942341258));
#53063=CARTESIAN_POINT('Ctrl Pts',(-2.91557726271063,-1.,-3.02314558451372));
#53064=CARTESIAN_POINT('Ctrl Pts',(-2.91409518070399,-1.,-3.02261975104593));
#53065=CARTESIAN_POINT('Ctrl Pts',(-2.91113297348212,-1.,-3.02156522742431));
#53066=CARTESIAN_POINT('Ctrl Pts',(-2.90669553302526,-1.,-3.01997487193503));
#53067=CARTESIAN_POINT('Ctrl Pts',(-2.9007906910105,-1.,-3.01783725121981));
#53068=CARTESIAN_POINT('Ctrl Pts',(-2.89342925566321,-1.,-3.01513660431928));
#53069=CARTESIAN_POINT('Ctrl Pts',(-2.8860875170608,-1.,-3.01240727308829));
#53070=CARTESIAN_POINT('Ctrl Pts',(-2.87876560072727,-1.,-3.00964918108476));
#53071=CARTESIAN_POINT('Ctrl Pts',(-2.87146368430502,-1.,-3.00686224485784));
#53072=CARTESIAN_POINT('Ctrl Pts',(-2.86418200833667,-1.,-3.00404638316867));
#53073=CARTESIAN_POINT('Ctrl Pts',(-2.85692085715686,-1.,-3.00120150796095));
#53074=CARTESIAN_POINT('Ctrl Pts',(-2.84968053289451,-1.,-2.99832751144925));
#53075=CARTESIAN_POINT('Ctrl Pts',(-2.84246132984415,-1.,-2.99542425341685));
#53076=CARTESIAN_POINT('Ctrl Pts',(-2.83526351254248,-1.,-2.99249155170339));
#53077=CARTESIAN_POINT('Ctrl Pts',(-2.82808728190157,-1.,-2.98952916401446));
#53078=CARTESIAN_POINT('Ctrl Pts',(-2.82093279065457,-1.,-2.9865368066918));
#53079=CARTESIAN_POINT('Ctrl Pts',(-2.81380019196286,-1.,-2.98351419779767));
#53080=CARTESIAN_POINT('Ctrl Pts',(-2.80668968101106,-1.,-2.98046109647241));
#53081=CARTESIAN_POINT('Ctrl Pts',(-2.7996015327823,-1.,-2.97737733718287));
#53082=CARTESIAN_POINT('Ctrl Pts',(-2.79253615718248,-1.,-2.9742628834758));
#53083=CARTESIAN_POINT('Ctrl Pts',(-2.78549409123769,-1.,-2.97111781461465));
#53084=CARTESIAN_POINT('Ctrl Pts',(-2.7784758954285,-1.,-2.96794221043036));
#53085=CARTESIAN_POINT('Ctrl Pts',(-2.77148206836498,-1.,-2.96473605585583));
#53086=CARTESIAN_POINT('Ctrl Pts',(-2.76451296269557,-1.,-2.96149914764818));
#53087=CARTESIAN_POINT('Ctrl Pts',(-2.7575686788835,-1.,-2.95823097665896));
#53088=CARTESIAN_POINT('Ctrl Pts',(-2.75064903318947,-1.,-2.95493069316161));
#53089=CARTESIAN_POINT('Ctrl Pts',(-2.74375379492172,-1.,-2.95159737214266));
#53090=CARTESIAN_POINT('Ctrl Pts',(-2.73688288329808,-1.,-2.94823023414364));
#53091=CARTESIAN_POINT('Ctrl Pts',(-2.73003657371617,-1.,-2.94482887675143));
#53092=CARTESIAN_POINT('Ctrl Pts',(-2.72321571511337,-1.,-2.94139351933897));
#53093=CARTESIAN_POINT('Ctrl Pts',(-2.71642190053592,-1.,-2.93792519474972));
#53094=CARTESIAN_POINT('Ctrl Pts',(-2.70965695523787,-1.,-2.93442516311179));
#53095=CARTESIAN_POINT('Ctrl Pts',(-2.70292247416885,-1.,-2.93089438233749));
#53096=CARTESIAN_POINT('Ctrl Pts',(-2.69621932864301,-1.,-2.92733294395267));
#53097=CARTESIAN_POINT('Ctrl Pts',(-2.68954721165339,-1.,-2.92373955325875));
#53098=CARTESIAN_POINT('Ctrl Pts',(-2.68290409279688,-1.,-2.92011090722152));
#53099=CARTESIAN_POINT('Ctrl Pts',(-2.67628728855312,-1.,-2.91644290704285));
#53100=CARTESIAN_POINT('Ctrl Pts',(-2.66969458792631,-1.,-2.91273193382882));
#53101=CARTESIAN_POINT('Ctrl Pts',(-2.6631254261681,-1.,-2.90897617968923));
#53102=CARTESIAN_POINT('Ctrl Pts',(-2.65658188464282,-1.,-2.90517678087461));
#53103=CARTESIAN_POINT('Ctrl Pts',(-2.65007017365564,-1.,-2.90133950224867));
#53104=CARTESIAN_POINT('Ctrl Pts',(-2.64359851684131,-1.,-2.89747231723345));
#53105=CARTESIAN_POINT('Ctrl Pts',(-2.63717442263932,-1.,-2.89358228854544));
#53106=CARTESIAN_POINT('Ctrl Pts',(-2.63080195420767,-1.,-2.88967244854239));
#53107=CARTESIAN_POINT('Ctrl Pts',(-2.62447947640262,-1.,-2.88573922195059));
#53108=CARTESIAN_POINT('Ctrl Pts',(-2.61819596473108,-1.,-2.88176821427525));
#53109=CARTESIAN_POINT('Ctrl Pts',(-2.61193507170955,-1.,-2.87773881947915));
#53110=CARTESIAN_POINT('Ctrl Pts',(-2.60568177881303,-1.,-2.87363176656501));
#53111=CARTESIAN_POINT('Ctrl Pts',(-2.5994287522321,-1.,-2.86943633170722));
#53112=CARTESIAN_POINT('Ctrl Pts',(-2.59318160184908,-1.,-2.86515629953513));
#53113=CARTESIAN_POINT('Ctrl Pts',(-2.58696770643524,-1.,-2.86081999003629));
#53114=CARTESIAN_POINT('Ctrl Pts',(-2.58082875254357,-1.,-2.85647171715092));
#53115=CARTESIAN_POINT('Ctrl Pts',(-2.57480482727081,-1.,-2.85215360144431));
#53116=CARTESIAN_POINT('Ctrl Pts',(-2.56891984251721,-1.,-2.84788893329067));
#53117=CARTESIAN_POINT('Ctrl Pts',(-2.56316920798513,-1.,-2.84366802680237));
#53118=CARTESIAN_POINT('Ctrl Pts',(-2.55749952145241,-1.,-2.83942515220782));
#53119=CARTESIAN_POINT('Ctrl Pts',(-2.55182152807077,-1.,-2.83505269592536));
#53120=CARTESIAN_POINT('Ctrl Pts',(-2.54604736792655,-1.,-2.83044254225917));
#53121=CARTESIAN_POINT('Ctrl Pts',(-2.54012272520199,-1.,-2.8255216764922));
#53122=CARTESIAN_POINT('Ctrl Pts',(-2.53405679667412,-1.,-2.82028550483689));
#53123=CARTESIAN_POINT('Ctrl Pts',(-2.52796388055278,-1.,-2.81484379048475));
#53124=CARTESIAN_POINT('Ctrl Pts',(-2.52205778589653,-1.,-2.80941521966941));
#53125=CARTESIAN_POINT('Ctrl Pts',(-2.51660190465805,-1.,-2.80427363984653));
#53126=CARTESIAN_POINT('Ctrl Pts',(-2.51186983687818,-1.,-2.79970585014168));
#53127=CARTESIAN_POINT('Ctrl Pts',(-2.50810555977671,-1.,-2.79596878057287));
#53128=CARTESIAN_POINT('Ctrl Pts',(-2.50567182569081,-1.,-2.79344192164147));
#53129=CARTESIAN_POINT('Ctrl Pts',(-2.50455968395146,-1.,-2.79217568804755));
#53130=CARTESIAN_POINT('Ctrl Pts',(-2.50417932839313,-1.,-2.79164172518905));
#53131=CARTESIAN_POINT('Ctrl Pts',(-2.50410700351493,-1.,-2.79145823440781));
#53132=CARTESIAN_POINT('Ctrl Pts',(-2.50410331873176,-1.,-2.79140942341258));
#53133=CARTESIAN_POINT('',(-2.36531447826213,-1.,-2.90994629141562));
#53134=CARTESIAN_POINT('Origin',(0.,-1.,0.));
#53135=CARTESIAN_POINT('',(-2.52982887637028,-1.,-3.35260583073571));
#53136=CARTESIAN_POINT('Ctrl Pts',(-2.36531447826213,-1.,-2.90994629141562));
#53137=CARTESIAN_POINT('Ctrl Pts',(-2.3653621118858,-1.,-2.90995756655558));
#53138=CARTESIAN_POINT('Ctrl Pts',(-2.36553202948741,-1.,-2.9100577052777));
#53139=CARTESIAN_POINT('Ctrl Pts',(-2.36599991765853,-1.,-2.91051690822262));
#53140=CARTESIAN_POINT('Ctrl Pts',(-2.36707658451709,-1.,-2.91181344022628));
#53141=CARTESIAN_POINT('Ctrl Pts',(-2.36919161373074,-1.,-2.91461249883016));
#53142=CARTESIAN_POINT('Ctrl Pts',(-2.37229381109939,-1.,-2.9189150379156));
#53143=CARTESIAN_POINT('Ctrl Pts',(-2.37606510524271,-1.,-2.92430340582912));
#53144=CARTESIAN_POINT('Ctrl Pts',(-2.3802898958232,-1.,-2.93049643640517));
#53145=CARTESIAN_POINT('Ctrl Pts',(-2.38472771516476,-1.,-2.93717903280599));
#53146=CARTESIAN_POINT('Ctrl Pts',(-2.38914929090806,-1.,-2.94404820669135));
#53147=CARTESIAN_POINT('Ctrl Pts',(-2.39337207631613,-1.,-2.95085857128372));
#53148=CARTESIAN_POINT('Ctrl Pts',(-2.39730553974412,-1.,-2.95748006482811));
#53149=CARTESIAN_POINT('Ctrl Pts',(-2.40095565711535,-1.,-2.96390432240181));
#53150=CARTESIAN_POINT('Ctrl Pts',(-2.40438604734848,-1.,-2.97019641312272));
#53151=CARTESIAN_POINT('Ctrl Pts',(-2.40768975073691,-1.,-2.97646002822395));
#53152=CARTESIAN_POINT('Ctrl Pts',(-2.41095909342591,-1.,-2.98280015815132));
#53153=CARTESIAN_POINT('Ctrl Pts',(-2.4142506419963,-1.,-2.98927983005851));
#53154=CARTESIAN_POINT('Ctrl Pts',(-2.4175732450056,-1.,-2.99590509293561));
#53155=CARTESIAN_POINT('Ctrl Pts',(-2.42090763946812,-1.,-3.00264868586038));
#53156=CARTESIAN_POINT('Ctrl Pts',(-2.42421849439625,-1.,-3.00946442616674));
#53157=CARTESIAN_POINT('Ctrl Pts',(-2.4274685626416,-1.,-3.01630420830494));
#53158=CARTESIAN_POINT('Ctrl Pts',(-2.43063415586615,-1.,-3.02313656035977));
#53159=CARTESIAN_POINT('Ctrl Pts',(-2.43371241361462,-1.,-3.02995534946946));
#53160=CARTESIAN_POINT('Ctrl Pts',(-2.43671278042394,-1.,-3.03676949672797));
#53161=CARTESIAN_POINT('Ctrl Pts',(-2.43965194061849,-1.,-3.04359685040545));
#53162=CARTESIAN_POINT('Ctrl Pts',(-2.44254768923109,-1.,-3.05045678021509));
#53163=CARTESIAN_POINT('Ctrl Pts',(-2.44541251892568,-1.,-3.05736242671521));
#53164=CARTESIAN_POINT('Ctrl Pts',(-2.44824970516558,-1.,-3.06431596421422));
#53165=CARTESIAN_POINT('Ctrl Pts',(-2.45105688854432,-1.,-3.0713129052131));
#53166=CARTESIAN_POINT('Ctrl Pts',(-2.45382826787795,-1.,-3.07834472886145));
#53167=CARTESIAN_POINT('Ctrl Pts',(-2.45655725437037,-1.,-3.08540206545313));
#53168=CARTESIAN_POINT('Ctrl Pts',(-2.45923912563875,-1.,-3.09247787931881));
#53169=CARTESIAN_POINT('Ctrl Pts',(-2.4618730850188,-1.,-3.09956993697048));
#53170=CARTESIAN_POINT('Ctrl Pts',(-2.46446082979645,-1.,-3.10667907901981));
#53171=CARTESIAN_POINT('Ctrl Pts',(-2.46700558843507,-1.,-3.11380805536124));
#53172=CARTESIAN_POINT('Ctrl Pts',(-2.4695109894747,-1.,-3.12096015766984));
#53173=CARTESIAN_POINT('Ctrl Pts',(-2.47197997765868,-1.,-3.12813790805948));
#53174=CARTESIAN_POINT('Ctrl Pts',(-2.47441378371923,-1.,-3.13534181229282));
#53175=CARTESIAN_POINT('Ctrl Pts',(-2.47681245356095,-1.,-3.14257099546531));
#53176=CARTESIAN_POINT('Ctrl Pts',(-2.47917529057016,-1.,-3.14982373241335));
#53177=CARTESIAN_POINT('Ctrl Pts',(-2.48150133566568,-1.,-3.15709802322735));
#53178=CARTESIAN_POINT('Ctrl Pts',(-2.48378981792739,-1.,-3.16439213290181));
#53179=CARTESIAN_POINT('Ctrl Pts',(-2.48604065348619,-1.,-3.17170518863357));
#53180=CARTESIAN_POINT('Ctrl Pts',(-2.48825428288243,-1.,-3.17903698136679));
#53181=CARTESIAN_POINT('Ctrl Pts',(-2.49043146334095,-1.,-3.18638771282315));
#53182=CARTESIAN_POINT('Ctrl Pts',(-2.4925730723986,-1.,-3.19375775555814));
#53183=CARTESIAN_POINT('Ctrl Pts',(-2.49467992057726,-1.,-3.20114742397549));
#53184=CARTESIAN_POINT('Ctrl Pts',(-2.49675252647298,-1.,-3.2085566984974));
#53185=CARTESIAN_POINT('Ctrl Pts',(-2.49879114599293,-1.,-3.21598526261157));
#53186=CARTESIAN_POINT('Ctrl Pts',(-2.5007958720187,-1.,-3.22343262620387));
#53187=CARTESIAN_POINT('Ctrl Pts',(-2.50276671338074,-1.,-3.23089822320596));
#53188=CARTESIAN_POINT('Ctrl Pts',(-2.50470367580078,-1.,-3.23838151080383));
#53189=CARTESIAN_POINT('Ctrl Pts',(-2.50660685940645,-1.,-3.24588208984042));
#53190=CARTESIAN_POINT('Ctrl Pts',(-2.50847647070936,-1.,-3.25339971461265));
#53191=CARTESIAN_POINT('Ctrl Pts',(-2.51031277813697,-1.,-3.26093423001716));
#53192=CARTESIAN_POINT('Ctrl Pts',(-2.51211608411539,-1.,-3.26848552888271));
#53193=CARTESIAN_POINT('Ctrl Pts',(-2.51388669270329,-1.,-3.27605350473048));
#53194=CARTESIAN_POINT('Ctrl Pts',(-2.51562487464215,-1.,-3.28363799702583));
#53195=CARTESIAN_POINT('Ctrl Pts',(-2.51733085123316,-1.,-3.2912387729863));
#53196=CARTESIAN_POINT('Ctrl Pts',(-2.51900480700548,-1.,-3.29885556387661));
#53197=CARTESIAN_POINT('Ctrl Pts',(-2.52064689568167,-1.,-3.30648808814986));
#53198=CARTESIAN_POINT('Ctrl Pts',(-2.52225724871375,-1.,-3.31413607874727));
#53199=CARTESIAN_POINT('Ctrl Pts',(-2.52383598396878,-1.,-3.32179931079521));
#53200=CARTESIAN_POINT('Ctrl Pts',(-2.52538321165774,-1.,-3.32947762189049));
#53201=CARTESIAN_POINT('Ctrl Pts',(-2.52689902691551,-1.,-3.33717090000955));
#53202=CARTESIAN_POINT('Ctrl Pts',(-2.52808660916879,-1.,-3.34333744117093));
#53203=CARTESIAN_POINT('Ctrl Pts',(-2.5289632161143,-1.,-3.34796903577628));
#53204=CARTESIAN_POINT('Ctrl Pts',(-2.52954136549357,-1.,-3.35105973714426));
#53205=CARTESIAN_POINT('Ctrl Pts',(-2.52982887637028,-1.,-3.35260583073571));
#53206=CARTESIAN_POINT('',(-2.40675750623143,-1.,-3.44202241512147));
#53207=CARTESIAN_POINT('',(-2.52982887637028,-1.,-3.35260583073571));
#53208=CARTESIAN_POINT('',(-2.03660101169715,-1.,-3.14877060440327));
#53209=CARTESIAN_POINT('Ctrl Pts',(-2.40675750623143,-1.,-3.44202241512147));
#53210=CARTESIAN_POINT('Ctrl Pts',(-2.4053759295909,-1.,-3.44127120683039));
#53211=CARTESIAN_POINT('Ctrl Pts',(-2.40261515589405,-1.,-3.43976627484234));
#53212=CARTESIAN_POINT('Ctrl Pts',(-2.39848113410292,-1.,-3.43750133064416));
#53213=CARTESIAN_POINT('Ctrl Pts',(-2.39298338804493,-1.,-3.4344663067854));
#53214=CARTESIAN_POINT('Ctrl Pts',(-2.38613505843552,-1.,-3.4306473271292));
#53215=CARTESIAN_POINT('Ctrl Pts',(-2.37931067028926,-1.,-3.42680309754399));
#53216=CARTESIAN_POINT('Ctrl Pts',(-2.37251035954292,-1.,-3.42293356216511));
#53217=CARTESIAN_POINT('Ctrl Pts',(-2.36573431470642,-1.,-3.41903866635852));
#53218=CARTESIAN_POINT('Ctrl Pts',(-2.35898278606946,-1.,-3.41511836751469));
#53219=CARTESIAN_POINT('Ctrl Pts',(-2.35225606824109,-1.,-3.41117262314119));
#53220=CARTESIAN_POINT('Ctrl Pts',(-2.34555447649188,-1.,-3.40720137404297));
#53221=CARTESIAN_POINT('Ctrl Pts',(-2.33887832342782,-1.,-3.40320452776743));
#53222=CARTESIAN_POINT('Ctrl Pts',(-2.33222789882489,-1.,-3.39918194577956));
#53223=CARTESIAN_POINT('Ctrl Pts',(-2.3256034390248,-1.,-3.39513342019756));
#53224=CARTESIAN_POINT('Ctrl Pts',(-2.31900513925424,-1.,-3.39105869474822));
#53225=CARTESIAN_POINT('Ctrl Pts',(-2.31243319489367,-1.,-3.38695751492462));
#53226=CARTESIAN_POINT('Ctrl Pts',(-2.30588783640343,-1.,-3.3828296733661));
#53227=CARTESIAN_POINT('Ctrl Pts',(-2.29936936127624,-1.,-3.37867504959433));
#53228=CARTESIAN_POINT('Ctrl Pts',(-2.29287818007393,-1.,-3.37449367172826));
#53229=CARTESIAN_POINT('Ctrl Pts',(-2.28641481081137,-1.,-3.37028570206488));
#53230=CARTESIAN_POINT('Ctrl Pts',(-2.27997979458037,-1.,-3.36605130713076));
#53231=CARTESIAN_POINT('Ctrl Pts',(-2.2735736262093,-1.,-3.36179055004409));
#53232=CARTESIAN_POINT('Ctrl Pts',(-2.2671966857991,-1.,-3.35750328523061));
#53233=CARTESIAN_POINT('Ctrl Pts',(-2.26084915222449,-1.,-3.35318902552626));
#53234=CARTESIAN_POINT('Ctrl Pts',(-2.25453097693483,-1.,-3.34884690292285));
#53235=CARTESIAN_POINT('Ctrl Pts',(-2.24824207678256,-1.,-3.34447596770723));
#53236=CARTESIAN_POINT('Ctrl Pts',(-2.24198249391422,-1.,-3.34007543738025));
#53237=CARTESIAN_POINT('Ctrl Pts',(-2.23575256328812,-1.,-3.33564495756482));
#53238=CARTESIAN_POINT('Ctrl Pts',(-2.22955308907233,-1.,-3.33118487773611));
#53239=CARTESIAN_POINT('Ctrl Pts',(-2.22338548312772,-1.,-3.3266964672289));
#53240=CARTESIAN_POINT('Ctrl Pts',(-2.21725135110898,-1.,-3.32218125618968));
#53241=CARTESIAN_POINT('Ctrl Pts',(-2.21115211847875,-1.,-3.31764044024235));
#53242=CARTESIAN_POINT('Ctrl Pts',(-2.20508863150607,-1.,-3.31307424608949));
#53243=CARTESIAN_POINT('Ctrl Pts',(-2.19906078949923,-1.,-3.30848134694595));
#53244=CARTESIAN_POINT('Ctrl Pts',(-2.19306710376111,-1.,-3.30385816281831));
#53245=CARTESIAN_POINT('Ctrl Pts',(-2.18710556500327,-1.,-3.29920022557639));
#53246=CARTESIAN_POINT('Ctrl Pts',(-2.18117455557065,-1.,-3.2945036150049));
#53247=CARTESIAN_POINT('Ctrl Pts',(-2.17527380048423,-1.,-3.28976645712568));
#53248=CARTESIAN_POINT('Ctrl Pts',(-2.16940517773455,-1.,-3.28499019979724));
#53249=CARTESIAN_POINT('Ctrl Pts',(-2.16357391934425,-1.,-3.280181508414));
#53250=CARTESIAN_POINT('Ctrl Pts',(-2.15778690038347,-1.,-3.27534954469187));
#53251=CARTESIAN_POINT('Ctrl Pts',(-2.15205043199808,-1.,-3.27050245897228));
#53252=CARTESIAN_POINT('Ctrl Pts',(-2.1463680529566,-1.,-3.26564388189759));
#53253=CARTESIAN_POINT('Ctrl Pts',(-2.14073870754264,-1.,-3.26077002641879));
#53254=CARTESIAN_POINT('Ctrl Pts',(-2.13515375878803,-1.,-3.25586495065054));
#53255=CARTESIAN_POINT('Ctrl Pts',(-2.12960028396832,-1.,-3.25090574494028));
#53256=CARTESIAN_POINT('Ctrl Pts',(-2.12406646410962,-1.,-3.24587102613376));
#53257=CARTESIAN_POINT('Ctrl Pts',(-2.11854673326979,-1.,-3.24074905517293));
#53258=CARTESIAN_POINT('Ctrl Pts',(-2.11304604021773,-1.,-3.23554444767099));
#53259=CARTESIAN_POINT('Ctrl Pts',(-2.10758699642451,-1.,-3.23028945793289));
#53260=CARTESIAN_POINT('Ctrl Pts',(-2.10220384298492,-1.,-3.22503437553434));
#53261=CARTESIAN_POINT('Ctrl Pts',(-2.09692958434895,-1.,-3.21982707347009));
#53262=CARTESIAN_POINT('Ctrl Pts',(-2.09178419460443,-1.,-3.21469429601654));
#53263=CARTESIAN_POINT('Ctrl Pts',(-2.08676465517455,-1.,-3.20962575845463));
#53264=CARTESIAN_POINT('Ctrl Pts',(-2.08182850370878,-1.,-3.2045481863073));
#53265=CARTESIAN_POINT('Ctrl Pts',(-2.07690441870722,-1.,-3.19934132836019));
#53266=CARTESIAN_POINT('Ctrl Pts',(-2.07192253497857,-1.,-3.19388465568252));
#53267=CARTESIAN_POINT('Ctrl Pts',(-2.06684062744112,-1.,-3.18809755562368));
#53268=CARTESIAN_POINT('Ctrl Pts',(-2.06166849827101,-1.,-3.18197692964614));
#53269=CARTESIAN_POINT('Ctrl Pts',(-2.05650186773132,-1.,-3.17564906975371));
#53270=CARTESIAN_POINT('Ctrl Pts',(-2.05151770247233,-1.,-3.16936341689527));
#53271=CARTESIAN_POINT('Ctrl Pts',(-2.04693331247446,-1.,-3.16343165058912));
#53272=CARTESIAN_POINT('Ctrl Pts',(-2.04297406404027,-1.,-3.15817983946367));
#53273=CARTESIAN_POINT('Ctrl Pts',(-2.03984073791519,-1.,-3.15389991674792));
#53274=CARTESIAN_POINT('Ctrl Pts',(-2.03783225495961,-1.,-3.15102344775328));
#53275=CARTESIAN_POINT('Ctrl Pts',(-2.03693188810544,-1.,-3.14959882629805));
#53276=CARTESIAN_POINT('Ctrl Pts',(-2.03663974554932,-1.,-3.1490119366901));
#53277=CARTESIAN_POINT('Ctrl Pts',(-2.03659701539259,-1.,-3.14881939088124));
#53278=CARTESIAN_POINT('Ctrl Pts',(-2.03660101169715,-1.,-3.14877060440328));
#53279=CARTESIAN_POINT('',(-1.88097764062697,-1.,-3.24413672884812));
#53280=CARTESIAN_POINT('Origin',(0.,-1.,0.));
#53281=CARTESIAN_POINT('',(-1.97421938526992,-1.,-3.70708211654725));
#53282=CARTESIAN_POINT('Ctrl Pts',(-1.88097764062697,-1.,-3.24413672884812));
#53283=CARTESIAN_POINT('Ctrl Pts',(-1.8810229239812,-1.,-3.24415531671284));
#53284=CARTESIAN_POINT('Ctrl Pts',(-1.88117508446775,-1.,-3.24428080353022));
#53285=CARTESIAN_POINT('Ctrl Pts',(-1.88156537699203,-1.,-3.24480754676064));
#53286=CARTESIAN_POINT('Ctrl Pts',(-1.88242596600454,-1.,-3.2462565441079));
#53287=CARTESIAN_POINT('Ctrl Pts',(-1.88407708646357,-1.,-3.24935200511918));
#53288=CARTESIAN_POINT('Ctrl Pts',(-1.88646802523466,-1.,-3.25408686339463));
#53289=CARTESIAN_POINT('Ctrl Pts',(-1.88934996203698,-1.,-3.25999885193947));
#53290=CARTESIAN_POINT('Ctrl Pts',(-1.89255393500965,-1.,-3.26677653888676));
#53291=CARTESIAN_POINT('Ctrl Pts',(-1.89589172903793,-1.,-3.27407108933139));
#53292=CARTESIAN_POINT('Ctrl Pts',(-1.89918429230462,-1.,-3.28154737912352));
#53293=CARTESIAN_POINT('Ctrl Pts',(-1.90228971247527,-1.,-3.2889344860029));
#53294=CARTESIAN_POINT('Ctrl Pts',(-1.90513891864087,-1.,-3.29608978722113));
#53295=CARTESIAN_POINT('Ctrl Pts',(-1.90773912171341,-1.,-3.30300595568195));
#53296=CARTESIAN_POINT('Ctrl Pts',(-1.91014297830446,-1.,-3.30975721158596));
#53297=CARTESIAN_POINT('Ctrl Pts',(-1.91242616234442,-1.,-3.31646052426364));
#53298=CARTESIAN_POINT('Ctrl Pts',(-1.91466343916628,-1.,-3.32323403454535));
#53299=CARTESIAN_POINT('Ctrl Pts',(-1.91690081930331,-1.,-3.33014884257873));
#53300=CARTESIAN_POINT('Ctrl Pts',(-1.9191460961021,-1.,-3.33721230710012));
#53301=CARTESIAN_POINT('Ctrl Pts',(-1.92138450828404,-1.,-3.34439448941961));
#53302=CARTESIAN_POINT('Ctrl Pts',(-1.92358838440528,-1.,-3.35164424847223));
#53303=CARTESIAN_POINT('Ctrl Pts',(-1.92572846125756,-1.,-3.35890824422965));
#53304=CARTESIAN_POINT('Ctrl Pts',(-1.92778626543786,-1.,-3.36615168657567));
#53305=CARTESIAN_POINT('Ctrl Pts',(-1.92975993109877,-1.,-3.37336807068043));
#53306=CARTESIAN_POINT('Ctrl Pts',(-1.93165739093276,-1.,-3.3805676852555));
#53307=CARTESIAN_POINT('Ctrl Pts',(-1.93349233176788,-1.,-3.38777076883256));
#53308=CARTESIAN_POINT('Ctrl Pts',(-1.93527929945985,-1.,-3.39499923640795));
#53309=CARTESIAN_POINT('Ctrl Pts',(-1.93702857723098,-1.,-3.40226802104109));
#53310=CARTESIAN_POINT('Ctrl Pts',(-1.93874306008143,-1.,-3.40957978266642));
#53311=CARTESIAN_POINT('Ctrl Pts',(-1.94042111965246,-1.,-3.41692971994096));
#53312=CARTESIAN_POINT('Ctrl Pts',(-1.94205835913696,-1.,-3.42430850941503));
#53313=CARTESIAN_POINT('Ctrl Pts',(-1.94364973660284,-1.,-3.43170586602434));
#53314=CARTESIAN_POINT('Ctrl Pts',(-1.94519168842879,-1.,-3.43911410197687));
#53315=CARTESIAN_POINT('Ctrl Pts',(-1.94668377715329,-1.,-3.44653088665681));
#53316=CARTESIAN_POINT('Ctrl Pts',(-1.94812754766524,-1.,-3.45395731584051));
#53317=CARTESIAN_POINT('Ctrl Pts',(-1.94952575850197,-1.,-3.46139661060962));
#53318=CARTESIAN_POINT('Ctrl Pts',(-1.95088147859877,-1.,-3.46885258974191));
#53319=CARTESIAN_POINT('Ctrl Pts',(-1.95219722189876,-1.,-3.47632820495921));
#53320=CARTESIAN_POINT('Ctrl Pts',(-1.95347412486309,-1.,-3.48382414832634));
#53321=CARTESIAN_POINT('Ctrl Pts',(-1.95471236969643,-1.,-3.49133956289133));
#53322=CARTESIAN_POINT('Ctrl Pts',(-1.95591153823661,-1.,-3.49887263575583));
#53323=CARTESIAN_POINT('Ctrl Pts',(-1.95707099606511,-1.,-3.50642124159909));
#53324=CARTESIAN_POINT('Ctrl Pts',(-1.95819025316779,-1.,-3.51398354617794));
#53325=CARTESIAN_POINT('Ctrl Pts',(-1.95926936324461,-1.,-3.52155867431486));
#53326=CARTESIAN_POINT('Ctrl Pts',(-1.96030879411566,-1.,-3.52914648844351));
#53327=CARTESIAN_POINT('Ctrl Pts',(-1.96130926212689,-1.,-3.53674730625813));
#53328=CARTESIAN_POINT('Ctrl Pts',(-1.96227157573067,-1.,-3.54436163300443));
#53329=CARTESIAN_POINT('Ctrl Pts',(-1.96319648628644,-1.,-3.55198990600886));
#53330=CARTESIAN_POINT('Ctrl Pts',(-1.96408450906812,-1.,-3.55963218706096));
#53331=CARTESIAN_POINT('Ctrl Pts',(-1.96493594634567,-1.,-3.56728820357791));
#53332=CARTESIAN_POINT('Ctrl Pts',(-1.96575096652789,-1.,-3.57495748600959));
#53333=CARTESIAN_POINT('Ctrl Pts',(-1.96652966688911,-1.,-3.58263947663829));
#53334=CARTESIAN_POINT('Ctrl Pts',(-1.96727213799544,-1.,-3.59033364022801));
#53335=CARTESIAN_POINT('Ctrl Pts',(-1.96797854118369,-1.,-3.59803959819938));
#53336=CARTESIAN_POINT('Ctrl Pts',(-1.9686491188594,-1.,-3.60575714017989));
#53337=CARTESIAN_POINT('Ctrl Pts',(-1.96928416040877,-1.,-3.61348615496704));
#53338=CARTESIAN_POINT('Ctrl Pts',(-1.96988398129978,-1.,-3.62122658401893));
#53339=CARTESIAN_POINT('Ctrl Pts',(-1.97044889850463,-1.,-3.62897836973293));
#53340=CARTESIAN_POINT('Ctrl Pts',(-1.97097920454464,-1.,-3.63674139590412));
#53341=CARTESIAN_POINT('Ctrl Pts',(-1.97147515441164,-1.,-3.64451546723514));
#53342=CARTESIAN_POINT('Ctrl Pts',(-1.9719369724024,-1.,-3.652300347166));
#53343=CARTESIAN_POINT('Ctrl Pts',(-1.9723648543905,-1.,-3.6600957816636));
#53344=CARTESIAN_POINT('Ctrl Pts',(-1.97275897198678,-1.,-3.66790152752075));
#53345=CARTESIAN_POINT('Ctrl Pts',(-1.97311947678517,-1.,-3.67571738107084));
#53346=CARTESIAN_POINT('Ctrl Pts',(-1.97344650304519,-1.,-3.68354319915092));
#53347=CARTESIAN_POINT('Ctrl Pts',(-1.97374016225483,-1.,-3.69137888599902));
#53348=CARTESIAN_POINT('Ctrl Pts',(-1.97394846383216,-1.,-3.6976552856004));
#53349=CARTESIAN_POINT('Ctrl Pts',(-1.97408973726715,-1.,-3.70236698912904));
#53350=CARTESIAN_POINT('Ctrl Pts',(-1.97417727645308,-1.,-3.70551008132332));
#53351=CARTESIAN_POINT('Ctrl Pts',(-1.97421938526992,-1.,-3.70708211654725));
#53352=CARTESIAN_POINT('',(-1.83867539237861,-1.,-3.77614523045147));
#53353=CARTESIAN_POINT('',(-1.97421938526992,-1.,-3.70708211654725));
#53354=CARTESIAN_POINT('',(-1.5189508286633,-1.,-3.42859860294306));
#53355=CARTESIAN_POINT('Ctrl Pts',(-1.83867539237861,-1.,-3.77614523045147));
#53356=CARTESIAN_POINT('Ctrl Pts',(-1.83742834010626,-1.,-3.77518714457833));
#53357=CARTESIAN_POINT('Ctrl Pts',(-1.83493697934534,-1.,-3.77326886064398));
#53358=CARTESIAN_POINT('Ctrl Pts',(-1.83120816955645,-1.,-3.77038509817999));
#53359=CARTESIAN_POINT('Ctrl Pts',(-1.82625289220915,-1.,-3.76652740353775));
#53360=CARTESIAN_POINT('Ctrl Pts',(-1.82008629694091,-1.,-3.76168412707948));
#53361=CARTESIAN_POINT('Ctrl Pts',(-1.8139472983358,-1.,-3.75681965683071));
#53362=CARTESIAN_POINT('Ctrl Pts',(-1.80783603939617,-1.,-3.75193395887977));
#53363=CARTESIAN_POINT('Ctrl Pts',(-1.8017527148577,-1.,-3.74702700875467));
#53364=CARTESIAN_POINT('Ctrl Pts',(-1.79569757859422,-1.,-3.74209880352445));
#53365=CARTESIAN_POINT('Ctrl Pts',(-1.78967092823491,-1.,-3.73714934730681));
#53366=CARTESIAN_POINT('Ctrl Pts',(-1.78367308442901,-1.,-3.7321786309547));
#53367=CARTESIAN_POINT('Ctrl Pts',(-1.77770437039658,-1.,-3.72718661205609));
#53368=CARTESIAN_POINT('Ctrl Pts',(-1.77176509401761,-1.,-3.72217319911254));
#53369=CARTESIAN_POINT('Ctrl Pts',(-1.76585552124394,-1.,-3.71713822377359));
#53370=CARTESIAN_POINT('Ctrl Pts',(-1.75997588498865,-1.,-3.71208146346136));
#53371=CARTESIAN_POINT('Ctrl Pts',(-1.75412641804042,-1.,-3.70700269736659));
#53372=CARTESIAN_POINT('Ctrl Pts',(-1.74830738046057,-1.,-3.7019017567335));
#53373=CARTESIAN_POINT('Ctrl Pts',(-1.74251908492617,-1.,-3.69677856910517));
#53374=CARTESIAN_POINT('Ctrl Pts',(-1.73676193254557,-1.,-3.69163322648036));
#53375=CARTESIAN_POINT('Ctrl Pts',(-1.73103640956717,-1.,-3.68646597019332));
#53376=CARTESIAN_POINT('Ctrl Pts',(-1.72534302437056,-1.,-3.68127704936579));
#53377=CARTESIAN_POINT('Ctrl Pts',(-1.71968225581808,-1.,-3.67606660374709));
#53378=CARTESIAN_POINT('Ctrl Pts',(-1.71405450210384,-1.,-3.67083454901611));
#53379=CARTESIAN_POINT('Ctrl Pts',(-1.70846001610956,-1.,-3.66558043198876));
#53380=CARTESIAN_POINT('Ctrl Pts',(-1.70289888566873,-1.,-3.66030338774847));
#53381=CARTESIAN_POINT('Ctrl Pts',(-1.69737117722534,-1.,-3.65500246526749));
#53382=CARTESIAN_POINT('Ctrl Pts',(-1.69187705481689,-1.,-3.64967689827371));
#53383=CARTESIAN_POINT('Ctrl Pts',(-1.68641690471457,-1.,-3.64432638915203));
#53384=CARTESIAN_POINT('Ctrl Pts',(-1.68099146651586,-1.,-3.63895140887462));
#53385=CARTESIAN_POINT('Ctrl Pts',(-1.67560193613156,-1.,-3.63355343201232));
#53386=CARTESIAN_POINT('Ctrl Pts',(-1.67024966008045,-1.,-3.62813422105271));
#53387=CARTESIAN_POINT('Ctrl Pts',(-1.66493585923855,-1.,-3.62269517989109));
#53388=CARTESIAN_POINT('Ctrl Pts',(-1.65966133399186,-1.,-3.61723666482456));
#53389=CARTESIAN_POINT('Ctrl Pts',(-1.65442619244325,-1.,-3.61175734965127));
#53390=CARTESIAN_POINT('Ctrl Pts',(-1.64922952425832,-1.,-3.60625346556992));
#53391=CARTESIAN_POINT('Ctrl Pts',(-1.64407004385582,-1.,-3.60072028513845));
#53392=CARTESIAN_POINT('Ctrl Pts',(-1.63894676675352,-1.,-3.59515368334893));
#53393=CARTESIAN_POINT('Ctrl Pts',(-1.6338597145126,-1.,-3.58955176627879));
#53394=CARTESIAN_POINT('Ctrl Pts',(-1.62881051550745,-1.,-3.58391625774343));
#53395=CARTESIAN_POINT('Ctrl Pts',(-1.62380329464844,-1.,-3.5782545595439));
#53396=CARTESIAN_POINT('Ctrl Pts',(-1.61884340915404,-1.,-3.57257679609806));
#53397=CARTESIAN_POINT('Ctrl Pts',(-1.61393581747514,-1.,-3.56689200468387));
#53398=CARTESIAN_POINT('Ctrl Pts',(-1.60908344685457,-1.,-3.5612043248298));
#53399=CARTESIAN_POINT('Ctrl Pts',(-1.60428584699853,-1.,-3.55550985096129));
#53400=CARTESIAN_POINT('Ctrl Pts',(-1.59953698113457,-1.,-3.54979148634454));
#53401=CARTESIAN_POINT('Ctrl Pts',(-1.59482766949766,-1.,-3.54402458182337));
#53402=CARTESIAN_POINT('Ctrl Pts',(-1.59014958368739,-1.,-3.53818616861077));
#53403=CARTESIAN_POINT('Ctrl Pts',(-1.58549906268088,-1.,-3.5322637814708));
#53404=CARTESIAN_POINT('Ctrl Pts',(-1.58088027227848,-1.,-3.52626275334881));
#53405=CARTESIAN_POINT('Ctrl Pts',(-1.57631049988158,-1.,-3.52021847865912));
#53406=CARTESIAN_POINT('Ctrl Pts',(-1.57181569799743,-1.,-3.51418598431665));
#53407=CARTESIAN_POINT('Ctrl Pts',(-1.56742097575012,-1.,-3.50821771695363));
#53408=CARTESIAN_POINT('Ctrl Pts',(-1.56314187758675,-1.,-3.50234321621578));
#53409=CARTESIAN_POINT('Ctrl Pts',(-1.55897703097874,-1.,-3.49655185179655));
#53410=CARTESIAN_POINT('Ctrl Pts',(-1.55489595901116,-1.,-3.4907646087742));
#53411=CARTESIAN_POINT('Ctrl Pts',(-1.55084702970452,-1.,-3.48485155928567));
#53412=CARTESIAN_POINT('Ctrl Pts',(-1.54678009290276,-1.,-3.47868272898751));
#53413=CARTESIAN_POINT('Ctrl Pts',(-1.54266605398187,-1.,-3.47217189224653));
#53414=CARTESIAN_POINT('Ctrl Pts',(-1.53851507915502,-1.,-3.46531752207153));
#53415=CARTESIAN_POINT('Ctrl Pts',(-1.53440195378792,-1.,-3.45825932955032));
#53416=CARTESIAN_POINT('Ctrl Pts',(-1.53046244461635,-1.,-3.45127136828305));
#53417=CARTESIAN_POINT('Ctrl Pts',(-1.52686242875556,-1.,-3.44469547526647));
#53418=CARTESIAN_POINT('Ctrl Pts',(-1.5237734895035,-1.,-3.4388889597401));
#53419=CARTESIAN_POINT('Ctrl Pts',(-1.52134826724293,-1.,-3.43417156977893));
#53420=CARTESIAN_POINT('Ctrl Pts',(-1.5198144909338,-1.,-3.43101631893414));
#53421=CARTESIAN_POINT('Ctrl Pts',(-1.51914806898491,-1.,-3.42946838852587));
#53422=CARTESIAN_POINT('Ctrl Pts',(-1.5189513329503,-1.,-3.42884302333841));
#53423=CARTESIAN_POINT('Ctrl Pts',(-1.51893924967331,-1.,-3.42864616361875));
#53424=CARTESIAN_POINT('Ctrl Pts',(-1.5189508286633,-1.,-3.42859860294306));
#53425=CARTESIAN_POINT('',(-1.35032489087269,-1.,-3.49844575334386));
#53426=CARTESIAN_POINT('Origin',(0.,-1.,0.));
#53427=CARTESIAN_POINT('',(-1.36999806084572,-1.,-3.97027773754922));
#53428=CARTESIAN_POINT('Ctrl Pts',(-1.35032489087269,-1.,-3.49844575334386));
#53429=CARTESIAN_POINT('Ctrl Pts',(-1.35036670893102,-1.,-3.49847119623841));
#53430=CARTESIAN_POINT('Ctrl Pts',(-1.35049736560633,-1.,-3.49861894124915));
#53431=CARTESIAN_POINT('Ctrl Pts',(-1.35080045218652,-1.,-3.49920025459856));
#53432=CARTESIAN_POINT('Ctrl Pts',(-1.35142377279535,-1.,-3.5007660381658));
#53433=CARTESIAN_POINT('Ctrl Pts',(-1.3525703284343,-1.,-3.50408168106113));
#53434=CARTESIAN_POINT('Ctrl Pts',(-1.35419113576022,-1.,-3.50913227060177));
#53435=CARTESIAN_POINT('Ctrl Pts',(-1.35611275237288,-1.,-3.51542230699919));
#53436=CARTESIAN_POINT('Ctrl Pts',(-1.35821701528975,-1.,-3.52261776117121));
#53437=CARTESIAN_POINT('Ctrl Pts',(-1.36037259643827,-1.,-3.53034464961849));
#53438=CARTESIAN_POINT('Ctrl Pts',(-1.36245507339334,-1.,-3.53824396425032));
#53439=CARTESIAN_POINT('Ctrl Pts',(-1.36436666257567,-1.,-3.54602591832893));
#53440=CARTESIAN_POINT('Ctrl Pts',(-1.36606145456711,-1.,-3.55353883995793));
#53441=CARTESIAN_POINT('Ctrl Pts',(-1.36754771771174,-1.,-3.56077662028492));
#53442=CARTESIAN_POINT('Ctrl Pts',(-1.36886584973349,-1.,-3.56782080304554));
#53443=CARTESIAN_POINT('Ctrl Pts',(-1.37007229485646,-1.,-3.57479875549453));
#53444=CARTESIAN_POINT('Ctrl Pts',(-1.37122241663073,-1.,-3.58183885982745));
#53445=CARTESIAN_POINT('Ctrl Pts',(-1.37235053661,-1.,-3.5890185384643));
#53446=CARTESIAN_POINT('Ctrl Pts',(-1.37346320103184,-1.,-3.59634627869117));
#53447=CARTESIAN_POINT('Ctrl Pts',(-1.37455051379642,-1.,-3.60379020124038));
#53448=CARTESIAN_POINT('Ctrl Pts',(-1.37559314436641,-1.,-3.61129546591082));
#53449=CARTESIAN_POINT('Ctrl Pts',(-1.37657053403102,-1.,-3.61880481160408));
#53450=CARTESIAN_POINT('Ctrl Pts',(-1.37746987919868,-1.,-3.62628098665112));
#53451=CARTESIAN_POINT('Ctrl Pts',(-1.37829035457324,-1.,-3.63371727442448));
#53452=CARTESIAN_POINT('Ctrl Pts',(-1.37903818567347,-1.,-3.64112507791112));
#53453=CARTESIAN_POINT('Ctrl Pts',(-1.37972372481598,-1.,-3.64852652756444));
#53454=CARTESIAN_POINT('Ctrl Pts',(-1.38035791051215,-1.,-3.65594554404396));
#53455=CARTESIAN_POINT('Ctrl Pts',(-1.38094856333558,-1.,-3.66339848520874));
#53456=CARTESIAN_POINT('Ctrl Pts',(-1.38149812653876,-1.,-3.67088843112282));
#53457=CARTESIAN_POINT('Ctrl Pts',(-1.38200574290626,-1.,-3.6784103848243));
#53458=CARTESIAN_POINT('Ctrl Pts',(-1.38246852827185,-1.,-3.68595444983844));
#53459=CARTESIAN_POINT('Ctrl Pts',(-1.38288311171649,-1.,-3.69350967899523));
#53460=CARTESIAN_POINT('Ctrl Pts',(-1.38324717612862,-1.,-3.70106792167894));
#53461=CARTESIAN_POINT('Ctrl Pts',(-1.38356065402122,-1.,-3.70862680753343));
#53462=CARTESIAN_POINT('Ctrl Pts',(-1.38382489984585,-1.,-3.7161876605181));
#53463=CARTESIAN_POINT('Ctrl Pts',(-1.3840421342895,-1.,-3.72375409358805));
#53464=CARTESIAN_POINT('Ctrl Pts',(-1.38421479111531,-1.,-3.73133035859283));
#53465=CARTESIAN_POINT('Ctrl Pts',(-1.38434489156456,-1.,-3.73891976418099));
#53466=CARTESIAN_POINT('Ctrl Pts',(-1.38443344984389,-1.,-3.7465231716786));
#53467=CARTESIAN_POINT('Ctrl Pts',(-1.38448077997155,-1.,-3.75413976318727));
#53468=CARTESIAN_POINT('Ctrl Pts',(-1.38448675253343,-1.,-3.76176768271347));
#53469=CARTESIAN_POINT('Ctrl Pts',(-1.38445107339517,-1.,-3.76940473185775));
#53470=CARTESIAN_POINT('Ctrl Pts',(-1.38437354551435,-1.,-3.77704902230441));
#53471=CARTESIAN_POINT('Ctrl Pts',(-1.38425435883773,-1.,-3.78469969805134));
#53472=CARTESIAN_POINT('Ctrl Pts',(-1.38409399694589,-1.,-3.79235669640907));
#53473=CARTESIAN_POINT('Ctrl Pts',(-1.38389311766701,-1.,-3.80002044322169));
#53474=CARTESIAN_POINT('Ctrl Pts',(-1.38365244046226,-1.,-3.80769156398429));
#53475=CARTESIAN_POINT('Ctrl Pts',(-1.38337263902766,-1.,-3.81537060817765));
#53476=CARTESIAN_POINT('Ctrl Pts',(-1.38305421262724,-1.,-3.82305771743715));
#53477=CARTESIAN_POINT('Ctrl Pts',(-1.38269750245086,-1.,-3.83075266982138));
#53478=CARTESIAN_POINT('Ctrl Pts',(-1.38230274828774,-1.,-3.83845502790609));
#53479=CARTESIAN_POINT('Ctrl Pts',(-1.38187013346089,-1.,-3.84616425605705));
#53480=CARTESIAN_POINT('Ctrl Pts',(-1.38139983115075,-1.,-3.85387983979557));
#53481=CARTESIAN_POINT('Ctrl Pts',(-1.38089205993067,-1.,-3.86160143044187));
#53482=CARTESIAN_POINT('Ctrl Pts',(-1.38034709213129,-1.,-3.86932885813403));
#53483=CARTESIAN_POINT('Ctrl Pts',(-1.37976523097187,-1.,-3.87706205830865));
#53484=CARTESIAN_POINT('Ctrl Pts',(-1.37914679719446,-1.,-3.88480102249461));
#53485=CARTESIAN_POINT('Ctrl Pts',(-1.37849211287981,-1.,-3.89254574338385));
#53486=CARTESIAN_POINT('Ctrl Pts',(-1.3778014851263,-1.,-3.90029615196255));
#53487=CARTESIAN_POINT('Ctrl Pts',(-1.3770751963376,-1.,-3.90805209522729));
#53488=CARTESIAN_POINT('Ctrl Pts',(-1.37631350505516,-1.,-3.91581337461825));
#53489=CARTESIAN_POINT('Ctrl Pts',(-1.37551664448057,-1.,-3.92357976987132));
#53490=CARTESIAN_POINT('Ctrl Pts',(-1.37468482215784,-1.,-3.93135106761941));
#53491=CARTESIAN_POINT('Ctrl Pts',(-1.37381821967499,-1.,-3.93912709041791));
#53492=CARTESIAN_POINT('Ctrl Pts',(-1.37291699203423,-1.,-3.94690771786926));
#53493=CARTESIAN_POINT('Ctrl Pts',(-1.37198126433139,-1.,-3.95469287283105));
#53494=CARTESIAN_POINT('Ctrl Pts',(-1.37120515615663,-1.,-3.96092458508407));
#53495=CARTESIAN_POINT('Ctrl Pts',(-1.37060761746027,-1.,-3.96560037975788));
#53496=CARTESIAN_POINT('Ctrl Pts',(-1.37020239094758,-1.,-3.9687184694173));
#53497=CARTESIAN_POINT('Ctrl Pts',(-1.36999806084572,-1.,-3.97027773754922));
#53498=CARTESIAN_POINT('',(-1.22531898815164,-1.,-4.01728681790024));
#53499=CARTESIAN_POINT('',(-1.36999806084572,-1.,-3.97027773754922));
#53500=CARTESIAN_POINT('',(-0.963899035118986,-1.,-3.62400312501199));
#53501=CARTESIAN_POINT('Ctrl Pts',(-1.22531898815164,-1.,-4.01728681790024));
#53502=CARTESIAN_POINT('Ctrl Pts',(-1.22423716681317,-1.,-4.01614544569895));
#53503=CARTESIAN_POINT('Ctrl Pts',(-1.22207656455845,-1.,-4.01386104433519));
#53504=CARTESIAN_POINT('Ctrl Pts',(-1.21884478244403,-1.,-4.01042947140789));
#53505=CARTESIAN_POINT('Ctrl Pts',(-1.21455398918133,-1.,-4.00584409522722));
#53506=CARTESIAN_POINT('Ctrl Pts',(-1.20922097029551,-1.,-4.00009577950721));
#53507=CARTESIAN_POINT('Ctrl Pts',(-1.20391852375139,-1.,-3.99433084799666));
#53508=CARTESIAN_POINT('Ctrl Pts',(-1.19864679609566,-1.,-3.98854928957189));
#53509=CARTESIAN_POINT('Ctrl Pts',(-1.19340598349475,-1.,-3.98275111052561));
#53510=CARTESIAN_POINT('Ctrl Pts',(-1.18819633715539,-1.,-3.97693634767754));
#53511=CARTESIAN_POINT('Ctrl Pts',(-1.18301815039831,-1.,-3.97110505165415));
#53512=CARTESIAN_POINT('Ctrl Pts',(-1.17787174135592,-1.,-3.96525726358159));
#53513=CARTESIAN_POINT('Ctrl Pts',(-1.17275743590361,-1.,-3.95939299213276));
#53514=CARTESIAN_POINT('Ctrl Pts',(-1.16767555244438,-1.,-3.95351219509876));
#53515=CARTESIAN_POINT('Ctrl Pts',(-1.16262637999157,-1.,-3.94761474780583));
#53516=CARTESIAN_POINT('Ctrl Pts',(-1.15761018340956,-1.,-3.94170046685203));
#53517=CARTESIAN_POINT('Ctrl Pts',(-1.1526272271632,-1.,-3.9357691705628));
#53518=CARTESIAN_POINT('Ctrl Pts',(-1.14767779451123,-1.,-3.92982073294257));
#53519=CARTESIAN_POINT('Ctrl Pts',(-1.14276220561593,-1.,-3.92385513133997));
#53520=CARTESIAN_POINT('Ctrl Pts',(-1.13788084225554,-1.,-3.91787251936827));
#53521=CARTESIAN_POINT('Ctrl Pts',(-1.13303414693896,-1.,-3.91187321145649));
#53522=CARTESIAN_POINT('Ctrl Pts',(-1.12822258281553,-1.,-3.90585753318737));
#53523=CARTESIAN_POINT('Ctrl Pts',(-1.12344660099043,-1.,-3.89982569750025));
#53524=CARTESIAN_POINT('Ctrl Pts',(-1.11870660794603,-1.,-3.89377768340344));
#53525=CARTESIAN_POINT('Ctrl Pts',(-1.11400292434429,-1.,-3.88771308285171));
#53526=CARTESIAN_POINT('Ctrl Pts',(-1.10933577224008,-1.,-3.88163105531724));
#53527=CARTESIAN_POINT('Ctrl Pts',(-1.10470536603287,-1.,-3.87553067187514));
#53528=CARTESIAN_POINT('Ctrl Pts',(-1.10011198761195,-1.,-3.86941120134849));
#53529=CARTESIAN_POINT('Ctrl Pts',(-1.09555606505013,-1.,-3.86327241021247));
#53530=CARTESIAN_POINT('Ctrl Pts',(-1.09103825516294,-1.,-3.85711487933931));
#53531=CARTESIAN_POINT('Ctrl Pts',(-1.08655950846384,-1.,-3.85094025222713));
#53532=CARTESIAN_POINT('Ctrl Pts',(-1.08212087917991,-1.,-3.8447504803063));
#53533=CARTESIAN_POINT('Ctrl Pts',(-1.07772335353858,-1.,-3.83854714117491));
#53534=CARTESIAN_POINT('Ctrl Pts',(-1.07336766633459,-1.,-3.83233071195144));
#53535=CARTESIAN_POINT('Ctrl Pts',(-1.06905413180359,-1.,-3.82609989967276));
#53536=CARTESIAN_POINT('Ctrl Pts',(-1.0647824403893,-1.,-3.81985083953012));
#53537=CARTESIAN_POINT('Ctrl Pts',(-1.06055206187299,-1.,-3.8135786611749));
#53538=CARTESIAN_POINT('Ctrl Pts',(-1.05636266918644,-1.,-3.80727913637791));
#53539=CARTESIAN_POINT('Ctrl Pts',(-1.05221457990016,-1.,-3.80095039790681));
#53540=CARTESIAN_POINT('Ctrl Pts',(-1.04810913267639,-1.,-3.79459440308786));
#53541=CARTESIAN_POINT('Ctrl Pts',(-1.04404924374422,-1.,-3.78821910787179));
#53542=CARTESIAN_POINT('Ctrl Pts',(-1.04003862055798,-1.,-3.7818353500817));
#53543=CARTESIAN_POINT('Ctrl Pts',(-1.03608074678008,-1.,-3.77545283140427));
#53544=CARTESIAN_POINT('Ctrl Pts',(-1.03217786604919,-1.,-3.76907609832516));
#53545=CARTESIAN_POINT('Ctrl Pts',(-1.02833014458184,-1.,-3.76270122291245));
#53546=CARTESIAN_POINT('Ctrl Pts',(-1.02453429444668,-1.,-3.75631037456224));
#53547=CARTESIAN_POINT('Ctrl Pts',(-1.02078510487439,-1.,-3.74987777155873));
#53548=CARTESIAN_POINT('Ctrl Pts',(-1.01707794311088,-1.,-3.74337942504993));
#53549=CARTESIAN_POINT('Ctrl Pts',(-1.01341114319906,-1.,-3.73680245055747));
#53550=CARTESIAN_POINT('Ctrl Pts',(-1.00978798539491,-1.,-3.73015276704407));
#53551=CARTESIAN_POINT('Ctrl Pts',(-1.00622000735696,-1.,-3.72346803750544));
#53552=CARTESIAN_POINT('Ctrl Pts',(-1.00272423396802,-1.,-3.71680667125047));
#53553=CARTESIAN_POINT('Ctrl Pts',(-0.999317260756344,-1.,-3.7102243971387));
#53554=CARTESIAN_POINT('Ctrl Pts',(-0.996009819772432,-1.,-3.70375282282107));
#53555=CARTESIAN_POINT('Ctrl Pts',(-0.992802218332104,-1.,-3.69738123415696));
#53556=CARTESIAN_POINT('Ctrl Pts',(-0.989676715398858,-1.,-3.69102682138955));
#53557=CARTESIAN_POINT('Ctrl Pts',(-0.986602639864286,-1.,-3.6845531792623));
#53558=CARTESIAN_POINT('Ctrl Pts',(-0.983550791470864,-1.,-3.67782408841876));
#53559=CARTESIAN_POINT('Ctrl Pts',(-0.980505922458494,-1.,-3.67074983340444));
#53560=CARTESIAN_POINT('Ctrl Pts',(-0.977478312751416,-1.,-3.66333049637403));
#53561=CARTESIAN_POINT('Ctrl Pts',(-0.974519971354139,-1.,-3.6557157673487));
#53562=CARTESIAN_POINT('Ctrl Pts',(-0.971722122060277,-1.,-3.64819756447072));
#53563=CARTESIAN_POINT('Ctrl Pts',(-0.969195124674829,-1.,-3.64113946505393));
#53564=CARTESIAN_POINT('Ctrl Pts',(-0.967052554540877,-1.,-3.6349212208096));
#53565=CARTESIAN_POINT('Ctrl Pts',(-0.965395153165716,-1.,-3.62988252139998));
#53566=CARTESIAN_POINT('Ctrl Pts',(-0.964373850166081,-1.,-3.62652618145252));
#53567=CARTESIAN_POINT('Ctrl Pts',(-0.963957782642589,-1.,-3.62489305727516));
#53568=CARTESIAN_POINT('Ctrl Pts',(-0.963861297423579,-1.,-3.62424461507455));
#53569=CARTESIAN_POINT('Ctrl Pts',(-0.963880158556713,-1.,-3.62404828878374));
#53570=CARTESIAN_POINT('Ctrl Pts',(-0.963899035118986,-1.,-3.62400312501199));
#53571=CARTESIAN_POINT('',(-0.786422660833743,-1.,-3.66661143271648));
#53572=CARTESIAN_POINT('Origin',(0.,-1.,0.));
#53573=CARTESIAN_POINT('',(-0.732042837400619,-1.,-4.13571194405636));
#53574=CARTESIAN_POINT('Ctrl Pts',(-0.786422660833743,-1.,-3.66661143271648));
#53575=CARTESIAN_POINT('Ctrl Pts',(-0.786459983896781,-1.,-3.66664310415236));
#53576=CARTESIAN_POINT('Ctrl Pts',(-0.78656591955989,-1.,-3.66680946938396));
#53577=CARTESIAN_POINT('Ctrl Pts',(-0.786774337198499,-1.,-3.66743103898844));
#53578=CARTESIAN_POINT('Ctrl Pts',(-0.787145041181589,-1.,-3.66907505398769));
#53579=CARTESIAN_POINT('Ctrl Pts',(-0.787758799995426,-1.,-3.672529236635));
#53580=CARTESIAN_POINT('Ctrl Pts',(-0.788569566220662,-1.,-3.67777119516438));
#53581=CARTESIAN_POINT('Ctrl Pts',(-0.789483546065158,-1.,-3.68428439784285));
#53582=CARTESIAN_POINT('Ctrl Pts',(-0.79043628498958,-1.,-3.69172044327754));
#53583=CARTESIAN_POINT('Ctrl Pts',(-0.791356575696509,-1.,-3.69968940808982));
#53584=CARTESIAN_POINT('Ctrl Pts',(-0.792177688845968,-1.,-3.70781724021879));
#53585=CARTESIAN_POINT('Ctrl Pts',(-0.792848377370115,-1.,-3.7158024239604));
#53586=CARTESIAN_POINT('Ctrl Pts',(-0.79334702378387,-1.,-3.7234879729357));
#53587=CARTESIAN_POINT('Ctrl Pts',(-0.793682750269347,-1.,-3.7308691469564));
#53588=CARTESIAN_POINT('Ctrl Pts',(-0.79388270093679,-1.,-3.73803280541576));
#53589=CARTESIAN_POINT('Ctrl Pts',(-0.79398270045988,-1.,-3.74511357728827));
#53590=CARTESIAN_POINT('Ctrl Pts',(-0.794017347371441,-1.,-3.75224692493895));
#53591=CARTESIAN_POINT('Ctrl Pts',(-0.794008429135047,-1.,-3.75951468666325));
#53592=CARTESIAN_POINT('Ctrl Pts',(-0.793961083689141,-1.,-3.76692626931184));
#53593=CARTESIAN_POINT('Ctrl Pts',(-0.793870523787515,-1.,-3.77444863801264));
#53594=CARTESIAN_POINT('Ctrl Pts',(-0.793726235781339,-1.,-3.78202460377617));
#53595=CARTESIAN_POINT('Ctrl Pts',(-0.793516871680966,-1.,-3.78959439439222));
#53596=CARTESIAN_POINT('Ctrl Pts',(-0.7932356129732,-1.,-3.79711921389862));
#53597=CARTESIAN_POINT('Ctrl Pts',(-0.792882695234693,-1.,-3.80459229925598));
#53598=CARTESIAN_POINT('Ctrl Pts',(-0.792462483517568,-1.,-3.81202588694726));
#53599=CARTESIAN_POINT('Ctrl Pts',(-0.791981740718606,-1.,-3.81944345442237));
#53600=CARTESIAN_POINT('Ctrl Pts',(-0.791447528662381,-1.,-3.82687033899799));
#53601=CARTESIAN_POINT('Ctrl Pts',(-0.79086501270534,-1.,-3.83432392054804));
#53602=CARTESIAN_POINT('Ctrl Pts',(-0.790236124191289,-1.,-3.84180762342476));
#53603=CARTESIAN_POINT('Ctrl Pts',(-0.789560798155619,-1.,-3.8493163780891));
#53604=CARTESIAN_POINT('Ctrl Pts',(-0.788837734090688,-1.,-3.85683995872536));
#53605=CARTESIAN_POINT('Ctrl Pts',(-0.788065315093771,-1.,-3.86436702561342));
#53606=CARTESIAN_POINT('Ctrl Pts',(-0.78724252761798,-1.,-3.87188916600905));
#53607=CARTESIAN_POINT('Ctrl Pts',(-0.786369675812592,-1.,-3.87940402818186));
#53608=CARTESIAN_POINT('Ctrl Pts',(-0.785447890340723,-1.,-3.88691313167399));
#53609=CARTESIAN_POINT('Ctrl Pts',(-0.784478799358336,-1.,-3.89442039235105));
#53610=CARTESIAN_POINT('Ctrl Pts',(-0.783464141529082,-1.,-3.90193039043971));
#53611=CARTESIAN_POINT('Ctrl Pts',(-0.782405395622759,-1.,-3.90944671004536));
#53612=CARTESIAN_POINT('Ctrl Pts',(-0.781303428618344,-1.,-3.9169703605466));
#53613=CARTESIAN_POINT('Ctrl Pts',(-0.780158678615507,-1.,-3.92450058323799));
#53614=CARTESIAN_POINT('Ctrl Pts',(-0.778971308134786,-1.,-3.93203552473153));
#53615=CARTESIAN_POINT('Ctrl Pts',(-0.77774137056855,-1.,-3.93957296768098));
#53616=CARTESIAN_POINT('Ctrl Pts',(-0.77646896669796,-1.,-3.94711101619471));
#53617=CARTESIAN_POINT('Ctrl Pts',(-0.775154418039441,-1.,-3.95464885452364));
#53618=CARTESIAN_POINT('Ctrl Pts',(-0.773798212026683,-1.,-3.96218649639876));
#53619=CARTESIAN_POINT('Ctrl Pts',(-0.772400931772239,-1.,-3.96972446532832));
#53620=CARTESIAN_POINT('Ctrl Pts',(-0.770963190030504,-1.,-3.97726349165507));
#53621=CARTESIAN_POINT('Ctrl Pts',(-0.769485566245459,-1.,-3.98480422348403));
#53622=CARTESIAN_POINT('Ctrl Pts',(-0.767968531377708,-1.,-3.99234687880892));
#53623=CARTESIAN_POINT('Ctrl Pts',(-0.766412457135786,-1.,-3.99989129179464));
#53624=CARTESIAN_POINT('Ctrl Pts',(-0.764817648784946,-1.,-4.00743706791366));
#53625=CARTESIAN_POINT('Ctrl Pts',(-0.763184371182827,-1.,-4.01498370680434));
#53626=CARTESIAN_POINT('Ctrl Pts',(-0.761512875859942,-1.,-4.02253072741347));
#53627=CARTESIAN_POINT('Ctrl Pts',(-0.759803433244166,-1.,-4.0300778195465));
#53628=CARTESIAN_POINT('Ctrl Pts',(-0.758056338885554,-1.,-4.03762485803468));
#53629=CARTESIAN_POINT('Ctrl Pts',(-0.756271902370187,-1.,-4.04517182654344));
#53630=CARTESIAN_POINT('Ctrl Pts',(-0.754450441816412,-1.,-4.05271876688106));
#53631=CARTESIAN_POINT('Ctrl Pts',(-0.752592276482869,-1.,-4.06026572221399));
#53632=CARTESIAN_POINT('Ctrl Pts',(-0.750697720483176,-1.,-4.06781267241886));
#53633=CARTESIAN_POINT('Ctrl Pts',(-0.748767076679177,-1.,-4.07535951055363));
#53634=CARTESIAN_POINT('Ctrl Pts',(-0.746800631490822,-1.,-4.08290608094789));
#53635=CARTESIAN_POINT('Ctrl Pts',(-0.744798649705514,-1.,-4.09045220253011));
#53636=CARTESIAN_POINT('Ctrl Pts',(-0.742761369690018,-1.,-4.09799769702712));
#53637=CARTESIAN_POINT('Ctrl Pts',(-0.740688998555152,-1.,-4.1055424175856));
#53638=CARTESIAN_POINT('Ctrl Pts',(-0.738581708229119,-1.,-4.11308626953795));
#53639=CARTESIAN_POINT('Ctrl Pts',(-0.736439634335347,-1.,-4.12062919626082));
#53640=CARTESIAN_POINT('Ctrl Pts',(-0.734698226767512,-1.,-4.12666277572794));
#53641=CARTESIAN_POINT('Ctrl Pts',(-0.733376589325634,-1.,-4.13118752796397));
#53642=CARTESIAN_POINT('Ctrl Pts',(-0.732488575135926,-1.,-4.13420383737278));
#53643=CARTESIAN_POINT('Ctrl Pts',(-0.732042837400619,-1.,-4.13571194405636));
#53644=CARTESIAN_POINT('',(-0.581791163835814,-1.,-4.15950947128175));
#53645=CARTESIAN_POINT('',(-0.732042837400619,-1.,-4.13571194405636));
#53646=CARTESIAN_POINT('',(-0.385112848332549,-1.,-3.73017266276632));
#53647=CARTESIAN_POINT('Ctrl Pts',(-0.581791163835814,-1.,-4.15950947128175));
#53648=CARTESIAN_POINT('Ctrl Pts',(-0.580901211462913,-1.,-4.15821291712391));
#53649=CARTESIAN_POINT('Ctrl Pts',(-0.579124568912543,-1.,-4.15561864787379));
#53650=CARTESIAN_POINT('Ctrl Pts',(-0.576469391673917,-1.,-4.1517237611974));
#53651=CARTESIAN_POINT('Ctrl Pts',(-0.572948736066277,-1.,-4.14652361065787));
#53652=CARTESIAN_POINT('Ctrl Pts',(-0.568580610187116,-1.,-4.14001179828669));
#53653=CARTESIAN_POINT('Ctrl Pts',(-0.564245279535705,-1.,-4.13348835726086));
#53654=CARTESIAN_POINT('Ctrl Pts',(-0.559942890594628,-1.,-4.12695329951859));
#53655=CARTESIAN_POINT('Ctrl Pts',(-0.555673636130778,-1.,-4.1204066619623));
#53656=CARTESIAN_POINT('Ctrl Pts',(-0.551437758498247,-1.,-4.11384852025578));
#53657=CARTESIAN_POINT('Ctrl Pts',(-0.54723553948676,-1.,-4.1072789702877));
#53658=CARTESIAN_POINT('Ctrl Pts',(-0.543067286878457,-1.,-4.10069810244473));
#53659=CARTESIAN_POINT('Ctrl Pts',(-0.538933321179921,-1.,-4.09410597627116));
#53660=CARTESIAN_POINT('Ctrl Pts',(-0.534833963476999,-1.,-4.08750259988693));
#53661=CARTESIAN_POINT('Ctrl Pts',(-0.530769518728075,-1.,-4.08088789536488));
#53662=CARTESIAN_POINT('Ctrl Pts',(-0.526740277227,-1.,-4.07426172299496));
#53663=CARTESIAN_POINT('Ctrl Pts',(-0.522746528602768,-1.,-4.06762394471075));
#53664=CARTESIAN_POINT('Ctrl Pts',(-0.51878857233681,-1.,-4.06097448037934));
#53665=CARTESIAN_POINT('Ctrl Pts',(-0.514866728193104,-1.,-4.05431335771261));
#53666=CARTESIAN_POINT('Ctrl Pts',(-0.510981349219174,-1.,-4.04764078815591));
#53667=CARTESIAN_POINT('Ctrl Pts',(-0.507132823288362,-1.,-4.04095715149074));
#53668=CARTESIAN_POINT('Ctrl Pts',(-0.503321556915514,-1.,-4.0342628417439));
#53669=CARTESIAN_POINT('Ctrl Pts',(-0.49954796234089,-1.,-4.0275581398015));
#53670=CARTESIAN_POINT('Ctrl Pts',(-0.495812444326223,-1.,-4.02084308851813));
#53671=CARTESIAN_POINT('Ctrl Pts',(-0.492115383417931,-1.,-4.01411733503486));
#53672=CARTESIAN_POINT('Ctrl Pts',(-0.488457130424531,-1.,-4.0073800839092));
#53673=CARTESIAN_POINT('Ctrl Pts',(-0.484838042421754,-1.,-4.00063045119234));
#53674=CARTESIAN_POINT('Ctrl Pts',(-0.481258512209638,-1.,-3.99386775880655));
#53675=CARTESIAN_POINT('Ctrl Pts',(-0.477718999122033,-1.,-3.98709184306743));
#53676=CARTESIAN_POINT('Ctrl Pts',(-0.474220061019542,-1.,-3.9803033804443));
#53677=CARTESIAN_POINT('Ctrl Pts',(-0.470762379613477,-1.,-3.97350414289415));
#53678=CARTESIAN_POINT('Ctrl Pts',(-0.467346690880672,-1.,-3.96669622273946));
#53679=CARTESIAN_POINT('Ctrl Pts',(-0.463973722115744,-1.,-3.95988133243543));
#53680=CARTESIAN_POINT('Ctrl Pts',(-0.460644124429119,-1.,-3.95306005817363));
#53681=CARTESIAN_POINT('Ctrl Pts',(-0.457358410451674,-1.,-3.94623117206675));
#53682=CARTESIAN_POINT('Ctrl Pts',(-0.454116879027576,-1.,-3.93939080846298));
#53683=CARTESIAN_POINT('Ctrl Pts',(-0.450919768356347,-1.,-3.93253407403128));
#53684=CARTESIAN_POINT('Ctrl Pts',(-0.447767416837297,-1.,-3.92565674143424));
#53685=CARTESIAN_POINT('Ctrl Pts',(-0.444660430230593,-1.,-3.91875701610721));
#53686=CARTESIAN_POINT('Ctrl Pts',(-0.441599824524047,-1.,-3.91183704069146));
#53687=CARTESIAN_POINT('Ctrl Pts',(-0.438587235458233,-1.,-3.90490512938546));
#53688=CARTESIAN_POINT('Ctrl Pts',(-0.435624629433506,-1.,-3.8979725665544));
#53689=CARTESIAN_POINT('Ctrl Pts',(-0.432713929544439,-1.,-3.89104947940592));
#53690=CARTESIAN_POINT('Ctrl Pts',(-0.429856640579734,-1.,-3.88414070943334));
#53691=CARTESIAN_POINT('Ctrl Pts',(-0.427053541173469,-1.,-3.87724240306609));
#53692=CARTESIAN_POINT('Ctrl Pts',(-0.424304173195142,-1.,-3.87033643487882));
#53693=CARTESIAN_POINT('Ctrl Pts',(-0.421607423177576,-1.,-3.86339652542749));
#53694=CARTESIAN_POINT('Ctrl Pts',(-0.41896246808681,-1.,-3.85639825648031));
#53695=CARTESIAN_POINT('Ctrl Pts',(-0.41636967805292,-1.,-3.8493286415751));
#53696=CARTESIAN_POINT('Ctrl Pts',(-0.413831367016727,-1.,-3.84219403994742));
#53697=CARTESIAN_POINT('Ctrl Pts',(-0.41135303879846,-1.,-3.83503345578645));
#53698=CARTESIAN_POINT('Ctrl Pts',(-0.408942371447377,-1.,-3.82790724256397));
#53699=CARTESIAN_POINT('Ctrl Pts',(-0.406607038258906,-1.,-3.82087303913741));
#53700=CARTESIAN_POINT('Ctrl Pts',(-0.404352694628236,-1.,-3.81396374287762));
#53701=CARTESIAN_POINT('Ctrl Pts',(-0.402181320148475,-1.,-3.80716881962763));
#53702=CARTESIAN_POINT('Ctrl Pts',(-0.400088346504727,-1.,-3.80040370384659));
#53703=CARTESIAN_POINT('Ctrl Pts',(-0.398064818684158,-1.,-3.79352887163457));
#53704=CARTESIAN_POINT('Ctrl Pts',(-0.396103205335029,-1.,-3.78640521279479));
#53705=CARTESIAN_POINT('Ctrl Pts',(-0.394202481011595,-1.,-3.77894173114368));
#53706=CARTESIAN_POINT('Ctrl Pts',(-0.392372786223347,-1.,-3.77114011595892));
#53707=CARTESIAN_POINT('Ctrl Pts',(-0.390642072979259,-1.,-3.76315635032993));
#53708=CARTESIAN_POINT('Ctrl Pts',(-0.389054775898251,-1.,-3.75529302894757));
#53709=CARTESIAN_POINT('Ctrl Pts',(-0.387663020050396,-1.,-3.74792651696269));
#53710=CARTESIAN_POINT('Ctrl Pts',(-0.386519576222035,-1.,-3.74144965781088));
#53711=CARTESIAN_POINT('Ctrl Pts',(-0.385670806454744,-1.,-3.73621371845475));
#53712=CARTESIAN_POINT('Ctrl Pts',(-0.385187124633965,-1.,-3.73273893363318));
#53713=CARTESIAN_POINT('Ctrl Pts',(-0.385031656499141,-1.,-3.73106082862399));
#53714=CARTESIAN_POINT('Ctrl Pts',(-0.385037797882046,-1.,-3.73040527620929));
#53715=CARTESIAN_POINT('Ctrl Pts',(-0.385087139001609,-1.,-3.73021431755218));
#53716=CARTESIAN_POINT('Ctrl Pts',(-0.385112848332549,-1.,-3.73017266276632));
#53717=CARTESIAN_POINT('',(-0.203156094897896,-1.,-3.74449296982994));
#53718=CARTESIAN_POINT('Origin',(0.,-1.,0.));
#53719=CARTESIAN_POINT('',(-0.0760622897878238,-1.,-4.19931119685982));
#53720=CARTESIAN_POINT('Ctrl Pts',(-0.203156094897896,-1.,-3.74449296982994));
#53721=CARTESIAN_POINT('Ctrl Pts',(-0.203188003947965,-1.,-3.74453008995129));
#53722=CARTESIAN_POINT('Ctrl Pts',(-0.203266610111264,-1.,-3.74471097893961));
#53723=CARTESIAN_POINT('Ctrl Pts',(-0.203375226874331,-1.,-3.74535749969262));
#53724=CARTESIAN_POINT('Ctrl Pts',(-0.203484186269315,-1.,-3.74703926501843));
#53725=CARTESIAN_POINT('Ctrl Pts',(-0.203550035479097,-1.,-3.75054693397716));
#53726=CARTESIAN_POINT('Ctrl Pts',(-0.203530796848404,-1.,-3.75585118707924));
#53727=CARTESIAN_POINT('Ctrl Pts',(-0.203414634707646,-1.,-3.76242717937273));
#53728=CARTESIAN_POINT('Ctrl Pts',(-0.203192390045337,-1.,-3.76992071595267));
#53729=CARTESIAN_POINT('Ctrl Pts',(-0.202854729699197,-1.,-3.77793553476879));
#53730=CARTESIAN_POINT('Ctrl Pts',(-0.202394260512193,-1.,-3.78609175019317));
#53731=CARTESIAN_POINT('Ctrl Pts',(-0.201807533800799,-1.,-3.79408354187274));
#53732=CARTESIAN_POINT('Ctrl Pts',(-0.201097756307252,-1.,-3.80175247447171));
#53733=CARTESIAN_POINT('Ctrl Pts',(-0.20027467943329,-1.,-3.80909529318501));
#53734=CARTESIAN_POINT('Ctrl Pts',(-0.199351525297396,-1.,-3.81620203429702));
#53735=CARTESIAN_POINT('Ctrl Pts',(-0.19834261690047,-1.,-3.82321127348981));
#53736=CARTESIAN_POINT('Ctrl Pts',(-0.197260935827375,-1.,-3.83026221776488));
#53737=CARTESIAN_POINT('Ctrl Pts',(-0.19611519897189,-1.,-3.83743910616265));
#53738=CARTESIAN_POINT('Ctrl Pts',(-0.194909009460255,-1.,-3.84475203347052));
#53739=CARTESIAN_POINT('Ctrl Pts',(-0.193642806777748,-1.,-3.85216762264019));
#53740=CARTESIAN_POINT('Ctrl Pts',(-0.19231515304498,-1.,-3.85962774407652));
#53741=CARTESIAN_POINT('Ctrl Pts',(-0.190924190418613,-1.,-3.8670715862477));
#53742=CARTESIAN_POINT('Ctrl Pts',(-0.189469253358254,-1.,-3.87445976418377));
#53743=CARTESIAN_POINT('Ctrl Pts',(-0.187951632512663,-1.,-3.88178563496187));
#53744=CARTESIAN_POINT('Ctrl Pts',(-0.186373724985263,-1.,-3.88906196725817));
#53745=CARTESIAN_POINT('Ctrl Pts',(-0.184738537728035,-1.,-3.89631300742633));
#53746=CARTESIAN_POINT('Ctrl Pts',(-0.183049081993193,-1.,-3.90356488555138));
#53747=CARTESIAN_POINT('Ctrl Pts',(-0.181307740731796,-1.,-3.91083557557193));
#53748=CARTESIAN_POINT('Ctrl Pts',(-0.179515885822895,-1.,-3.91812876180948));
#53749=CARTESIAN_POINT('Ctrl Pts',(-0.177674246152328,-1.,-3.92543942697672));
#53750=CARTESIAN_POINT('Ctrl Pts',(-0.175783136893873,-1.,-3.93275726771049));
#53751=CARTESIAN_POINT('Ctrl Pts',(-0.173842734974607,-1.,-3.94007083096214));
#53752=CARTESIAN_POINT('Ctrl Pts',(-0.171853355369233,-1.,-3.94737164900861));
#53753=CARTESIAN_POINT('Ctrl Pts',(-0.16981566637413,-1.,-3.95465744665263));
#53754=CARTESIAN_POINT('Ctrl Pts',(-0.167730547023312,-1.,-3.96192990160296));
#53755=CARTESIAN_POINT('Ctrl Pts',(-0.165598992851098,-1.,-3.9691931362141));
#53756=CARTESIAN_POINT('Ctrl Pts',(-0.163422004609999,-1.,-3.97645194630944));
#53757=CARTESIAN_POINT('Ctrl Pts',(-0.161200482186088,-1.,-3.98371010319866));
#53758=CARTESIAN_POINT('Ctrl Pts',(-0.158935123982796,-1.,-3.99096873945862));
#53759=CARTESIAN_POINT('Ctrl Pts',(-0.156626481393736,-1.,-3.99822717425869));
#53760=CARTESIAN_POINT('Ctrl Pts',(-0.15427500487231,-1.,-4.00548360245297));
#53761=CARTESIAN_POINT('Ctrl Pts',(-0.151881094022909,-1.,-4.01273584234684));
#53762=CARTESIAN_POINT('Ctrl Pts',(-0.149445144968708,-1.,-4.01998203715588));
#53763=CARTESIAN_POINT('Ctrl Pts',(-0.146967602878999,-1.,-4.02722143147048));
#53764=CARTESIAN_POINT('Ctrl Pts',(-0.144448947038352,-1.,-4.03445411510403));
#53765=CARTESIAN_POINT('Ctrl Pts',(-0.141889671485508,-1.,-4.04168069633842));
#53766=CARTESIAN_POINT('Ctrl Pts',(-0.13929026718006,-1.,-4.04890199238056));
#53767=CARTESIAN_POINT('Ctrl Pts',(-0.136651205046111,-1.,-4.05611873400122));
#53768=CARTESIAN_POINT('Ctrl Pts',(-0.133972916144225,-1.,-4.06333121018476));
#53769=CARTESIAN_POINT('Ctrl Pts',(-0.131255793548914,-1.,-4.07053931528579));
#53770=CARTESIAN_POINT('Ctrl Pts',(-0.128500200484814,-1.,-4.07774270738809));
#53771=CARTESIAN_POINT('Ctrl Pts',(-0.125706476822529,-1.,-4.08494093372315));
#53772=CARTESIAN_POINT('Ctrl Pts',(-0.122874946249119,-1.,-4.09213355850836));
#53773=CARTESIAN_POINT('Ctrl Pts',(-0.120005924388162,-1.,-4.09932031767243));
#53774=CARTESIAN_POINT('Ctrl Pts',(-0.117099722731705,-1.,-4.10650113382187));
#53775=CARTESIAN_POINT('Ctrl Pts',(-0.114156649609602,-1.,-4.11367603925313));
#53776=CARTESIAN_POINT('Ctrl Pts',(-0.111177012683377,-1.,-4.12084512502444));
#53777=CARTESIAN_POINT('Ctrl Pts',(-0.10816112052835,-1.,-4.12800848371386));
#53778=CARTESIAN_POINT('Ctrl Pts',(-0.105109286538864,-1.,-4.13516614458396));
#53779=CARTESIAN_POINT('Ctrl Pts',(-0.102021826577454,-1.,-4.14231804938737));
#53780=CARTESIAN_POINT('Ctrl Pts',(-0.0988990478899814,-1.,-4.1494640891762));
#53781=CARTESIAN_POINT('Ctrl Pts',(-0.095741240329707,-1.,-4.15660412653006));
#53782=CARTESIAN_POINT('Ctrl Pts',(-0.0925486672167692,-1.,-4.16373802265942));
#53783=CARTESIAN_POINT('Ctrl Pts',(-0.089321556085033,-1.,-4.17086566491823));
#53784=CARTESIAN_POINT('Ctrl Pts',(-0.0860600915552517,-1.,-4.17798698669991));
#53785=CARTESIAN_POINT('Ctrl Pts',(-0.0827644164389512,-1.,-4.1851019532944));
#53786=CARTESIAN_POINT('Ctrl Pts',(-0.0801005887117605,-1.,-4.19078883322483));
#53787=CARTESIAN_POINT('Ctrl Pts',(-0.0780873956244405,-1.,-4.19505112860624));
#53788=CARTESIAN_POINT('Ctrl Pts',(-0.0767384596142197,-1.,-4.19789138621624));
#53789=CARTESIAN_POINT('Ctrl Pts',(-0.0760622897878238,-1.,-4.19931119685982));
#53790=CARTESIAN_POINT('',(0.0760622897878244,-1.,-4.19931119685982));
#53791=CARTESIAN_POINT('',(-0.0760622897878238,-1.,-4.19931119685982));
#53792=CARTESIAN_POINT('',(0.2031560948961,-1.,-3.74449296983004));
#53793=CARTESIAN_POINT('Ctrl Pts',(0.0760622897878244,-1.,-4.19931119685982));
#53794=CARTESIAN_POINT('Ctrl Pts',(0.0767384596141462,-1.,-4.1978913862118));
#53795=CARTESIAN_POINT('Ctrl Pts',(0.0780873956242395,-1.,-4.19505112859416));
#53796=CARTESIAN_POINT('Ctrl Pts',(0.0801005887114317,-1.,-4.19078883320504));
#53797=CARTESIAN_POINT('Ctrl Pts',(0.0827644164385676,-1.,-4.18510195327123));
#53798=CARTESIAN_POINT('Ctrl Pts',(0.0860600915549394,-1.,-4.17798698668094));
#53799=CARTESIAN_POINT('Ctrl Pts',(0.0893215560848647,-1.,-4.17086566490794));
#53800=CARTESIAN_POINT('Ctrl Pts',(0.0925486672167528,-1.,-4.16373802265839));
#53801=CARTESIAN_POINT('Ctrl Pts',(0.0957412403298004,-1.,-4.15660412653577));
#53802=CARTESIAN_POINT('Ctrl Pts',(0.0988990478901223,-1.,-4.14946408918485));
#53803=CARTESIAN_POINT('Ctrl Pts',(0.102021826577584,-1.,-4.14231804939538));
#53804=CARTESIAN_POINT('Ctrl Pts',(0.105109286538945,-1.,-4.13516614458895));
#53805=CARTESIAN_POINT('Ctrl Pts',(0.108161120528369,-1.,-4.12800848371504));
#53806=CARTESIAN_POINT('Ctrl Pts',(0.111177012683346,-1.,-4.1208451250225));
#53807=CARTESIAN_POINT('Ctrl Pts',(0.114156649609545,-1.,-4.11367603924961));
#53808=CARTESIAN_POINT('Ctrl Pts',(0.117099722731648,-1.,-4.10650113381833));
#53809=CARTESIAN_POINT('Ctrl Pts',(0.120005924388124,-1.,-4.09932031767002));
#53810=CARTESIAN_POINT('Ctrl Pts',(0.122874946249107,-1.,-4.09213355850756));
#53811=CARTESIAN_POINT('Ctrl Pts',(0.12570647682254,-1.,-4.08494093372377));
#53812=CARTESIAN_POINT('Ctrl Pts',(0.128500200484837,-1.,-4.07774270738954));
#53813=CARTESIAN_POINT('Ctrl Pts',(0.13125579354894,-1.,-4.0705393152874));
#53814=CARTESIAN_POINT('Ctrl Pts',(0.133972916144245,-1.,-4.06333121018596));
#53815=CARTESIAN_POINT('Ctrl Pts',(0.136651205046119,-1.,-4.05611873400172));
#53816=CARTESIAN_POINT('Ctrl Pts',(0.139290267180057,-1.,-4.04890199238036));
#53817=CARTESIAN_POINT('Ctrl Pts',(0.1418896714855,-1.,-4.04168069633781));
#53818=CARTESIAN_POINT('Ctrl Pts',(0.144448947038344,-1.,-4.03445411510333));
#53819=CARTESIAN_POINT('Ctrl Pts',(0.146967602878994,-1.,-4.02722143146994));
#53820=CARTESIAN_POINT('Ctrl Pts',(0.149445144968707,-1.,-4.01998203715564));
#53821=CARTESIAN_POINT('Ctrl Pts',(0.15188109402291,-1.,-4.01273584234689));
#53822=CARTESIAN_POINT('Ctrl Pts',(0.15427500487231,-1.,-4.00548360245319));
#53823=CARTESIAN_POINT('Ctrl Pts',(0.156626481393734,-1.,-3.99822717425893));
#53824=CARTESIAN_POINT('Ctrl Pts',(0.158935123982793,-1.,-3.99096873945878));
#53825=CARTESIAN_POINT('Ctrl Pts',(0.161200482186084,-1.,-3.98371010319872));
#53826=CARTESIAN_POINT('Ctrl Pts',(0.163422004609999,-1.,-3.97645194630943));
#53827=CARTESIAN_POINT('Ctrl Pts',(0.165598992851102,-1.,-3.96919313621407));
#53828=CARTESIAN_POINT('Ctrl Pts',(0.167730547023319,-1.,-3.96192990160296));
#53829=CARTESIAN_POINT('Ctrl Pts',(0.169815666374139,-1.,-3.95465744665268));
#53830=CARTESIAN_POINT('Ctrl Pts',(0.17185335536924,-1.,-3.94737164900868));
#53831=CARTESIAN_POINT('Ctrl Pts',(0.173842734974609,-1.,-3.94007083096217));
#53832=CARTESIAN_POINT('Ctrl Pts',(0.175783136893868,-1.,-3.93275726771042));
#53833=CARTESIAN_POINT('Ctrl Pts',(0.177674246152317,-1.,-3.92543942697655));
#53834=CARTESIAN_POINT('Ctrl Pts',(0.179515885822881,-1.,-3.91812876180926));
#53835=CARTESIAN_POINT('Ctrl Pts',(0.181307740731785,-1.,-3.91083557557175));
#53836=CARTESIAN_POINT('Ctrl Pts',(0.18304908199319,-1.,-3.90356488555132));
#53837=CARTESIAN_POINT('Ctrl Pts',(0.184738537728043,-1.,-3.89631300742646));
#53838=CARTESIAN_POINT('Ctrl Pts',(0.18637372498528,-1.,-3.88906196725848));
#53839=CARTESIAN_POINT('Ctrl Pts',(0.187951632512685,-1.,-3.88178563496228));
#53840=CARTESIAN_POINT('Ctrl Pts',(0.189469253358272,-1.,-3.87445976418412));
#53841=CARTESIAN_POINT('Ctrl Pts',(0.19092419041862,-1.,-3.86707158624783));
#53842=CARTESIAN_POINT('Ctrl Pts',(0.19231515304497,-1.,-3.85962774407633));
#53843=CARTESIAN_POINT('Ctrl Pts',(0.193642806777723,-1.,-3.85216762263966));
#53844=CARTESIAN_POINT('Ctrl Pts',(0.19490900946022,-1.,-3.84475203346977));
#53845=CARTESIAN_POINT('Ctrl Pts',(0.196115198971859,-1.,-3.83743910616195));
#53846=CARTESIAN_POINT('Ctrl Pts',(0.197260935827361,-1.,-3.83026221776456));
#53847=CARTESIAN_POINT('Ctrl Pts',(0.198342616900486,-1.,-3.82321127349016));
#53848=CARTESIAN_POINT('Ctrl Pts',(0.199351525297447,-1.,-3.81620203429815));
#53849=CARTESIAN_POINT('Ctrl Pts',(0.200274679433364,-1.,-3.80909529318669));
#53850=CARTESIAN_POINT('Ctrl Pts',(0.201097756307326,-1.,-3.80175247447337));
#53851=CARTESIAN_POINT('Ctrl Pts',(0.201807533800837,-1.,-3.7940835418736));
#53852=CARTESIAN_POINT('Ctrl Pts',(0.20239426051216,-1.,-3.78609175019242));
#53853=CARTESIAN_POINT('Ctrl Pts',(0.202854729699081,-1.,-3.77793553476614));
#53854=CARTESIAN_POINT('Ctrl Pts',(0.203192390045164,-1.,-3.7699207159487));
#53855=CARTESIAN_POINT('Ctrl Pts',(0.203414634707478,-1.,-3.76242717936885));
#53856=CARTESIAN_POINT('Ctrl Pts',(0.203530796848321,-1.,-3.75585118707734));
#53857=CARTESIAN_POINT('Ctrl Pts',(0.203550035479166,-1.,-3.75054693397875));
#53858=CARTESIAN_POINT('Ctrl Pts',(0.203484186269415,-1.,-3.74703926501752));
#53859=CARTESIAN_POINT('Ctrl Pts',(0.203375226874121,-1.,-3.74535749969115));
#53860=CARTESIAN_POINT('Ctrl Pts',(0.203266610110531,-1.,-3.74471097893845));
#53861=CARTESIAN_POINT('Ctrl Pts',(0.203188003946657,-1.,-3.74453008995092));
#53862=CARTESIAN_POINT('Ctrl Pts',(0.2031560948961,-1.,-3.74449296983004));
#53863=CARTESIAN_POINT('',(0.385112848330761,-1.,-3.73017266276651));
#53864=CARTESIAN_POINT('Origin',(0.,-1.,0.));
#53865=CARTESIAN_POINT('',(0.581791163835815,-1.,-4.15950947128175));
#53866=CARTESIAN_POINT('Ctrl Pts',(0.385112848330761,-1.,-3.73017266276651));
#53867=CARTESIAN_POINT('Ctrl Pts',(0.385087139000374,-1.,-3.73021431755274));
#53868=CARTESIAN_POINT('Ctrl Pts',(0.385037797881504,-1.,-3.73040527621055));
#53869=CARTESIAN_POINT('Ctrl Pts',(0.385031656499164,-1.,-3.73106082862548));
#53870=CARTESIAN_POINT('Ctrl Pts',(0.385187124634206,-1.,-3.73273893363406));
#53871=CARTESIAN_POINT('Ctrl Pts',(0.385670806454565,-1.,-3.73621371845318));
#53872=CARTESIAN_POINT('Ctrl Pts',(0.386519576222251,-1.,-3.74144965781276));
#53873=CARTESIAN_POINT('Ctrl Pts',(0.387663020050836,-1.,-3.74792651696654));
#53874=CARTESIAN_POINT('Ctrl Pts',(0.389054775898701,-1.,-3.75529302895152));
#53875=CARTESIAN_POINT('Ctrl Pts',(0.390642072979559,-1.,-3.76315635033257));
#53876=CARTESIAN_POINT('Ctrl Pts',(0.392372786223432,-1.,-3.77114011595967));
#53877=CARTESIAN_POINT('Ctrl Pts',(0.394202481011499,-1.,-3.77894173114283));
#53878=CARTESIAN_POINT('Ctrl Pts',(0.39610320533484,-1.,-3.78640521279313));
#53879=CARTESIAN_POINT('Ctrl Pts',(0.398064818683969,-1.,-3.7935288716329));
#53880=CARTESIAN_POINT('Ctrl Pts',(0.4000883465046,-1.,-3.80040370384546));
#53881=CARTESIAN_POINT('Ctrl Pts',(0.402181320148435,-1.,-3.80716881962728));
#53882=CARTESIAN_POINT('Ctrl Pts',(0.404352694628273,-1.,-3.81396374287793));
#53883=CARTESIAN_POINT('Ctrl Pts',(0.406607038258985,-1.,-3.8208730391381));
#53884=CARTESIAN_POINT('Ctrl Pts',(0.408942371447459,-1.,-3.82790724256471));
#53885=CARTESIAN_POINT('Ctrl Pts',(0.411353038798518,-1.,-3.83503345578698));
#53886=CARTESIAN_POINT('Ctrl Pts',(0.413831367016748,-1.,-3.84219403994762));
#53887=CARTESIAN_POINT('Ctrl Pts',(0.416369678052906,-1.,-3.84932864157497));
#53888=CARTESIAN_POINT('Ctrl Pts',(0.418962468086773,-1.,-3.85639825647996));
#53889=CARTESIAN_POINT('Ctrl Pts',(0.421607423177534,-1.,-3.86339652542709));
#53890=CARTESIAN_POINT('Ctrl Pts',(0.42430417319511,-1.,-3.87033643487851));
#53891=CARTESIAN_POINT('Ctrl Pts',(0.427053541173457,-1.,-3.87724240306597));
#53892=CARTESIAN_POINT('Ctrl Pts',(0.429856640579741,-1.,-3.88414070943341));
#53893=CARTESIAN_POINT('Ctrl Pts',(0.432713929544458,-1.,-3.89104947940611));
#53894=CARTESIAN_POINT('Ctrl Pts',(0.435624629433527,-1.,-3.89797256655462));
#53895=CARTESIAN_POINT('Ctrl Pts',(0.438587235458249,-1.,-3.90490512938563));
#53896=CARTESIAN_POINT('Ctrl Pts',(0.441599824524054,-1.,-3.91183704069153));
#53897=CARTESIAN_POINT('Ctrl Pts',(0.44466043023059,-1.,-3.91875701610719));
#53898=CARTESIAN_POINT('Ctrl Pts',(0.447767416837292,-1.,-3.92565674143416));
#53899=CARTESIAN_POINT('Ctrl Pts',(0.450919768356348,-1.,-3.93253407403123));
#53900=CARTESIAN_POINT('Ctrl Pts',(0.454116879027584,-1.,-3.93939080846298));
#53901=CARTESIAN_POINT('Ctrl Pts',(0.457358410451682,-1.,-3.94623117206678));
#53902=CARTESIAN_POINT('Ctrl Pts',(0.460644124429121,-1.,-3.95306005817364));
#53903=CARTESIAN_POINT('Ctrl Pts',(0.463973722115733,-1.,-3.95988133243538));
#53904=CARTESIAN_POINT('Ctrl Pts',(0.467346690880643,-1.,-3.9666962227393));
#53905=CARTESIAN_POINT('Ctrl Pts',(0.470762379613439,-1.,-3.97350414289392));
#53906=CARTESIAN_POINT('Ctrl Pts',(0.474220061019509,-1.,-3.98030338044409));
#53907=CARTESIAN_POINT('Ctrl Pts',(0.477718999122027,-1.,-3.98709184306738));
#53908=CARTESIAN_POINT('Ctrl Pts',(0.481258512209675,-1.,-3.99386775880679));
#53909=CARTESIAN_POINT('Ctrl Pts',(0.484838042421834,-1.,-4.00063045119288));
#53910=CARTESIAN_POINT('Ctrl Pts',(0.488457130424633,-1.,-4.0073800839099));
#53911=CARTESIAN_POINT('Ctrl Pts',(0.492115383418018,-1.,-4.01411733503546));
#53912=CARTESIAN_POINT('Ctrl Pts',(0.495812444326251,-1.,-4.02084308851832));
#53913=CARTESIAN_POINT('Ctrl Pts',(0.499547962340821,-1.,-4.02755813980101));
#53914=CARTESIAN_POINT('Ctrl Pts',(0.503321556915346,-1.,-4.03426284174272));
#53915=CARTESIAN_POINT('Ctrl Pts',(0.507132823288136,-1.,-4.04095715148915));
#53916=CARTESIAN_POINT('Ctrl Pts',(0.51098134921897,-1.,-4.04764078815447));
#53917=CARTESIAN_POINT('Ctrl Pts',(0.514866728193016,-1.,-4.05431335771199));
#53918=CARTESIAN_POINT('Ctrl Pts',(0.518788572336923,-1.,-4.06097448038013));
#53919=CARTESIAN_POINT('Ctrl Pts',(0.522746528603107,-1.,-4.06762394471314));
#53920=CARTESIAN_POINT('Ctrl Pts',(0.526740277227498,-1.,-4.07426172299847));
#53921=CARTESIAN_POINT('Ctrl Pts',(0.53076951872857,-1.,-4.08088789536836));
#53922=CARTESIAN_POINT('Ctrl Pts',(0.534833963477273,-1.,-4.08750259988885));
#53923=CARTESIAN_POINT('Ctrl Pts',(0.538933321179755,-1.,-4.09410597627));
#53924=CARTESIAN_POINT('Ctrl Pts',(0.543067286877757,-1.,-4.10069810243979));
#53925=CARTESIAN_POINT('Ctrl Pts',(0.547235539485636,-1.,-4.10727897027977));
#53926=CARTESIAN_POINT('Ctrl Pts',(0.551437758497032,-1.,-4.11384852024721));
#53927=CARTESIAN_POINT('Ctrl Pts',(0.555673636129977,-1.,-4.12040666195664));
#53928=CARTESIAN_POINT('Ctrl Pts',(0.559942890594773,-1.,-4.12695329951961));
#53929=CARTESIAN_POINT('Ctrl Pts',(0.564245279537148,-1.,-4.13348835727104));
#53930=CARTESIAN_POINT('Ctrl Pts',(0.568580610189774,-1.,-4.14001179830547));
#53931=CARTESIAN_POINT('Ctrl Pts',(0.572948736069522,-1.,-4.14652361068081));
#53932=CARTESIAN_POINT('Ctrl Pts',(0.576469391676688,-1.,-4.151723761217));
#53933=CARTESIAN_POINT('Ctrl Pts',(0.579124568914235,-1.,-4.15561864788576));
#53934=CARTESIAN_POINT('Ctrl Pts',(0.580901211463535,-1.,-4.1582129171283));
#53935=CARTESIAN_POINT('Ctrl Pts',(0.581791163835815,-1.,-4.15950947128175));
#53936=CARTESIAN_POINT('',(0.73204283740062,-1.,-4.13571194405636));
#53937=CARTESIAN_POINT('',(0.581791163835815,-1.,-4.15950947128175));
#53938=CARTESIAN_POINT('',(0.786422660831985,-1.,-3.66661143271685));
#53939=CARTESIAN_POINT('Ctrl Pts',(0.73204283740062,-1.,-4.13571194405636));
#53940=CARTESIAN_POINT('Ctrl Pts',(0.732488575135159,-1.,-4.1342038373684));
#53941=CARTESIAN_POINT('Ctrl Pts',(0.733376589323546,-1.,-4.13118752795207));
#53942=CARTESIAN_POINT('Ctrl Pts',(0.734698226764092,-1.,-4.12666277570844));
#53943=CARTESIAN_POINT('Ctrl Pts',(0.736439634331344,-1.,-4.120629196238));
#53944=CARTESIAN_POINT('Ctrl Pts',(0.738581708225843,-1.,-4.11308626951927));
#53945=CARTESIAN_POINT('Ctrl Pts',(0.740688998553376,-1.,-4.10554241757547));
#53946=CARTESIAN_POINT('Ctrl Pts',(0.742761369689841,-1.,-4.09799769702611));
#53947=CARTESIAN_POINT('Ctrl Pts',(0.7447986497065,-1.,-4.09045220253573));
#53948=CARTESIAN_POINT('Ctrl Pts',(0.746800631492315,-1.,-4.08290608095642));
#53949=CARTESIAN_POINT('Ctrl Pts',(0.748767076680557,-1.,-4.07535951056152));
#53950=CARTESIAN_POINT('Ctrl Pts',(0.750697720484036,-1.,-4.06781267242378));
#53951=CARTESIAN_POINT('Ctrl Pts',(0.752592276483072,-1.,-4.06026572221515));
#53952=CARTESIAN_POINT('Ctrl Pts',(0.754450441816078,-1.,-4.05271876687915));
#53953=CARTESIAN_POINT('Ctrl Pts',(0.75627190236958,-1.,-4.04517182653997));
#53954=CARTESIAN_POINT('Ctrl Pts',(0.758056338884944,-1.,-4.03762485803119));
#53955=CARTESIAN_POINT('Ctrl Pts',(0.759803433243751,-1.,-4.03007781954412));
#53956=CARTESIAN_POINT('Ctrl Pts',(0.761512875859804,-1.,-4.02253072741268));
#53957=CARTESIAN_POINT('Ctrl Pts',(0.763184371182935,-1.,-4.01498370680496));
#53958=CARTESIAN_POINT('Ctrl Pts',(0.764817648785197,-1.,-4.00743706791509));
#53959=CARTESIAN_POINT('Ctrl Pts',(0.766412457136063,-1.,-3.99989129179622));
#53960=CARTESIAN_POINT('Ctrl Pts',(0.767968531377914,-1.,-3.9923468788101));
#53961=CARTESIAN_POINT('Ctrl Pts',(0.769485566245544,-1.,-3.98480422348451));
#53962=CARTESIAN_POINT('Ctrl Pts',(0.77096319003047,-1.,-3.97726349165488));
#53963=CARTESIAN_POINT('Ctrl Pts',(0.772400931772136,-1.,-3.96972446532772));
#53964=CARTESIAN_POINT('Ctrl Pts',(0.773798212026565,-1.,-3.96218649639807));
#53965=CARTESIAN_POINT('Ctrl Pts',(0.775154418039351,-1.,-3.9546488545231));
#53966=CARTESIAN_POINT('Ctrl Pts',(0.776468966697921,-1.,-3.94711101619447));
#53967=CARTESIAN_POINT('Ctrl Pts',(0.777741370568558,-1.,-3.93957296768103));
#53968=CARTESIAN_POINT('Ctrl Pts',(0.77897130813482,-1.,-3.93203552473174));
#53969=CARTESIAN_POINT('Ctrl Pts',(0.780158678615542,-1.,-3.92450058323823));
#53970=CARTESIAN_POINT('Ctrl Pts',(0.781303428618366,-1.,-3.91697036054676));
#53971=CARTESIAN_POINT('Ctrl Pts',(0.782405395622764,-1.,-3.90944671004542));
#53972=CARTESIAN_POINT('Ctrl Pts',(0.783464141529081,-1.,-3.9019303904397));
#53973=CARTESIAN_POINT('Ctrl Pts',(0.784478799358336,-1.,-3.89442039235103));
#53974=CARTESIAN_POINT('Ctrl Pts',(0.78544789034073,-1.,-3.88691313167398));
#53975=CARTESIAN_POINT('Ctrl Pts',(0.786369675812608,-1.,-3.8794040281819));
#53976=CARTESIAN_POINT('Ctrl Pts',(0.787242527617999,-1.,-3.87188916600912));
#53977=CARTESIAN_POINT('Ctrl Pts',(0.788065315093777,-1.,-3.86436702561345));
#53978=CARTESIAN_POINT('Ctrl Pts',(0.788837734090671,-1.,-3.85683995872529));
#53979=CARTESIAN_POINT('Ctrl Pts',(0.789560798155582,-1.,-3.84931637808894));
#53980=CARTESIAN_POINT('Ctrl Pts',(0.790236124191242,-1.,-3.84180762342454));
#53981=CARTESIAN_POINT('Ctrl Pts',(0.7908650127053,-1.,-3.83432392054786));
#53982=CARTESIAN_POINT('Ctrl Pts',(0.791447528662369,-1.,-3.82687033899792));
#53983=CARTESIAN_POINT('Ctrl Pts',(0.791981740718634,-1.,-3.81944345442249));
#53984=CARTESIAN_POINT('Ctrl Pts',(0.792462483517634,-1.,-3.81202588694756));
#53985=CARTESIAN_POINT('Ctrl Pts',(0.792882695234777,-1.,-3.80459229925637));
#53986=CARTESIAN_POINT('Ctrl Pts',(0.793235612973273,-1.,-3.79711921389897));
#53987=CARTESIAN_POINT('Ctrl Pts',(0.793516871680993,-1.,-3.78959439439235));
#53988=CARTESIAN_POINT('Ctrl Pts',(0.7937262357813,-1.,-3.78202460377598));
#53989=CARTESIAN_POINT('Ctrl Pts',(0.793870523787407,-1.,-3.77444863801212));
#53990=CARTESIAN_POINT('Ctrl Pts',(0.793961083688991,-1.,-3.76692626931111));
#53991=CARTESIAN_POINT('Ctrl Pts',(0.794008429134907,-1.,-3.75951468666257));
#53992=CARTESIAN_POINT('Ctrl Pts',(0.794017347371377,-1.,-3.75224692493864));
#53993=CARTESIAN_POINT('Ctrl Pts',(0.793982700459951,-1.,-3.74511357728861));
#53994=CARTESIAN_POINT('Ctrl Pts',(0.793882700937016,-1.,-3.73803280541687));
#53995=CARTESIAN_POINT('Ctrl Pts',(0.793682750269684,-1.,-3.73086914695805));
#53996=CARTESIAN_POINT('Ctrl Pts',(0.793347023784204,-1.,-3.72348797293734));
#53997=CARTESIAN_POINT('Ctrl Pts',(0.792848377370287,-1.,-3.71580242396124));
#53998=CARTESIAN_POINT('Ctrl Pts',(0.792177688845817,-1.,-3.70781724021806));
#53999=CARTESIAN_POINT('Ctrl Pts',(0.79135657569598,-1.,-3.69968940808721));
#54000=CARTESIAN_POINT('Ctrl Pts',(0.790436284988787,-1.,-3.69172044327364));
#54001=CARTESIAN_POINT('Ctrl Pts',(0.789483546064386,-1.,-3.68428439783905));
#54002=CARTESIAN_POINT('Ctrl Pts',(0.788569566220285,-1.,-3.67777119516252));
#54003=CARTESIAN_POINT('Ctrl Pts',(0.787758799995742,-1.,-3.67252923663655));
#54004=CARTESIAN_POINT('Ctrl Pts',(0.787145041181545,-1.,-3.66907505398677));
#54005=CARTESIAN_POINT('Ctrl Pts',(0.786774337198062,-1.,-3.66743103898702));
#54006=CARTESIAN_POINT('Ctrl Pts',(0.786565919558984,-1.,-3.66680946938292));
#54007=CARTESIAN_POINT('Ctrl Pts',(0.786459983895431,-1.,-3.6666431041522));
#54008=CARTESIAN_POINT('Ctrl Pts',(0.786422660831985,-1.,-3.66661143271685));
#54009=CARTESIAN_POINT('',(0.963899035117249,-1.,-3.62400312501245));
#54010=CARTESIAN_POINT('Origin',(0.,-1.,0.));
#54011=CARTESIAN_POINT('',(1.22531898815164,-1.,-4.01728681790024));
#54012=CARTESIAN_POINT('Ctrl Pts',(0.963899035117249,-1.,-3.62400312501245));
#54013=CARTESIAN_POINT('Ctrl Pts',(0.963880158555582,-1.,-3.6240482887845));
#54014=CARTESIAN_POINT('Ctrl Pts',(0.963861297423241,-1.,-3.62424461507588));
#54015=CARTESIAN_POINT('Ctrl Pts',(0.963957782642843,-1.,-3.62489305727662));
#54016=CARTESIAN_POINT('Ctrl Pts',(0.964373850166457,-1.,-3.62652618145335));
#54017=CARTESIAN_POINT('Ctrl Pts',(0.965395153165293,-1.,-3.62988252139846));
#54018=CARTESIAN_POINT('Ctrl Pts',(0.967052554541385,-1.,-3.63492122081143));
#54019=CARTESIAN_POINT('Ctrl Pts',(0.969195124675865,-1.,-3.64113946505766));
#54020=CARTESIAN_POINT('Ctrl Pts',(0.971722122061341,-1.,-3.64819756447455));
#54021=CARTESIAN_POINT('Ctrl Pts',(0.974519971354848,-1.,-3.65571576735126));
#54022=CARTESIAN_POINT('Ctrl Pts',(0.977478312751618,-1.,-3.66333049637475));
#54023=CARTESIAN_POINT('Ctrl Pts',(0.980505922458267,-1.,-3.67074983340361));
#54024=CARTESIAN_POINT('Ctrl Pts',(0.983550791470419,-1.,-3.67782408841715));
#54025=CARTESIAN_POINT('Ctrl Pts',(0.986602639863837,-1.,-3.68455317926068));
#54026=CARTESIAN_POINT('Ctrl Pts',(0.989676715398558,-1.,-3.69102682138847));
#54027=CARTESIAN_POINT('Ctrl Pts',(0.99280221833201,-1.,-3.69738123415662));
#54028=CARTESIAN_POINT('Ctrl Pts',(0.996009819772518,-1.,-3.70375282282138));
#54029=CARTESIAN_POINT('Ctrl Pts',(0.99931726075653,-1.,-3.71022439713938));
#54030=CARTESIAN_POINT('Ctrl Pts',(1.00272423396822,-1.,-3.71680667125119));
#54031=CARTESIAN_POINT('Ctrl Pts',(1.0062200073571,-1.,-3.72346803750596));
#54032=CARTESIAN_POINT('Ctrl Pts',(1.00978798539496,-1.,-3.73015276704426));
#54033=CARTESIAN_POINT('Ctrl Pts',(1.01341114319903,-1.,-3.73680245055734));
#54034=CARTESIAN_POINT('Ctrl Pts',(1.01707794311079,-1.,-3.74337942504959));
#54035=CARTESIAN_POINT('Ctrl Pts',(1.02078510487428,-1.,-3.74987777155834));
#54036=CARTESIAN_POINT('Ctrl Pts',(1.0245342944466,-1.,-3.75631037456194));
#54037=CARTESIAN_POINT('Ctrl Pts',(1.02833014458181,-1.,-3.76270122291232));
#54038=CARTESIAN_POINT('Ctrl Pts',(1.0321778660492,-1.,-3.76907609832522));
#54039=CARTESIAN_POINT('Ctrl Pts',(1.03608074678013,-1.,-3.77545283140445));
#54040=CARTESIAN_POINT('Ctrl Pts',(1.04003862055804,-1.,-3.78183535008192));
#54041=CARTESIAN_POINT('Ctrl Pts',(1.04404924374426,-1.,-3.78821910787195));
#54042=CARTESIAN_POINT('Ctrl Pts',(1.04810913267641,-1.,-3.79459440308793));
#54043=CARTESIAN_POINT('Ctrl Pts',(1.05221457990015,-1.,-3.80095039790678));
#54044=CARTESIAN_POINT('Ctrl Pts',(1.05636266918643,-1.,-3.80727913637784));
#54045=CARTESIAN_POINT('Ctrl Pts',(1.06055206187298,-1.,-3.81357866117485));
#54046=CARTESIAN_POINT('Ctrl Pts',(1.06478244038931,-1.,-3.81985083953012));
#54047=CARTESIAN_POINT('Ctrl Pts',(1.0690541318036,-1.,-3.82609989967278));
#54048=CARTESIAN_POINT('Ctrl Pts',(1.0733676663346,-1.,-3.83233071195145));
#54049=CARTESIAN_POINT('Ctrl Pts',(1.07772335353856,-1.,-3.83854714117486));
#54050=CARTESIAN_POINT('Ctrl Pts',(1.08212087917986,-1.,-3.84475048030615));
#54051=CARTESIAN_POINT('Ctrl Pts',(1.08655950846377,-1.,-3.85094025222691));
#54052=CARTESIAN_POINT('Ctrl Pts',(1.09103825516288,-1.,-3.85711487933911));
#54053=CARTESIAN_POINT('Ctrl Pts',(1.09555606505012,-1.,-3.86327241021242));
#54054=CARTESIAN_POINT('Ctrl Pts',(1.10011198761202,-1.,-3.86941120134872));
#54055=CARTESIAN_POINT('Ctrl Pts',(1.10470536603303,-1.,-3.87553067187566));
#54056=CARTESIAN_POINT('Ctrl Pts',(1.10933577224029,-1.,-3.88163105531791));
#54057=CARTESIAN_POINT('Ctrl Pts',(1.11400292434447,-1.,-3.88771308285229));
#54058=CARTESIAN_POINT('Ctrl Pts',(1.11870660794609,-1.,-3.89377768340362));
#54059=CARTESIAN_POINT('Ctrl Pts',(1.12344660099029,-1.,-3.89982569749978));
#54060=CARTESIAN_POINT('Ctrl Pts',(1.12822258281518,-1.,-3.90585753318622));
#54061=CARTESIAN_POINT('Ctrl Pts',(1.13303414693849,-1.,-3.91187321145495));
#54062=CARTESIAN_POINT('Ctrl Pts',(1.13788084225511,-1.,-3.91787251936688));
#54063=CARTESIAN_POINT('Ctrl Pts',(1.14276220561575,-1.,-3.92385513133937));
#54064=CARTESIAN_POINT('Ctrl Pts',(1.14767779451147,-1.,-3.92982073294334));
#54065=CARTESIAN_POINT('Ctrl Pts',(1.1526272271639,-1.,-3.9357691705651));
#54066=CARTESIAN_POINT('Ctrl Pts',(1.1576101834106,-1.,-3.94170046685542));
#54067=CARTESIAN_POINT('Ctrl Pts',(1.16262637999261,-1.,-3.9476147478092));
#54068=CARTESIAN_POINT('Ctrl Pts',(1.16767555244495,-1.,-3.95351219510062));
#54069=CARTESIAN_POINT('Ctrl Pts',(1.17275743590327,-1.,-3.95939299213164));
#54070=CARTESIAN_POINT('Ctrl Pts',(1.17787174135445,-1.,-3.96525726357682));
#54071=CARTESIAN_POINT('Ctrl Pts',(1.18301815039596,-1.,-3.9711050516465));
#54072=CARTESIAN_POINT('Ctrl Pts',(1.18819633715285,-1.,-3.97693634766926));
#54073=CARTESIAN_POINT('Ctrl Pts',(1.19340598349307,-1.,-3.98275111052015));
#54074=CARTESIAN_POINT('Ctrl Pts',(1.19864679609596,-1.,-3.98854928957287));
#54075=CARTESIAN_POINT('Ctrl Pts',(1.2039185237544,-1.,-3.99433084800649));
#54076=CARTESIAN_POINT('Ctrl Pts',(1.20922097030107,-1.,-4.00009577952534));
#54077=CARTESIAN_POINT('Ctrl Pts',(1.21455398918813,-1.,-4.00584409524937));
#54078=CARTESIAN_POINT('Ctrl Pts',(1.21884478244983,-1.,-4.01042947142681));
#54079=CARTESIAN_POINT('Ctrl Pts',(1.22207656456199,-1.,-4.01386104434674));
#54080=CARTESIAN_POINT('Ctrl Pts',(1.22423716681447,-1.,-4.0161454457032));
#54081=CARTESIAN_POINT('Ctrl Pts',(1.22531898815164,-1.,-4.01728681790024));
#54082=CARTESIAN_POINT('',(1.36999806084572,-1.,-3.97027773754922));
#54083=CARTESIAN_POINT('',(1.22531898815164,-1.,-4.01728681790024));
#54084=CARTESIAN_POINT('',(1.35032489087101,-1.,-3.4984457533445));
#54085=CARTESIAN_POINT('Ctrl Pts',(1.36999806084572,-1.,-3.97027773754922));
#54086=CARTESIAN_POINT('Ctrl Pts',(1.37020239094614,-1.,-3.9687184694131));
#54087=CARTESIAN_POINT('Ctrl Pts',(1.37060761745635,-1.,-3.96560037974645));
#54088=CARTESIAN_POINT('Ctrl Pts',(1.3712051561502,-1.,-3.96092458506535));
#54089=CARTESIAN_POINT('Ctrl Pts',(1.37198126432386,-1.,-3.95469287280914));
#54090=CARTESIAN_POINT('Ctrl Pts',(1.37291699202807,-1.,-3.94690771785133));
#54091=CARTESIAN_POINT('Ctrl Pts',(1.37381821967165,-1.,-3.93912709040818));
#54092=CARTESIAN_POINT('Ctrl Pts',(1.37468482215751,-1.,-3.93135106761844));
#54093=CARTESIAN_POINT('Ctrl Pts',(1.37551664448242,-1.,-3.92357976987672));
#54094=CARTESIAN_POINT('Ctrl Pts',(1.37631350505797,-1.,-3.91581337462644));
#54095=CARTESIAN_POINT('Ctrl Pts',(1.3770751963402,-1.,-3.90805209523486));
#54096=CARTESIAN_POINT('Ctrl Pts',(1.37780148512792,-1.,-3.90029615196727));
#54097=CARTESIAN_POINT('Ctrl Pts',(1.3784921128802,-1.,-3.89254574338496));
#54098=CARTESIAN_POINT('Ctrl Pts',(1.37914679719383,-1.,-3.88480102249278));
#54099=CARTESIAN_POINT('Ctrl Pts',(1.37976523097073,-1.,-3.87706205830532));
#54100=CARTESIAN_POINT('Ctrl Pts',(1.38034709213014,-1.,-3.86932885813068));
#54101=CARTESIAN_POINT('Ctrl Pts',(1.38089205992989,-1.,-3.86160143043959));
#54102=CARTESIAN_POINT('Ctrl Pts',(1.38139983115049,-1.,-3.85387983979481));
#54103=CARTESIAN_POINT('Ctrl Pts',(1.38187013346109,-1.,-3.84616425605764));
#54104=CARTESIAN_POINT('Ctrl Pts',(1.38230274828821,-1.,-3.83845502790746));
#54105=CARTESIAN_POINT('Ctrl Pts',(1.38269750245138,-1.,-3.8307526698229));
#54106=CARTESIAN_POINT('Ctrl Pts',(1.38305421262763,-1.,-3.82305771743829));
#54107=CARTESIAN_POINT('Ctrl Pts',(1.38337263902782,-1.,-3.81537060817811));
#54108=CARTESIAN_POINT('Ctrl Pts',(1.3836524404622,-1.,-3.80769156398411));
#54109=CARTESIAN_POINT('Ctrl Pts',(1.38389311766682,-1.,-3.80002044322111));
#54110=CARTESIAN_POINT('Ctrl Pts',(1.38409399694566,-1.,-3.79235669640841));
#54111=CARTESIAN_POINT('Ctrl Pts',(1.38425435883756,-1.,-3.78469969805082));
#54112=CARTESIAN_POINT('Ctrl Pts',(1.38437354551428,-1.,-3.77704902230418));
#54113=CARTESIAN_POINT('Ctrl Pts',(1.38445107339518,-1.,-3.76940473185779));
#54114=CARTESIAN_POINT('Ctrl Pts',(1.3844867525335,-1.,-3.76176768271367));
#54115=CARTESIAN_POINT('Ctrl Pts',(1.38448077997163,-1.,-3.7541397631875));
#54116=CARTESIAN_POINT('Ctrl Pts',(1.38443344984394,-1.,-3.74652317167876));
#54117=CARTESIAN_POINT('Ctrl Pts',(1.38434489156458,-1.,-3.73891976418104));
#54118=CARTESIAN_POINT('Ctrl Pts',(1.38421479111531,-1.,-3.73133035859282));
#54119=CARTESIAN_POINT('Ctrl Pts',(1.3840421342895,-1.,-3.72375409358803));
#54120=CARTESIAN_POINT('Ctrl Pts',(1.38382489984586,-1.,-3.7161876605181));
#54121=CARTESIAN_POINT('Ctrl Pts',(1.38356065402124,-1.,-3.70862680753347));
#54122=CARTESIAN_POINT('Ctrl Pts',(1.38324717612865,-1.,-3.701067921679));
#54123=CARTESIAN_POINT('Ctrl Pts',(1.3828831117165,-1.,-3.69350967899526));
#54124=CARTESIAN_POINT('Ctrl Pts',(1.38246852827182,-1.,-3.68595444983838));
#54125=CARTESIAN_POINT('Ctrl Pts',(1.3820057429062,-1.,-3.67841038482414));
#54126=CARTESIAN_POINT('Ctrl Pts',(1.38149812653868,-1.,-3.67088843112262));
#54127=CARTESIAN_POINT('Ctrl Pts',(1.38094856333552,-1.,-3.66339848520857));
#54128=CARTESIAN_POINT('Ctrl Pts',(1.38035791051212,-1.,-3.6559455440439));
#54129=CARTESIAN_POINT('Ctrl Pts',(1.37972372481603,-1.,-3.64852652756456));
#54130=CARTESIAN_POINT('Ctrl Pts',(1.37903818567359,-1.,-3.64112507791141));
#54131=CARTESIAN_POINT('Ctrl Pts',(1.37829035457339,-1.,-3.63371727442486));
#54132=CARTESIAN_POINT('Ctrl Pts',(1.37746987919881,-1.,-3.62628098665145));
#54133=CARTESIAN_POINT('Ctrl Pts',(1.37657053403107,-1.,-3.61880481160421));
#54134=CARTESIAN_POINT('Ctrl Pts',(1.37559314436634,-1.,-3.61129546591064));
#54135=CARTESIAN_POINT('Ctrl Pts',(1.37455051379623,-1.,-3.60379020123988));
#54136=CARTESIAN_POINT('Ctrl Pts',(1.37346320103157,-1.,-3.59634627869048));
#54137=CARTESIAN_POINT('Ctrl Pts',(1.37235053660976,-1.,-3.58901853846365));
#54138=CARTESIAN_POINT('Ctrl Pts',(1.37122241663062,-1.,-3.58183885982715));
#54139=CARTESIAN_POINT('Ctrl Pts',(1.37007229485659,-1.,-3.57479875549486));
#54140=CARTESIAN_POINT('Ctrl Pts',(1.36886584973389,-1.,-3.5678208030466));
#54141=CARTESIAN_POINT('Ctrl Pts',(1.36754771771233,-1.,-3.56077662028649));
#54142=CARTESIAN_POINT('Ctrl Pts',(1.3660614545677,-1.,-3.55353883995949));
#54143=CARTESIAN_POINT('Ctrl Pts',(1.36436666257597,-1.,-3.54602591832973));
#54144=CARTESIAN_POINT('Ctrl Pts',(1.36245507339307,-1.,-3.53824396424961));
#54145=CARTESIAN_POINT('Ctrl Pts',(1.36037259643734,-1.,-3.530344649616));
#54146=CARTESIAN_POINT('Ctrl Pts',(1.35821701528836,-1.,-3.52261776116748));
#54147=CARTESIAN_POINT('Ctrl Pts',(1.35611275237152,-1.,-3.51542230699556));
#54148=CARTESIAN_POINT('Ctrl Pts',(1.35419113575956,-1.,-3.50913227059999));
#54149=CARTESIAN_POINT('Ctrl Pts',(1.35257032843486,-1.,-3.50408168106261));
#54150=CARTESIAN_POINT('Ctrl Pts',(1.35142377279517,-1.,-3.5007660381649));
#54151=CARTESIAN_POINT('Ctrl Pts',(1.35080045218586,-1.,-3.49920025459723));
#54152=CARTESIAN_POINT('Ctrl Pts',(1.35049736560527,-1.,-3.49861894124827));
#54153=CARTESIAN_POINT('Ctrl Pts',(1.35036670892966,-1.,-3.49847119623846));
#54154=CARTESIAN_POINT('Ctrl Pts',(1.35032489087101,-1.,-3.4984457533445));
#54155=CARTESIAN_POINT('',(1.51895082866166,-1.,-3.42859860294378));
#54156=CARTESIAN_POINT('Origin',(0.,-1.,0.));
#54157=CARTESIAN_POINT('',(1.83867539237861,-1.,-3.77614523045147));
#54158=CARTESIAN_POINT('Ctrl Pts',(1.51895082866166,-1.,-3.42859860294378));
#54159=CARTESIAN_POINT('Ctrl Pts',(1.51893924967231,-1.,-3.42864616361967));
#54160=CARTESIAN_POINT('Ctrl Pts',(1.51895133295017,-1.,-3.42884302333978));
#54161=CARTESIAN_POINT('Ctrl Pts',(1.51914806898539,-1.,-3.42946838852728));
#54162=CARTESIAN_POINT('Ctrl Pts',(1.5198144909343,-1.,-3.43101631893491));
#54163=CARTESIAN_POINT('Ctrl Pts',(1.52134826724227,-1.,-3.43417156977749));
#54164=CARTESIAN_POINT('Ctrl Pts',(1.52377348950429,-1.,-3.43888895974182));
#54165=CARTESIAN_POINT('Ctrl Pts',(1.52686242875717,-1.,-3.44469547527));
#54166=CARTESIAN_POINT('Ctrl Pts',(1.530462444618,-1.,-3.45127136828667));
#54167=CARTESIAN_POINT('Ctrl Pts',(1.53440195378902,-1.,-3.45825932955273));
#54168=CARTESIAN_POINT('Ctrl Pts',(1.53851507915533,-1.,-3.46531752207222));
#54169=CARTESIAN_POINT('Ctrl Pts',(1.54266605398152,-1.,-3.47217189224576));
#54170=CARTESIAN_POINT('Ctrl Pts',(1.54678009290206,-1.,-3.47868272898599));
#54171=CARTESIAN_POINT('Ctrl Pts',(1.55084702970382,-1.,-3.48485155928414));
#54172=CARTESIAN_POINT('Ctrl Pts',(1.5548959590107,-1.,-3.49076460877317));
#54173=CARTESIAN_POINT('Ctrl Pts',(1.55897703097859,-1.,-3.49655185179623));
#54174=CARTESIAN_POINT('Ctrl Pts',(1.56314187758689,-1.,-3.50234321621607));
#54175=CARTESIAN_POINT('Ctrl Pts',(1.56742097575041,-1.,-3.50821771695427));
#54176=CARTESIAN_POINT('Ctrl Pts',(1.57181569799774,-1.,-3.51418598431733));
#54177=CARTESIAN_POINT('Ctrl Pts',(1.5763104998818,-1.,-3.52021847865961));
#54178=CARTESIAN_POINT('Ctrl Pts',(1.58088027227856,-1.,-3.52626275334899));
#54179=CARTESIAN_POINT('Ctrl Pts',(1.58549906268083,-1.,-3.53226378147068));
#54180=CARTESIAN_POINT('Ctrl Pts',(1.59014958368725,-1.,-3.53818616861045));
#54181=CARTESIAN_POINT('Ctrl Pts',(1.5948276694975,-1.,-3.544024581823));
#54182=CARTESIAN_POINT('Ctrl Pts',(1.59953698113444,-1.,-3.54979148634426));
#54183=CARTESIAN_POINT('Ctrl Pts',(1.60428584699848,-1.,-3.55550985096117));
#54184=CARTESIAN_POINT('Ctrl Pts',(1.60908344685459,-1.,-3.56120432482986));
#54185=CARTESIAN_POINT('Ctrl Pts',(1.61393581747522,-1.,-3.56689200468404));
#54186=CARTESIAN_POINT('Ctrl Pts',(1.61884340915412,-1.,-3.57257679609826));
#54187=CARTESIAN_POINT('Ctrl Pts',(1.62380329464851,-1.,-3.57825455954405));
#54188=CARTESIAN_POINT('Ctrl Pts',(1.62881051550748,-1.,-3.5839162577435));
#54189=CARTESIAN_POINT('Ctrl Pts',(1.63385971451259,-1.,-3.58955176627876));
#54190=CARTESIAN_POINT('Ctrl Pts',(1.63894676675349,-1.,-3.59515368334887));
#54191=CARTESIAN_POINT('Ctrl Pts',(1.6440700438558,-1.,-3.6007202851384));
#54192=CARTESIAN_POINT('Ctrl Pts',(1.64922952425833,-1.,-3.60625346556992));
#54193=CARTESIAN_POINT('Ctrl Pts',(1.65442619244327,-1.,-3.61175734965129));
#54194=CARTESIAN_POINT('Ctrl Pts',(1.65966133399186,-1.,-3.61723666482457));
#54195=CARTESIAN_POINT('Ctrl Pts',(1.66493585923853,-1.,-3.62269517989104));
#54196=CARTESIAN_POINT('Ctrl Pts',(1.67024966008037,-1.,-3.62813422105257));
#54197=CARTESIAN_POINT('Ctrl Pts',(1.67560193613145,-1.,-3.63355343201211));
#54198=CARTESIAN_POINT('Ctrl Pts',(1.68099146651577,-1.,-3.63895140887443));
#54199=CARTESIAN_POINT('Ctrl Pts',(1.68641690471455,-1.,-3.64432638915199));
#54200=CARTESIAN_POINT('Ctrl Pts',(1.691877054817,-1.,-3.64967689827393));
#54201=CARTESIAN_POINT('Ctrl Pts',(1.69737117722558,-1.,-3.65500246526798));
#54202=CARTESIAN_POINT('Ctrl Pts',(1.70289888566904,-1.,-3.6603033877491));
#54203=CARTESIAN_POINT('Ctrl Pts',(1.70846001610983,-1.,-3.6655804319893));
#54204=CARTESIAN_POINT('Ctrl Pts',(1.71405450210392,-1.,-3.67083454901629));
#54205=CARTESIAN_POINT('Ctrl Pts',(1.71968225581787,-1.,-3.67606660374665));
#54206=CARTESIAN_POINT('Ctrl Pts',(1.72534302437003,-1.,-3.68127704936472));
#54207=CARTESIAN_POINT('Ctrl Pts',(1.73103640956647,-1.,-3.68646597019188));
#54208=CARTESIAN_POINT('Ctrl Pts',(1.73676193254493,-1.,-3.69163322647906));
#54209=CARTESIAN_POINT('Ctrl Pts',(1.74251908492589,-1.,-3.6967785691046));
#54210=CARTESIAN_POINT('Ctrl Pts',(1.74830738046092,-1.,-3.70190175673422));
#54211=CARTESIAN_POINT('Ctrl Pts',(1.75412641804148,-1.,-3.70700269736876));
#54212=CARTESIAN_POINT('Ctrl Pts',(1.75997588499021,-1.,-3.71208146346455));
#54213=CARTESIAN_POINT('Ctrl Pts',(1.76585552124549,-1.,-3.71713822377676));
#54214=CARTESIAN_POINT('Ctrl Pts',(1.77176509401846,-1.,-3.72217319911429));
#54215=CARTESIAN_POINT('Ctrl Pts',(1.77770437039606,-1.,-3.72718661205504));
#54216=CARTESIAN_POINT('Ctrl Pts',(1.78367308442682,-1.,-3.73217863095022));
#54217=CARTESIAN_POINT('Ctrl Pts',(1.78967092823139,-1.,-3.73714934729962));
#54218=CARTESIAN_POINT('Ctrl Pts',(1.79569757859041,-1.,-3.74209880351667));
#54219=CARTESIAN_POINT('Ctrl Pts',(1.80175271485519,-1.,-3.74702700874954));
#54220=CARTESIAN_POINT('Ctrl Pts',(1.80783603939662,-1.,-3.75193395888069));
#54221=CARTESIAN_POINT('Ctrl Pts',(1.81394729834032,-1.,-3.75681965683995));
#54222=CARTESIAN_POINT('Ctrl Pts',(1.82008629694924,-1.,-3.76168412709652));
#54223=CARTESIAN_POINT('Ctrl Pts',(1.82625289221933,-1.,-3.76652740355856));
#54224=CARTESIAN_POINT('Ctrl Pts',(1.83120816956515,-1.,-3.77038509819777));
#54225=CARTESIAN_POINT('Ctrl Pts',(1.83493697935064,-1.,-3.77326886065484));
#54226=CARTESIAN_POINT('Ctrl Pts',(1.83742834010821,-1.,-3.77518714458232));
#54227=CARTESIAN_POINT('Ctrl Pts',(1.83867539237861,-1.,-3.77614523045147));
#54228=CARTESIAN_POINT('',(1.97421938526992,-1.,-3.70708211654725));
#54229=CARTESIAN_POINT('',(1.83867539237861,-1.,-3.77614523045147));
#54230=CARTESIAN_POINT('',(1.88097764062541,-1.,-3.24413672884902));
#54231=CARTESIAN_POINT('Ctrl Pts',(1.97421938526992,-1.,-3.70708211654725));
#54232=CARTESIAN_POINT('Ctrl Pts',(1.974177276451,-1.,-3.7055100813194));
#54233=CARTESIAN_POINT('Ctrl Pts',(1.97408973726149,-1.,-3.70236698911837));
#54234=CARTESIAN_POINT('Ctrl Pts',(1.97394846382288,-1.,-3.69765528558292));
#54235=CARTESIAN_POINT('Ctrl Pts',(1.97374016224397,-1.,-3.69137888597855));
#54236=CARTESIAN_POINT('Ctrl Pts',(1.9734465030363,-1.,-3.68354319913416));
#54237=CARTESIAN_POINT('Ctrl Pts',(1.97311947678035,-1.,-3.67571738106175));
#54238=CARTESIAN_POINT('Ctrl Pts',(1.9727589719863,-1.,-3.66790152751984));
#54239=CARTESIAN_POINT('Ctrl Pts',(1.97236485439317,-1.,-3.66009578166865));
#54240=CARTESIAN_POINT('Ctrl Pts',(1.97193697240645,-1.,-3.65230034717364));
#54241=CARTESIAN_POINT('Ctrl Pts',(1.97147515441539,-1.,-3.64451546724222));
#54242=CARTESIAN_POINT('Ctrl Pts',(1.97097920454698,-1.,-3.63674139590853));
#54243=CARTESIAN_POINT('Ctrl Pts',(1.97044889850518,-1.,-3.62897836973397));
#54244=CARTESIAN_POINT('Ctrl Pts',(1.96988398129888,-1.,-3.62122658401722));
#54245=CARTESIAN_POINT('Ctrl Pts',(1.96928416040712,-1.,-3.61348615496393));
#54246=CARTESIAN_POINT('Ctrl Pts',(1.96864911885775,-1.,-3.60575714017676));
#54247=CARTESIAN_POINT('Ctrl Pts',(1.96797854118257,-1.,-3.59803959819725));
#54248=CARTESIAN_POINT('Ctrl Pts',(1.96727213799507,-1.,-3.5903336402273));
#54249=CARTESIAN_POINT('Ctrl Pts',(1.9665296668894,-1.,-3.58263947663884));
#54250=CARTESIAN_POINT('Ctrl Pts',(1.96575096652857,-1.,-3.57495748601088));
#54251=CARTESIAN_POINT('Ctrl Pts',(1.96493594634643,-1.,-3.56728820357933));
#54252=CARTESIAN_POINT('Ctrl Pts',(1.96408450906868,-1.,-3.55963218706201));
#54253=CARTESIAN_POINT('Ctrl Pts',(1.96319648628667,-1.,-3.55198990600929));
#54254=CARTESIAN_POINT('Ctrl Pts',(1.96227157573058,-1.,-3.54436163300425));
#54255=CARTESIAN_POINT('Ctrl Pts',(1.96130926212661,-1.,-3.53674730625759));
#54256=CARTESIAN_POINT('Ctrl Pts',(1.96030879411534,-1.,-3.52914648844289));
#54257=CARTESIAN_POINT('Ctrl Pts',(1.95926936324436,-1.,-3.52155867431438));
#54258=CARTESIAN_POINT('Ctrl Pts',(1.95819025316768,-1.,-3.51398354617773));
#54259=CARTESIAN_POINT('Ctrl Pts',(1.95707099606513,-1.,-3.50642124159913));
#54260=CARTESIAN_POINT('Ctrl Pts',(1.9559115382367,-1.,-3.49887263575602));
#54261=CARTESIAN_POINT('Ctrl Pts',(1.95471236969653,-1.,-3.49133956289154));
#54262=CARTESIAN_POINT('Ctrl Pts',(1.95347412486316,-1.,-3.48382414832649));
#54263=CARTESIAN_POINT('Ctrl Pts',(1.95219722189878,-1.,-3.47632820495926));
#54264=CARTESIAN_POINT('Ctrl Pts',(1.95088147859876,-1.,-3.4688525897419));
#54265=CARTESIAN_POINT('Ctrl Pts',(1.94952575850196,-1.,-3.46139661060959));
#54266=CARTESIAN_POINT('Ctrl Pts',(1.94812754766524,-1.,-3.45395731584051));
#54267=CARTESIAN_POINT('Ctrl Pts',(1.94668377715332,-1.,-3.44653088665685));
#54268=CARTESIAN_POINT('Ctrl Pts',(1.94519168842883,-1.,-3.43911410197693));
#54269=CARTESIAN_POINT('Ctrl Pts',(1.94364973660285,-1.,-3.43170586602436));
#54270=CARTESIAN_POINT('Ctrl Pts',(1.94205835913692,-1.,-3.42430850941497));
#54271=CARTESIAN_POINT('Ctrl Pts',(1.94042111965237,-1.,-3.41692971994082));
#54272=CARTESIAN_POINT('Ctrl Pts',(1.93874306008132,-1.,-3.40957978266623));
#54273=CARTESIAN_POINT('Ctrl Pts',(1.93702857723089,-1.,-3.40226802104093));
#54274=CARTESIAN_POINT('Ctrl Pts',(1.93527929945982,-1.,-3.39499923640789));
#54275=CARTESIAN_POINT('Ctrl Pts',(1.93349233176794,-1.,-3.38777076883267));
#54276=CARTESIAN_POINT('Ctrl Pts',(1.93165739093292,-1.,-3.38056768525577));
#54277=CARTESIAN_POINT('Ctrl Pts',(1.92975993109897,-1.,-3.37336807068078));
#54278=CARTESIAN_POINT('Ctrl Pts',(1.92778626543803,-1.,-3.36615168657597));
#54279=CARTESIAN_POINT('Ctrl Pts',(1.92572846125763,-1.,-3.35890824422976));
#54280=CARTESIAN_POINT('Ctrl Pts',(1.92358838440518,-1.,-3.35164424847207));
#54281=CARTESIAN_POINT('Ctrl Pts',(1.92138450828378,-1.,-3.34439448941915));
#54282=CARTESIAN_POINT('Ctrl Pts',(1.91914609610173,-1.,-3.33721230709948));
#54283=CARTESIAN_POINT('Ctrl Pts',(1.91690081930297,-1.,-3.33014884257812));
#54284=CARTESIAN_POINT('Ctrl Pts',(1.91466343916612,-1.,-3.32323403454507));
#54285=CARTESIAN_POINT('Ctrl Pts',(1.91242616234459,-1.,-3.31646052426395));
#54286=CARTESIAN_POINT('Ctrl Pts',(1.91014297830502,-1.,-3.30975721158694));
#54287=CARTESIAN_POINT('Ctrl Pts',(1.90773912171424,-1.,-3.30300595568341));
#54288=CARTESIAN_POINT('Ctrl Pts',(1.9051389186417,-1.,-3.29608978722258));
#54289=CARTESIAN_POINT('Ctrl Pts',(1.9022897124757,-1.,-3.28893448600364));
#54290=CARTESIAN_POINT('Ctrl Pts',(1.89918429230424,-1.,-3.28154737912287));
#54291=CARTESIAN_POINT('Ctrl Pts',(1.89589172903662,-1.,-3.27407108932908));
#54292=CARTESIAN_POINT('Ctrl Pts',(1.89255393500769,-1.,-3.2667765388833));
#54293=CARTESIAN_POINT('Ctrl Pts',(1.88934996203508,-1.,-3.2599988519361));
#54294=CARTESIAN_POINT('Ctrl Pts',(1.88646802523372,-1.,-3.25408686339298));
#54295=CARTESIAN_POINT('Ctrl Pts',(1.88407708646435,-1.,-3.24935200512055));
#54296=CARTESIAN_POINT('Ctrl Pts',(1.88242596600422,-1.,-3.24625654410705));
#54297=CARTESIAN_POINT('Ctrl Pts',(1.88156537699118,-1.,-3.24480754675942));
#54298=CARTESIAN_POINT('Ctrl Pts',(1.88117508446657,-1.,-3.24428080352952));
#54299=CARTESIAN_POINT('Ctrl Pts',(1.88102292397987,-1.,-3.24415531671311));
#54300=CARTESIAN_POINT('Ctrl Pts',(1.88097764062541,-1.,-3.24413672884902));
#54301=CARTESIAN_POINT('',(2.03660101169564,-1.,-3.14877060440425));
#54302=CARTESIAN_POINT('Origin',(0.,-1.,0.));
#54303=CARTESIAN_POINT('',(2.40675750623143,-1.,-3.44202241512147));
#54304=CARTESIAN_POINT('Ctrl Pts',(2.03660101169564,-1.,-3.14877060440425));
#54305=CARTESIAN_POINT('Ctrl Pts',(2.03659701539175,-1.,-3.1488193908823));
#54306=CARTESIAN_POINT('Ctrl Pts',(2.03663974554941,-1.,-3.14901193669147));
#54307=CARTESIAN_POINT('Ctrl Pts',(2.03693188810614,-1.,-3.14959882629936));
#54308=CARTESIAN_POINT('Ctrl Pts',(2.03783225496023,-1.,-3.15102344775396));
#54309=CARTESIAN_POINT('Ctrl Pts',(2.03984073791432,-1.,-3.1538999167466));
#54310=CARTESIAN_POINT('Ctrl Pts',(2.04297406404132,-1.,-3.15817983946525));
#54311=CARTESIAN_POINT('Ctrl Pts',(2.0469333124766,-1.,-3.16343165059235));
#54312=CARTESIAN_POINT('Ctrl Pts',(2.05151770247452,-1.,-3.16936341689859));
#54313=CARTESIAN_POINT('Ctrl Pts',(2.05650186773279,-1.,-3.17564906975592));
#54314=CARTESIAN_POINT('Ctrl Pts',(2.06166849827143,-1.,-3.18197692964677));
#54315=CARTESIAN_POINT('Ctrl Pts',(2.06684062744065,-1.,-3.18809755562297));
#54316=CARTESIAN_POINT('Ctrl Pts',(2.07192253497765,-1.,-3.19388465568113));
#54317=CARTESIAN_POINT('Ctrl Pts',(2.0769044187063,-1.,-3.19934132835879));
#54318=CARTESIAN_POINT('Ctrl Pts',(2.08182850370816,-1.,-3.20454818630635));
#54319=CARTESIAN_POINT('Ctrl Pts',(2.08676465517435,-1.,-3.20962575845433));
#54320=CARTESIAN_POINT('Ctrl Pts',(2.0917841946046,-1.,-3.2146942960168));
#54321=CARTESIAN_POINT('Ctrl Pts',(2.09692958434933,-1.,-3.21982707347067));
#54322=CARTESIAN_POINT('Ctrl Pts',(2.10220384298533,-1.,-3.22503437553496));
#54323=CARTESIAN_POINT('Ctrl Pts',(2.1075869964248,-1.,-3.23028945793334));
#54324=CARTESIAN_POINT('Ctrl Pts',(2.11304604021784,-1.,-3.23554444767115));
#54325=CARTESIAN_POINT('Ctrl Pts',(2.11854673326972,-1.,-3.24074905517282));
#54326=CARTESIAN_POINT('Ctrl Pts',(2.12406646410943,-1.,-3.24587102613347));
#54327=CARTESIAN_POINT('Ctrl Pts',(2.1296002839681,-1.,-3.25090574493994));
#54328=CARTESIAN_POINT('Ctrl Pts',(2.13515375878786,-1.,-3.25586495065027));
#54329=CARTESIAN_POINT('Ctrl Pts',(2.14073870754257,-1.,-3.26077002641868));
#54330=CARTESIAN_POINT('Ctrl Pts',(2.14636805295663,-1.,-3.26564388189764));
#54331=CARTESIAN_POINT('Ctrl Pts',(2.15205043199818,-1.,-3.27050245897244));
#54332=CARTESIAN_POINT('Ctrl Pts',(2.15778690038359,-1.,-3.27534954469206));
#54333=CARTESIAN_POINT('Ctrl Pts',(2.16357391934434,-1.,-3.28018150841414));
#54334=CARTESIAN_POINT('Ctrl Pts',(2.16940517773459,-1.,-3.2849901997973));
#54335=CARTESIAN_POINT('Ctrl Pts',(2.17527380048422,-1.,-3.28976645712566));
#54336=CARTESIAN_POINT('Ctrl Pts',(2.18117455557062,-1.,-3.29450361500484));
#54337=CARTESIAN_POINT('Ctrl Pts',(2.18710556500325,-1.,-3.29920022557635));
#54338=CARTESIAN_POINT('Ctrl Pts',(2.19306710376112,-1.,-3.30385816281831));
#54339=CARTESIAN_POINT('Ctrl Pts',(2.19906078949924,-1.,-3.30848134694597));
#54340=CARTESIAN_POINT('Ctrl Pts',(2.20508863150608,-1.,-3.3130742460895));
#54341=CARTESIAN_POINT('Ctrl Pts',(2.21115211847872,-1.,-3.31764044024231));
#54342=CARTESIAN_POINT('Ctrl Pts',(2.21725135110889,-1.,-3.32218125618955));
#54343=CARTESIAN_POINT('Ctrl Pts',(2.22338548312758,-1.,-3.32669646722871));
#54344=CARTESIAN_POINT('Ctrl Pts',(2.22955308907221,-1.,-3.33118487773593));
#54345=CARTESIAN_POINT('Ctrl Pts',(2.23575256328809,-1.,-3.33564495756478));
#54346=CARTESIAN_POINT('Ctrl Pts',(2.24198249391437,-1.,-3.34007543738044));
#54347=CARTESIAN_POINT('Ctrl Pts',(2.24824207678287,-1.,-3.34447596770768));
#54348=CARTESIAN_POINT('Ctrl Pts',(2.25453097693524,-1.,-3.34884690292342));
#54349=CARTESIAN_POINT('Ctrl Pts',(2.26084915222484,-1.,-3.35318902552676));
#54350=CARTESIAN_POINT('Ctrl Pts',(2.26719668579921,-1.,-3.35750328523077));
#54351=CARTESIAN_POINT('Ctrl Pts',(2.27357362620902,-1.,-3.36179055004369));
#54352=CARTESIAN_POINT('Ctrl Pts',(2.27997979457968,-1.,-3.36605130712978));
#54353=CARTESIAN_POINT('Ctrl Pts',(2.28641481081045,-1.,-3.37028570206357));
#54354=CARTESIAN_POINT('Ctrl Pts',(2.2928781800731,-1.,-3.37449367172707));
#54355=CARTESIAN_POINT('Ctrl Pts',(2.29936936127588,-1.,-3.37867504959382));
#54356=CARTESIAN_POINT('Ctrl Pts',(2.30588783640389,-1.,-3.38282967336676));
#54357=CARTESIAN_POINT('Ctrl Pts',(2.31243319489505,-1.,-3.38695751492659));
#54358=CARTESIAN_POINT('Ctrl Pts',(2.31900513925627,-1.,-3.39105869475112));
#54359=CARTESIAN_POINT('Ctrl Pts',(2.32560343902683,-1.,-3.39513342020045));
#54360=CARTESIAN_POINT('Ctrl Pts',(2.33222789882601,-1.,-3.39918194578115));
#54361=CARTESIAN_POINT('Ctrl Pts',(2.33887832342715,-1.,-3.40320452776646));
#54362=CARTESIAN_POINT('Ctrl Pts',(2.34555447648901,-1.,-3.40720137403888));
#54363=CARTESIAN_POINT('Ctrl Pts',(2.35225606823649,-1.,-3.41117262313464));
#54364=CARTESIAN_POINT('Ctrl Pts',(2.35898278606449,-1.,-3.4151183675076));
#54365=CARTESIAN_POINT('Ctrl Pts',(2.36573431470313,-1.,-3.41903866635384));
#54366=CARTESIAN_POINT('Ctrl Pts',(2.37251035954351,-1.,-3.42293356216595));
#54367=CARTESIAN_POINT('Ctrl Pts',(2.37931067029517,-1.,-3.42680309755241));
#54368=CARTESIAN_POINT('Ctrl Pts',(2.38613505844641,-1.,-3.43064732714472));
#54369=CARTESIAN_POINT('Ctrl Pts',(2.39298338805823,-1.,-3.43446630680436));
#54370=CARTESIAN_POINT('Ctrl Pts',(2.39848113411428,-1.,-3.43750133066037));
#54371=CARTESIAN_POINT('Ctrl Pts',(2.40261515590099,-1.,-3.43976627485223));
#54372=CARTESIAN_POINT('Ctrl Pts',(2.40537592959345,-1.,-3.44127120683402));
#54373=CARTESIAN_POINT('Ctrl Pts',(2.40675750623143,-1.,-3.44202241512147));
#54374=CARTESIAN_POINT('',(2.52982887637028,-1.,-3.35260583073571));
#54375=CARTESIAN_POINT('',(2.40675750623143,-1.,-3.44202241512147));
#54376=CARTESIAN_POINT('',(2.36531447826073,-1.,-2.90994629141676));
#54377=CARTESIAN_POINT('Ctrl Pts',(2.52982887637028,-1.,-3.35260583073571));
#54378=CARTESIAN_POINT('Ctrl Pts',(2.5295413654909,-1.,-3.35105973714072));
#54379=CARTESIAN_POINT('Ctrl Pts',(2.52896321610703,-1.,-3.34796903576663));
#54380=CARTESIAN_POINT('Ctrl Pts',(2.52808660915689,-1.,-3.34333744115511));
#54381=CARTESIAN_POINT('Ctrl Pts',(2.52689902690158,-1.,-3.33717089999103));
#54382=CARTESIAN_POINT('Ctrl Pts',(2.52538321164634,-1.,-3.32947762187533));
#54383=CARTESIAN_POINT('Ctrl Pts',(2.5238359839626,-1.,-3.32179931078699));
#54384=CARTESIAN_POINT('Ctrl Pts',(2.52225724871313,-1.,-3.31413607874645));
#54385=CARTESIAN_POINT('Ctrl Pts',(2.52064689568511,-1.,-3.30648808815443));
#54386=CARTESIAN_POINT('Ctrl Pts',(2.51900480701068,-1.,-3.29885556388353));
#54387=CARTESIAN_POINT('Ctrl Pts',(2.51733085123797,-1.,-3.2912387729927));
#54388=CARTESIAN_POINT('Ctrl Pts',(2.51562487464514,-1.,-3.28363799702982));
#54389=CARTESIAN_POINT('Ctrl Pts',(2.513886692704,-1.,-3.27605350473142));
#54390=CARTESIAN_POINT('Ctrl Pts',(2.51211608411423,-1.,-3.26848552888116));
#54391=CARTESIAN_POINT('Ctrl Pts',(2.51031277813486,-1.,-3.26093423001434));
#54392=CARTESIAN_POINT('Ctrl Pts',(2.50847647070723,-1.,-3.25339971460982));
#54393=CARTESIAN_POINT('Ctrl Pts',(2.506606859405,-1.,-3.24588208983849));
#54394=CARTESIAN_POINT('Ctrl Pts',(2.5047036758003,-1.,-3.23838151080319));
#54395=CARTESIAN_POINT('Ctrl Pts',(2.50276671338111,-1.,-3.23089822320646));
#54396=CARTESIAN_POINT('Ctrl Pts',(2.50079587201957,-1.,-3.22343262620503));
#54397=CARTESIAN_POINT('Ctrl Pts',(2.4987911459939,-1.,-3.21598526261286));
#54398=CARTESIAN_POINT('Ctrl Pts',(2.4967525264737,-1.,-3.20855669849836));
#54399=CARTESIAN_POINT('Ctrl Pts',(2.49467992057755,-1.,-3.20114742397588));
#54400=CARTESIAN_POINT('Ctrl Pts',(2.49257307239848,-1.,-3.19375775555798));
#54401=CARTESIAN_POINT('Ctrl Pts',(2.49043146334059,-1.,-3.18638771282266));
#54402=CARTESIAN_POINT('Ctrl Pts',(2.48825428288201,-1.,-3.17903698136622));
#54403=CARTESIAN_POINT('Ctrl Pts',(2.48604065348587,-1.,-3.17170518863313));
#54404=CARTESIAN_POINT('Ctrl Pts',(2.48378981792725,-1.,-3.16439213290161));
#54405=CARTESIAN_POINT('Ctrl Pts',(2.48150133566571,-1.,-3.15709802322739));
#54406=CARTESIAN_POINT('Ctrl Pts',(2.47917529057029,-1.,-3.14982373241352));
#54407=CARTESIAN_POINT('Ctrl Pts',(2.47681245356109,-1.,-3.1425709954655));
#54408=CARTESIAN_POINT('Ctrl Pts',(2.47441378371932,-1.,-3.13534181229295));
#54409=CARTESIAN_POINT('Ctrl Pts',(2.47197997765871,-1.,-3.12813790805952));
#54410=CARTESIAN_POINT('Ctrl Pts',(2.46951098947469,-1.,-3.12096015766983));
#54411=CARTESIAN_POINT('Ctrl Pts',(2.46700558843506,-1.,-3.11380805536122));
#54412=CARTESIAN_POINT('Ctrl Pts',(2.46446082979646,-1.,-3.1066790790198));
#54413=CARTESIAN_POINT('Ctrl Pts',(2.46187308501884,-1.,-3.09956993697052));
#54414=CARTESIAN_POINT('Ctrl Pts',(2.4592391256388,-1.,-3.09247787931887));
#54415=CARTESIAN_POINT('Ctrl Pts',(2.45655725437039,-1.,-3.08540206545315));
#54416=CARTESIAN_POINT('Ctrl Pts',(2.4538282678779,-1.,-3.07834472886139));
#54417=CARTESIAN_POINT('Ctrl Pts',(2.45105688854422,-1.,-3.07131290521297));
#54418=CARTESIAN_POINT('Ctrl Pts',(2.44824970516543,-1.,-3.06431596421405));
#54419=CARTESIAN_POINT('Ctrl Pts',(2.44541251892556,-1.,-3.05736242671506));
#54420=CARTESIAN_POINT('Ctrl Pts',(2.44254768923105,-1.,-3.05045678021504));
#54421=CARTESIAN_POINT('Ctrl Pts',(2.43965194061857,-1.,-3.04359685040555));
#54422=CARTESIAN_POINT('Ctrl Pts',(2.43671278042414,-1.,-3.03676949672822));
#54423=CARTESIAN_POINT('Ctrl Pts',(2.43371241361488,-1.,-3.02995534946978));
#54424=CARTESIAN_POINT('Ctrl Pts',(2.43063415586637,-1.,-3.02313656036004));
#54425=CARTESIAN_POINT('Ctrl Pts',(2.42746856264168,-1.,-3.01630420830504));
#54426=CARTESIAN_POINT('Ctrl Pts',(2.42421849439613,-1.,-3.00946442616659));
#54427=CARTESIAN_POINT('Ctrl Pts',(2.42090763946779,-1.,-3.00264868585996));
#54428=CARTESIAN_POINT('Ctrl Pts',(2.41757324500514,-1.,-2.99590509293503));
#54429=CARTESIAN_POINT('Ctrl Pts',(2.41425064199586,-1.,-2.98927983005796));
#54430=CARTESIAN_POINT('Ctrl Pts',(2.41095909342571,-1.,-2.98280015815107));
#54431=CARTESIAN_POINT('Ctrl Pts',(2.40768975073713,-1.,-2.97646002822422));
#54432=CARTESIAN_POINT('Ctrl Pts',(2.40438604734919,-1.,-2.9701964131236));
#54433=CARTESIAN_POINT('Ctrl Pts',(2.4009556571164,-1.,-2.96390432240312));
#54434=CARTESIAN_POINT('Ctrl Pts',(2.39730553974516,-1.,-2.95748006482942));
#54435=CARTESIAN_POINT('Ctrl Pts',(2.39337207631667,-1.,-2.95085857128439));
#54436=CARTESIAN_POINT('Ctrl Pts',(2.38914929090759,-1.,-2.94404820669076));
#54437=CARTESIAN_POINT('Ctrl Pts',(2.38472771516311,-1.,-2.93717903280391));
#54438=CARTESIAN_POINT('Ctrl Pts',(2.38028989582073,-1.,-2.93049643640206));
#54439=CARTESIAN_POINT('Ctrl Pts',(2.3760651052403,-1.,-2.92430340582608));
#54440=CARTESIAN_POINT('Ctrl Pts',(2.37229381109821,-1.,-2.91891503791411));
#54441=CARTESIAN_POINT('Ctrl Pts',(2.36919161373173,-1.,-2.9146124988314));
#54442=CARTESIAN_POINT('Ctrl Pts',(2.36707658451664,-1.,-2.91181344022549));
#54443=CARTESIAN_POINT('Ctrl Pts',(2.36599991765749,-1.,-2.91051690822156));
#54444=CARTESIAN_POINT('Ctrl Pts',(2.36553202948613,-1.,-2.91005770527719));
#54445=CARTESIAN_POINT('Ctrl Pts',(2.36536211188453,-1.,-2.90995756655606));
#54446=CARTESIAN_POINT('Ctrl Pts',(2.36531447826073,-1.,-2.90994629141676));
#54447=CARTESIAN_POINT('',(2.50410331873042,-1.,-2.79140942341378));
#54448=CARTESIAN_POINT('Origin',(0.,-1.,0.));
#54449=CARTESIAN_POINT('',(2.91557726271063,-1.,-3.02314558451372));
#54450=CARTESIAN_POINT('Ctrl Pts',(2.50410331873042,-1.,-2.79140942341378));
#54451=CARTESIAN_POINT('Ctrl Pts',(2.50410700351426,-1.,-2.79145823440899));
#54452=CARTESIAN_POINT('Ctrl Pts',(2.50417932839343,-1.,-2.79164172519039));
#54453=CARTESIAN_POINT('Ctrl Pts',(2.50455968395235,-1.,-2.79217568804874));
#54454=CARTESIAN_POINT('Ctrl Pts',(2.50567182569153,-1.,-2.79344192164204));
#54455=CARTESIAN_POINT('Ctrl Pts',(2.50810555977564,-1.,-2.7959687805717));
#54456=CARTESIAN_POINT('Ctrl Pts',(2.51186983687947,-1.,-2.79970585014308));
#54457=CARTESIAN_POINT('Ctrl Pts',(2.51660190466067,-1.,-2.80427363984939));
#54458=CARTESIAN_POINT('Ctrl Pts',(2.52205778589922,-1.,-2.80941521967234));
#54459=CARTESIAN_POINT('Ctrl Pts',(2.52796388055457,-1.,-2.8148437904867));
#54460=CARTESIAN_POINT('Ctrl Pts',(2.53405679667463,-1.,-2.82028550483744));
#54461=CARTESIAN_POINT('Ctrl Pts',(2.54012272520141,-1.,-2.82552167649157));
#54462=CARTESIAN_POINT('Ctrl Pts',(2.54604736792542,-1.,-2.83044254225794));
#54463=CARTESIAN_POINT('Ctrl Pts',(2.55182152806964,-1.,-2.83505269592412));
#54464=CARTESIAN_POINT('Ctrl Pts',(2.55749952145165,-1.,-2.83942515220699));
#54465=CARTESIAN_POINT('Ctrl Pts',(2.56316920798489,-1.,-2.84366802680211));
#54466=CARTESIAN_POINT('Ctrl Pts',(2.56891984251743,-1.,-2.84788893329091));
#54467=CARTESIAN_POINT('Ctrl Pts',(2.57480482727128,-1.,-2.85215360144483));
#54468=CARTESIAN_POINT('Ctrl Pts',(2.58082875254407,-1.,-2.85647171715147));
#54469=CARTESIAN_POINT('Ctrl Pts',(2.5869677064356,-1.,-2.86081999003668));
#54470=CARTESIAN_POINT('Ctrl Pts',(2.59318160184921,-1.,-2.86515629953528));
#54471=CARTESIAN_POINT('Ctrl Pts',(2.59942875223202,-1.,-2.86943633170712));
#54472=CARTESIAN_POINT('Ctrl Pts',(2.6056817788128,-1.,-2.87363176656475));
#54473=CARTESIAN_POINT('Ctrl Pts',(2.61193507170928,-1.,-2.87773881947885));
#54474=CARTESIAN_POINT('Ctrl Pts',(2.61819596473087,-1.,-2.88176821427502));
#54475=CARTESIAN_POINT('Ctrl Pts',(2.62447947640253,-1.,-2.88573922195049));
#54476=CARTESIAN_POINT('Ctrl Pts',(2.63080195420771,-1.,-2.88967244854243));
#54477=CARTESIAN_POINT('Ctrl Pts',(2.63717442263944,-1.,-2.89358228854557));
#54478=CARTESIAN_POINT('Ctrl Pts',(2.64359851684146,-1.,-2.89747231723361));
#54479=CARTESIAN_POINT('Ctrl Pts',(2.65007017365576,-1.,-2.90133950224879));
#54480=CARTESIAN_POINT('Ctrl Pts',(2.65658188464287,-1.,-2.90517678087467));
#54481=CARTESIAN_POINT('Ctrl Pts',(2.66312542616808,-1.,-2.90897617968921));
#54482=CARTESIAN_POINT('Ctrl Pts',(2.66969458792627,-1.,-2.91273193382876));
#54483=CARTESIAN_POINT('Ctrl Pts',(2.67628728855309,-1.,-2.91644290704281));
#54484=CARTESIAN_POINT('Ctrl Pts',(2.68290409279689,-1.,-2.92011090722152));
#54485=CARTESIAN_POINT('Ctrl Pts',(2.68954721165342,-1.,-2.92373955325876));
#54486=CARTESIAN_POINT('Ctrl Pts',(2.69621932864302,-1.,-2.92733294395268));
#54487=CARTESIAN_POINT('Ctrl Pts',(2.70292247416881,-1.,-2.93089438233746));
#54488=CARTESIAN_POINT('Ctrl Pts',(2.70965695523776,-1.,-2.93442516311168));
#54489=CARTESIAN_POINT('Ctrl Pts',(2.71642190053575,-1.,-2.93792519474955));
#54490=CARTESIAN_POINT('Ctrl Pts',(2.72321571511322,-1.,-2.94139351933882));
#54491=CARTESIAN_POINT('Ctrl Pts',(2.73003657371613,-1.,-2.94482887675139));
#54492=CARTESIAN_POINT('Ctrl Pts',(2.73688288329825,-1.,-2.94823023414381));
#54493=CARTESIAN_POINT('Ctrl Pts',(2.7437537949221,-1.,-2.95159737214305));
#54494=CARTESIAN_POINT('Ctrl Pts',(2.75064903318996,-1.,-2.95493069316211));
#54495=CARTESIAN_POINT('Ctrl Pts',(2.75756867888393,-1.,-2.9582309766594));
#54496=CARTESIAN_POINT('Ctrl Pts',(2.76451296269571,-1.,-2.96149914764832));
#54497=CARTESIAN_POINT('Ctrl Pts',(2.77148206836464,-1.,-2.96473605585548));
#54498=CARTESIAN_POINT('Ctrl Pts',(2.77847589542767,-1.,-2.9679422104295));
#54499=CARTESIAN_POINT('Ctrl Pts',(2.78549409123657,-1.,-2.97111781461349));
#54500=CARTESIAN_POINT('Ctrl Pts',(2.79253615718147,-1.,-2.97426288347475));
#54501=CARTESIAN_POINT('Ctrl Pts',(2.79960153278186,-1.,-2.97737733718242));
#54502=CARTESIAN_POINT('Ctrl Pts',(2.80668968101162,-1.,-2.98046109647299));
#54503=CARTESIAN_POINT('Ctrl Pts',(2.81380019196454,-1.,-2.9835141977994));
#54504=CARTESIAN_POINT('Ctrl Pts',(2.82093279065704,-1.,-2.98653680669434));
#54505=CARTESIAN_POINT('Ctrl Pts',(2.82808728190402,-1.,-2.98952916401699));
#54506=CARTESIAN_POINT('Ctrl Pts',(2.83526351254383,-1.,-2.99249155170479));
#54507=CARTESIAN_POINT('Ctrl Pts',(2.84246132984334,-1.,-2.995424253416));
#54508=CARTESIAN_POINT('Ctrl Pts',(2.84968053289104,-1.,-2.99832751144566));
#54509=CARTESIAN_POINT('Ctrl Pts',(2.85692085715129,-1.,-3.0012015079552));
#54510=CARTESIAN_POINT('Ctrl Pts',(2.86418200833065,-1.,-3.00404638316245));
#54511=CARTESIAN_POINT('Ctrl Pts',(2.87146368430104,-1.,-3.00686224485374));
#54512=CARTESIAN_POINT('Ctrl Pts',(2.87876560072799,-1.,-3.0096491810855));
#54513=CARTESIAN_POINT('Ctrl Pts',(2.88608751706796,-1.,-3.01240727309568));
#54514=CARTESIAN_POINT('Ctrl Pts',(2.8934292556764,-1.,-3.01513660433291));
#54515=CARTESIAN_POINT('Ctrl Pts',(2.90079069102661,-1.,-3.01783725123646));
#54516=CARTESIAN_POINT('Ctrl Pts',(2.90669553303902,-1.,-3.01997487194926));
#54517=CARTESIAN_POINT('Ctrl Pts',(2.91113297349052,-1.,-3.02156522743299));
#54518=CARTESIAN_POINT('Ctrl Pts',(2.91409518070707,-1.,-3.02261975104912));
#54519=CARTESIAN_POINT('Ctrl Pts',(2.91557726271063,-1.,-3.02314558451372));
#54520=CARTESIAN_POINT('',(3.02314558451372,-1.,-2.91557726271063));
#54521=CARTESIAN_POINT('',(2.91557726271063,-1.,-3.02314558451372));
#54522=CARTESIAN_POINT('',(2.79140942341258,-1.,-2.50410331873176));
#54523=CARTESIAN_POINT('Ctrl Pts',(3.02314558451372,-1.,-2.91557726271063));
#54524=CARTESIAN_POINT('Ctrl Pts',(3.02261975104593,-1.,-2.91409518070399));
#54525=CARTESIAN_POINT('Ctrl Pts',(3.02156522742431,-1.,-2.91113297348212));
#54526=CARTESIAN_POINT('Ctrl Pts',(3.01997487193503,-1.,-2.90669553302526));
#54527=CARTESIAN_POINT('Ctrl Pts',(3.01783725121981,-1.,-2.9007906910105));
#54528=CARTESIAN_POINT('Ctrl Pts',(3.01513660431928,-1.,-2.89342925566321));
#54529=CARTESIAN_POINT('Ctrl Pts',(3.01240727308829,-1.,-2.8860875170608));
#54530=CARTESIAN_POINT('Ctrl Pts',(3.00964918108476,-1.,-2.87876560072727));
#54531=CARTESIAN_POINT('Ctrl Pts',(3.00686224485784,-1.,-2.87146368430502));
#54532=CARTESIAN_POINT('Ctrl Pts',(3.00404638316867,-1.,-2.86418200833667));
#54533=CARTESIAN_POINT('Ctrl Pts',(3.00120150796095,-1.,-2.85692085715686));
#54534=CARTESIAN_POINT('Ctrl Pts',(2.99832751144925,-1.,-2.84968053289451));
#54535=CARTESIAN_POINT('Ctrl Pts',(2.99542425341685,-1.,-2.84246132984415));
#54536=CARTESIAN_POINT('Ctrl Pts',(2.99249155170339,-1.,-2.83526351254248));
#54537=CARTESIAN_POINT('Ctrl Pts',(2.98952916401446,-1.,-2.82808728190157));
#54538=CARTESIAN_POINT('Ctrl Pts',(2.9865368066918,-1.,-2.82093279065457));
#54539=CARTESIAN_POINT('Ctrl Pts',(2.98351419779767,-1.,-2.81380019196286));
#54540=CARTESIAN_POINT('Ctrl Pts',(2.98046109647241,-1.,-2.80668968101106));
#54541=CARTESIAN_POINT('Ctrl Pts',(2.97737733718287,-1.,-2.7996015327823));
#54542=CARTESIAN_POINT('Ctrl Pts',(2.9742628834758,-1.,-2.79253615718248));
#54543=CARTESIAN_POINT('Ctrl Pts',(2.97111781461465,-1.,-2.78549409123769));
#54544=CARTESIAN_POINT('Ctrl Pts',(2.96794221043036,-1.,-2.7784758954285));
#54545=CARTESIAN_POINT('Ctrl Pts',(2.96473605585583,-1.,-2.77148206836498));
#54546=CARTESIAN_POINT('Ctrl Pts',(2.96149914764818,-1.,-2.76451296269557));
#54547=CARTESIAN_POINT('Ctrl Pts',(2.95823097665896,-1.,-2.7575686788835));
#54548=CARTESIAN_POINT('Ctrl Pts',(2.95493069316161,-1.,-2.75064903318947));
#54549=CARTESIAN_POINT('Ctrl Pts',(2.95159737214266,-1.,-2.74375379492172));
#54550=CARTESIAN_POINT('Ctrl Pts',(2.94823023414364,-1.,-2.73688288329808));
#54551=CARTESIAN_POINT('Ctrl Pts',(2.94482887675143,-1.,-2.73003657371617));
#54552=CARTESIAN_POINT('Ctrl Pts',(2.94139351933897,-1.,-2.72321571511337));
#54553=CARTESIAN_POINT('Ctrl Pts',(2.93792519474972,-1.,-2.71642190053592));
#54554=CARTESIAN_POINT('Ctrl Pts',(2.93442516311179,-1.,-2.70965695523787));
#54555=CARTESIAN_POINT('Ctrl Pts',(2.93089438233749,-1.,-2.70292247416885));
#54556=CARTESIAN_POINT('Ctrl Pts',(2.92733294395267,-1.,-2.69621932864301));
#54557=CARTESIAN_POINT('Ctrl Pts',(2.92373955325875,-1.,-2.68954721165339));
#54558=CARTESIAN_POINT('Ctrl Pts',(2.92011090722152,-1.,-2.68290409279688));
#54559=CARTESIAN_POINT('Ctrl Pts',(2.91644290704285,-1.,-2.67628728855312));
#54560=CARTESIAN_POINT('Ctrl Pts',(2.91273193382882,-1.,-2.66969458792631));
#54561=CARTESIAN_POINT('Ctrl Pts',(2.90897617968923,-1.,-2.6631254261681));
#54562=CARTESIAN_POINT('Ctrl Pts',(2.90517678087461,-1.,-2.65658188464282));
#54563=CARTESIAN_POINT('Ctrl Pts',(2.90133950224867,-1.,-2.65007017365564));
#54564=CARTESIAN_POINT('Ctrl Pts',(2.89747231723345,-1.,-2.64359851684131));
#54565=CARTESIAN_POINT('Ctrl Pts',(2.89358228854544,-1.,-2.63717442263932));
#54566=CARTESIAN_POINT('Ctrl Pts',(2.88967244854239,-1.,-2.63080195420767));
#54567=CARTESIAN_POINT('Ctrl Pts',(2.88573922195059,-1.,-2.62447947640262));
#54568=CARTESIAN_POINT('Ctrl Pts',(2.88176821427525,-1.,-2.61819596473108));
#54569=CARTESIAN_POINT('Ctrl Pts',(2.87773881947915,-1.,-2.61193507170955));
#54570=CARTESIAN_POINT('Ctrl Pts',(2.87363176656501,-1.,-2.60568177881303));
#54571=CARTESIAN_POINT('Ctrl Pts',(2.86943633170722,-1.,-2.5994287522321));
#54572=CARTESIAN_POINT('Ctrl Pts',(2.86515629953513,-1.,-2.59318160184908));
#54573=CARTESIAN_POINT('Ctrl Pts',(2.86081999003629,-1.,-2.58696770643524));
#54574=CARTESIAN_POINT('Ctrl Pts',(2.85647171715092,-1.,-2.58082875254357));
#54575=CARTESIAN_POINT('Ctrl Pts',(2.85215360144431,-1.,-2.57480482727081));
#54576=CARTESIAN_POINT('Ctrl Pts',(2.84788893329067,-1.,-2.56891984251721));
#54577=CARTESIAN_POINT('Ctrl Pts',(2.84366802680237,-1.,-2.56316920798513));
#54578=CARTESIAN_POINT('Ctrl Pts',(2.83942515220782,-1.,-2.55749952145241));
#54579=CARTESIAN_POINT('Ctrl Pts',(2.83505269592536,-1.,-2.55182152807077));
#54580=CARTESIAN_POINT('Ctrl Pts',(2.83044254225917,-1.,-2.54604736792655));
#54581=CARTESIAN_POINT('Ctrl Pts',(2.8255216764922,-1.,-2.54012272520199));
#54582=CARTESIAN_POINT('Ctrl Pts',(2.82028550483689,-1.,-2.53405679667412));
#54583=CARTESIAN_POINT('Ctrl Pts',(2.81484379048475,-1.,-2.52796388055278));
#54584=CARTESIAN_POINT('Ctrl Pts',(2.80941521966941,-1.,-2.52205778589653));
#54585=CARTESIAN_POINT('Ctrl Pts',(2.80427363984653,-1.,-2.51660190465805));
#54586=CARTESIAN_POINT('Ctrl Pts',(2.79970585014168,-1.,-2.51186983687818));
#54587=CARTESIAN_POINT('Ctrl Pts',(2.79596878057287,-1.,-2.50810555977671));
#54588=CARTESIAN_POINT('Ctrl Pts',(2.79344192164147,-1.,-2.50567182569081));
#54589=CARTESIAN_POINT('Ctrl Pts',(2.79217568804755,-1.,-2.50455968395146));
#54590=CARTESIAN_POINT('Ctrl Pts',(2.79164172518905,-1.,-2.50417932839313));
#54591=CARTESIAN_POINT('Ctrl Pts',(2.79145823440781,-1.,-2.50410700351493));
#54592=CARTESIAN_POINT('Ctrl Pts',(2.79140942341258,-1.,-2.50410331873176));
#54593=CARTESIAN_POINT('',(2.90994629141562,-1.,-2.36531447826213));
#54594=CARTESIAN_POINT('Origin',(0.,-1.,0.));
#54595=CARTESIAN_POINT('',(3.35260583073571,-1.,-2.52982887637028));
#54596=CARTESIAN_POINT('Ctrl Pts',(2.90994629141562,-1.,-2.36531447826213));
#54597=CARTESIAN_POINT('Ctrl Pts',(2.90995756655558,-1.,-2.3653621118858));
#54598=CARTESIAN_POINT('Ctrl Pts',(2.9100577052777,-1.,-2.36553202948741));
#54599=CARTESIAN_POINT('Ctrl Pts',(2.91051690822262,-1.,-2.36599991765853));
#54600=CARTESIAN_POINT('Ctrl Pts',(2.91181344022628,-1.,-2.36707658451709));
#54601=CARTESIAN_POINT('Ctrl Pts',(2.91461249883016,-1.,-2.36919161373074));
#54602=CARTESIAN_POINT('Ctrl Pts',(2.9189150379156,-1.,-2.37229381109939));
#54603=CARTESIAN_POINT('Ctrl Pts',(2.92430340582912,-1.,-2.37606510524271));
#54604=CARTESIAN_POINT('Ctrl Pts',(2.93049643640517,-1.,-2.3802898958232));
#54605=CARTESIAN_POINT('Ctrl Pts',(2.93717903280599,-1.,-2.38472771516476));
#54606=CARTESIAN_POINT('Ctrl Pts',(2.94404820669135,-1.,-2.38914929090806));
#54607=CARTESIAN_POINT('Ctrl Pts',(2.95085857128372,-1.,-2.39337207631613));
#54608=CARTESIAN_POINT('Ctrl Pts',(2.95748006482811,-1.,-2.39730553974412));
#54609=CARTESIAN_POINT('Ctrl Pts',(2.9639043224018,-1.,-2.40095565711535));
#54610=CARTESIAN_POINT('Ctrl Pts',(2.97019641312272,-1.,-2.40438604734848));
#54611=CARTESIAN_POINT('Ctrl Pts',(2.97646002822395,-1.,-2.40768975073691));
#54612=CARTESIAN_POINT('Ctrl Pts',(2.98280015815132,-1.,-2.41095909342591));
#54613=CARTESIAN_POINT('Ctrl Pts',(2.98927983005851,-1.,-2.4142506419963));
#54614=CARTESIAN_POINT('Ctrl Pts',(2.99590509293561,-1.,-2.4175732450056));
#54615=CARTESIAN_POINT('Ctrl Pts',(3.00264868586038,-1.,-2.42090763946812));
#54616=CARTESIAN_POINT('Ctrl Pts',(3.00946442616674,-1.,-2.42421849439625));
#54617=CARTESIAN_POINT('Ctrl Pts',(3.01630420830493,-1.,-2.4274685626416));
#54618=CARTESIAN_POINT('Ctrl Pts',(3.02313656035977,-1.,-2.43063415586615));
#54619=CARTESIAN_POINT('Ctrl Pts',(3.02995534946946,-1.,-2.43371241361462));
#54620=CARTESIAN_POINT('Ctrl Pts',(3.03676949672797,-1.,-2.43671278042394));
#54621=CARTESIAN_POINT('Ctrl Pts',(3.04359685040545,-1.,-2.43965194061849));
#54622=CARTESIAN_POINT('Ctrl Pts',(3.05045678021509,-1.,-2.44254768923109));
#54623=CARTESIAN_POINT('Ctrl Pts',(3.05736242671521,-1.,-2.44541251892568));
#54624=CARTESIAN_POINT('Ctrl Pts',(3.06431596421422,-1.,-2.44824970516558));
#54625=CARTESIAN_POINT('Ctrl Pts',(3.0713129052131,-1.,-2.45105688854432));
#54626=CARTESIAN_POINT('Ctrl Pts',(3.07834472886145,-1.,-2.45382826787795));
#54627=CARTESIAN_POINT('Ctrl Pts',(3.08540206545313,-1.,-2.45655725437037));
#54628=CARTESIAN_POINT('Ctrl Pts',(3.09247787931881,-1.,-2.45923912563875));
#54629=CARTESIAN_POINT('Ctrl Pts',(3.09956993697048,-1.,-2.4618730850188));
#54630=CARTESIAN_POINT('Ctrl Pts',(3.10667907901981,-1.,-2.46446082979645));
#54631=CARTESIAN_POINT('Ctrl Pts',(3.11380805536124,-1.,-2.46700558843507));
#54632=CARTESIAN_POINT('Ctrl Pts',(3.12096015766984,-1.,-2.4695109894747));
#54633=CARTESIAN_POINT('Ctrl Pts',(3.12813790805948,-1.,-2.47197997765868));
#54634=CARTESIAN_POINT('Ctrl Pts',(3.13534181229282,-1.,-2.47441378371923));
#54635=CARTESIAN_POINT('Ctrl Pts',(3.14257099546531,-1.,-2.47681245356095));
#54636=CARTESIAN_POINT('Ctrl Pts',(3.14982373241335,-1.,-2.47917529057016));
#54637=CARTESIAN_POINT('Ctrl Pts',(3.15709802322735,-1.,-2.48150133566568));
#54638=CARTESIAN_POINT('Ctrl Pts',(3.16439213290181,-1.,-2.48378981792739));
#54639=CARTESIAN_POINT('Ctrl Pts',(3.17170518863357,-1.,-2.48604065348619));
#54640=CARTESIAN_POINT('Ctrl Pts',(3.17903698136678,-1.,-2.48825428288243));
#54641=CARTESIAN_POINT('Ctrl Pts',(3.18638771282315,-1.,-2.49043146334095));
#54642=CARTESIAN_POINT('Ctrl Pts',(3.19375775555814,-1.,-2.4925730723986));
#54643=CARTESIAN_POINT('Ctrl Pts',(3.20114742397549,-1.,-2.49467992057726));
#54644=CARTESIAN_POINT('Ctrl Pts',(3.2085566984974,-1.,-2.49675252647298));
#54645=CARTESIAN_POINT('Ctrl Pts',(3.21598526261157,-1.,-2.49879114599293));
#54646=CARTESIAN_POINT('Ctrl Pts',(3.22343262620387,-1.,-2.5007958720187));
#54647=CARTESIAN_POINT('Ctrl Pts',(3.23089822320596,-1.,-2.50276671338074));
#54648=CARTESIAN_POINT('Ctrl Pts',(3.23838151080383,-1.,-2.50470367580078));
#54649=CARTESIAN_POINT('Ctrl Pts',(3.24588208984042,-1.,-2.50660685940645));
#54650=CARTESIAN_POINT('Ctrl Pts',(3.25339971461265,-1.,-2.50847647070936));
#54651=CARTESIAN_POINT('Ctrl Pts',(3.26093423001716,-1.,-2.51031277813697));
#54652=CARTESIAN_POINT('Ctrl Pts',(3.26848552888271,-1.,-2.51211608411539));
#54653=CARTESIAN_POINT('Ctrl Pts',(3.27605350473048,-1.,-2.51388669270329));
#54654=CARTESIAN_POINT('Ctrl Pts',(3.28363799702583,-1.,-2.51562487464215));
#54655=CARTESIAN_POINT('Ctrl Pts',(3.2912387729863,-1.,-2.51733085123316));
#54656=CARTESIAN_POINT('Ctrl Pts',(3.29885556387661,-1.,-2.51900480700548));
#54657=CARTESIAN_POINT('Ctrl Pts',(3.30648808814986,-1.,-2.52064689568167));
#54658=CARTESIAN_POINT('Ctrl Pts',(3.31413607874727,-1.,-2.52225724871375));
#54659=CARTESIAN_POINT('Ctrl Pts',(3.32179931079521,-1.,-2.52383598396878));
#54660=CARTESIAN_POINT('Ctrl Pts',(3.32947762189049,-1.,-2.52538321165774));
#54661=CARTESIAN_POINT('Ctrl Pts',(3.33717090000955,-1.,-2.52689902691551));
#54662=CARTESIAN_POINT('Ctrl Pts',(3.34333744117093,-1.,-2.52808660916879));
#54663=CARTESIAN_POINT('Ctrl Pts',(3.34796903577628,-1.,-2.5289632161143));
#54664=CARTESIAN_POINT('Ctrl Pts',(3.35105973714426,-1.,-2.52954136549357));
#54665=CARTESIAN_POINT('Ctrl Pts',(3.35260583073571,-1.,-2.52982887637028));
#54666=CARTESIAN_POINT('',(3.44202241512147,-1.,-2.40675750623143));
#54667=CARTESIAN_POINT('',(3.35260583073571,-1.,-2.52982887637028));
#54668=CARTESIAN_POINT('',(3.14877060440327,-1.,-2.03660101169714));
#54669=CARTESIAN_POINT('Ctrl Pts',(3.44202241512147,-1.,-2.40675750623143));
#54670=CARTESIAN_POINT('Ctrl Pts',(3.44127120683039,-1.,-2.4053759295909));
#54671=CARTESIAN_POINT('Ctrl Pts',(3.43976627484234,-1.,-2.40261515589405));
#54672=CARTESIAN_POINT('Ctrl Pts',(3.43750133064416,-1.,-2.39848113410292));
#54673=CARTESIAN_POINT('Ctrl Pts',(3.4344663067854,-1.,-2.39298338804493));
#54674=CARTESIAN_POINT('Ctrl Pts',(3.43064732712919,-1.,-2.38613505843552));
#54675=CARTESIAN_POINT('Ctrl Pts',(3.42680309754399,-1.,-2.37931067028926));
#54676=CARTESIAN_POINT('Ctrl Pts',(3.42293356216511,-1.,-2.37251035954292));
#54677=CARTESIAN_POINT('Ctrl Pts',(3.41903866635852,-1.,-2.36573431470642));
#54678=CARTESIAN_POINT('Ctrl Pts',(3.41511836751469,-1.,-2.35898278606946));
#54679=CARTESIAN_POINT('Ctrl Pts',(3.41117262314119,-1.,-2.35225606824109));
#54680=CARTESIAN_POINT('Ctrl Pts',(3.40720137404297,-1.,-2.34555447649188));
#54681=CARTESIAN_POINT('Ctrl Pts',(3.40320452776743,-1.,-2.33887832342782));
#54682=CARTESIAN_POINT('Ctrl Pts',(3.39918194577956,-1.,-2.33222789882489));
#54683=CARTESIAN_POINT('Ctrl Pts',(3.39513342019756,-1.,-2.3256034390248));
#54684=CARTESIAN_POINT('Ctrl Pts',(3.39105869474822,-1.,-2.31900513925424));
#54685=CARTESIAN_POINT('Ctrl Pts',(3.38695751492462,-1.,-2.31243319489367));
#54686=CARTESIAN_POINT('Ctrl Pts',(3.3828296733661,-1.,-2.30588783640343));
#54687=CARTESIAN_POINT('Ctrl Pts',(3.37867504959433,-1.,-2.29936936127624));
#54688=CARTESIAN_POINT('Ctrl Pts',(3.37449367172826,-1.,-2.29287818007393));
#54689=CARTESIAN_POINT('Ctrl Pts',(3.37028570206488,-1.,-2.28641481081137));
#54690=CARTESIAN_POINT('Ctrl Pts',(3.36605130713076,-1.,-2.27997979458037));
#54691=CARTESIAN_POINT('Ctrl Pts',(3.36179055004409,-1.,-2.2735736262093));
#54692=CARTESIAN_POINT('Ctrl Pts',(3.35750328523061,-1.,-2.2671966857991));
#54693=CARTESIAN_POINT('Ctrl Pts',(3.35318902552626,-1.,-2.26084915222449));
#54694=CARTESIAN_POINT('Ctrl Pts',(3.34884690292285,-1.,-2.25453097693483));
#54695=CARTESIAN_POINT('Ctrl Pts',(3.34447596770723,-1.,-2.24824207678256));
#54696=CARTESIAN_POINT('Ctrl Pts',(3.34007543738025,-1.,-2.24198249391422));
#54697=CARTESIAN_POINT('Ctrl Pts',(3.33564495756481,-1.,-2.23575256328812));
#54698=CARTESIAN_POINT('Ctrl Pts',(3.33118487773611,-1.,-2.22955308907233));
#54699=CARTESIAN_POINT('Ctrl Pts',(3.3266964672289,-1.,-2.22338548312772));
#54700=CARTESIAN_POINT('Ctrl Pts',(3.32218125618968,-1.,-2.21725135110898));
#54701=CARTESIAN_POINT('Ctrl Pts',(3.31764044024235,-1.,-2.21115211847875));
#54702=CARTESIAN_POINT('Ctrl Pts',(3.31307424608949,-1.,-2.20508863150607));
#54703=CARTESIAN_POINT('Ctrl Pts',(3.30848134694595,-1.,-2.19906078949923));
#54704=CARTESIAN_POINT('Ctrl Pts',(3.30385816281831,-1.,-2.19306710376111));
#54705=CARTESIAN_POINT('Ctrl Pts',(3.29920022557639,-1.,-2.18710556500327));
#54706=CARTESIAN_POINT('Ctrl Pts',(3.2945036150049,-1.,-2.18117455557065));
#54707=CARTESIAN_POINT('Ctrl Pts',(3.28976645712568,-1.,-2.17527380048423));
#54708=CARTESIAN_POINT('Ctrl Pts',(3.28499019979724,-1.,-2.16940517773455));
#54709=CARTESIAN_POINT('Ctrl Pts',(3.280181508414,-1.,-2.16357391934425));
#54710=CARTESIAN_POINT('Ctrl Pts',(3.27534954469187,-1.,-2.15778690038347));
#54711=CARTESIAN_POINT('Ctrl Pts',(3.27050245897228,-1.,-2.15205043199808));
#54712=CARTESIAN_POINT('Ctrl Pts',(3.26564388189759,-1.,-2.1463680529566));
#54713=CARTESIAN_POINT('Ctrl Pts',(3.26077002641879,-1.,-2.14073870754264));
#54714=CARTESIAN_POINT('Ctrl Pts',(3.25586495065054,-1.,-2.13515375878803));
#54715=CARTESIAN_POINT('Ctrl Pts',(3.25090574494028,-1.,-2.12960028396832));
#54716=CARTESIAN_POINT('Ctrl Pts',(3.24587102613376,-1.,-2.12406646410962));
#54717=CARTESIAN_POINT('Ctrl Pts',(3.24074905517293,-1.,-2.11854673326979));
#54718=CARTESIAN_POINT('Ctrl Pts',(3.23554444767099,-1.,-2.11304604021773));
#54719=CARTESIAN_POINT('Ctrl Pts',(3.23028945793289,-1.,-2.10758699642451));
#54720=CARTESIAN_POINT('Ctrl Pts',(3.22503437553434,-1.,-2.10220384298492));
#54721=CARTESIAN_POINT('Ctrl Pts',(3.21982707347009,-1.,-2.09692958434895));
#54722=CARTESIAN_POINT('Ctrl Pts',(3.21469429601654,-1.,-2.09178419460443));
#54723=CARTESIAN_POINT('Ctrl Pts',(3.20962575845463,-1.,-2.08676465517455));
#54724=CARTESIAN_POINT('Ctrl Pts',(3.2045481863073,-1.,-2.08182850370878));
#54725=CARTESIAN_POINT('Ctrl Pts',(3.19934132836019,-1.,-2.07690441870722));
#54726=CARTESIAN_POINT('Ctrl Pts',(3.19388465568252,-1.,-2.07192253497857));
#54727=CARTESIAN_POINT('Ctrl Pts',(3.18809755562368,-1.,-2.06684062744112));
#54728=CARTESIAN_POINT('Ctrl Pts',(3.18197692964614,-1.,-2.06166849827101));
#54729=CARTESIAN_POINT('Ctrl Pts',(3.17564906975371,-1.,-2.05650186773132));
#54730=CARTESIAN_POINT('Ctrl Pts',(3.16936341689527,-1.,-2.05151770247233));
#54731=CARTESIAN_POINT('Ctrl Pts',(3.16343165058912,-1.,-2.04693331247446));
#54732=CARTESIAN_POINT('Ctrl Pts',(3.15817983946367,-1.,-2.04297406404027));
#54733=CARTESIAN_POINT('Ctrl Pts',(3.15389991674792,-1.,-2.03984073791519));
#54734=CARTESIAN_POINT('Ctrl Pts',(3.15102344775328,-1.,-2.03783225495961));
#54735=CARTESIAN_POINT('Ctrl Pts',(3.14959882629805,-1.,-2.03693188810545));
#54736=CARTESIAN_POINT('Ctrl Pts',(3.1490119366901,-1.,-2.03663974554932));
#54737=CARTESIAN_POINT('Ctrl Pts',(3.14881939088124,-1.,-2.03659701539259));
#54738=CARTESIAN_POINT('Ctrl Pts',(3.14877060440327,-1.,-2.03660101169714));
#54739=CARTESIAN_POINT('',(3.24413672884812,-1.,-1.88097764062697));
#54740=CARTESIAN_POINT('Origin',(0.,-1.,0.));
#54741=CARTESIAN_POINT('',(3.70708211654725,-1.,-1.97421938526992));
#54742=CARTESIAN_POINT('Ctrl Pts',(3.24413672884812,-1.,-1.88097764062697));
#54743=CARTESIAN_POINT('Ctrl Pts',(3.24415531671284,-1.,-1.8810229239812));
#54744=CARTESIAN_POINT('Ctrl Pts',(3.24428080353022,-1.,-1.88117508446775));
#54745=CARTESIAN_POINT('Ctrl Pts',(3.24480754676064,-1.,-1.88156537699203));
#54746=CARTESIAN_POINT('Ctrl Pts',(3.2462565441079,-1.,-1.88242596600454));
#54747=CARTESIAN_POINT('Ctrl Pts',(3.24935200511918,-1.,-1.88407708646357));
#54748=CARTESIAN_POINT('Ctrl Pts',(3.25408686339463,-1.,-1.88646802523466));
#54749=CARTESIAN_POINT('Ctrl Pts',(3.25999885193947,-1.,-1.88934996203698));
#54750=CARTESIAN_POINT('Ctrl Pts',(3.26677653888676,-1.,-1.89255393500965));
#54751=CARTESIAN_POINT('Ctrl Pts',(3.27407108933139,-1.,-1.89589172903793));
#54752=CARTESIAN_POINT('Ctrl Pts',(3.28154737912352,-1.,-1.89918429230462));
#54753=CARTESIAN_POINT('Ctrl Pts',(3.2889344860029,-1.,-1.90228971247527));
#54754=CARTESIAN_POINT('Ctrl Pts',(3.29608978722113,-1.,-1.90513891864087));
#54755=CARTESIAN_POINT('Ctrl Pts',(3.30300595568195,-1.,-1.90773912171341));
#54756=CARTESIAN_POINT('Ctrl Pts',(3.30975721158596,-1.,-1.91014297830446));
#54757=CARTESIAN_POINT('Ctrl Pts',(3.31646052426364,-1.,-1.91242616234442));
#54758=CARTESIAN_POINT('Ctrl Pts',(3.32323403454535,-1.,-1.91466343916628));
#54759=CARTESIAN_POINT('Ctrl Pts',(3.33014884257873,-1.,-1.91690081930332));
#54760=CARTESIAN_POINT('Ctrl Pts',(3.33721230710012,-1.,-1.9191460961021));
#54761=CARTESIAN_POINT('Ctrl Pts',(3.34439448941961,-1.,-1.92138450828404));
#54762=CARTESIAN_POINT('Ctrl Pts',(3.35164424847223,-1.,-1.92358838440528));
#54763=CARTESIAN_POINT('Ctrl Pts',(3.35890824422965,-1.,-1.92572846125756));
#54764=CARTESIAN_POINT('Ctrl Pts',(3.36615168657567,-1.,-1.92778626543786));
#54765=CARTESIAN_POINT('Ctrl Pts',(3.37336807068043,-1.,-1.92975993109877));
#54766=CARTESIAN_POINT('Ctrl Pts',(3.3805676852555,-1.,-1.93165739093276));
#54767=CARTESIAN_POINT('Ctrl Pts',(3.38777076883256,-1.,-1.93349233176788));
#54768=CARTESIAN_POINT('Ctrl Pts',(3.39499923640795,-1.,-1.93527929945985));
#54769=CARTESIAN_POINT('Ctrl Pts',(3.40226802104109,-1.,-1.93702857723098));
#54770=CARTESIAN_POINT('Ctrl Pts',(3.40957978266642,-1.,-1.93874306008143));
#54771=CARTESIAN_POINT('Ctrl Pts',(3.41692971994096,-1.,-1.94042111965246));
#54772=CARTESIAN_POINT('Ctrl Pts',(3.42430850941503,-1.,-1.94205835913696));
#54773=CARTESIAN_POINT('Ctrl Pts',(3.43170586602434,-1.,-1.94364973660284));
#54774=CARTESIAN_POINT('Ctrl Pts',(3.43911410197687,-1.,-1.94519168842879));
#54775=CARTESIAN_POINT('Ctrl Pts',(3.44653088665681,-1.,-1.94668377715329));
#54776=CARTESIAN_POINT('Ctrl Pts',(3.45395731584051,-1.,-1.94812754766524));
#54777=CARTESIAN_POINT('Ctrl Pts',(3.46139661060962,-1.,-1.94952575850197));
#54778=CARTESIAN_POINT('Ctrl Pts',(3.46885258974191,-1.,-1.95088147859877));
#54779=CARTESIAN_POINT('Ctrl Pts',(3.47632820495921,-1.,-1.95219722189876));
#54780=CARTESIAN_POINT('Ctrl Pts',(3.48382414832634,-1.,-1.95347412486309));
#54781=CARTESIAN_POINT('Ctrl Pts',(3.49133956289133,-1.,-1.95471236969643));
#54782=CARTESIAN_POINT('Ctrl Pts',(3.49887263575583,-1.,-1.95591153823661));
#54783=CARTESIAN_POINT('Ctrl Pts',(3.50642124159909,-1.,-1.95707099606511));
#54784=CARTESIAN_POINT('Ctrl Pts',(3.51398354617794,-1.,-1.95819025316779));
#54785=CARTESIAN_POINT('Ctrl Pts',(3.52155867431486,-1.,-1.95926936324461));
#54786=CARTESIAN_POINT('Ctrl Pts',(3.52914648844351,-1.,-1.96030879411566));
#54787=CARTESIAN_POINT('Ctrl Pts',(3.53674730625813,-1.,-1.96130926212689));
#54788=CARTESIAN_POINT('Ctrl Pts',(3.54436163300443,-1.,-1.96227157573067));
#54789=CARTESIAN_POINT('Ctrl Pts',(3.55198990600886,-1.,-1.96319648628644));
#54790=CARTESIAN_POINT('Ctrl Pts',(3.55963218706096,-1.,-1.96408450906812));
#54791=CARTESIAN_POINT('Ctrl Pts',(3.56728820357791,-1.,-1.96493594634567));
#54792=CARTESIAN_POINT('Ctrl Pts',(3.57495748600959,-1.,-1.96575096652789));
#54793=CARTESIAN_POINT('Ctrl Pts',(3.58263947663829,-1.,-1.96652966688911));
#54794=CARTESIAN_POINT('Ctrl Pts',(3.59033364022801,-1.,-1.96727213799544));
#54795=CARTESIAN_POINT('Ctrl Pts',(3.59803959819938,-1.,-1.96797854118369));
#54796=CARTESIAN_POINT('Ctrl Pts',(3.60575714017989,-1.,-1.9686491188594));
#54797=CARTESIAN_POINT('Ctrl Pts',(3.61348615496704,-1.,-1.96928416040877));
#54798=CARTESIAN_POINT('Ctrl Pts',(3.62122658401893,-1.,-1.96988398129978));
#54799=CARTESIAN_POINT('Ctrl Pts',(3.62897836973293,-1.,-1.97044889850463));
#54800=CARTESIAN_POINT('Ctrl Pts',(3.63674139590412,-1.,-1.97097920454464));
#54801=CARTESIAN_POINT('Ctrl Pts',(3.64451546723514,-1.,-1.97147515441164));
#54802=CARTESIAN_POINT('Ctrl Pts',(3.652300347166,-1.,-1.9719369724024));
#54803=CARTESIAN_POINT('Ctrl Pts',(3.6600957816636,-1.,-1.9723648543905));
#54804=CARTESIAN_POINT('Ctrl Pts',(3.66790152752075,-1.,-1.97275897198678));
#54805=CARTESIAN_POINT('Ctrl Pts',(3.67571738107084,-1.,-1.97311947678517));
#54806=CARTESIAN_POINT('Ctrl Pts',(3.68354319915092,-1.,-1.97344650304519));
#54807=CARTESIAN_POINT('Ctrl Pts',(3.69137888599902,-1.,-1.97374016225483));
#54808=CARTESIAN_POINT('Ctrl Pts',(3.6976552856004,-1.,-1.97394846383216));
#54809=CARTESIAN_POINT('Ctrl Pts',(3.70236698912904,-1.,-1.97408973726715));
#54810=CARTESIAN_POINT('Ctrl Pts',(3.70551008132332,-1.,-1.97417727645308));
#54811=CARTESIAN_POINT('Ctrl Pts',(3.70708211654725,-1.,-1.97421938526992));
#54812=CARTESIAN_POINT('',(3.77614523045147,-1.,-1.83867539237861));
#54813=CARTESIAN_POINT('',(3.70708211654725,-1.,-1.97421938526992));
#54814=CARTESIAN_POINT('',(3.42859860294305,-1.,-1.5189508286633));
#54815=CARTESIAN_POINT('Ctrl Pts',(3.77614523045147,-1.,-1.83867539237861));
#54816=CARTESIAN_POINT('Ctrl Pts',(3.77518714457833,-1.,-1.83742834010626));
#54817=CARTESIAN_POINT('Ctrl Pts',(3.77326886064398,-1.,-1.83493697934534));
#54818=CARTESIAN_POINT('Ctrl Pts',(3.77038509817999,-1.,-1.83120816955646));
#54819=CARTESIAN_POINT('Ctrl Pts',(3.76652740353775,-1.,-1.82625289220915));
#54820=CARTESIAN_POINT('Ctrl Pts',(3.76168412707948,-1.,-1.82008629694091));
#54821=CARTESIAN_POINT('Ctrl Pts',(3.75681965683071,-1.,-1.8139472983358));
#54822=CARTESIAN_POINT('Ctrl Pts',(3.75193395887977,-1.,-1.80783603939617));
#54823=CARTESIAN_POINT('Ctrl Pts',(3.74702700875467,-1.,-1.8017527148577));
#54824=CARTESIAN_POINT('Ctrl Pts',(3.74209880352445,-1.,-1.79569757859422));
#54825=CARTESIAN_POINT('Ctrl Pts',(3.73714934730681,-1.,-1.78967092823491));
#54826=CARTESIAN_POINT('Ctrl Pts',(3.7321786309547,-1.,-1.78367308442901));
#54827=CARTESIAN_POINT('Ctrl Pts',(3.72718661205609,-1.,-1.77770437039658));
#54828=CARTESIAN_POINT('Ctrl Pts',(3.72217319911254,-1.,-1.77176509401761));
#54829=CARTESIAN_POINT('Ctrl Pts',(3.71713822377359,-1.,-1.76585552124394));
#54830=CARTESIAN_POINT('Ctrl Pts',(3.71208146346136,-1.,-1.75997588498865));
#54831=CARTESIAN_POINT('Ctrl Pts',(3.70700269736659,-1.,-1.75412641804042));
#54832=CARTESIAN_POINT('Ctrl Pts',(3.7019017567335,-1.,-1.74830738046057));
#54833=CARTESIAN_POINT('Ctrl Pts',(3.69677856910517,-1.,-1.74251908492617));
#54834=CARTESIAN_POINT('Ctrl Pts',(3.69163322648036,-1.,-1.73676193254557));
#54835=CARTESIAN_POINT('Ctrl Pts',(3.68646597019332,-1.,-1.73103640956717));
#54836=CARTESIAN_POINT('Ctrl Pts',(3.68127704936579,-1.,-1.72534302437056));
#54837=CARTESIAN_POINT('Ctrl Pts',(3.67606660374709,-1.,-1.71968225581808));
#54838=CARTESIAN_POINT('Ctrl Pts',(3.67083454901611,-1.,-1.71405450210384));
#54839=CARTESIAN_POINT('Ctrl Pts',(3.66558043198876,-1.,-1.70846001610956));
#54840=CARTESIAN_POINT('Ctrl Pts',(3.66030338774847,-1.,-1.70289888566873));
#54841=CARTESIAN_POINT('Ctrl Pts',(3.65500246526749,-1.,-1.69737117722534));
#54842=CARTESIAN_POINT('Ctrl Pts',(3.64967689827371,-1.,-1.69187705481689));
#54843=CARTESIAN_POINT('Ctrl Pts',(3.64432638915203,-1.,-1.68641690471457));
#54844=CARTESIAN_POINT('Ctrl Pts',(3.63895140887462,-1.,-1.68099146651586));
#54845=CARTESIAN_POINT('Ctrl Pts',(3.63355343201232,-1.,-1.67560193613156));
#54846=CARTESIAN_POINT('Ctrl Pts',(3.62813422105271,-1.,-1.67024966008045));
#54847=CARTESIAN_POINT('Ctrl Pts',(3.62269517989109,-1.,-1.66493585923855));
#54848=CARTESIAN_POINT('Ctrl Pts',(3.61723666482456,-1.,-1.65966133399186));
#54849=CARTESIAN_POINT('Ctrl Pts',(3.61175734965127,-1.,-1.65442619244325));
#54850=CARTESIAN_POINT('Ctrl Pts',(3.60625346556992,-1.,-1.64922952425832));
#54851=CARTESIAN_POINT('Ctrl Pts',(3.60072028513845,-1.,-1.64407004385582));
#54852=CARTESIAN_POINT('Ctrl Pts',(3.59515368334893,-1.,-1.63894676675352));
#54853=CARTESIAN_POINT('Ctrl Pts',(3.58955176627879,-1.,-1.6338597145126));
#54854=CARTESIAN_POINT('Ctrl Pts',(3.58391625774343,-1.,-1.62881051550745));
#54855=CARTESIAN_POINT('Ctrl Pts',(3.5782545595439,-1.,-1.62380329464844));
#54856=CARTESIAN_POINT('Ctrl Pts',(3.57257679609806,-1.,-1.61884340915404));
#54857=CARTESIAN_POINT('Ctrl Pts',(3.56689200468387,-1.,-1.61393581747514));
#54858=CARTESIAN_POINT('Ctrl Pts',(3.5612043248298,-1.,-1.60908344685457));
#54859=CARTESIAN_POINT('Ctrl Pts',(3.55550985096129,-1.,-1.60428584699853));
#54860=CARTESIAN_POINT('Ctrl Pts',(3.54979148634454,-1.,-1.59953698113457));
#54861=CARTESIAN_POINT('Ctrl Pts',(3.54402458182337,-1.,-1.59482766949766));
#54862=CARTESIAN_POINT('Ctrl Pts',(3.53818616861077,-1.,-1.59014958368739));
#54863=CARTESIAN_POINT('Ctrl Pts',(3.5322637814708,-1.,-1.58549906268088));
#54864=CARTESIAN_POINT('Ctrl Pts',(3.52626275334881,-1.,-1.58088027227848));
#54865=CARTESIAN_POINT('Ctrl Pts',(3.52021847865912,-1.,-1.57631049988158));
#54866=CARTESIAN_POINT('Ctrl Pts',(3.51418598431665,-1.,-1.57181569799743));
#54867=CARTESIAN_POINT('Ctrl Pts',(3.50821771695363,-1.,-1.56742097575012));
#54868=CARTESIAN_POINT('Ctrl Pts',(3.50234321621578,-1.,-1.56314187758675));
#54869=CARTESIAN_POINT('Ctrl Pts',(3.49655185179655,-1.,-1.55897703097874));
#54870=CARTESIAN_POINT('Ctrl Pts',(3.4907646087742,-1.,-1.55489595901116));
#54871=CARTESIAN_POINT('Ctrl Pts',(3.48485155928567,-1.,-1.55084702970452));
#54872=CARTESIAN_POINT('Ctrl Pts',(3.47868272898751,-1.,-1.54678009290276));
#54873=CARTESIAN_POINT('Ctrl Pts',(3.47217189224653,-1.,-1.54266605398188));
#54874=CARTESIAN_POINT('Ctrl Pts',(3.46531752207153,-1.,-1.53851507915502));
#54875=CARTESIAN_POINT('Ctrl Pts',(3.45825932955032,-1.,-1.53440195378792));
#54876=CARTESIAN_POINT('Ctrl Pts',(3.45127136828305,-1.,-1.53046244461635));
#54877=CARTESIAN_POINT('Ctrl Pts',(3.44469547526647,-1.,-1.52686242875556));
#54878=CARTESIAN_POINT('Ctrl Pts',(3.4388889597401,-1.,-1.5237734895035));
#54879=CARTESIAN_POINT('Ctrl Pts',(3.43417156977893,-1.,-1.52134826724293));
#54880=CARTESIAN_POINT('Ctrl Pts',(3.43101631893414,-1.,-1.5198144909338));
#54881=CARTESIAN_POINT('Ctrl Pts',(3.42946838852587,-1.,-1.51914806898491));
#54882=CARTESIAN_POINT('Ctrl Pts',(3.42884302333841,-1.,-1.5189513329503));
#54883=CARTESIAN_POINT('Ctrl Pts',(3.42864616361875,-1.,-1.51893924967331));
#54884=CARTESIAN_POINT('Ctrl Pts',(3.42859860294305,-1.,-1.5189508286633));
#54885=CARTESIAN_POINT('',(3.49844575334386,-1.,-1.35032489087269));
#54886=CARTESIAN_POINT('Origin',(0.,-1.,0.));
#54887=CARTESIAN_POINT('',(3.97027773754922,-1.,-1.36999806084572));
#54888=CARTESIAN_POINT('Ctrl Pts',(3.49844575334386,-1.,-1.35032489087269));
#54889=CARTESIAN_POINT('Ctrl Pts',(3.49847119623841,-1.,-1.35036670893102));
#54890=CARTESIAN_POINT('Ctrl Pts',(3.49861894124915,-1.,-1.35049736560633));
#54891=CARTESIAN_POINT('Ctrl Pts',(3.49920025459856,-1.,-1.35080045218652));
#54892=CARTESIAN_POINT('Ctrl Pts',(3.5007660381658,-1.,-1.35142377279535));
#54893=CARTESIAN_POINT('Ctrl Pts',(3.50408168106113,-1.,-1.3525703284343));
#54894=CARTESIAN_POINT('Ctrl Pts',(3.50913227060177,-1.,-1.35419113576022));
#54895=CARTESIAN_POINT('Ctrl Pts',(3.51542230699919,-1.,-1.35611275237288));
#54896=CARTESIAN_POINT('Ctrl Pts',(3.52261776117121,-1.,-1.35821701528975));
#54897=CARTESIAN_POINT('Ctrl Pts',(3.53034464961849,-1.,-1.36037259643827));
#54898=CARTESIAN_POINT('Ctrl Pts',(3.53824396425032,-1.,-1.36245507339334));
#54899=CARTESIAN_POINT('Ctrl Pts',(3.54602591832893,-1.,-1.36436666257568));
#54900=CARTESIAN_POINT('Ctrl Pts',(3.55353883995793,-1.,-1.36606145456711));
#54901=CARTESIAN_POINT('Ctrl Pts',(3.56077662028492,-1.,-1.36754771771174));
#54902=CARTESIAN_POINT('Ctrl Pts',(3.56782080304554,-1.,-1.36886584973349));
#54903=CARTESIAN_POINT('Ctrl Pts',(3.57479875549453,-1.,-1.37007229485646));
#54904=CARTESIAN_POINT('Ctrl Pts',(3.58183885982745,-1.,-1.37122241663073));
#54905=CARTESIAN_POINT('Ctrl Pts',(3.5890185384643,-1.,-1.37235053661));
#54906=CARTESIAN_POINT('Ctrl Pts',(3.59634627869117,-1.,-1.37346320103184));
#54907=CARTESIAN_POINT('Ctrl Pts',(3.60379020124038,-1.,-1.37455051379642));
#54908=CARTESIAN_POINT('Ctrl Pts',(3.61129546591082,-1.,-1.37559314436641));
#54909=CARTESIAN_POINT('Ctrl Pts',(3.61880481160408,-1.,-1.37657053403102));
#54910=CARTESIAN_POINT('Ctrl Pts',(3.62628098665112,-1.,-1.37746987919868));
#54911=CARTESIAN_POINT('Ctrl Pts',(3.63371727442448,-1.,-1.37829035457325));
#54912=CARTESIAN_POINT('Ctrl Pts',(3.64112507791112,-1.,-1.37903818567347));
#54913=CARTESIAN_POINT('Ctrl Pts',(3.64852652756444,-1.,-1.37972372481598));
#54914=CARTESIAN_POINT('Ctrl Pts',(3.65594554404396,-1.,-1.38035791051215));
#54915=CARTESIAN_POINT('Ctrl Pts',(3.66339848520874,-1.,-1.38094856333558));
#54916=CARTESIAN_POINT('Ctrl Pts',(3.67088843112282,-1.,-1.38149812653876));
#54917=CARTESIAN_POINT('Ctrl Pts',(3.6784103848243,-1.,-1.38200574290626));
#54918=CARTESIAN_POINT('Ctrl Pts',(3.68595444983844,-1.,-1.38246852827185));
#54919=CARTESIAN_POINT('Ctrl Pts',(3.69350967899523,-1.,-1.38288311171649));
#54920=CARTESIAN_POINT('Ctrl Pts',(3.70106792167894,-1.,-1.38324717612862));
#54921=CARTESIAN_POINT('Ctrl Pts',(3.70862680753343,-1.,-1.38356065402122));
#54922=CARTESIAN_POINT('Ctrl Pts',(3.7161876605181,-1.,-1.38382489984585));
#54923=CARTESIAN_POINT('Ctrl Pts',(3.72375409358805,-1.,-1.3840421342895));
#54924=CARTESIAN_POINT('Ctrl Pts',(3.73133035859283,-1.,-1.38421479111531));
#54925=CARTESIAN_POINT('Ctrl Pts',(3.73891976418099,-1.,-1.38434489156456));
#54926=CARTESIAN_POINT('Ctrl Pts',(3.7465231716786,-1.,-1.38443344984389));
#54927=CARTESIAN_POINT('Ctrl Pts',(3.75413976318727,-1.,-1.38448077997155));
#54928=CARTESIAN_POINT('Ctrl Pts',(3.76176768271347,-1.,-1.38448675253343));
#54929=CARTESIAN_POINT('Ctrl Pts',(3.76940473185775,-1.,-1.38445107339517));
#54930=CARTESIAN_POINT('Ctrl Pts',(3.77704902230441,-1.,-1.38437354551435));
#54931=CARTESIAN_POINT('Ctrl Pts',(3.78469969805134,-1.,-1.38425435883773));
#54932=CARTESIAN_POINT('Ctrl Pts',(3.79235669640907,-1.,-1.38409399694589));
#54933=CARTESIAN_POINT('Ctrl Pts',(3.80002044322169,-1.,-1.38389311766701));
#54934=CARTESIAN_POINT('Ctrl Pts',(3.80769156398429,-1.,-1.38365244046226));
#54935=CARTESIAN_POINT('Ctrl Pts',(3.81537060817765,-1.,-1.38337263902766));
#54936=CARTESIAN_POINT('Ctrl Pts',(3.82305771743715,-1.,-1.38305421262724));
#54937=CARTESIAN_POINT('Ctrl Pts',(3.83075266982138,-1.,-1.38269750245086));
#54938=CARTESIAN_POINT('Ctrl Pts',(3.83845502790609,-1.,-1.38230274828774));
#54939=CARTESIAN_POINT('Ctrl Pts',(3.84616425605705,-1.,-1.38187013346089));
#54940=CARTESIAN_POINT('Ctrl Pts',(3.85387983979557,-1.,-1.38139983115075));
#54941=CARTESIAN_POINT('Ctrl Pts',(3.86160143044187,-1.,-1.38089205993068));
#54942=CARTESIAN_POINT('Ctrl Pts',(3.86932885813403,-1.,-1.38034709213129));
#54943=CARTESIAN_POINT('Ctrl Pts',(3.87706205830865,-1.,-1.37976523097187));
#54944=CARTESIAN_POINT('Ctrl Pts',(3.88480102249461,-1.,-1.37914679719446));
#54945=CARTESIAN_POINT('Ctrl Pts',(3.89254574338385,-1.,-1.37849211287981));
#54946=CARTESIAN_POINT('Ctrl Pts',(3.90029615196255,-1.,-1.3778014851263));
#54947=CARTESIAN_POINT('Ctrl Pts',(3.90805209522729,-1.,-1.3770751963376));
#54948=CARTESIAN_POINT('Ctrl Pts',(3.91581337461825,-1.,-1.37631350505516));
#54949=CARTESIAN_POINT('Ctrl Pts',(3.92357976987132,-1.,-1.37551664448057));
#54950=CARTESIAN_POINT('Ctrl Pts',(3.93135106761941,-1.,-1.37468482215784));
#54951=CARTESIAN_POINT('Ctrl Pts',(3.93912709041791,-1.,-1.37381821967499));
#54952=CARTESIAN_POINT('Ctrl Pts',(3.94690771786926,-1.,-1.37291699203423));
#54953=CARTESIAN_POINT('Ctrl Pts',(3.95469287283105,-1.,-1.37198126433139));
#54954=CARTESIAN_POINT('Ctrl Pts',(3.96092458508407,-1.,-1.37120515615663));
#54955=CARTESIAN_POINT('Ctrl Pts',(3.96560037975788,-1.,-1.37060761746027));
#54956=CARTESIAN_POINT('Ctrl Pts',(3.9687184694173,-1.,-1.37020239094758));
#54957=CARTESIAN_POINT('Ctrl Pts',(3.97027773754922,-1.,-1.36999806084572));
#54958=CARTESIAN_POINT('',(4.01728681790024,-1.,-1.22531898815164));
#54959=CARTESIAN_POINT('',(3.97027773754922,-1.,-1.36999806084572));
#54960=CARTESIAN_POINT('',(3.62400312501199,-1.,-0.963899035118986));
#54961=CARTESIAN_POINT('Ctrl Pts',(4.01728681790024,-1.,-1.22531898815164));
#54962=CARTESIAN_POINT('Ctrl Pts',(4.01614544569895,-1.,-1.22423716681317));
#54963=CARTESIAN_POINT('Ctrl Pts',(4.01386104433519,-1.,-1.22207656455845));
#54964=CARTESIAN_POINT('Ctrl Pts',(4.01042947140789,-1.,-1.21884478244403));
#54965=CARTESIAN_POINT('Ctrl Pts',(4.00584409522722,-1.,-1.21455398918133));
#54966=CARTESIAN_POINT('Ctrl Pts',(4.00009577950721,-1.,-1.20922097029551));
#54967=CARTESIAN_POINT('Ctrl Pts',(3.99433084799666,-1.,-1.20391852375139));
#54968=CARTESIAN_POINT('Ctrl Pts',(3.98854928957189,-1.,-1.19864679609566));
#54969=CARTESIAN_POINT('Ctrl Pts',(3.98275111052561,-1.,-1.19340598349475));
#54970=CARTESIAN_POINT('Ctrl Pts',(3.97693634767754,-1.,-1.18819633715539));
#54971=CARTESIAN_POINT('Ctrl Pts',(3.97110505165415,-1.,-1.18301815039831));
#54972=CARTESIAN_POINT('Ctrl Pts',(3.96525726358159,-1.,-1.17787174135592));
#54973=CARTESIAN_POINT('Ctrl Pts',(3.95939299213276,-1.,-1.17275743590361));
#54974=CARTESIAN_POINT('Ctrl Pts',(3.95351219509876,-1.,-1.16767555244438));
#54975=CARTESIAN_POINT('Ctrl Pts',(3.94761474780583,-1.,-1.16262637999157));
#54976=CARTESIAN_POINT('Ctrl Pts',(3.94170046685203,-1.,-1.15761018340956));
#54977=CARTESIAN_POINT('Ctrl Pts',(3.9357691705628,-1.,-1.1526272271632));
#54978=CARTESIAN_POINT('Ctrl Pts',(3.92982073294257,-1.,-1.14767779451124));
#54979=CARTESIAN_POINT('Ctrl Pts',(3.92385513133997,-1.,-1.14276220561593));
#54980=CARTESIAN_POINT('Ctrl Pts',(3.91787251936827,-1.,-1.13788084225554));
#54981=CARTESIAN_POINT('Ctrl Pts',(3.91187321145649,-1.,-1.13303414693896));
#54982=CARTESIAN_POINT('Ctrl Pts',(3.90585753318737,-1.,-1.12822258281553));
#54983=CARTESIAN_POINT('Ctrl Pts',(3.89982569750025,-1.,-1.12344660099043));
#54984=CARTESIAN_POINT('Ctrl Pts',(3.89377768340344,-1.,-1.11870660794603));
#54985=CARTESIAN_POINT('Ctrl Pts',(3.88771308285171,-1.,-1.11400292434429));
#54986=CARTESIAN_POINT('Ctrl Pts',(3.88163105531724,-1.,-1.10933577224008));
#54987=CARTESIAN_POINT('Ctrl Pts',(3.87553067187514,-1.,-1.10470536603287));
#54988=CARTESIAN_POINT('Ctrl Pts',(3.86941120134849,-1.,-1.10011198761195));
#54989=CARTESIAN_POINT('Ctrl Pts',(3.86327241021247,-1.,-1.09555606505013));
#54990=CARTESIAN_POINT('Ctrl Pts',(3.85711487933931,-1.,-1.09103825516294));
#54991=CARTESIAN_POINT('Ctrl Pts',(3.85094025222713,-1.,-1.08655950846384));
#54992=CARTESIAN_POINT('Ctrl Pts',(3.8447504803063,-1.,-1.08212087917991));
#54993=CARTESIAN_POINT('Ctrl Pts',(3.83854714117491,-1.,-1.07772335353858));
#54994=CARTESIAN_POINT('Ctrl Pts',(3.83233071195144,-1.,-1.07336766633459));
#54995=CARTESIAN_POINT('Ctrl Pts',(3.82609989967276,-1.,-1.06905413180359));
#54996=CARTESIAN_POINT('Ctrl Pts',(3.81985083953012,-1.,-1.0647824403893));
#54997=CARTESIAN_POINT('Ctrl Pts',(3.8135786611749,-1.,-1.06055206187299));
#54998=CARTESIAN_POINT('Ctrl Pts',(3.80727913637791,-1.,-1.05636266918644));
#54999=CARTESIAN_POINT('Ctrl Pts',(3.80095039790681,-1.,-1.05221457990016));
#55000=CARTESIAN_POINT('Ctrl Pts',(3.79459440308786,-1.,-1.04810913267639));
#55001=CARTESIAN_POINT('Ctrl Pts',(3.78821910787179,-1.,-1.04404924374422));
#55002=CARTESIAN_POINT('Ctrl Pts',(3.7818353500817,-1.,-1.04003862055798));
#55003=CARTESIAN_POINT('Ctrl Pts',(3.77545283140427,-1.,-1.03608074678008));
#55004=CARTESIAN_POINT('Ctrl Pts',(3.76907609832516,-1.,-1.03217786604919));
#55005=CARTESIAN_POINT('Ctrl Pts',(3.76270122291245,-1.,-1.02833014458184));
#55006=CARTESIAN_POINT('Ctrl Pts',(3.75631037456224,-1.,-1.02453429444668));
#55007=CARTESIAN_POINT('Ctrl Pts',(3.74987777155873,-1.,-1.02078510487439));
#55008=CARTESIAN_POINT('Ctrl Pts',(3.74337942504993,-1.,-1.01707794311088));
#55009=CARTESIAN_POINT('Ctrl Pts',(3.73680245055747,-1.,-1.01341114319906));
#55010=CARTESIAN_POINT('Ctrl Pts',(3.73015276704407,-1.,-1.00978798539491));
#55011=CARTESIAN_POINT('Ctrl Pts',(3.72346803750544,-1.,-1.00622000735696));
#55012=CARTESIAN_POINT('Ctrl Pts',(3.71680667125047,-1.,-1.00272423396802));
#55013=CARTESIAN_POINT('Ctrl Pts',(3.7102243971387,-1.,-0.999317260756345));
#55014=CARTESIAN_POINT('Ctrl Pts',(3.70375282282107,-1.,-0.996009819772432));
#55015=CARTESIAN_POINT('Ctrl Pts',(3.69738123415696,-1.,-0.992802218332104));
#55016=CARTESIAN_POINT('Ctrl Pts',(3.69102682138955,-1.,-0.989676715398859));
#55017=CARTESIAN_POINT('Ctrl Pts',(3.6845531792623,-1.,-0.986602639864286));
#55018=CARTESIAN_POINT('Ctrl Pts',(3.67782408841876,-1.,-0.983550791470865));
#55019=CARTESIAN_POINT('Ctrl Pts',(3.67074983340444,-1.,-0.980505922458495));
#55020=CARTESIAN_POINT('Ctrl Pts',(3.66333049637403,-1.,-0.977478312751416));
#55021=CARTESIAN_POINT('Ctrl Pts',(3.6557157673487,-1.,-0.974519971354139));
#55022=CARTESIAN_POINT('Ctrl Pts',(3.64819756447072,-1.,-0.971722122060278));
#55023=CARTESIAN_POINT('Ctrl Pts',(3.64113946505393,-1.,-0.969195124674829));
#55024=CARTESIAN_POINT('Ctrl Pts',(3.6349212208096,-1.,-0.967052554540878));
#55025=CARTESIAN_POINT('Ctrl Pts',(3.62988252139998,-1.,-0.965395153165716));
#55026=CARTESIAN_POINT('Ctrl Pts',(3.62652618145252,-1.,-0.964373850166081));
#55027=CARTESIAN_POINT('Ctrl Pts',(3.62489305727516,-1.,-0.963957782642589));
#55028=CARTESIAN_POINT('Ctrl Pts',(3.62424461507455,-1.,-0.963861297423579));
#55029=CARTESIAN_POINT('Ctrl Pts',(3.62404828878374,-1.,-0.963880158556713));
#55030=CARTESIAN_POINT('Ctrl Pts',(3.62400312501199,-1.,-0.963899035118986));
#55031=CARTESIAN_POINT('',(3.66661143271648,-1.,-0.786422660833743));
#55032=CARTESIAN_POINT('Origin',(0.,-1.,0.));
#55033=CARTESIAN_POINT('',(4.13571194405636,-1.,-0.73204283740062));
#55034=CARTESIAN_POINT('Ctrl Pts',(3.66661143271648,-1.,-0.786422660833743));
#55035=CARTESIAN_POINT('Ctrl Pts',(3.66664310415236,-1.,-0.786459983896781));
#55036=CARTESIAN_POINT('Ctrl Pts',(3.66680946938396,-1.,-0.78656591955989));
#55037=CARTESIAN_POINT('Ctrl Pts',(3.66743103898844,-1.,-0.7867743371985));
#55038=CARTESIAN_POINT('Ctrl Pts',(3.66907505398769,-1.,-0.787145041181589));
#55039=CARTESIAN_POINT('Ctrl Pts',(3.672529236635,-1.,-0.787758799995427));
#55040=CARTESIAN_POINT('Ctrl Pts',(3.67777119516438,-1.,-0.788569566220663));
#55041=CARTESIAN_POINT('Ctrl Pts',(3.68428439784285,-1.,-0.789483546065159));
#55042=CARTESIAN_POINT('Ctrl Pts',(3.69172044327754,-1.,-0.79043628498958));
#55043=CARTESIAN_POINT('Ctrl Pts',(3.69968940808982,-1.,-0.791356575696509));
#55044=CARTESIAN_POINT('Ctrl Pts',(3.70781724021879,-1.,-0.792177688845968));
#55045=CARTESIAN_POINT('Ctrl Pts',(3.7158024239604,-1.,-0.792848377370116));
#55046=CARTESIAN_POINT('Ctrl Pts',(3.7234879729357,-1.,-0.793347023783871));
#55047=CARTESIAN_POINT('Ctrl Pts',(3.7308691469564,-1.,-0.793682750269348));
#55048=CARTESIAN_POINT('Ctrl Pts',(3.73803280541576,-1.,-0.793882700936791));
#55049=CARTESIAN_POINT('Ctrl Pts',(3.74511357728827,-1.,-0.79398270045988));
#55050=CARTESIAN_POINT('Ctrl Pts',(3.75224692493895,-1.,-0.794017347371441));
#55051=CARTESIAN_POINT('Ctrl Pts',(3.75951468666325,-1.,-0.794008429135047));
#55052=CARTESIAN_POINT('Ctrl Pts',(3.76692626931184,-1.,-0.793961083689141));
#55053=CARTESIAN_POINT('Ctrl Pts',(3.77444863801264,-1.,-0.793870523787515));
#55054=CARTESIAN_POINT('Ctrl Pts',(3.78202460377617,-1.,-0.79372623578134));
#55055=CARTESIAN_POINT('Ctrl Pts',(3.78959439439222,-1.,-0.793516871680966));
#55056=CARTESIAN_POINT('Ctrl Pts',(3.79711921389862,-1.,-0.793235612973201));
#55057=CARTESIAN_POINT('Ctrl Pts',(3.80459229925598,-1.,-0.792882695234693));
#55058=CARTESIAN_POINT('Ctrl Pts',(3.81202588694726,-1.,-0.792462483517568));
#55059=CARTESIAN_POINT('Ctrl Pts',(3.81944345442237,-1.,-0.791981740718607));
#55060=CARTESIAN_POINT('Ctrl Pts',(3.82687033899799,-1.,-0.791447528662381));
#55061=CARTESIAN_POINT('Ctrl Pts',(3.83432392054804,-1.,-0.79086501270534));
#55062=CARTESIAN_POINT('Ctrl Pts',(3.84180762342476,-1.,-0.790236124191289));
#55063=CARTESIAN_POINT('Ctrl Pts',(3.8493163780891,-1.,-0.789560798155619));
#55064=CARTESIAN_POINT('Ctrl Pts',(3.85683995872536,-1.,-0.788837734090688));
#55065=CARTESIAN_POINT('Ctrl Pts',(3.86436702561342,-1.,-0.788065315093771));
#55066=CARTESIAN_POINT('Ctrl Pts',(3.87188916600905,-1.,-0.787242527617981));
#55067=CARTESIAN_POINT('Ctrl Pts',(3.87940402818186,-1.,-0.786369675812592));
#55068=CARTESIAN_POINT('Ctrl Pts',(3.88691313167399,-1.,-0.785447890340723));
#55069=CARTESIAN_POINT('Ctrl Pts',(3.89442039235105,-1.,-0.784478799358336));
#55070=CARTESIAN_POINT('Ctrl Pts',(3.90193039043971,-1.,-0.783464141529083));
#55071=CARTESIAN_POINT('Ctrl Pts',(3.90944671004536,-1.,-0.782405395622759));
#55072=CARTESIAN_POINT('Ctrl Pts',(3.9169703605466,-1.,-0.781303428618344));
#55073=CARTESIAN_POINT('Ctrl Pts',(3.92450058323799,-1.,-0.780158678615507));
#55074=CARTESIAN_POINT('Ctrl Pts',(3.93203552473153,-1.,-0.778971308134786));
#55075=CARTESIAN_POINT('Ctrl Pts',(3.93957296768098,-1.,-0.77774137056855));
#55076=CARTESIAN_POINT('Ctrl Pts',(3.94711101619471,-1.,-0.77646896669796));
#55077=CARTESIAN_POINT('Ctrl Pts',(3.95464885452364,-1.,-0.775154418039442));
#55078=CARTESIAN_POINT('Ctrl Pts',(3.96218649639876,-1.,-0.773798212026683));
#55079=CARTESIAN_POINT('Ctrl Pts',(3.96972446532832,-1.,-0.772400931772239));
#55080=CARTESIAN_POINT('Ctrl Pts',(3.97726349165507,-1.,-0.770963190030504));
#55081=CARTESIAN_POINT('Ctrl Pts',(3.98480422348403,-1.,-0.76948556624546));
#55082=CARTESIAN_POINT('Ctrl Pts',(3.99234687880892,-1.,-0.767968531377708));
#55083=CARTESIAN_POINT('Ctrl Pts',(3.99989129179464,-1.,-0.766412457135786));
#55084=CARTESIAN_POINT('Ctrl Pts',(4.00743706791366,-1.,-0.764817648784947));
#55085=CARTESIAN_POINT('Ctrl Pts',(4.01498370680434,-1.,-0.763184371182827));
#55086=CARTESIAN_POINT('Ctrl Pts',(4.02253072741347,-1.,-0.761512875859942));
#55087=CARTESIAN_POINT('Ctrl Pts',(4.0300778195465,-1.,-0.759803433244166));
#55088=CARTESIAN_POINT('Ctrl Pts',(4.03762485803468,-1.,-0.758056338885554));
#55089=CARTESIAN_POINT('Ctrl Pts',(4.04517182654344,-1.,-0.756271902370187));
#55090=CARTESIAN_POINT('Ctrl Pts',(4.05271876688106,-1.,-0.754450441816412));
#55091=CARTESIAN_POINT('Ctrl Pts',(4.06026572221399,-1.,-0.752592276482869));
#55092=CARTESIAN_POINT('Ctrl Pts',(4.06781267241886,-1.,-0.750697720483176));
#55093=CARTESIAN_POINT('Ctrl Pts',(4.07535951055363,-1.,-0.748767076679177));
#55094=CARTESIAN_POINT('Ctrl Pts',(4.08290608094789,-1.,-0.746800631490822));
#55095=CARTESIAN_POINT('Ctrl Pts',(4.09045220253011,-1.,-0.744798649705514));
#55096=CARTESIAN_POINT('Ctrl Pts',(4.09799769702712,-1.,-0.742761369690018));
#55097=CARTESIAN_POINT('Ctrl Pts',(4.1055424175856,-1.,-0.740688998555152));
#55098=CARTESIAN_POINT('Ctrl Pts',(4.11308626953795,-1.,-0.738581708229119));
#55099=CARTESIAN_POINT('Ctrl Pts',(4.12062919626082,-1.,-0.736439634335347));
#55100=CARTESIAN_POINT('Ctrl Pts',(4.12666277572794,-1.,-0.734698226767513));
#55101=CARTESIAN_POINT('Ctrl Pts',(4.13118752796397,-1.,-0.733376589325634));
#55102=CARTESIAN_POINT('Ctrl Pts',(4.13420383737278,-1.,-0.732488575135926));
#55103=CARTESIAN_POINT('Ctrl Pts',(4.13571194405636,-1.,-0.73204283740062));
#55104=CARTESIAN_POINT('',(4.15950947128175,-1.,-0.581791163835815));
#55105=CARTESIAN_POINT('',(4.13571194405636,-1.,-0.73204283740062));
#55106=CARTESIAN_POINT('',(3.73017266276632,-1.,-0.385112848332549));
#55107=CARTESIAN_POINT('Ctrl Pts',(4.15950947128175,-1.,-0.581791163835815));
#55108=CARTESIAN_POINT('Ctrl Pts',(4.15821291712391,-1.,-0.580901211462913));
#55109=CARTESIAN_POINT('Ctrl Pts',(4.15561864787379,-1.,-0.579124568912544));
#55110=CARTESIAN_POINT('Ctrl Pts',(4.1517237611974,-1.,-0.576469391673917));
#55111=CARTESIAN_POINT('Ctrl Pts',(4.14652361065787,-1.,-0.572948736066277));
#55112=CARTESIAN_POINT('Ctrl Pts',(4.14001179828669,-1.,-0.568580610187116));
#55113=CARTESIAN_POINT('Ctrl Pts',(4.13348835726086,-1.,-0.564245279535706));
#55114=CARTESIAN_POINT('Ctrl Pts',(4.12695329951859,-1.,-0.559942890594628));
#55115=CARTESIAN_POINT('Ctrl Pts',(4.1204066619623,-1.,-0.555673636130778));
#55116=CARTESIAN_POINT('Ctrl Pts',(4.11384852025578,-1.,-0.551437758498247));
#55117=CARTESIAN_POINT('Ctrl Pts',(4.1072789702877,-1.,-0.54723553948676));
#55118=CARTESIAN_POINT('Ctrl Pts',(4.10069810244473,-1.,-0.543067286878457));
#55119=CARTESIAN_POINT('Ctrl Pts',(4.09410597627116,-1.,-0.538933321179921));
#55120=CARTESIAN_POINT('Ctrl Pts',(4.08750259988693,-1.,-0.534833963477));
#55121=CARTESIAN_POINT('Ctrl Pts',(4.08088789536488,-1.,-0.530769518728076));
#55122=CARTESIAN_POINT('Ctrl Pts',(4.07426172299496,-1.,-0.526740277227));
#55123=CARTESIAN_POINT('Ctrl Pts',(4.06762394471075,-1.,-0.522746528602768));
#55124=CARTESIAN_POINT('Ctrl Pts',(4.06097448037934,-1.,-0.51878857233681));
#55125=CARTESIAN_POINT('Ctrl Pts',(4.05431335771261,-1.,-0.514866728193104));
#55126=CARTESIAN_POINT('Ctrl Pts',(4.04764078815591,-1.,-0.510981349219174));
#55127=CARTESIAN_POINT('Ctrl Pts',(4.04095715149074,-1.,-0.507132823288362));
#55128=CARTESIAN_POINT('Ctrl Pts',(4.0342628417439,-1.,-0.503321556915514));
#55129=CARTESIAN_POINT('Ctrl Pts',(4.0275581398015,-1.,-0.49954796234089));
#55130=CARTESIAN_POINT('Ctrl Pts',(4.02084308851813,-1.,-0.495812444326223));
#55131=CARTESIAN_POINT('Ctrl Pts',(4.01411733503486,-1.,-0.492115383417931));
#55132=CARTESIAN_POINT('Ctrl Pts',(4.0073800839092,-1.,-0.488457130424531));
#55133=CARTESIAN_POINT('Ctrl Pts',(4.00063045119234,-1.,-0.484838042421754));
#55134=CARTESIAN_POINT('Ctrl Pts',(3.99386775880655,-1.,-0.481258512209638));
#55135=CARTESIAN_POINT('Ctrl Pts',(3.98709184306743,-1.,-0.477718999122033));
#55136=CARTESIAN_POINT('Ctrl Pts',(3.9803033804443,-1.,-0.474220061019542));
#55137=CARTESIAN_POINT('Ctrl Pts',(3.97350414289415,-1.,-0.470762379613478));
#55138=CARTESIAN_POINT('Ctrl Pts',(3.96669622273946,-1.,-0.467346690880672));
#55139=CARTESIAN_POINT('Ctrl Pts',(3.95988133243543,-1.,-0.463973722115745));
#55140=CARTESIAN_POINT('Ctrl Pts',(3.95306005817363,-1.,-0.460644124429119));
#55141=CARTESIAN_POINT('Ctrl Pts',(3.94623117206675,-1.,-0.457358410451674));
#55142=CARTESIAN_POINT('Ctrl Pts',(3.93939080846298,-1.,-0.454116879027576));
#55143=CARTESIAN_POINT('Ctrl Pts',(3.93253407403128,-1.,-0.450919768356347));
#55144=CARTESIAN_POINT('Ctrl Pts',(3.92565674143424,-1.,-0.447767416837297));
#55145=CARTESIAN_POINT('Ctrl Pts',(3.91875701610721,-1.,-0.444660430230593));
#55146=CARTESIAN_POINT('Ctrl Pts',(3.91183704069146,-1.,-0.441599824524048));
#55147=CARTESIAN_POINT('Ctrl Pts',(3.90490512938546,-1.,-0.438587235458234));
#55148=CARTESIAN_POINT('Ctrl Pts',(3.8979725665544,-1.,-0.435624629433506));
#55149=CARTESIAN_POINT('Ctrl Pts',(3.89104947940592,-1.,-0.43271392954444));
#55150=CARTESIAN_POINT('Ctrl Pts',(3.88414070943334,-1.,-0.429856640579734));
#55151=CARTESIAN_POINT('Ctrl Pts',(3.87724240306609,-1.,-0.427053541173469));
#55152=CARTESIAN_POINT('Ctrl Pts',(3.87033643487882,-1.,-0.424304173195143));
#55153=CARTESIAN_POINT('Ctrl Pts',(3.86339652542749,-1.,-0.421607423177576));
#55154=CARTESIAN_POINT('Ctrl Pts',(3.85639825648031,-1.,-0.41896246808681));
#55155=CARTESIAN_POINT('Ctrl Pts',(3.8493286415751,-1.,-0.41636967805292));
#55156=CARTESIAN_POINT('Ctrl Pts',(3.84219403994742,-1.,-0.413831367016727));
#55157=CARTESIAN_POINT('Ctrl Pts',(3.83503345578645,-1.,-0.41135303879846));
#55158=CARTESIAN_POINT('Ctrl Pts',(3.82790724256397,-1.,-0.408942371447377));
#55159=CARTESIAN_POINT('Ctrl Pts',(3.82087303913741,-1.,-0.406607038258907));
#55160=CARTESIAN_POINT('Ctrl Pts',(3.81396374287762,-1.,-0.404352694628237));
#55161=CARTESIAN_POINT('Ctrl Pts',(3.80716881962763,-1.,-0.402181320148475));
#55162=CARTESIAN_POINT('Ctrl Pts',(3.80040370384659,-1.,-0.400088346504727));
#55163=CARTESIAN_POINT('Ctrl Pts',(3.79352887163457,-1.,-0.398064818684159));
#55164=CARTESIAN_POINT('Ctrl Pts',(3.78640521279479,-1.,-0.396103205335029));
#55165=CARTESIAN_POINT('Ctrl Pts',(3.77894173114368,-1.,-0.394202481011595));
#55166=CARTESIAN_POINT('Ctrl Pts',(3.77114011595892,-1.,-0.392372786223347));
#55167=CARTESIAN_POINT('Ctrl Pts',(3.76315635032993,-1.,-0.390642072979259));
#55168=CARTESIAN_POINT('Ctrl Pts',(3.75529302894757,-1.,-0.389054775898251));
#55169=CARTESIAN_POINT('Ctrl Pts',(3.74792651696269,-1.,-0.387663020050396));
#55170=CARTESIAN_POINT('Ctrl Pts',(3.74144965781088,-1.,-0.386519576222036));
#55171=CARTESIAN_POINT('Ctrl Pts',(3.73621371845475,-1.,-0.385670806454744));
#55172=CARTESIAN_POINT('Ctrl Pts',(3.73273893363318,-1.,-0.385187124633965));
#55173=CARTESIAN_POINT('Ctrl Pts',(3.73106082862399,-1.,-0.385031656499142));
#55174=CARTESIAN_POINT('Ctrl Pts',(3.73040527620929,-1.,-0.385037797882046));
#55175=CARTESIAN_POINT('Ctrl Pts',(3.73021431755218,-1.,-0.385087139001609));
#55176=CARTESIAN_POINT('Ctrl Pts',(3.73017266276632,-1.,-0.385112848332549));
#55177=CARTESIAN_POINT('',(3.74449296982994,-1.,-0.203156094897896));
#55178=CARTESIAN_POINT('Origin',(0.,-1.,0.));
#55179=CARTESIAN_POINT('',(4.19931119685982,-1.,-0.0760622897878241));
#55180=CARTESIAN_POINT('Ctrl Pts',(3.74449296982994,-1.,-0.203156094897896));
#55181=CARTESIAN_POINT('Ctrl Pts',(3.74453008995129,-1.,-0.203188003947965));
#55182=CARTESIAN_POINT('Ctrl Pts',(3.74471097893961,-1.,-0.203266610111264));
#55183=CARTESIAN_POINT('Ctrl Pts',(3.74535749969262,-1.,-0.203375226874332));
#55184=CARTESIAN_POINT('Ctrl Pts',(3.74703926501843,-1.,-0.203484186269315));
#55185=CARTESIAN_POINT('Ctrl Pts',(3.75054693397716,-1.,-0.203550035479097));
#55186=CARTESIAN_POINT('Ctrl Pts',(3.75585118707924,-1.,-0.203530796848404));
#55187=CARTESIAN_POINT('Ctrl Pts',(3.76242717937273,-1.,-0.203414634707647));
#55188=CARTESIAN_POINT('Ctrl Pts',(3.76992071595267,-1.,-0.203192390045338));
#55189=CARTESIAN_POINT('Ctrl Pts',(3.77793553476879,-1.,-0.202854729699197));
#55190=CARTESIAN_POINT('Ctrl Pts',(3.78609175019317,-1.,-0.202394260512193));
#55191=CARTESIAN_POINT('Ctrl Pts',(3.79408354187274,-1.,-0.201807533800799));
#55192=CARTESIAN_POINT('Ctrl Pts',(3.80175247447171,-1.,-0.201097756307252));
#55193=CARTESIAN_POINT('Ctrl Pts',(3.80909529318501,-1.,-0.20027467943329));
#55194=CARTESIAN_POINT('Ctrl Pts',(3.81620203429702,-1.,-0.199351525297397));
#55195=CARTESIAN_POINT('Ctrl Pts',(3.82321127348981,-1.,-0.19834261690047));
#55196=CARTESIAN_POINT('Ctrl Pts',(3.83026221776488,-1.,-0.197260935827375));
#55197=CARTESIAN_POINT('Ctrl Pts',(3.83743910616265,-1.,-0.19611519897189));
#55198=CARTESIAN_POINT('Ctrl Pts',(3.84475203347052,-1.,-0.194909009460255));
#55199=CARTESIAN_POINT('Ctrl Pts',(3.85216762264019,-1.,-0.193642806777748));
#55200=CARTESIAN_POINT('Ctrl Pts',(3.85962774407652,-1.,-0.19231515304498));
#55201=CARTESIAN_POINT('Ctrl Pts',(3.8670715862477,-1.,-0.190924190418613));
#55202=CARTESIAN_POINT('Ctrl Pts',(3.87445976418377,-1.,-0.189469253358255));
#55203=CARTESIAN_POINT('Ctrl Pts',(3.88178563496187,-1.,-0.187951632512664));
#55204=CARTESIAN_POINT('Ctrl Pts',(3.88906196725817,-1.,-0.186373724985263));
#55205=CARTESIAN_POINT('Ctrl Pts',(3.89631300742633,-1.,-0.184738537728035));
#55206=CARTESIAN_POINT('Ctrl Pts',(3.90356488555138,-1.,-0.183049081993193));
#55207=CARTESIAN_POINT('Ctrl Pts',(3.91083557557193,-1.,-0.181307740731796));
#55208=CARTESIAN_POINT('Ctrl Pts',(3.91812876180948,-1.,-0.179515885822895));
#55209=CARTESIAN_POINT('Ctrl Pts',(3.92543942697672,-1.,-0.177674246152328));
#55210=CARTESIAN_POINT('Ctrl Pts',(3.93275726771049,-1.,-0.175783136893873));
#55211=CARTESIAN_POINT('Ctrl Pts',(3.94007083096214,-1.,-0.173842734974608));
#55212=CARTESIAN_POINT('Ctrl Pts',(3.94737164900861,-1.,-0.171853355369233));
#55213=CARTESIAN_POINT('Ctrl Pts',(3.95465744665263,-1.,-0.16981566637413));
#55214=CARTESIAN_POINT('Ctrl Pts',(3.96192990160296,-1.,-0.167730547023312));
#55215=CARTESIAN_POINT('Ctrl Pts',(3.9691931362141,-1.,-0.165598992851098));
#55216=CARTESIAN_POINT('Ctrl Pts',(3.97645194630944,-1.,-0.163422004609999));
#55217=CARTESIAN_POINT('Ctrl Pts',(3.98371010319866,-1.,-0.161200482186088));
#55218=CARTESIAN_POINT('Ctrl Pts',(3.99096873945862,-1.,-0.158935123982796));
#55219=CARTESIAN_POINT('Ctrl Pts',(3.99822717425869,-1.,-0.156626481393736));
#55220=CARTESIAN_POINT('Ctrl Pts',(4.00548360245297,-1.,-0.15427500487231));
#55221=CARTESIAN_POINT('Ctrl Pts',(4.01273584234684,-1.,-0.151881094022909));
#55222=CARTESIAN_POINT('Ctrl Pts',(4.01998203715588,-1.,-0.149445144968708));
#55223=CARTESIAN_POINT('Ctrl Pts',(4.02722143147048,-1.,-0.146967602878999));
#55224=CARTESIAN_POINT('Ctrl Pts',(4.03445411510403,-1.,-0.144448947038352));
#55225=CARTESIAN_POINT('Ctrl Pts',(4.04168069633842,-1.,-0.141889671485508));
#55226=CARTESIAN_POINT('Ctrl Pts',(4.04890199238056,-1.,-0.13929026718006));
#55227=CARTESIAN_POINT('Ctrl Pts',(4.05611873400122,-1.,-0.136651205046111));
#55228=CARTESIAN_POINT('Ctrl Pts',(4.06333121018476,-1.,-0.133972916144225));
#55229=CARTESIAN_POINT('Ctrl Pts',(4.07053931528579,-1.,-0.131255793548914));
#55230=CARTESIAN_POINT('Ctrl Pts',(4.07774270738809,-1.,-0.128500200484814));
#55231=CARTESIAN_POINT('Ctrl Pts',(4.08494093372315,-1.,-0.12570647682253));
#55232=CARTESIAN_POINT('Ctrl Pts',(4.09213355850836,-1.,-0.122874946249119));
#55233=CARTESIAN_POINT('Ctrl Pts',(4.09932031767243,-1.,-0.120005924388162));
#55234=CARTESIAN_POINT('Ctrl Pts',(4.10650113382187,-1.,-0.117099722731705));
#55235=CARTESIAN_POINT('Ctrl Pts',(4.11367603925313,-1.,-0.114156649609602));
#55236=CARTESIAN_POINT('Ctrl Pts',(4.12084512502444,-1.,-0.111177012683378));
#55237=CARTESIAN_POINT('Ctrl Pts',(4.12800848371386,-1.,-0.10816112052835));
#55238=CARTESIAN_POINT('Ctrl Pts',(4.13516614458396,-1.,-0.105109286538864));
#55239=CARTESIAN_POINT('Ctrl Pts',(4.14231804938737,-1.,-0.102021826577454));
#55240=CARTESIAN_POINT('Ctrl Pts',(4.1494640891762,-1.,-0.0988990478899816));
#55241=CARTESIAN_POINT('Ctrl Pts',(4.15660412653006,-1.,-0.0957412403297072));
#55242=CARTESIAN_POINT('Ctrl Pts',(4.16373802265942,-1.,-0.0925486672167695));
#55243=CARTESIAN_POINT('Ctrl Pts',(4.17086566491823,-1.,-0.0893215560850332));
#55244=CARTESIAN_POINT('Ctrl Pts',(4.17798698669991,-1.,-0.086060091555252));
#55245=CARTESIAN_POINT('Ctrl Pts',(4.1851019532944,-1.,-0.0827644164389515));
#55246=CARTESIAN_POINT('Ctrl Pts',(4.19078883322483,-1.,-0.0801005887117608));
#55247=CARTESIAN_POINT('Ctrl Pts',(4.19505112860624,-1.,-0.0780873956244407));
#55248=CARTESIAN_POINT('Ctrl Pts',(4.19789138621624,-1.,-0.07673845961422));
#55249=CARTESIAN_POINT('Ctrl Pts',(4.19931119685982,-1.,-0.0760622897878241));
#55250=CARTESIAN_POINT('',(4.19931119685982,-1.,0.0760622897878241));
#55251=CARTESIAN_POINT('',(4.19931119685982,-1.,-0.0760622897878241));
#55252=CARTESIAN_POINT('',(3.74449296983004,-1.,0.2031560948961));
#55253=CARTESIAN_POINT('Ctrl Pts',(4.19931119685982,-1.,0.0760622897878241));
#55254=CARTESIAN_POINT('Ctrl Pts',(4.1978913862118,-1.,0.0767384596141459));
#55255=CARTESIAN_POINT('Ctrl Pts',(4.19505112859416,-1.,0.0780873956242392));
#55256=CARTESIAN_POINT('Ctrl Pts',(4.19078883320504,-1.,0.0801005887114315));
#55257=CARTESIAN_POINT('Ctrl Pts',(4.18510195327123,-1.,0.0827644164385674));
#55258=CARTESIAN_POINT('Ctrl Pts',(4.17798698668094,-1.,0.0860600915549391));
#55259=CARTESIAN_POINT('Ctrl Pts',(4.17086566490794,-1.,0.0893215560848644));
#55260=CARTESIAN_POINT('Ctrl Pts',(4.16373802265839,-1.,0.0925486672167526));
#55261=CARTESIAN_POINT('Ctrl Pts',(4.15660412653577,-1.,0.0957412403298002));
#55262=CARTESIAN_POINT('Ctrl Pts',(4.14946408918485,-1.,0.0988990478901221));
#55263=CARTESIAN_POINT('Ctrl Pts',(4.14231804939538,-1.,0.102021826577583));
#55264=CARTESIAN_POINT('Ctrl Pts',(4.13516614458895,-1.,0.105109286538945));
#55265=CARTESIAN_POINT('Ctrl Pts',(4.12800848371504,-1.,0.108161120528369));
#55266=CARTESIAN_POINT('Ctrl Pts',(4.1208451250225,-1.,0.111177012683346));
#55267=CARTESIAN_POINT('Ctrl Pts',(4.11367603924961,-1.,0.114156649609545));
#55268=CARTESIAN_POINT('Ctrl Pts',(4.10650113381833,-1.,0.117099722731648));
#55269=CARTESIAN_POINT('Ctrl Pts',(4.09932031767002,-1.,0.120005924388124));
#55270=CARTESIAN_POINT('Ctrl Pts',(4.09213355850756,-1.,0.122874946249106));
#55271=CARTESIAN_POINT('Ctrl Pts',(4.08494093372377,-1.,0.125706476822539));
#55272=CARTESIAN_POINT('Ctrl Pts',(4.07774270738954,-1.,0.128500200484837));
#55273=CARTESIAN_POINT('Ctrl Pts',(4.0705393152874,-1.,0.13125579354894));
#55274=CARTESIAN_POINT('Ctrl Pts',(4.06333121018596,-1.,0.133972916144244));
#55275=CARTESIAN_POINT('Ctrl Pts',(4.05611873400172,-1.,0.136651205046119));
#55276=CARTESIAN_POINT('Ctrl Pts',(4.04890199238036,-1.,0.139290267180057));
#55277=CARTESIAN_POINT('Ctrl Pts',(4.04168069633781,-1.,0.1418896714855));
#55278=CARTESIAN_POINT('Ctrl Pts',(4.03445411510333,-1.,0.144448947038344));
#55279=CARTESIAN_POINT('Ctrl Pts',(4.02722143146994,-1.,0.146967602878994));
#55280=CARTESIAN_POINT('Ctrl Pts',(4.01998203715564,-1.,0.149445144968706));
#55281=CARTESIAN_POINT('Ctrl Pts',(4.01273584234689,-1.,0.15188109402291));
#55282=CARTESIAN_POINT('Ctrl Pts',(4.00548360245319,-1.,0.15427500487231));
#55283=CARTESIAN_POINT('Ctrl Pts',(3.99822717425893,-1.,0.156626481393734));
#55284=CARTESIAN_POINT('Ctrl Pts',(3.99096873945878,-1.,0.158935123982793));
#55285=CARTESIAN_POINT('Ctrl Pts',(3.98371010319872,-1.,0.161200482186084));
#55286=CARTESIAN_POINT('Ctrl Pts',(3.97645194630943,-1.,0.163422004609999));
#55287=CARTESIAN_POINT('Ctrl Pts',(3.96919313621407,-1.,0.165598992851102));
#55288=CARTESIAN_POINT('Ctrl Pts',(3.96192990160296,-1.,0.167730547023319));
#55289=CARTESIAN_POINT('Ctrl Pts',(3.95465744665268,-1.,0.169815666374138));
#55290=CARTESIAN_POINT('Ctrl Pts',(3.94737164900868,-1.,0.17185335536924));
#55291=CARTESIAN_POINT('Ctrl Pts',(3.94007083096217,-1.,0.173842734974609));
#55292=CARTESIAN_POINT('Ctrl Pts',(3.93275726771042,-1.,0.175783136893867));
#55293=CARTESIAN_POINT('Ctrl Pts',(3.92543942697655,-1.,0.177674246152317));
#55294=CARTESIAN_POINT('Ctrl Pts',(3.91812876180926,-1.,0.179515885822881));
#55295=CARTESIAN_POINT('Ctrl Pts',(3.91083557557175,-1.,0.181307740731785));
#55296=CARTESIAN_POINT('Ctrl Pts',(3.90356488555132,-1.,0.18304908199319));
#55297=CARTESIAN_POINT('Ctrl Pts',(3.89631300742646,-1.,0.184738537728042));
#55298=CARTESIAN_POINT('Ctrl Pts',(3.88906196725848,-1.,0.18637372498528));
#55299=CARTESIAN_POINT('Ctrl Pts',(3.88178563496228,-1.,0.187951632512684));
#55300=CARTESIAN_POINT('Ctrl Pts',(3.87445976418412,-1.,0.189469253358272));
#55301=CARTESIAN_POINT('Ctrl Pts',(3.86707158624783,-1.,0.190924190418619));
#55302=CARTESIAN_POINT('Ctrl Pts',(3.85962774407633,-1.,0.19231515304497));
#55303=CARTESIAN_POINT('Ctrl Pts',(3.85216762263966,-1.,0.193642806777722));
#55304=CARTESIAN_POINT('Ctrl Pts',(3.84475203346977,-1.,0.19490900946022));
#55305=CARTESIAN_POINT('Ctrl Pts',(3.83743910616195,-1.,0.196115198971858));
#55306=CARTESIAN_POINT('Ctrl Pts',(3.83026221776456,-1.,0.197260935827361));
#55307=CARTESIAN_POINT('Ctrl Pts',(3.82321127349016,-1.,0.198342616900486));
#55308=CARTESIAN_POINT('Ctrl Pts',(3.81620203429815,-1.,0.199351525297447));
#55309=CARTESIAN_POINT('Ctrl Pts',(3.80909529318669,-1.,0.200274679433364));
#55310=CARTESIAN_POINT('Ctrl Pts',(3.80175247447337,-1.,0.201097756307325));
#55311=CARTESIAN_POINT('Ctrl Pts',(3.7940835418736,-1.,0.201807533800837));
#55312=CARTESIAN_POINT('Ctrl Pts',(3.78609175019242,-1.,0.20239426051216));
#55313=CARTESIAN_POINT('Ctrl Pts',(3.77793553476614,-1.,0.20285472969908));
#55314=CARTESIAN_POINT('Ctrl Pts',(3.7699207159487,-1.,0.203192390045164));
#55315=CARTESIAN_POINT('Ctrl Pts',(3.76242717936885,-1.,0.203414634707478));
#55316=CARTESIAN_POINT('Ctrl Pts',(3.75585118707734,-1.,0.203530796848321));
#55317=CARTESIAN_POINT('Ctrl Pts',(3.75054693397875,-1.,0.203550035479166));
#55318=CARTESIAN_POINT('Ctrl Pts',(3.74703926501752,-1.,0.203484186269415));
#55319=CARTESIAN_POINT('Ctrl Pts',(3.74535749969115,-1.,0.203375226874121));
#55320=CARTESIAN_POINT('Ctrl Pts',(3.74471097893845,-1.,0.20326661011053));
#55321=CARTESIAN_POINT('Ctrl Pts',(3.74453008995092,-1.,0.203188003946656));
#55322=CARTESIAN_POINT('Ctrl Pts',(3.74449296983004,-1.,0.2031560948961));
#55323=CARTESIAN_POINT('',(3.73017266276651,-1.,0.385112848330762));
#55324=CARTESIAN_POINT('Origin',(0.,-1.,0.));
#55325=CARTESIAN_POINT('',(4.15950947128175,-1.,0.581791163835816));
#55326=CARTESIAN_POINT('Ctrl Pts',(3.73017266276651,-1.,0.385112848330762));
#55327=CARTESIAN_POINT('Ctrl Pts',(3.73021431755274,-1.,0.385087139000375));
#55328=CARTESIAN_POINT('Ctrl Pts',(3.73040527621055,-1.,0.385037797881504));
#55329=CARTESIAN_POINT('Ctrl Pts',(3.73106082862548,-1.,0.385031656499164));
#55330=CARTESIAN_POINT('Ctrl Pts',(3.73273893363406,-1.,0.385187124634207));
#55331=CARTESIAN_POINT('Ctrl Pts',(3.73621371845318,-1.,0.385670806454566));
#55332=CARTESIAN_POINT('Ctrl Pts',(3.74144965781276,-1.,0.386519576222252));
#55333=CARTESIAN_POINT('Ctrl Pts',(3.74792651696654,-1.,0.387663020050836));
#55334=CARTESIAN_POINT('Ctrl Pts',(3.75529302895152,-1.,0.389054775898702));
#55335=CARTESIAN_POINT('Ctrl Pts',(3.76315635033257,-1.,0.39064207297956));
#55336=CARTESIAN_POINT('Ctrl Pts',(3.77114011595967,-1.,0.392372786223433));
#55337=CARTESIAN_POINT('Ctrl Pts',(3.77894173114283,-1.,0.3942024810115));
#55338=CARTESIAN_POINT('Ctrl Pts',(3.78640521279313,-1.,0.396103205334841));
#55339=CARTESIAN_POINT('Ctrl Pts',(3.7935288716329,-1.,0.39806481868397));
#55340=CARTESIAN_POINT('Ctrl Pts',(3.80040370384546,-1.,0.400088346504601));
#55341=CARTESIAN_POINT('Ctrl Pts',(3.80716881962728,-1.,0.402181320148436));
#55342=CARTESIAN_POINT('Ctrl Pts',(3.81396374287793,-1.,0.404352694628274));
#55343=CARTESIAN_POINT('Ctrl Pts',(3.8208730391381,-1.,0.406607038258986));
#55344=CARTESIAN_POINT('Ctrl Pts',(3.82790724256471,-1.,0.40894237144746));
#55345=CARTESIAN_POINT('Ctrl Pts',(3.83503345578698,-1.,0.411353038798519));
#55346=CARTESIAN_POINT('Ctrl Pts',(3.84219403994762,-1.,0.413831367016748));
#55347=CARTESIAN_POINT('Ctrl Pts',(3.84932864157497,-1.,0.416369678052907));
#55348=CARTESIAN_POINT('Ctrl Pts',(3.85639825647996,-1.,0.418962468086773));
#55349=CARTESIAN_POINT('Ctrl Pts',(3.86339652542709,-1.,0.421607423177534));
#55350=CARTESIAN_POINT('Ctrl Pts',(3.87033643487851,-1.,0.424304173195111));
#55351=CARTESIAN_POINT('Ctrl Pts',(3.87724240306597,-1.,0.427053541173458));
#55352=CARTESIAN_POINT('Ctrl Pts',(3.88414070943341,-1.,0.429856640579741));
#55353=CARTESIAN_POINT('Ctrl Pts',(3.89104947940611,-1.,0.432713929544459));
#55354=CARTESIAN_POINT('Ctrl Pts',(3.89797256655462,-1.,0.435624629433528));
#55355=CARTESIAN_POINT('Ctrl Pts',(3.90490512938563,-1.,0.43858723545825));
#55356=CARTESIAN_POINT('Ctrl Pts',(3.91183704069153,-1.,0.441599824524055));
#55357=CARTESIAN_POINT('Ctrl Pts',(3.91875701610719,-1.,0.444660430230591));
#55358=CARTESIAN_POINT('Ctrl Pts',(3.92565674143416,-1.,0.447767416837293));
#55359=CARTESIAN_POINT('Ctrl Pts',(3.93253407403123,-1.,0.450919768356349));
#55360=CARTESIAN_POINT('Ctrl Pts',(3.93939080846298,-1.,0.454116879027584));
#55361=CARTESIAN_POINT('Ctrl Pts',(3.94623117206678,-1.,0.457358410451683));
#55362=CARTESIAN_POINT('Ctrl Pts',(3.95306005817364,-1.,0.460644124429122));
#55363=CARTESIAN_POINT('Ctrl Pts',(3.95988133243538,-1.,0.463973722115734));
#55364=CARTESIAN_POINT('Ctrl Pts',(3.9666962227393,-1.,0.467346690880644));
#55365=CARTESIAN_POINT('Ctrl Pts',(3.97350414289392,-1.,0.47076237961344));
#55366=CARTESIAN_POINT('Ctrl Pts',(3.98030338044409,-1.,0.47422006101951));
#55367=CARTESIAN_POINT('Ctrl Pts',(3.98709184306738,-1.,0.477718999122028));
#55368=CARTESIAN_POINT('Ctrl Pts',(3.99386775880679,-1.,0.481258512209676));
#55369=CARTESIAN_POINT('Ctrl Pts',(4.00063045119288,-1.,0.484838042421835));
#55370=CARTESIAN_POINT('Ctrl Pts',(4.0073800839099,-1.,0.488457130424634));
#55371=CARTESIAN_POINT('Ctrl Pts',(4.01411733503546,-1.,0.492115383418019));
#55372=CARTESIAN_POINT('Ctrl Pts',(4.02084308851832,-1.,0.495812444326251));
#55373=CARTESIAN_POINT('Ctrl Pts',(4.02755813980101,-1.,0.499547962340822));
#55374=CARTESIAN_POINT('Ctrl Pts',(4.03426284174272,-1.,0.503321556915346));
#55375=CARTESIAN_POINT('Ctrl Pts',(4.04095715148915,-1.,0.507132823288137));
#55376=CARTESIAN_POINT('Ctrl Pts',(4.04764078815447,-1.,0.510981349218971));
#55377=CARTESIAN_POINT('Ctrl Pts',(4.05431335771199,-1.,0.514866728193017));
#55378=CARTESIAN_POINT('Ctrl Pts',(4.06097448038013,-1.,0.518788572336924));
#55379=CARTESIAN_POINT('Ctrl Pts',(4.06762394471314,-1.,0.522746528603108));
#55380=CARTESIAN_POINT('Ctrl Pts',(4.07426172299847,-1.,0.526740277227498));
#55381=CARTESIAN_POINT('Ctrl Pts',(4.08088789536836,-1.,0.530769518728571));
#55382=CARTESIAN_POINT('Ctrl Pts',(4.08750259988885,-1.,0.534833963477273));
#55383=CARTESIAN_POINT('Ctrl Pts',(4.09410597627,-1.,0.538933321179756));
#55384=CARTESIAN_POINT('Ctrl Pts',(4.10069810243979,-1.,0.543067286877758));
#55385=CARTESIAN_POINT('Ctrl Pts',(4.10727897027977,-1.,0.547235539485637));
#55386=CARTESIAN_POINT('Ctrl Pts',(4.11384852024721,-1.,0.551437758497033));
#55387=CARTESIAN_POINT('Ctrl Pts',(4.12040666195664,-1.,0.555673636129978));
#55388=CARTESIAN_POINT('Ctrl Pts',(4.12695329951961,-1.,0.559942890594774));
#55389=CARTESIAN_POINT('Ctrl Pts',(4.13348835727104,-1.,0.564245279537149));
#55390=CARTESIAN_POINT('Ctrl Pts',(4.14001179830547,-1.,0.568580610189775));
#55391=CARTESIAN_POINT('Ctrl Pts',(4.14652361068081,-1.,0.572948736069523));
#55392=CARTESIAN_POINT('Ctrl Pts',(4.151723761217,-1.,0.576469391676689));
#55393=CARTESIAN_POINT('Ctrl Pts',(4.15561864788576,-1.,0.579124568914236));
#55394=CARTESIAN_POINT('Ctrl Pts',(4.1582129171283,-1.,0.580901211463535));
#55395=CARTESIAN_POINT('Ctrl Pts',(4.15950947128175,-1.,0.581791163835816));
#55396=CARTESIAN_POINT('',(4.13571194405636,-1.,0.732042837400621));
#55397=CARTESIAN_POINT('',(4.15950947128175,-1.,0.581791163835816));
#55398=CARTESIAN_POINT('Ctrl Pts',(4.13571194405636,-1.,0.732042837400621));
#55399=CARTESIAN_POINT('Ctrl Pts',(4.1342038373684,-1.,0.73248857513516));
#55400=CARTESIAN_POINT('Ctrl Pts',(4.13118752795207,-1.,0.733376589323547));
#55401=CARTESIAN_POINT('Ctrl Pts',(4.12666277570844,-1.,0.734698226764093));
#55402=CARTESIAN_POINT('Ctrl Pts',(4.120629196238,-1.,0.736439634331345));
#55403=CARTESIAN_POINT('Ctrl Pts',(4.11308626951927,-1.,0.738581708225844));
#55404=CARTESIAN_POINT('Ctrl Pts',(4.10554241757547,-1.,0.740688998553377));
#55405=CARTESIAN_POINT('Ctrl Pts',(4.09799769702611,-1.,0.742761369689842));
#55406=CARTESIAN_POINT('Ctrl Pts',(4.09045220253573,-1.,0.744798649706501));
#55407=CARTESIAN_POINT('Ctrl Pts',(4.08290608095642,-1.,0.746800631492316));
#55408=CARTESIAN_POINT('Ctrl Pts',(4.07535951056152,-1.,0.748767076680558));
#55409=CARTESIAN_POINT('Ctrl Pts',(4.06781267242378,-1.,0.750697720484037));
#55410=CARTESIAN_POINT('Ctrl Pts',(4.06026572221515,-1.,0.752592276483073));
#55411=CARTESIAN_POINT('Ctrl Pts',(4.05271876687915,-1.,0.754450441816078));
#55412=CARTESIAN_POINT('Ctrl Pts',(4.04517182653997,-1.,0.756271902369581));
#55413=CARTESIAN_POINT('Ctrl Pts',(4.03762485803119,-1.,0.758056338884945));
#55414=CARTESIAN_POINT('Ctrl Pts',(4.03007781954412,-1.,0.759803433243752));
#55415=CARTESIAN_POINT('Ctrl Pts',(4.02253072741268,-1.,0.761512875859805));
#55416=CARTESIAN_POINT('Ctrl Pts',(4.01498370680496,-1.,0.763184371182936));
#55417=CARTESIAN_POINT('Ctrl Pts',(4.00743706791509,-1.,0.764817648785198));
#55418=CARTESIAN_POINT('Ctrl Pts',(3.99989129179622,-1.,0.766412457136064));
#55419=CARTESIAN_POINT('Ctrl Pts',(3.9923468788101,-1.,0.767968531377915));
#55420=CARTESIAN_POINT('Ctrl Pts',(3.98480422348451,-1.,0.769485566245545));
#55421=CARTESIAN_POINT('Ctrl Pts',(3.97726349165488,-1.,0.770963190030471));
#55422=CARTESIAN_POINT('Ctrl Pts',(3.96972446532772,-1.,0.772400931772137));
#55423=CARTESIAN_POINT('Ctrl Pts',(3.96218649639807,-1.,0.773798212026566));
#55424=CARTESIAN_POINT('Ctrl Pts',(3.9546488545231,-1.,0.775154418039352));
#55425=CARTESIAN_POINT('Ctrl Pts',(3.94711101619447,-1.,0.776468966697922));
#55426=CARTESIAN_POINT('Ctrl Pts',(3.93957296768103,-1.,0.777741370568559));
#55427=CARTESIAN_POINT('Ctrl Pts',(3.93203552473174,-1.,0.778971308134821));
#55428=CARTESIAN_POINT('Ctrl Pts',(3.92450058323823,-1.,0.780158678615543));
#55429=CARTESIAN_POINT('Ctrl Pts',(3.91697036054676,-1.,0.781303428618367));
#55430=CARTESIAN_POINT('Ctrl Pts',(3.90944671004542,-1.,0.782405395622765));
#55431=CARTESIAN_POINT('Ctrl Pts',(3.9019303904397,-1.,0.783464141529082));
#55432=CARTESIAN_POINT('Ctrl Pts',(3.89442039235103,-1.,0.784478799358337));
#55433=CARTESIAN_POINT('Ctrl Pts',(3.88691313167398,-1.,0.785447890340731));
#55434=CARTESIAN_POINT('Ctrl Pts',(3.8794040281819,-1.,0.786369675812609));
#55435=CARTESIAN_POINT('Ctrl Pts',(3.87188916600912,-1.,0.787242527617999));
#55436=CARTESIAN_POINT('Ctrl Pts',(3.86436702561345,-1.,0.788065315093778));
#55437=CARTESIAN_POINT('Ctrl Pts',(3.85683995872529,-1.,0.788837734090672));
#55438=CARTESIAN_POINT('Ctrl Pts',(3.84931637808894,-1.,0.789560798155583));
#55439=CARTESIAN_POINT('Ctrl Pts',(3.84180762342454,-1.,0.790236124191243));
#55440=CARTESIAN_POINT('Ctrl Pts',(3.83432392054786,-1.,0.790865012705301));
#55441=CARTESIAN_POINT('Ctrl Pts',(3.82687033899792,-1.,0.791447528662369));
#55442=CARTESIAN_POINT('Ctrl Pts',(3.81944345442249,-1.,0.791981740718635));
#55443=CARTESIAN_POINT('Ctrl Pts',(3.81202588694756,-1.,0.792462483517635));
#55444=CARTESIAN_POINT('Ctrl Pts',(3.80459229925637,-1.,0.792882695234778));
#55445=CARTESIAN_POINT('Ctrl Pts',(3.79711921389897,-1.,0.793235612973274));
#55446=CARTESIAN_POINT('Ctrl Pts',(3.78959439439235,-1.,0.793516871680994));
#55447=CARTESIAN_POINT('Ctrl Pts',(3.78202460377598,-1.,0.793726235781301));
#55448=CARTESIAN_POINT('Ctrl Pts',(3.77444863801212,-1.,0.793870523787408));
#55449=CARTESIAN_POINT('Ctrl Pts',(3.76692626931111,-1.,0.793961083688992));
#55450=CARTESIAN_POINT('Ctrl Pts',(3.75951468666257,-1.,0.794008429134908));
#55451=CARTESIAN_POINT('Ctrl Pts',(3.75224692493864,-1.,0.794017347371378));
#55452=CARTESIAN_POINT('Ctrl Pts',(3.74511357728861,-1.,0.793982700459952));
#55453=CARTESIAN_POINT('Ctrl Pts',(3.73803280541687,-1.,0.793882700937017));
#55454=CARTESIAN_POINT('Ctrl Pts',(3.73086914695805,-1.,0.793682750269684));
#55455=CARTESIAN_POINT('Ctrl Pts',(3.72348797293734,-1.,0.793347023784205));
#55456=CARTESIAN_POINT('Ctrl Pts',(3.71580242396124,-1.,0.792848377370287));
#55457=CARTESIAN_POINT('Ctrl Pts',(3.70781724021806,-1.,0.792177688845818));
#55458=CARTESIAN_POINT('Ctrl Pts',(3.69968940808721,-1.,0.79135657569598));
#55459=CARTESIAN_POINT('Ctrl Pts',(3.69172044327364,-1.,0.790436284988788));
#55460=CARTESIAN_POINT('Ctrl Pts',(3.68428439783905,-1.,0.789483546064387));
#55461=CARTESIAN_POINT('Ctrl Pts',(3.67777119516252,-1.,0.788569566220286));
#55462=CARTESIAN_POINT('Ctrl Pts',(3.67252923663655,-1.,0.787758799995743));
#55463=CARTESIAN_POINT('Ctrl Pts',(3.66907505398677,-1.,0.787145041181546));
#55464=CARTESIAN_POINT('Ctrl Pts',(3.66743103898702,-1.,0.786774337198063));
#55465=CARTESIAN_POINT('Ctrl Pts',(3.66680946938292,-1.,0.786565919558984));
#55466=CARTESIAN_POINT('Ctrl Pts',(3.6666431041522,-1.,0.786459983895432));
#55467=CARTESIAN_POINT('Ctrl Pts',(3.66661143271685,-1.,0.786422660831985));
#55468=CARTESIAN_POINT('Origin',(0.,-1.,0.));
#55469=CARTESIAN_POINT('Origin',(0.,0.,0.));
#55470=CARTESIAN_POINT('Origin',(0.,2.2,0.));
#55471=CARTESIAN_POINT('Origin',(0.,1.,0.));
#55472=CARTESIAN_POINT('',(-2.,2.2,2.44929359829471E-16));
#55473=CARTESIAN_POINT('Origin',(0.,2.2,0.));
#55474=CARTESIAN_POINT('',(-2.,1.,2.44929359829471E-16));
#55475=CARTESIAN_POINT('',(-2.,1.,2.44929359829471E-16));
#55476=CARTESIAN_POINT('Origin',(0.,1.,0.));
#55477=CARTESIAN_POINT('Origin',(0.,2.2,0.));
#55478=CARTESIAN_POINT('Ctrl Pts',(4.15950947128175,-1.,0.581791163835816));
#55479=CARTESIAN_POINT('Ctrl Pts',(4.15950947128175,1.,0.581791163835816));
#55480=CARTESIAN_POINT('Ctrl Pts',(4.1582129171283,-1.,0.580901211463535));
#55481=CARTESIAN_POINT('Ctrl Pts',(4.1582129171283,1.,0.580901211463535));
#55482=CARTESIAN_POINT('Ctrl Pts',(4.15561864788576,-1.,0.579124568914236));
#55483=CARTESIAN_POINT('Ctrl Pts',(4.15561864788576,1.,0.579124568914236));
#55484=CARTESIAN_POINT('Ctrl Pts',(4.151723761217,-1.,0.576469391676689));
#55485=CARTESIAN_POINT('Ctrl Pts',(4.151723761217,1.,0.576469391676689));
#55486=CARTESIAN_POINT('Ctrl Pts',(4.14652361068081,-1.,0.572948736069523));
#55487=CARTESIAN_POINT('Ctrl Pts',(4.14652361068081,1.,0.572948736069523));
#55488=CARTESIAN_POINT('Ctrl Pts',(4.14001179830547,-1.,0.568580610189775));
#55489=CARTESIAN_POINT('Ctrl Pts',(4.14001179830547,1.,0.568580610189775));
#55490=CARTESIAN_POINT('Ctrl Pts',(4.13348835727104,-1.,0.564245279537149));
#55491=CARTESIAN_POINT('Ctrl Pts',(4.13348835727104,1.,0.564245279537149));
#55492=CARTESIAN_POINT('Ctrl Pts',(4.12695329951961,-1.,0.559942890594774));
#55493=CARTESIAN_POINT('Ctrl Pts',(4.12695329951961,1.,0.559942890594774));
#55494=CARTESIAN_POINT('Ctrl Pts',(4.12040666195664,-1.,0.555673636129978));
#55495=CARTESIAN_POINT('Ctrl Pts',(4.12040666195664,1.,0.555673636129978));
#55496=CARTESIAN_POINT('Ctrl Pts',(4.11384852024721,-1.,0.551437758497033));
#55497=CARTESIAN_POINT('Ctrl Pts',(4.11384852024721,1.,0.551437758497033));
#55498=CARTESIAN_POINT('Ctrl Pts',(4.10727897027977,-1.,0.547235539485637));
#55499=CARTESIAN_POINT('Ctrl Pts',(4.10727897027977,1.,0.547235539485637));
#55500=CARTESIAN_POINT('Ctrl Pts',(4.10069810243979,-1.,0.543067286877758));
#55501=CARTESIAN_POINT('Ctrl Pts',(4.10069810243979,1.,0.543067286877758));
#55502=CARTESIAN_POINT('Ctrl Pts',(4.09410597627,-1.,0.538933321179756));
#55503=CARTESIAN_POINT('Ctrl Pts',(4.09410597627,1.,0.538933321179756));
#55504=CARTESIAN_POINT('Ctrl Pts',(4.08750259988885,-1.,0.534833963477273));
#55505=CARTESIAN_POINT('Ctrl Pts',(4.08750259988885,1.,0.534833963477273));
#55506=CARTESIAN_POINT('Ctrl Pts',(4.08088789536836,-1.,0.530769518728571));
#55507=CARTESIAN_POINT('Ctrl Pts',(4.08088789536836,1.,0.530769518728571));
#55508=CARTESIAN_POINT('Ctrl Pts',(4.07426172299847,-1.,0.526740277227498));
#55509=CARTESIAN_POINT('Ctrl Pts',(4.07426172299847,1.,0.526740277227498));
#55510=CARTESIAN_POINT('Ctrl Pts',(4.06762394471314,-1.,0.522746528603108));
#55511=CARTESIAN_POINT('Ctrl Pts',(4.06762394471314,1.,0.522746528603108));
#55512=CARTESIAN_POINT('Ctrl Pts',(4.06097448038013,-1.,0.518788572336924));
#55513=CARTESIAN_POINT('Ctrl Pts',(4.06097448038013,1.,0.518788572336924));
#55514=CARTESIAN_POINT('Ctrl Pts',(4.05431335771199,-1.,0.514866728193017));
#55515=CARTESIAN_POINT('Ctrl Pts',(4.05431335771199,1.,0.514866728193017));
#55516=CARTESIAN_POINT('Ctrl Pts',(4.04764078815447,-1.,0.510981349218971));
#55517=CARTESIAN_POINT('Ctrl Pts',(4.04764078815447,1.,0.510981349218971));
#55518=CARTESIAN_POINT('Ctrl Pts',(4.04095715148915,-1.,0.507132823288137));
#55519=CARTESIAN_POINT('Ctrl Pts',(4.04095715148915,1.,0.507132823288137));
#55520=CARTESIAN_POINT('Ctrl Pts',(4.03426284174272,-1.,0.503321556915346));
#55521=CARTESIAN_POINT('Ctrl Pts',(4.03426284174272,1.,0.503321556915346));
#55522=CARTESIAN_POINT('Ctrl Pts',(4.02755813980101,-1.,0.499547962340822));
#55523=CARTESIAN_POINT('Ctrl Pts',(4.02755813980101,1.,0.499547962340822));
#55524=CARTESIAN_POINT('Ctrl Pts',(4.02084308851832,-1.,0.495812444326251));
#55525=CARTESIAN_POINT('Ctrl Pts',(4.02084308851832,1.,0.495812444326251));
#55526=CARTESIAN_POINT('Ctrl Pts',(4.01411733503546,-1.,0.492115383418019));
#55527=CARTESIAN_POINT('Ctrl Pts',(4.01411733503546,1.,0.492115383418019));
#55528=CARTESIAN_POINT('Ctrl Pts',(4.0073800839099,-1.,0.488457130424634));
#55529=CARTESIAN_POINT('Ctrl Pts',(4.0073800839099,1.,0.488457130424634));
#55530=CARTESIAN_POINT('Ctrl Pts',(4.00063045119288,-1.,0.484838042421835));
#55531=CARTESIAN_POINT('Ctrl Pts',(4.00063045119288,1.,0.484838042421835));
#55532=CARTESIAN_POINT('Ctrl Pts',(3.99386775880679,-1.,0.481258512209676));
#55533=CARTESIAN_POINT('Ctrl Pts',(3.99386775880679,1.,0.481258512209676));
#55534=CARTESIAN_POINT('Ctrl Pts',(3.98709184306738,-1.,0.477718999122028));
#55535=CARTESIAN_POINT('Ctrl Pts',(3.98709184306738,1.,0.477718999122028));
#55536=CARTESIAN_POINT('Ctrl Pts',(3.98030338044409,-1.,0.47422006101951));
#55537=CARTESIAN_POINT('Ctrl Pts',(3.98030338044409,1.,0.47422006101951));
#55538=CARTESIAN_POINT('Ctrl Pts',(3.97350414289392,-1.,0.47076237961344));
#55539=CARTESIAN_POINT('Ctrl Pts',(3.97350414289392,1.,0.47076237961344));
#55540=CARTESIAN_POINT('Ctrl Pts',(3.9666962227393,-1.,0.467346690880644));
#55541=CARTESIAN_POINT('Ctrl Pts',(3.9666962227393,1.,0.467346690880644));
#55542=CARTESIAN_POINT('Ctrl Pts',(3.95988133243538,-1.,0.463973722115734));
#55543=CARTESIAN_POINT('Ctrl Pts',(3.95988133243538,1.,0.463973722115734));
#55544=CARTESIAN_POINT('Ctrl Pts',(3.95306005817364,-1.,0.460644124429122));
#55545=CARTESIAN_POINT('Ctrl Pts',(3.95306005817364,1.,0.460644124429122));
#55546=CARTESIAN_POINT('Ctrl Pts',(3.94623117206678,-1.,0.457358410451683));
#55547=CARTESIAN_POINT('Ctrl Pts',(3.94623117206678,1.,0.457358410451683));
#55548=CARTESIAN_POINT('Ctrl Pts',(3.93939080846298,-1.,0.454116879027584));
#55549=CARTESIAN_POINT('Ctrl Pts',(3.93939080846298,1.,0.454116879027584));
#55550=CARTESIAN_POINT('Ctrl Pts',(3.93253407403123,-1.,0.450919768356349));
#55551=CARTESIAN_POINT('Ctrl Pts',(3.93253407403123,1.,0.450919768356349));
#55552=CARTESIAN_POINT('Ctrl Pts',(3.92565674143416,-1.,0.447767416837293));
#55553=CARTESIAN_POINT('Ctrl Pts',(3.92565674143416,1.,0.447767416837293));
#55554=CARTESIAN_POINT('Ctrl Pts',(3.91875701610719,-1.,0.444660430230591));
#55555=CARTESIAN_POINT('Ctrl Pts',(3.91875701610719,1.,0.444660430230591));
#55556=CARTESIAN_POINT('Ctrl Pts',(3.91183704069153,-1.,0.441599824524055));
#55557=CARTESIAN_POINT('Ctrl Pts',(3.91183704069153,1.,0.441599824524055));
#55558=CARTESIAN_POINT('Ctrl Pts',(3.90490512938563,-1.,0.43858723545825));
#55559=CARTESIAN_POINT('Ctrl Pts',(3.90490512938563,1.,0.43858723545825));
#55560=CARTESIAN_POINT('Ctrl Pts',(3.89797256655462,-1.,0.435624629433528));
#55561=CARTESIAN_POINT('Ctrl Pts',(3.89797256655462,1.,0.435624629433528));
#55562=CARTESIAN_POINT('Ctrl Pts',(3.89104947940611,-1.,0.432713929544459));
#55563=CARTESIAN_POINT('Ctrl Pts',(3.89104947940611,1.,0.432713929544459));
#55564=CARTESIAN_POINT('Ctrl Pts',(3.88414070943341,-1.,0.429856640579741));
#55565=CARTESIAN_POINT('Ctrl Pts',(3.88414070943341,1.,0.429856640579741));
#55566=CARTESIAN_POINT('Ctrl Pts',(3.87724240306597,-1.,0.427053541173458));
#55567=CARTESIAN_POINT('Ctrl Pts',(3.87724240306597,1.,0.427053541173458));
#55568=CARTESIAN_POINT('Ctrl Pts',(3.87033643487851,-1.,0.424304173195111));
#55569=CARTESIAN_POINT('Ctrl Pts',(3.87033643487851,1.,0.424304173195111));
#55570=CARTESIAN_POINT('Ctrl Pts',(3.86339652542709,-1.,0.421607423177534));
#55571=CARTESIAN_POINT('Ctrl Pts',(3.86339652542709,1.,0.421607423177534));
#55572=CARTESIAN_POINT('Ctrl Pts',(3.85639825647996,-1.,0.418962468086773));
#55573=CARTESIAN_POINT('Ctrl Pts',(3.85639825647996,1.,0.418962468086773));
#55574=CARTESIAN_POINT('Ctrl Pts',(3.84932864157497,-1.,0.416369678052907));
#55575=CARTESIAN_POINT('Ctrl Pts',(3.84932864157497,1.,0.416369678052907));
#55576=CARTESIAN_POINT('Ctrl Pts',(3.84219403994762,-1.,0.413831367016748));
#55577=CARTESIAN_POINT('Ctrl Pts',(3.84219403994762,1.,0.413831367016748));
#55578=CARTESIAN_POINT('Ctrl Pts',(3.83503345578698,-1.,0.411353038798519));
#55579=CARTESIAN_POINT('Ctrl Pts',(3.83503345578698,1.,0.411353038798519));
#55580=CARTESIAN_POINT('Ctrl Pts',(3.82790724256471,-1.,0.40894237144746));
#55581=CARTESIAN_POINT('Ctrl Pts',(3.82790724256471,1.,0.40894237144746));
#55582=CARTESIAN_POINT('Ctrl Pts',(3.8208730391381,-1.,0.406607038258986));
#55583=CARTESIAN_POINT('Ctrl Pts',(3.8208730391381,1.,0.406607038258986));
#55584=CARTESIAN_POINT('Ctrl Pts',(3.81396374287793,-1.,0.404352694628274));
#55585=CARTESIAN_POINT('Ctrl Pts',(3.81396374287793,1.,0.404352694628274));
#55586=CARTESIAN_POINT('Ctrl Pts',(3.80716881962728,-1.,0.402181320148436));
#55587=CARTESIAN_POINT('Ctrl Pts',(3.80716881962728,1.,0.402181320148436));
#55588=CARTESIAN_POINT('Ctrl Pts',(3.80040370384546,-1.,0.400088346504601));
#55589=CARTESIAN_POINT('Ctrl Pts',(3.80040370384546,1.,0.400088346504601));
#55590=CARTESIAN_POINT('Ctrl Pts',(3.7935288716329,-1.,0.39806481868397));
#55591=CARTESIAN_POINT('Ctrl Pts',(3.7935288716329,1.,0.39806481868397));
#55592=CARTESIAN_POINT('Ctrl Pts',(3.78640521279313,-1.,0.396103205334841));
#55593=CARTESIAN_POINT('Ctrl Pts',(3.78640521279313,1.,0.396103205334841));
#55594=CARTESIAN_POINT('Ctrl Pts',(3.77894173114283,-1.,0.3942024810115));
#55595=CARTESIAN_POINT('Ctrl Pts',(3.77894173114283,1.,0.3942024810115));
#55596=CARTESIAN_POINT('Ctrl Pts',(3.77114011595967,-1.,0.392372786223433));
#55597=CARTESIAN_POINT('Ctrl Pts',(3.77114011595967,1.,0.392372786223433));
#55598=CARTESIAN_POINT('Ctrl Pts',(3.76315635033257,-1.,0.39064207297956));
#55599=CARTESIAN_POINT('Ctrl Pts',(3.76315635033257,1.,0.39064207297956));
#55600=CARTESIAN_POINT('Ctrl Pts',(3.75529302895152,-1.,0.389054775898702));
#55601=CARTESIAN_POINT('Ctrl Pts',(3.75529302895152,1.,0.389054775898702));
#55602=CARTESIAN_POINT('Ctrl Pts',(3.74792651696654,-1.,0.387663020050836));
#55603=CARTESIAN_POINT('Ctrl Pts',(3.74792651696654,1.,0.387663020050836));
#55604=CARTESIAN_POINT('Ctrl Pts',(3.74144965781276,-1.,0.386519576222252));
#55605=CARTESIAN_POINT('Ctrl Pts',(3.74144965781276,1.,0.386519576222252));
#55606=CARTESIAN_POINT('Ctrl Pts',(3.73621371845318,-1.,0.385670806454566));
#55607=CARTESIAN_POINT('Ctrl Pts',(3.73621371845318,1.,0.385670806454566));
#55608=CARTESIAN_POINT('Ctrl Pts',(3.73245705638843,-1.,0.385147887988952));
#55609=CARTESIAN_POINT('Ctrl Pts',(3.73245705638843,1.,0.385147887988952));
#55610=CARTESIAN_POINT('Ctrl Pts',(3.73072465900175,-1.,0.385001870183213));
#55611=CARTESIAN_POINT('Ctrl Pts',(3.73072465900175,1.,0.385001870183213));
#55612=CARTESIAN_POINT('Ctrl Pts',(3.73015851028356,-1.,0.385047711603463));
#55613=CARTESIAN_POINT('Ctrl Pts',(3.73015851028356,1.,0.385047711603463));
#55614=CARTESIAN_POINT('Ctrl Pts',(3.73010668803042,-1.,0.385147278814643));
#55615=CARTESIAN_POINT('Ctrl Pts',(3.73010668803042,1.,0.385147278814643));
#55616=CARTESIAN_POINT('Ctrl Pts',(3.73016218570874,-1.,0.38521431477633));
#55617=CARTESIAN_POINT('Ctrl Pts',(3.73016218570874,1.,0.38521431477633));
#55618=CARTESIAN_POINT('',(3.73017266276651,1.,0.385112848330762));
#55619=CARTESIAN_POINT('Ctrl Pts',(3.73017266276651,1.,0.385112848330762));
#55620=CARTESIAN_POINT('Ctrl Pts',(3.73017266276651,0.666666666666667,0.385112848330762));
#55621=CARTESIAN_POINT('Ctrl Pts',(3.73017266276651,0.333333333333333,0.385112848330762));
#55622=CARTESIAN_POINT('Ctrl Pts',(3.73017266276651,-0.333333333333333,
0.385112848330762));
#55623=CARTESIAN_POINT('Ctrl Pts',(3.73017266276651,-0.666666666666667,
0.385112848330763));
#55624=CARTESIAN_POINT('Ctrl Pts',(3.73017266276651,-1.,0.385112848330763));
#55625=CARTESIAN_POINT('',(4.15950947128175,1.,0.581791163835816));
#55626=CARTESIAN_POINT('Ctrl Pts',(4.15950947128175,1.,0.581791163835816));
#55627=CARTESIAN_POINT('Ctrl Pts',(4.1582129171283,1.,0.580901211463535));
#55628=CARTESIAN_POINT('Ctrl Pts',(4.15561864788576,1.,0.579124568914236));
#55629=CARTESIAN_POINT('Ctrl Pts',(4.151723761217,1.,0.576469391676689));
#55630=CARTESIAN_POINT('Ctrl Pts',(4.14652361068081,1.,0.572948736069523));
#55631=CARTESIAN_POINT('Ctrl Pts',(4.14001179830547,1.,0.568580610189775));
#55632=CARTESIAN_POINT('Ctrl Pts',(4.13348835727104,1.,0.564245279537149));
#55633=CARTESIAN_POINT('Ctrl Pts',(4.12695329951961,1.,0.559942890594774));
#55634=CARTESIAN_POINT('Ctrl Pts',(4.12040666195664,1.,0.555673636129978));
#55635=CARTESIAN_POINT('Ctrl Pts',(4.11384852024721,1.,0.551437758497033));
#55636=CARTESIAN_POINT('Ctrl Pts',(4.10727897027977,1.,0.547235539485637));
#55637=CARTESIAN_POINT('Ctrl Pts',(4.10069810243979,1.,0.543067286877758));
#55638=CARTESIAN_POINT('Ctrl Pts',(4.09410597627,1.,0.538933321179756));
#55639=CARTESIAN_POINT('Ctrl Pts',(4.08750259988885,1.,0.534833963477273));
#55640=CARTESIAN_POINT('Ctrl Pts',(4.08088789536836,1.,0.530769518728571));
#55641=CARTESIAN_POINT('Ctrl Pts',(4.07426172299847,1.,0.526740277227498));
#55642=CARTESIAN_POINT('Ctrl Pts',(4.06762394471314,1.,0.522746528603108));
#55643=CARTESIAN_POINT('Ctrl Pts',(4.06097448038013,1.,0.518788572336924));
#55644=CARTESIAN_POINT('Ctrl Pts',(4.05431335771199,1.,0.514866728193017));
#55645=CARTESIAN_POINT('Ctrl Pts',(4.04764078815447,1.,0.510981349218971));
#55646=CARTESIAN_POINT('Ctrl Pts',(4.04095715148915,1.,0.507132823288137));
#55647=CARTESIAN_POINT('Ctrl Pts',(4.03426284174272,1.,0.503321556915346));
#55648=CARTESIAN_POINT('Ctrl Pts',(4.02755813980101,1.,0.499547962340822));
#55649=CARTESIAN_POINT('Ctrl Pts',(4.02084308851832,1.,0.495812444326251));
#55650=CARTESIAN_POINT('Ctrl Pts',(4.01411733503546,1.,0.492115383418019));
#55651=CARTESIAN_POINT('Ctrl Pts',(4.0073800839099,1.,0.488457130424634));
#55652=CARTESIAN_POINT('Ctrl Pts',(4.00063045119288,1.,0.484838042421835));
#55653=CARTESIAN_POINT('Ctrl Pts',(3.99386775880679,1.,0.481258512209676));
#55654=CARTESIAN_POINT('Ctrl Pts',(3.98709184306738,1.,0.477718999122028));
#55655=CARTESIAN_POINT('Ctrl Pts',(3.98030338044409,1.,0.47422006101951));
#55656=CARTESIAN_POINT('Ctrl Pts',(3.97350414289392,1.,0.47076237961344));
#55657=CARTESIAN_POINT('Ctrl Pts',(3.9666962227393,1.,0.467346690880644));
#55658=CARTESIAN_POINT('Ctrl Pts',(3.95988133243538,1.,0.463973722115734));
#55659=CARTESIAN_POINT('Ctrl Pts',(3.95306005817364,1.,0.460644124429122));
#55660=CARTESIAN_POINT('Ctrl Pts',(3.94623117206678,1.,0.457358410451683));
#55661=CARTESIAN_POINT('Ctrl Pts',(3.93939080846298,1.,0.454116879027584));
#55662=CARTESIAN_POINT('Ctrl Pts',(3.93253407403123,1.,0.450919768356349));
#55663=CARTESIAN_POINT('Ctrl Pts',(3.92565674143416,1.,0.447767416837293));
#55664=CARTESIAN_POINT('Ctrl Pts',(3.91875701610719,1.,0.444660430230591));
#55665=CARTESIAN_POINT('Ctrl Pts',(3.91183704069153,1.,0.441599824524055));
#55666=CARTESIAN_POINT('Ctrl Pts',(3.90490512938563,1.,0.43858723545825));
#55667=CARTESIAN_POINT('Ctrl Pts',(3.89797256655462,1.,0.435624629433528));
#55668=CARTESIAN_POINT('Ctrl Pts',(3.89104947940611,1.,0.432713929544459));
#55669=CARTESIAN_POINT('Ctrl Pts',(3.88414070943341,1.,0.429856640579741));
#55670=CARTESIAN_POINT('Ctrl Pts',(3.87724240306597,1.,0.427053541173458));
#55671=CARTESIAN_POINT('Ctrl Pts',(3.87033643487851,1.,0.424304173195111));
#55672=CARTESIAN_POINT('Ctrl Pts',(3.86339652542709,1.,0.421607423177534));
#55673=CARTESIAN_POINT('Ctrl Pts',(3.85639825647996,1.,0.418962468086773));
#55674=CARTESIAN_POINT('Ctrl Pts',(3.84932864157497,1.,0.416369678052907));
#55675=CARTESIAN_POINT('Ctrl Pts',(3.84219403994762,1.,0.413831367016748));
#55676=CARTESIAN_POINT('Ctrl Pts',(3.83503345578698,1.,0.411353038798519));
#55677=CARTESIAN_POINT('Ctrl Pts',(3.82790724256471,1.,0.40894237144746));
#55678=CARTESIAN_POINT('Ctrl Pts',(3.8208730391381,1.,0.406607038258986));
#55679=CARTESIAN_POINT('Ctrl Pts',(3.81396374287793,1.,0.404352694628274));
#55680=CARTESIAN_POINT('Ctrl Pts',(3.80716881962728,1.,0.402181320148436));
#55681=CARTESIAN_POINT('Ctrl Pts',(3.80040370384546,1.,0.400088346504601));
#55682=CARTESIAN_POINT('Ctrl Pts',(3.7935288716329,1.,0.39806481868397));
#55683=CARTESIAN_POINT('Ctrl Pts',(3.78640521279313,1.,0.396103205334841));
#55684=CARTESIAN_POINT('Ctrl Pts',(3.77894173114283,1.,0.3942024810115));
#55685=CARTESIAN_POINT('Ctrl Pts',(3.77114011595967,1.,0.392372786223433));
#55686=CARTESIAN_POINT('Ctrl Pts',(3.76315635033257,1.,0.39064207297956));
#55687=CARTESIAN_POINT('Ctrl Pts',(3.75529302895152,1.,0.389054775898702));
#55688=CARTESIAN_POINT('Ctrl Pts',(3.74792651696654,1.,0.387663020050836));
#55689=CARTESIAN_POINT('Ctrl Pts',(3.74144965781276,1.,0.386519576222252));
#55690=CARTESIAN_POINT('Ctrl Pts',(3.73621371845318,1.,0.385670806454566));
#55691=CARTESIAN_POINT('Ctrl Pts',(3.73273893363406,1.,0.385187124634207));
#55692=CARTESIAN_POINT('Ctrl Pts',(3.73106082862548,1.,0.385031656499164));
#55693=CARTESIAN_POINT('Ctrl Pts',(3.73040527621055,1.,0.385037797881504));
#55694=CARTESIAN_POINT('Ctrl Pts',(3.73021431755274,1.,0.385087139000375));
#55695=CARTESIAN_POINT('Ctrl Pts',(3.73017266276651,1.,0.385112848330762));
#55696=CARTESIAN_POINT('',(4.15950947128175,0.,0.581791163835816));
#55697=CARTESIAN_POINT('Ctrl Pts',(3.66663282329846,-1.,0.7863229229206));
#55698=CARTESIAN_POINT('Ctrl Pts',(3.66663282329846,1.,0.7863229229206));
#55699=CARTESIAN_POINT('Ctrl Pts',(3.66655932661986,-1.,0.786369528183326));
#55700=CARTESIAN_POINT('Ctrl Pts',(3.66655932661986,1.,0.786369528183326));
#55701=CARTESIAN_POINT('Ctrl Pts',(3.66657784455334,-1.,0.786480236185697));
#55702=CARTESIAN_POINT('Ctrl Pts',(3.66657784455334,1.,0.786480236185697));
#55703=CARTESIAN_POINT('Ctrl Pts',(3.66710211820482,-1.,0.786698783542764));
#55704=CARTESIAN_POINT('Ctrl Pts',(3.66710211820482,1.,0.786698783542764));
#55705=CARTESIAN_POINT('Ctrl Pts',(3.66879484801113,-1.,0.787095252590501));
#55706=CARTESIAN_POINT('Ctrl Pts',(3.66879484801113,1.,0.787095252590501));
#55707=CARTESIAN_POINT('Ctrl Pts',(3.67252923663655,-1.,0.787758799995743));
#55708=CARTESIAN_POINT('Ctrl Pts',(3.67252923663655,1.,0.787758799995743));
#55709=CARTESIAN_POINT('Ctrl Pts',(3.67777119516252,-1.,0.788569566220286));
#55710=CARTESIAN_POINT('Ctrl Pts',(3.67777119516252,1.,0.788569566220286));
#55711=CARTESIAN_POINT('Ctrl Pts',(3.68428439783905,-1.,0.789483546064387));
#55712=CARTESIAN_POINT('Ctrl Pts',(3.68428439783905,1.,0.789483546064387));
#55713=CARTESIAN_POINT('Ctrl Pts',(3.69172044327364,-1.,0.790436284988788));
#55714=CARTESIAN_POINT('Ctrl Pts',(3.69172044327364,1.,0.790436284988788));
#55715=CARTESIAN_POINT('Ctrl Pts',(3.69968940808721,-1.,0.79135657569598));
#55716=CARTESIAN_POINT('Ctrl Pts',(3.69968940808721,1.,0.79135657569598));
#55717=CARTESIAN_POINT('Ctrl Pts',(3.70781724021806,-1.,0.792177688845818));
#55718=CARTESIAN_POINT('Ctrl Pts',(3.70781724021806,1.,0.792177688845818));
#55719=CARTESIAN_POINT('Ctrl Pts',(3.71580242396124,-1.,0.792848377370287));
#55720=CARTESIAN_POINT('Ctrl Pts',(3.71580242396124,1.,0.792848377370287));
#55721=CARTESIAN_POINT('Ctrl Pts',(3.72348797293734,-1.,0.793347023784205));
#55722=CARTESIAN_POINT('Ctrl Pts',(3.72348797293734,1.,0.793347023784205));
#55723=CARTESIAN_POINT('Ctrl Pts',(3.73086914695805,-1.,0.793682750269684));
#55724=CARTESIAN_POINT('Ctrl Pts',(3.73086914695805,1.,0.793682750269684));
#55725=CARTESIAN_POINT('Ctrl Pts',(3.73803280541687,-1.,0.793882700937017));
#55726=CARTESIAN_POINT('Ctrl Pts',(3.73803280541687,1.,0.793882700937017));
#55727=CARTESIAN_POINT('Ctrl Pts',(3.74511357728861,-1.,0.793982700459952));
#55728=CARTESIAN_POINT('Ctrl Pts',(3.74511357728861,1.,0.793982700459952));
#55729=CARTESIAN_POINT('Ctrl Pts',(3.75224692493864,-1.,0.794017347371378));
#55730=CARTESIAN_POINT('Ctrl Pts',(3.75224692493864,1.,0.794017347371378));
#55731=CARTESIAN_POINT('Ctrl Pts',(3.75951468666257,-1.,0.794008429134908));
#55732=CARTESIAN_POINT('Ctrl Pts',(3.75951468666257,1.,0.794008429134908));
#55733=CARTESIAN_POINT('Ctrl Pts',(3.76692626931111,-1.,0.793961083688992));
#55734=CARTESIAN_POINT('Ctrl Pts',(3.76692626931111,1.,0.793961083688992));
#55735=CARTESIAN_POINT('Ctrl Pts',(3.77444863801212,-1.,0.793870523787408));
#55736=CARTESIAN_POINT('Ctrl Pts',(3.77444863801212,1.,0.793870523787408));
#55737=CARTESIAN_POINT('Ctrl Pts',(3.78202460377598,-1.,0.793726235781301));
#55738=CARTESIAN_POINT('Ctrl Pts',(3.78202460377598,1.,0.793726235781301));
#55739=CARTESIAN_POINT('Ctrl Pts',(3.78959439439235,-1.,0.793516871680994));
#55740=CARTESIAN_POINT('Ctrl Pts',(3.78959439439235,1.,0.793516871680994));
#55741=CARTESIAN_POINT('Ctrl Pts',(3.79711921389897,-1.,0.793235612973274));
#55742=CARTESIAN_POINT('Ctrl Pts',(3.79711921389897,1.,0.793235612973274));
#55743=CARTESIAN_POINT('Ctrl Pts',(3.80459229925637,-1.,0.792882695234778));
#55744=CARTESIAN_POINT('Ctrl Pts',(3.80459229925637,1.,0.792882695234778));
#55745=CARTESIAN_POINT('Ctrl Pts',(3.81202588694756,-1.,0.792462483517635));
#55746=CARTESIAN_POINT('Ctrl Pts',(3.81202588694756,1.,0.792462483517635));
#55747=CARTESIAN_POINT('Ctrl Pts',(3.81944345442249,-1.,0.791981740718635));
#55748=CARTESIAN_POINT('Ctrl Pts',(3.81944345442249,1.,0.791981740718635));
#55749=CARTESIAN_POINT('Ctrl Pts',(3.82687033899792,-1.,0.791447528662369));
#55750=CARTESIAN_POINT('Ctrl Pts',(3.82687033899792,1.,0.791447528662369));
#55751=CARTESIAN_POINT('Ctrl Pts',(3.83432392054786,-1.,0.790865012705301));
#55752=CARTESIAN_POINT('Ctrl Pts',(3.83432392054786,1.,0.790865012705301));
#55753=CARTESIAN_POINT('Ctrl Pts',(3.84180762342454,-1.,0.790236124191243));
#55754=CARTESIAN_POINT('Ctrl Pts',(3.84180762342454,1.,0.790236124191243));
#55755=CARTESIAN_POINT('Ctrl Pts',(3.84931637808894,-1.,0.789560798155583));
#55756=CARTESIAN_POINT('Ctrl Pts',(3.84931637808894,1.,0.789560798155583));
#55757=CARTESIAN_POINT('Ctrl Pts',(3.85683995872529,-1.,0.788837734090672));
#55758=CARTESIAN_POINT('Ctrl Pts',(3.85683995872529,1.,0.788837734090672));
#55759=CARTESIAN_POINT('Ctrl Pts',(3.86436702561345,-1.,0.788065315093778));
#55760=CARTESIAN_POINT('Ctrl Pts',(3.86436702561345,1.,0.788065315093778));
#55761=CARTESIAN_POINT('Ctrl Pts',(3.87188916600912,-1.,0.787242527617999));
#55762=CARTESIAN_POINT('Ctrl Pts',(3.87188916600912,1.,0.787242527617999));
#55763=CARTESIAN_POINT('Ctrl Pts',(3.8794040281819,-1.,0.786369675812609));
#55764=CARTESIAN_POINT('Ctrl Pts',(3.8794040281819,1.,0.786369675812609));
#55765=CARTESIAN_POINT('Ctrl Pts',(3.88691313167398,-1.,0.785447890340731));
#55766=CARTESIAN_POINT('Ctrl Pts',(3.88691313167398,1.,0.785447890340731));
#55767=CARTESIAN_POINT('Ctrl Pts',(3.89442039235103,-1.,0.784478799358337));
#55768=CARTESIAN_POINT('Ctrl Pts',(3.89442039235103,1.,0.784478799358337));
#55769=CARTESIAN_POINT('Ctrl Pts',(3.9019303904397,-1.,0.783464141529082));
#55770=CARTESIAN_POINT('Ctrl Pts',(3.9019303904397,1.,0.783464141529082));
#55771=CARTESIAN_POINT('Ctrl Pts',(3.90944671004542,-1.,0.782405395622765));
#55772=CARTESIAN_POINT('Ctrl Pts',(3.90944671004542,1.,0.782405395622765));
#55773=CARTESIAN_POINT('Ctrl Pts',(3.91697036054676,-1.,0.781303428618367));
#55774=CARTESIAN_POINT('Ctrl Pts',(3.91697036054676,1.,0.781303428618367));
#55775=CARTESIAN_POINT('Ctrl Pts',(3.92450058323823,-1.,0.780158678615543));
#55776=CARTESIAN_POINT('Ctrl Pts',(3.92450058323823,1.,0.780158678615543));
#55777=CARTESIAN_POINT('Ctrl Pts',(3.93203552473174,-1.,0.778971308134821));
#55778=CARTESIAN_POINT('Ctrl Pts',(3.93203552473174,1.,0.778971308134821));
#55779=CARTESIAN_POINT('Ctrl Pts',(3.93957296768103,-1.,0.777741370568559));
#55780=CARTESIAN_POINT('Ctrl Pts',(3.93957296768103,1.,0.777741370568559));
#55781=CARTESIAN_POINT('Ctrl Pts',(3.94711101619447,-1.,0.776468966697922));
#55782=CARTESIAN_POINT('Ctrl Pts',(3.94711101619447,1.,0.776468966697922));
#55783=CARTESIAN_POINT('Ctrl Pts',(3.9546488545231,-1.,0.775154418039352));
#55784=CARTESIAN_POINT('Ctrl Pts',(3.9546488545231,1.,0.775154418039352));
#55785=CARTESIAN_POINT('Ctrl Pts',(3.96218649639807,-1.,0.773798212026566));
#55786=CARTESIAN_POINT('Ctrl Pts',(3.96218649639807,1.,0.773798212026566));
#55787=CARTESIAN_POINT('Ctrl Pts',(3.96972446532772,-1.,0.772400931772137));
#55788=CARTESIAN_POINT('Ctrl Pts',(3.96972446532772,1.,0.772400931772137));
#55789=CARTESIAN_POINT('Ctrl Pts',(3.97726349165488,-1.,0.770963190030471));
#55790=CARTESIAN_POINT('Ctrl Pts',(3.97726349165488,1.,0.770963190030471));
#55791=CARTESIAN_POINT('Ctrl Pts',(3.98480422348451,-1.,0.769485566245545));
#55792=CARTESIAN_POINT('Ctrl Pts',(3.98480422348451,1.,0.769485566245545));
#55793=CARTESIAN_POINT('Ctrl Pts',(3.9923468788101,-1.,0.767968531377915));
#55794=CARTESIAN_POINT('Ctrl Pts',(3.9923468788101,1.,0.767968531377915));
#55795=CARTESIAN_POINT('Ctrl Pts',(3.99989129179622,-1.,0.766412457136064));
#55796=CARTESIAN_POINT('Ctrl Pts',(3.99989129179622,1.,0.766412457136064));
#55797=CARTESIAN_POINT('Ctrl Pts',(4.00743706791509,-1.,0.764817648785198));
#55798=CARTESIAN_POINT('Ctrl Pts',(4.00743706791509,1.,0.764817648785198));
#55799=CARTESIAN_POINT('Ctrl Pts',(4.01498370680496,-1.,0.763184371182936));
#55800=CARTESIAN_POINT('Ctrl Pts',(4.01498370680496,1.,0.763184371182936));
#55801=CARTESIAN_POINT('Ctrl Pts',(4.02253072741268,-1.,0.761512875859805));
#55802=CARTESIAN_POINT('Ctrl Pts',(4.02253072741268,1.,0.761512875859805));
#55803=CARTESIAN_POINT('Ctrl Pts',(4.03007781954412,-1.,0.759803433243752));
#55804=CARTESIAN_POINT('Ctrl Pts',(4.03007781954412,1.,0.759803433243752));
#55805=CARTESIAN_POINT('Ctrl Pts',(4.03762485803119,-1.,0.758056338884945));
#55806=CARTESIAN_POINT('Ctrl Pts',(4.03762485803119,1.,0.758056338884945));
#55807=CARTESIAN_POINT('Ctrl Pts',(4.04517182653997,-1.,0.756271902369581));
#55808=CARTESIAN_POINT('Ctrl Pts',(4.04517182653997,1.,0.756271902369581));
#55809=CARTESIAN_POINT('Ctrl Pts',(4.05271876687915,-1.,0.754450441816078));
#55810=CARTESIAN_POINT('Ctrl Pts',(4.05271876687915,1.,0.754450441816078));
#55811=CARTESIAN_POINT('Ctrl Pts',(4.06026572221515,-1.,0.752592276483073));
#55812=CARTESIAN_POINT('Ctrl Pts',(4.06026572221515,1.,0.752592276483073));
#55813=CARTESIAN_POINT('Ctrl Pts',(4.06781267242378,-1.,0.750697720484037));
#55814=CARTESIAN_POINT('Ctrl Pts',(4.06781267242378,1.,0.750697720484037));
#55815=CARTESIAN_POINT('Ctrl Pts',(4.07535951056152,-1.,0.748767076680558));
#55816=CARTESIAN_POINT('Ctrl Pts',(4.07535951056152,1.,0.748767076680558));
#55817=CARTESIAN_POINT('Ctrl Pts',(4.08290608095642,-1.,0.746800631492316));
#55818=CARTESIAN_POINT('Ctrl Pts',(4.08290608095642,1.,0.746800631492316));
#55819=CARTESIAN_POINT('Ctrl Pts',(4.09045220253573,-1.,0.744798649706501));
#55820=CARTESIAN_POINT('Ctrl Pts',(4.09045220253573,1.,0.744798649706501));
#55821=CARTESIAN_POINT('Ctrl Pts',(4.09799769702611,-1.,0.742761369689842));
#55822=CARTESIAN_POINT('Ctrl Pts',(4.09799769702611,1.,0.742761369689842));
#55823=CARTESIAN_POINT('Ctrl Pts',(4.10554241757547,-1.,0.740688998553377));
#55824=CARTESIAN_POINT('Ctrl Pts',(4.10554241757547,1.,0.740688998553377));
#55825=CARTESIAN_POINT('Ctrl Pts',(4.11308626951927,-1.,0.738581708225844));
#55826=CARTESIAN_POINT('Ctrl Pts',(4.11308626951927,1.,0.738581708225844));
#55827=CARTESIAN_POINT('Ctrl Pts',(4.120629196238,-1.,0.736439634331345));
#55828=CARTESIAN_POINT('Ctrl Pts',(4.120629196238,1.,0.736439634331345));
#55829=CARTESIAN_POINT('Ctrl Pts',(4.12666277570844,-1.,0.734698226764093));
#55830=CARTESIAN_POINT('Ctrl Pts',(4.12666277570844,1.,0.734698226764093));
#55831=CARTESIAN_POINT('Ctrl Pts',(4.13118752795207,-1.,0.733376589323547));
#55832=CARTESIAN_POINT('Ctrl Pts',(4.13118752795207,1.,0.733376589323547));
#55833=CARTESIAN_POINT('Ctrl Pts',(4.1342038373684,-1.,0.73248857513516));
#55834=CARTESIAN_POINT('Ctrl Pts',(4.1342038373684,1.,0.73248857513516));
#55835=CARTESIAN_POINT('Ctrl Pts',(4.13571194405636,-1.,0.732042837400621));
#55836=CARTESIAN_POINT('Ctrl Pts',(4.13571194405636,1.,0.732042837400621));
#55837=CARTESIAN_POINT('',(3.66661143271685,1.,0.786422660831985));
#55838=CARTESIAN_POINT('Ctrl Pts',(3.66661143271685,-1.,0.786422660831986));
#55839=CARTESIAN_POINT('Ctrl Pts',(3.66661143271685,-0.666666666666667,
0.786422660831986));
#55840=CARTESIAN_POINT('Ctrl Pts',(3.66661143271685,-0.333333333333333,
0.786422660831986));
#55841=CARTESIAN_POINT('Ctrl Pts',(3.66661143271685,0.333333333333333,0.786422660831986));
#55842=CARTESIAN_POINT('Ctrl Pts',(3.66661143271685,0.666666666666667,0.786422660831986));
#55843=CARTESIAN_POINT('Ctrl Pts',(3.66661143271685,1.,0.786422660831986));
#55844=CARTESIAN_POINT('',(4.13571194405636,1.,0.732042837400621));
#55845=CARTESIAN_POINT('',(4.13571194405636,0.,0.732042837400621));
#55846=CARTESIAN_POINT('Ctrl Pts',(3.66661143271685,1.,0.786422660831985));
#55847=CARTESIAN_POINT('Ctrl Pts',(3.6666431041522,1.,0.786459983895432));
#55848=CARTESIAN_POINT('Ctrl Pts',(3.66680946938292,1.,0.786565919558984));
#55849=CARTESIAN_POINT('Ctrl Pts',(3.66743103898702,1.,0.786774337198063));
#55850=CARTESIAN_POINT('Ctrl Pts',(3.66907505398677,1.,0.787145041181546));
#55851=CARTESIAN_POINT('Ctrl Pts',(3.67252923663655,1.,0.787758799995743));
#55852=CARTESIAN_POINT('Ctrl Pts',(3.67777119516252,1.,0.788569566220286));
#55853=CARTESIAN_POINT('Ctrl Pts',(3.68428439783905,1.,0.789483546064387));
#55854=CARTESIAN_POINT('Ctrl Pts',(3.69172044327364,1.,0.790436284988788));
#55855=CARTESIAN_POINT('Ctrl Pts',(3.69968940808721,1.,0.79135657569598));
#55856=CARTESIAN_POINT('Ctrl Pts',(3.70781724021806,1.,0.792177688845818));
#55857=CARTESIAN_POINT('Ctrl Pts',(3.71580242396124,1.,0.792848377370287));
#55858=CARTESIAN_POINT('Ctrl Pts',(3.72348797293734,1.,0.793347023784205));
#55859=CARTESIAN_POINT('Ctrl Pts',(3.73086914695805,1.,0.793682750269684));
#55860=CARTESIAN_POINT('Ctrl Pts',(3.73803280541687,1.,0.793882700937017));
#55861=CARTESIAN_POINT('Ctrl Pts',(3.74511357728861,1.,0.793982700459952));
#55862=CARTESIAN_POINT('Ctrl Pts',(3.75224692493864,1.,0.794017347371378));
#55863=CARTESIAN_POINT('Ctrl Pts',(3.75951468666257,1.,0.794008429134908));
#55864=CARTESIAN_POINT('Ctrl Pts',(3.76692626931111,1.,0.793961083688992));
#55865=CARTESIAN_POINT('Ctrl Pts',(3.77444863801212,1.,0.793870523787408));
#55866=CARTESIAN_POINT('Ctrl Pts',(3.78202460377598,1.,0.793726235781301));
#55867=CARTESIAN_POINT('Ctrl Pts',(3.78959439439235,1.,0.793516871680994));
#55868=CARTESIAN_POINT('Ctrl Pts',(3.79711921389897,1.,0.793235612973274));
#55869=CARTESIAN_POINT('Ctrl Pts',(3.80459229925637,1.,0.792882695234778));
#55870=CARTESIAN_POINT('Ctrl Pts',(3.81202588694756,1.,0.792462483517635));
#55871=CARTESIAN_POINT('Ctrl Pts',(3.81944345442249,1.,0.791981740718635));
#55872=CARTESIAN_POINT('Ctrl Pts',(3.82687033899792,1.,0.791447528662369));
#55873=CARTESIAN_POINT('Ctrl Pts',(3.83432392054786,1.,0.790865012705301));
#55874=CARTESIAN_POINT('Ctrl Pts',(3.84180762342454,1.,0.790236124191243));
#55875=CARTESIAN_POINT('Ctrl Pts',(3.84931637808894,1.,0.789560798155583));
#55876=CARTESIAN_POINT('Ctrl Pts',(3.85683995872529,1.,0.788837734090672));
#55877=CARTESIAN_POINT('Ctrl Pts',(3.86436702561345,1.,0.788065315093778));
#55878=CARTESIAN_POINT('Ctrl Pts',(3.87188916600912,1.,0.787242527617999));
#55879=CARTESIAN_POINT('Ctrl Pts',(3.8794040281819,1.,0.786369675812609));
#55880=CARTESIAN_POINT('Ctrl Pts',(3.88691313167398,1.,0.785447890340731));
#55881=CARTESIAN_POINT('Ctrl Pts',(3.89442039235103,1.,0.784478799358337));
#55882=CARTESIAN_POINT('Ctrl Pts',(3.9019303904397,1.,0.783464141529082));
#55883=CARTESIAN_POINT('Ctrl Pts',(3.90944671004542,1.,0.782405395622765));
#55884=CARTESIAN_POINT('Ctrl Pts',(3.91697036054676,1.,0.781303428618367));
#55885=CARTESIAN_POINT('Ctrl Pts',(3.92450058323823,1.,0.780158678615543));
#55886=CARTESIAN_POINT('Ctrl Pts',(3.93203552473174,1.,0.778971308134821));
#55887=CARTESIAN_POINT('Ctrl Pts',(3.93957296768103,1.,0.777741370568559));
#55888=CARTESIAN_POINT('Ctrl Pts',(3.94711101619447,1.,0.776468966697922));
#55889=CARTESIAN_POINT('Ctrl Pts',(3.9546488545231,1.,0.775154418039352));
#55890=CARTESIAN_POINT('Ctrl Pts',(3.96218649639807,1.,0.773798212026566));
#55891=CARTESIAN_POINT('Ctrl Pts',(3.96972446532772,1.,0.772400931772137));
#55892=CARTESIAN_POINT('Ctrl Pts',(3.97726349165488,1.,0.770963190030471));
#55893=CARTESIAN_POINT('Ctrl Pts',(3.98480422348451,1.,0.769485566245545));
#55894=CARTESIAN_POINT('Ctrl Pts',(3.9923468788101,1.,0.767968531377915));
#55895=CARTESIAN_POINT('Ctrl Pts',(3.99989129179622,1.,0.766412457136064));
#55896=CARTESIAN_POINT('Ctrl Pts',(4.00743706791509,1.,0.764817648785198));
#55897=CARTESIAN_POINT('Ctrl Pts',(4.01498370680496,1.,0.763184371182936));
#55898=CARTESIAN_POINT('Ctrl Pts',(4.02253072741268,1.,0.761512875859805));
#55899=CARTESIAN_POINT('Ctrl Pts',(4.03007781954412,1.,0.759803433243752));
#55900=CARTESIAN_POINT('Ctrl Pts',(4.03762485803119,1.,0.758056338884945));
#55901=CARTESIAN_POINT('Ctrl Pts',(4.04517182653997,1.,0.756271902369581));
#55902=CARTESIAN_POINT('Ctrl Pts',(4.05271876687915,1.,0.754450441816078));
#55903=CARTESIAN_POINT('Ctrl Pts',(4.06026572221515,1.,0.752592276483073));
#55904=CARTESIAN_POINT('Ctrl Pts',(4.06781267242378,1.,0.750697720484037));
#55905=CARTESIAN_POINT('Ctrl Pts',(4.07535951056152,1.,0.748767076680558));
#55906=CARTESIAN_POINT('Ctrl Pts',(4.08290608095642,1.,0.746800631492316));
#55907=CARTESIAN_POINT('Ctrl Pts',(4.09045220253573,1.,0.744798649706501));
#55908=CARTESIAN_POINT('Ctrl Pts',(4.09799769702611,1.,0.742761369689842));
#55909=CARTESIAN_POINT('Ctrl Pts',(4.10554241757547,1.,0.740688998553377));
#55910=CARTESIAN_POINT('Ctrl Pts',(4.11308626951927,1.,0.738581708225844));
#55911=CARTESIAN_POINT('Ctrl Pts',(4.120629196238,1.,0.736439634331345));
#55912=CARTESIAN_POINT('Ctrl Pts',(4.12666277570844,1.,0.734698226764093));
#55913=CARTESIAN_POINT('Ctrl Pts',(4.13118752795207,1.,0.733376589323547));
#55914=CARTESIAN_POINT('Ctrl Pts',(4.1342038373684,1.,0.73248857513516));
#55915=CARTESIAN_POINT('Ctrl Pts',(4.13571194405636,1.,0.732042837400621));
#55916=CARTESIAN_POINT('Origin',(4.13571194405636,0.,0.732042837400621));
#55917=CARTESIAN_POINT('',(4.15950947128175,1.,0.581791163835816));
#55918=CARTESIAN_POINT('Origin',(0.,0.,0.));
#55919=CARTESIAN_POINT('',(3.62400312501245,1.,0.963899035117249));
#55920=CARTESIAN_POINT('Origin',(0.,1.,0.));
#55921=CARTESIAN_POINT('Ctrl Pts',(3.62400312501245,1.,0.963899035117249));
#55922=CARTESIAN_POINT('Ctrl Pts',(3.62400312501245,0.666666666666667,0.963899035117249));
#55923=CARTESIAN_POINT('Ctrl Pts',(3.62400312501245,0.333333333333333,0.963899035117249));
#55924=CARTESIAN_POINT('Ctrl Pts',(3.62400312501245,-0.333333333333333,
0.963899035117249));
#55925=CARTESIAN_POINT('Ctrl Pts',(3.62400312501245,-0.666666666666667,
0.96389903511725));
#55926=CARTESIAN_POINT('Ctrl Pts',(3.62400312501245,-1.,0.96389903511725));
#55927=CARTESIAN_POINT('Ctrl Pts',(4.01728681790024,-1.,1.22531898815164));
#55928=CARTESIAN_POINT('Ctrl Pts',(4.01728681790024,1.,1.22531898815164));
#55929=CARTESIAN_POINT('Ctrl Pts',(4.0161454457032,-1.,1.22423716681447));
#55930=CARTESIAN_POINT('Ctrl Pts',(4.0161454457032,1.,1.22423716681447));
#55931=CARTESIAN_POINT('Ctrl Pts',(4.01386104434674,-1.,1.22207656456199));
#55932=CARTESIAN_POINT('Ctrl Pts',(4.01386104434674,1.,1.22207656456199));
#55933=CARTESIAN_POINT('Ctrl Pts',(4.01042947142681,-1.,1.21884478244983));
#55934=CARTESIAN_POINT('Ctrl Pts',(4.01042947142681,1.,1.21884478244983));
#55935=CARTESIAN_POINT('Ctrl Pts',(4.00584409524937,-1.,1.21455398918813));
#55936=CARTESIAN_POINT('Ctrl Pts',(4.00584409524937,1.,1.21455398918813));
#55937=CARTESIAN_POINT('Ctrl Pts',(4.00009577952534,-1.,1.20922097030107));
#55938=CARTESIAN_POINT('Ctrl Pts',(4.00009577952534,1.,1.20922097030107));
#55939=CARTESIAN_POINT('Ctrl Pts',(3.99433084800649,-1.,1.2039185237544));
#55940=CARTESIAN_POINT('Ctrl Pts',(3.99433084800649,1.,1.2039185237544));
#55941=CARTESIAN_POINT('Ctrl Pts',(3.98854928957287,-1.,1.19864679609596));
#55942=CARTESIAN_POINT('Ctrl Pts',(3.98854928957287,1.,1.19864679609596));
#55943=CARTESIAN_POINT('Ctrl Pts',(3.98275111052015,-1.,1.19340598349307));
#55944=CARTESIAN_POINT('Ctrl Pts',(3.98275111052015,1.,1.19340598349307));
#55945=CARTESIAN_POINT('Ctrl Pts',(3.97693634766926,-1.,1.18819633715285));
#55946=CARTESIAN_POINT('Ctrl Pts',(3.97693634766926,1.,1.18819633715285));
#55947=CARTESIAN_POINT('Ctrl Pts',(3.9711050516465,-1.,1.18301815039596));
#55948=CARTESIAN_POINT('Ctrl Pts',(3.9711050516465,1.,1.18301815039596));
#55949=CARTESIAN_POINT('Ctrl Pts',(3.96525726357682,-1.,1.17787174135446));
#55950=CARTESIAN_POINT('Ctrl Pts',(3.96525726357682,1.,1.17787174135446));
#55951=CARTESIAN_POINT('Ctrl Pts',(3.95939299213164,-1.,1.17275743590327));
#55952=CARTESIAN_POINT('Ctrl Pts',(3.95939299213164,1.,1.17275743590327));
#55953=CARTESIAN_POINT('Ctrl Pts',(3.95351219510062,-1.,1.16767555244495));
#55954=CARTESIAN_POINT('Ctrl Pts',(3.95351219510062,1.,1.16767555244495));
#55955=CARTESIAN_POINT('Ctrl Pts',(3.9476147478092,-1.,1.16262637999261));
#55956=CARTESIAN_POINT('Ctrl Pts',(3.9476147478092,1.,1.16262637999261));
#55957=CARTESIAN_POINT('Ctrl Pts',(3.94170046685542,-1.,1.15761018341061));
#55958=CARTESIAN_POINT('Ctrl Pts',(3.94170046685542,1.,1.15761018341061));
#55959=CARTESIAN_POINT('Ctrl Pts',(3.9357691705651,-1.,1.15262722716391));
#55960=CARTESIAN_POINT('Ctrl Pts',(3.9357691705651,1.,1.15262722716391));
#55961=CARTESIAN_POINT('Ctrl Pts',(3.92982073294334,-1.,1.14767779451147));
#55962=CARTESIAN_POINT('Ctrl Pts',(3.92982073294334,1.,1.14767779451147));
#55963=CARTESIAN_POINT('Ctrl Pts',(3.92385513133937,-1.,1.14276220561575));
#55964=CARTESIAN_POINT('Ctrl Pts',(3.92385513133937,1.,1.14276220561575));
#55965=CARTESIAN_POINT('Ctrl Pts',(3.91787251936688,-1.,1.13788084225511));
#55966=CARTESIAN_POINT('Ctrl Pts',(3.91787251936688,1.,1.13788084225511));
#55967=CARTESIAN_POINT('Ctrl Pts',(3.91187321145495,-1.,1.13303414693849));
#55968=CARTESIAN_POINT('Ctrl Pts',(3.91187321145495,1.,1.13303414693849));
#55969=CARTESIAN_POINT('Ctrl Pts',(3.90585753318622,-1.,1.12822258281518));
#55970=CARTESIAN_POINT('Ctrl Pts',(3.90585753318622,1.,1.12822258281518));
#55971=CARTESIAN_POINT('Ctrl Pts',(3.89982569749978,-1.,1.12344660099029));
#55972=CARTESIAN_POINT('Ctrl Pts',(3.89982569749978,1.,1.12344660099029));
#55973=CARTESIAN_POINT('Ctrl Pts',(3.89377768340362,-1.,1.11870660794609));
#55974=CARTESIAN_POINT('Ctrl Pts',(3.89377768340362,1.,1.11870660794609));
#55975=CARTESIAN_POINT('Ctrl Pts',(3.88771308285229,-1.,1.11400292434447));
#55976=CARTESIAN_POINT('Ctrl Pts',(3.88771308285229,1.,1.11400292434447));
#55977=CARTESIAN_POINT('Ctrl Pts',(3.88163105531791,-1.,1.10933577224029));
#55978=CARTESIAN_POINT('Ctrl Pts',(3.88163105531791,1.,1.10933577224029));
#55979=CARTESIAN_POINT('Ctrl Pts',(3.87553067187566,-1.,1.10470536603303));
#55980=CARTESIAN_POINT('Ctrl Pts',(3.87553067187566,1.,1.10470536603303));
#55981=CARTESIAN_POINT('Ctrl Pts',(3.86941120134872,-1.,1.10011198761203));
#55982=CARTESIAN_POINT('Ctrl Pts',(3.86941120134872,1.,1.10011198761203));
#55983=CARTESIAN_POINT('Ctrl Pts',(3.86327241021242,-1.,1.09555606505012));
#55984=CARTESIAN_POINT('Ctrl Pts',(3.86327241021242,1.,1.09555606505012));
#55985=CARTESIAN_POINT('Ctrl Pts',(3.85711487933911,-1.,1.09103825516288));
#55986=CARTESIAN_POINT('Ctrl Pts',(3.85711487933911,1.,1.09103825516288));
#55987=CARTESIAN_POINT('Ctrl Pts',(3.8509402522269,-1.,1.08655950846377));
#55988=CARTESIAN_POINT('Ctrl Pts',(3.8509402522269,1.,1.08655950846377));
#55989=CARTESIAN_POINT('Ctrl Pts',(3.84475048030615,-1.,1.08212087917986));
#55990=CARTESIAN_POINT('Ctrl Pts',(3.84475048030615,1.,1.08212087917986));
#55991=CARTESIAN_POINT('Ctrl Pts',(3.83854714117486,-1.,1.07772335353856));
#55992=CARTESIAN_POINT('Ctrl Pts',(3.83854714117486,1.,1.07772335353856));
#55993=CARTESIAN_POINT('Ctrl Pts',(3.83233071195145,-1.,1.0733676663346));
#55994=CARTESIAN_POINT('Ctrl Pts',(3.83233071195145,1.,1.0733676663346));
#55995=CARTESIAN_POINT('Ctrl Pts',(3.82609989967278,-1.,1.0690541318036));
#55996=CARTESIAN_POINT('Ctrl Pts',(3.82609989967278,1.,1.0690541318036));
#55997=CARTESIAN_POINT('Ctrl Pts',(3.81985083953012,-1.,1.06478244038931));
#55998=CARTESIAN_POINT('Ctrl Pts',(3.81985083953012,1.,1.06478244038931));
#55999=CARTESIAN_POINT('Ctrl Pts',(3.81357866117485,-1.,1.06055206187298));
#56000=CARTESIAN_POINT('Ctrl Pts',(3.81357866117485,1.,1.06055206187298));
#56001=CARTESIAN_POINT('Ctrl Pts',(3.80727913637784,-1.,1.05636266918643));
#56002=CARTESIAN_POINT('Ctrl Pts',(3.80727913637784,1.,1.05636266918643));
#56003=CARTESIAN_POINT('Ctrl Pts',(3.80095039790678,-1.,1.05221457990015));
#56004=CARTESIAN_POINT('Ctrl Pts',(3.80095039790678,1.,1.05221457990015));
#56005=CARTESIAN_POINT('Ctrl Pts',(3.79459440308793,-1.,1.04810913267641));
#56006=CARTESIAN_POINT('Ctrl Pts',(3.79459440308793,1.,1.04810913267641));
#56007=CARTESIAN_POINT('Ctrl Pts',(3.78821910787195,-1.,1.04404924374426));
#56008=CARTESIAN_POINT('Ctrl Pts',(3.78821910787195,1.,1.04404924374426));
#56009=CARTESIAN_POINT('Ctrl Pts',(3.78183535008192,-1.,1.04003862055804));
#56010=CARTESIAN_POINT('Ctrl Pts',(3.78183535008192,1.,1.04003862055804));
#56011=CARTESIAN_POINT('Ctrl Pts',(3.77545283140445,-1.,1.03608074678013));
#56012=CARTESIAN_POINT('Ctrl Pts',(3.77545283140445,1.,1.03608074678013));
#56013=CARTESIAN_POINT('Ctrl Pts',(3.76907609832522,-1.,1.0321778660492));
#56014=CARTESIAN_POINT('Ctrl Pts',(3.76907609832522,1.,1.0321778660492));
#56015=CARTESIAN_POINT('Ctrl Pts',(3.76270122291232,-1.,1.02833014458181));
#56016=CARTESIAN_POINT('Ctrl Pts',(3.76270122291232,1.,1.02833014458181));
#56017=CARTESIAN_POINT('Ctrl Pts',(3.75631037456194,-1.,1.0245342944466));
#56018=CARTESIAN_POINT('Ctrl Pts',(3.75631037456194,1.,1.0245342944466));
#56019=CARTESIAN_POINT('Ctrl Pts',(3.74987777155834,-1.,1.02078510487428));
#56020=CARTESIAN_POINT('Ctrl Pts',(3.74987777155834,1.,1.02078510487428));
#56021=CARTESIAN_POINT('Ctrl Pts',(3.74337942504959,-1.,1.01707794311079));
#56022=CARTESIAN_POINT('Ctrl Pts',(3.74337942504959,1.,1.01707794311079));
#56023=CARTESIAN_POINT('Ctrl Pts',(3.73680245055734,-1.,1.01341114319903));
#56024=CARTESIAN_POINT('Ctrl Pts',(3.73680245055734,1.,1.01341114319903));
#56025=CARTESIAN_POINT('Ctrl Pts',(3.73015276704426,-1.,1.00978798539496));
#56026=CARTESIAN_POINT('Ctrl Pts',(3.73015276704426,1.,1.00978798539496));
#56027=CARTESIAN_POINT('Ctrl Pts',(3.72346803750595,-1.,1.0062200073571));
#56028=CARTESIAN_POINT('Ctrl Pts',(3.72346803750595,1.,1.0062200073571));
#56029=CARTESIAN_POINT('Ctrl Pts',(3.71680667125118,-1.,1.00272423396822));
#56030=CARTESIAN_POINT('Ctrl Pts',(3.71680667125118,1.,1.00272423396822));
#56031=CARTESIAN_POINT('Ctrl Pts',(3.71022439713938,-1.,0.999317260756531));
#56032=CARTESIAN_POINT('Ctrl Pts',(3.71022439713938,1.,0.999317260756531));
#56033=CARTESIAN_POINT('Ctrl Pts',(3.70375282282138,-1.,0.996009819772518));
#56034=CARTESIAN_POINT('Ctrl Pts',(3.70375282282138,1.,0.996009819772518));
#56035=CARTESIAN_POINT('Ctrl Pts',(3.69738123415662,-1.,0.992802218332011));
#56036=CARTESIAN_POINT('Ctrl Pts',(3.69738123415662,1.,0.992802218332011));
#56037=CARTESIAN_POINT('Ctrl Pts',(3.69102682138846,-1.,0.989676715398559));
#56038=CARTESIAN_POINT('Ctrl Pts',(3.69102682138846,1.,0.989676715398559));
#56039=CARTESIAN_POINT('Ctrl Pts',(3.68455317926068,-1.,0.986602639863838));
#56040=CARTESIAN_POINT('Ctrl Pts',(3.68455317926068,1.,0.986602639863838));
#56041=CARTESIAN_POINT('Ctrl Pts',(3.67782408841715,-1.,0.98355079147042));
#56042=CARTESIAN_POINT('Ctrl Pts',(3.67782408841715,1.,0.98355079147042));
#56043=CARTESIAN_POINT('Ctrl Pts',(3.67074983340361,-1.,0.980505922458267));
#56044=CARTESIAN_POINT('Ctrl Pts',(3.67074983340361,1.,0.980505922458267));
#56045=CARTESIAN_POINT('Ctrl Pts',(3.66333049637475,-1.,0.977478312751618));
#56046=CARTESIAN_POINT('Ctrl Pts',(3.66333049637475,1.,0.977478312751618));
#56047=CARTESIAN_POINT('Ctrl Pts',(3.65571576735126,-1.,0.974519971354849));
#56048=CARTESIAN_POINT('Ctrl Pts',(3.65571576735126,1.,0.974519971354849));
#56049=CARTESIAN_POINT('Ctrl Pts',(3.64819756447455,-1.,0.971722122061341));
#56050=CARTESIAN_POINT('Ctrl Pts',(3.64819756447455,1.,0.971722122061341));
#56051=CARTESIAN_POINT('Ctrl Pts',(3.64113946505766,-1.,0.969195124675866));
#56052=CARTESIAN_POINT('Ctrl Pts',(3.64113946505766,1.,0.969195124675866));
#56053=CARTESIAN_POINT('Ctrl Pts',(3.63492122081143,-1.,0.967052554541386));
#56054=CARTESIAN_POINT('Ctrl Pts',(3.63492122081143,1.,0.967052554541386));
#56055=CARTESIAN_POINT('Ctrl Pts',(3.62988252139846,-1.,0.965395153165294));
#56056=CARTESIAN_POINT('Ctrl Pts',(3.62988252139846,1.,0.965395153165294));
#56057=CARTESIAN_POINT('Ctrl Pts',(3.62625391254797,-1.,0.964291001273288));
#56058=CARTESIAN_POINT('Ctrl Pts',(3.62625391254797,1.,0.964291001273288));
#56059=CARTESIAN_POINT('Ctrl Pts',(3.6245656860652,-1.,0.96387577453062));
#56060=CARTESIAN_POINT('Ctrl Pts',(3.6245656860652,1.,0.96387577453062));
#56061=CARTESIAN_POINT('Ctrl Pts',(3.62399933639914,-1.,0.963832486395052));
#56062=CARTESIAN_POINT('Ctrl Pts',(3.62399933639914,1.,0.963832486395052));
#56063=CARTESIAN_POINT('Ctrl Pts',(3.62393257642052,-1.,0.963922720982194));
#56064=CARTESIAN_POINT('Ctrl Pts',(3.62393257642052,1.,0.963922720982194));
#56065=CARTESIAN_POINT('Ctrl Pts',(3.62397690409552,-1.,0.963997613369571));
#56066=CARTESIAN_POINT('Ctrl Pts',(3.62397690409552,1.,0.963997613369571));
#56067=CARTESIAN_POINT('',(4.01728681790024,1.,1.22531898815164));
#56068=CARTESIAN_POINT('Ctrl Pts',(4.01728681790024,1.,1.22531898815164));
#56069=CARTESIAN_POINT('Ctrl Pts',(4.0161454457032,1.,1.22423716681447));
#56070=CARTESIAN_POINT('Ctrl Pts',(4.01386104434674,1.,1.22207656456199));
#56071=CARTESIAN_POINT('Ctrl Pts',(4.01042947142681,1.,1.21884478244983));
#56072=CARTESIAN_POINT('Ctrl Pts',(4.00584409524937,1.,1.21455398918813));
#56073=CARTESIAN_POINT('Ctrl Pts',(4.00009577952534,1.,1.20922097030107));
#56074=CARTESIAN_POINT('Ctrl Pts',(3.99433084800649,1.,1.2039185237544));
#56075=CARTESIAN_POINT('Ctrl Pts',(3.98854928957287,1.,1.19864679609596));
#56076=CARTESIAN_POINT('Ctrl Pts',(3.98275111052015,1.,1.19340598349307));
#56077=CARTESIAN_POINT('Ctrl Pts',(3.97693634766926,1.,1.18819633715285));
#56078=CARTESIAN_POINT('Ctrl Pts',(3.9711050516465,1.,1.18301815039596));
#56079=CARTESIAN_POINT('Ctrl Pts',(3.96525726357682,1.,1.17787174135446));
#56080=CARTESIAN_POINT('Ctrl Pts',(3.95939299213164,1.,1.17275743590327));
#56081=CARTESIAN_POINT('Ctrl Pts',(3.95351219510062,1.,1.16767555244495));
#56082=CARTESIAN_POINT('Ctrl Pts',(3.9476147478092,1.,1.16262637999261));
#56083=CARTESIAN_POINT('Ctrl Pts',(3.94170046685542,1.,1.15761018341061));
#56084=CARTESIAN_POINT('Ctrl Pts',(3.9357691705651,1.,1.15262722716391));
#56085=CARTESIAN_POINT('Ctrl Pts',(3.92982073294334,1.,1.14767779451147));
#56086=CARTESIAN_POINT('Ctrl Pts',(3.92385513133937,1.,1.14276220561575));
#56087=CARTESIAN_POINT('Ctrl Pts',(3.91787251936688,1.,1.13788084225511));
#56088=CARTESIAN_POINT('Ctrl Pts',(3.91187321145495,1.,1.13303414693849));
#56089=CARTESIAN_POINT('Ctrl Pts',(3.90585753318622,1.,1.12822258281518));
#56090=CARTESIAN_POINT('Ctrl Pts',(3.89982569749978,1.,1.12344660099029));
#56091=CARTESIAN_POINT('Ctrl Pts',(3.89377768340362,1.,1.11870660794609));
#56092=CARTESIAN_POINT('Ctrl Pts',(3.88771308285229,1.,1.11400292434447));
#56093=CARTESIAN_POINT('Ctrl Pts',(3.88163105531791,1.,1.10933577224029));
#56094=CARTESIAN_POINT('Ctrl Pts',(3.87553067187566,1.,1.10470536603303));
#56095=CARTESIAN_POINT('Ctrl Pts',(3.86941120134872,1.,1.10011198761203));
#56096=CARTESIAN_POINT('Ctrl Pts',(3.86327241021242,1.,1.09555606505012));
#56097=CARTESIAN_POINT('Ctrl Pts',(3.85711487933911,1.,1.09103825516288));
#56098=CARTESIAN_POINT('Ctrl Pts',(3.8509402522269,1.,1.08655950846377));
#56099=CARTESIAN_POINT('Ctrl Pts',(3.84475048030615,1.,1.08212087917986));
#56100=CARTESIAN_POINT('Ctrl Pts',(3.83854714117486,1.,1.07772335353856));
#56101=CARTESIAN_POINT('Ctrl Pts',(3.83233071195145,1.,1.0733676663346));
#56102=CARTESIAN_POINT('Ctrl Pts',(3.82609989967278,1.,1.0690541318036));
#56103=CARTESIAN_POINT('Ctrl Pts',(3.81985083953012,1.,1.06478244038931));
#56104=CARTESIAN_POINT('Ctrl Pts',(3.81357866117485,1.,1.06055206187298));
#56105=CARTESIAN_POINT('Ctrl Pts',(3.80727913637784,1.,1.05636266918643));
#56106=CARTESIAN_POINT('Ctrl Pts',(3.80095039790678,1.,1.05221457990015));
#56107=CARTESIAN_POINT('Ctrl Pts',(3.79459440308793,1.,1.04810913267641));
#56108=CARTESIAN_POINT('Ctrl Pts',(3.78821910787195,1.,1.04404924374426));
#56109=CARTESIAN_POINT('Ctrl Pts',(3.78183535008192,1.,1.04003862055804));
#56110=CARTESIAN_POINT('Ctrl Pts',(3.77545283140445,1.,1.03608074678013));
#56111=CARTESIAN_POINT('Ctrl Pts',(3.76907609832522,1.,1.0321778660492));
#56112=CARTESIAN_POINT('Ctrl Pts',(3.76270122291232,1.,1.02833014458181));
#56113=CARTESIAN_POINT('Ctrl Pts',(3.75631037456194,1.,1.0245342944466));
#56114=CARTESIAN_POINT('Ctrl Pts',(3.74987777155834,1.,1.02078510487428));
#56115=CARTESIAN_POINT('Ctrl Pts',(3.74337942504959,1.,1.01707794311079));
#56116=CARTESIAN_POINT('Ctrl Pts',(3.73680245055734,1.,1.01341114319903));
#56117=CARTESIAN_POINT('Ctrl Pts',(3.73015276704426,1.,1.00978798539496));
#56118=CARTESIAN_POINT('Ctrl Pts',(3.72346803750595,1.,1.0062200073571));
#56119=CARTESIAN_POINT('Ctrl Pts',(3.71680667125118,1.,1.00272423396822));
#56120=CARTESIAN_POINT('Ctrl Pts',(3.71022439713938,1.,0.999317260756531));
#56121=CARTESIAN_POINT('Ctrl Pts',(3.70375282282138,1.,0.996009819772518));
#56122=CARTESIAN_POINT('Ctrl Pts',(3.69738123415662,1.,0.992802218332011));
#56123=CARTESIAN_POINT('Ctrl Pts',(3.69102682138846,1.,0.989676715398559));
#56124=CARTESIAN_POINT('Ctrl Pts',(3.68455317926068,1.,0.986602639863838));
#56125=CARTESIAN_POINT('Ctrl Pts',(3.67782408841715,1.,0.98355079147042));
#56126=CARTESIAN_POINT('Ctrl Pts',(3.67074983340361,1.,0.980505922458267));
#56127=CARTESIAN_POINT('Ctrl Pts',(3.66333049637475,1.,0.977478312751618));
#56128=CARTESIAN_POINT('Ctrl Pts',(3.65571576735126,1.,0.974519971354849));
#56129=CARTESIAN_POINT('Ctrl Pts',(3.64819756447455,1.,0.971722122061341));
#56130=CARTESIAN_POINT('Ctrl Pts',(3.64113946505766,1.,0.969195124675866));
#56131=CARTESIAN_POINT('Ctrl Pts',(3.63492122081143,1.,0.967052554541386));
#56132=CARTESIAN_POINT('Ctrl Pts',(3.62988252139846,1.,0.965395153165294));
#56133=CARTESIAN_POINT('Ctrl Pts',(3.62652618145335,1.,0.964373850166458));
#56134=CARTESIAN_POINT('Ctrl Pts',(3.62489305727662,1.,0.963957782642844));
#56135=CARTESIAN_POINT('Ctrl Pts',(3.62424461507588,1.,0.963861297423241));
#56136=CARTESIAN_POINT('Ctrl Pts',(3.6240482887845,1.,0.963880158555582));
#56137=CARTESIAN_POINT('Ctrl Pts',(3.62400312501245,1.,0.963899035117249));
#56138=CARTESIAN_POINT('',(4.01728681790024,0.,1.22531898815164));
#56139=CARTESIAN_POINT('Ctrl Pts',(3.49848248301936,-1.,1.35022972712301));
#56140=CARTESIAN_POINT('Ctrl Pts',(3.49848248301936,1.,1.35022972712301));
#56141=CARTESIAN_POINT('Ctrl Pts',(3.4984026005375,-1.,1.35026426118402));
#56142=CARTESIAN_POINT('Ctrl Pts',(3.4984026005375,1.,1.35026426118402));
#56143=CARTESIAN_POINT('Ctrl Pts',(3.49840357193736,-1.,1.35037650303019));
#56144=CARTESIAN_POINT('Ctrl Pts',(3.49840357193736,1.,1.35037650303019));
#56145=CARTESIAN_POINT('Ctrl Pts',(3.49888720257132,-1.,1.35067437417484));
#56146=CARTESIAN_POINT('Ctrl Pts',(3.49888720257132,1.,1.35067437417484));
#56147=CARTESIAN_POINT('Ctrl Pts',(3.5004970706414,-1.,1.3513307633124));
#56148=CARTESIAN_POINT('Ctrl Pts',(3.5004970706414,1.,1.3513307633124));
#56149=CARTESIAN_POINT('Ctrl Pts',(3.50408168106261,-1.,1.35257032843486));
#56150=CARTESIAN_POINT('Ctrl Pts',(3.50408168106261,1.,1.35257032843486));
#56151=CARTESIAN_POINT('Ctrl Pts',(3.50913227059999,-1.,1.35419113575956));
#56152=CARTESIAN_POINT('Ctrl Pts',(3.50913227059999,1.,1.35419113575956));
#56153=CARTESIAN_POINT('Ctrl Pts',(3.51542230699556,-1.,1.35611275237152));
#56154=CARTESIAN_POINT('Ctrl Pts',(3.51542230699556,1.,1.35611275237152));
#56155=CARTESIAN_POINT('Ctrl Pts',(3.52261776116748,-1.,1.35821701528836));
#56156=CARTESIAN_POINT('Ctrl Pts',(3.52261776116748,1.,1.35821701528836));
#56157=CARTESIAN_POINT('Ctrl Pts',(3.530344649616,-1.,1.36037259643734));
#56158=CARTESIAN_POINT('Ctrl Pts',(3.530344649616,1.,1.36037259643734));
#56159=CARTESIAN_POINT('Ctrl Pts',(3.53824396424961,-1.,1.36245507339307));
#56160=CARTESIAN_POINT('Ctrl Pts',(3.53824396424961,1.,1.36245507339307));
#56161=CARTESIAN_POINT('Ctrl Pts',(3.54602591832973,-1.,1.36436666257598));
#56162=CARTESIAN_POINT('Ctrl Pts',(3.54602591832973,1.,1.36436666257598));
#56163=CARTESIAN_POINT('Ctrl Pts',(3.55353883995949,-1.,1.3660614545677));
#56164=CARTESIAN_POINT('Ctrl Pts',(3.55353883995949,1.,1.3660614545677));
#56165=CARTESIAN_POINT('Ctrl Pts',(3.56077662028649,-1.,1.36754771771233));
#56166=CARTESIAN_POINT('Ctrl Pts',(3.56077662028649,1.,1.36754771771233));
#56167=CARTESIAN_POINT('Ctrl Pts',(3.5678208030466,-1.,1.36886584973389));
#56168=CARTESIAN_POINT('Ctrl Pts',(3.5678208030466,1.,1.36886584973389));
#56169=CARTESIAN_POINT('Ctrl Pts',(3.57479875549486,-1.,1.37007229485659));
#56170=CARTESIAN_POINT('Ctrl Pts',(3.57479875549486,1.,1.37007229485659));
#56171=CARTESIAN_POINT('Ctrl Pts',(3.58183885982715,-1.,1.37122241663062));
#56172=CARTESIAN_POINT('Ctrl Pts',(3.58183885982715,1.,1.37122241663062));
#56173=CARTESIAN_POINT('Ctrl Pts',(3.58901853846365,-1.,1.37235053660976));
#56174=CARTESIAN_POINT('Ctrl Pts',(3.58901853846365,1.,1.37235053660976));
#56175=CARTESIAN_POINT('Ctrl Pts',(3.59634627869048,-1.,1.37346320103157));
#56176=CARTESIAN_POINT('Ctrl Pts',(3.59634627869048,1.,1.37346320103157));
#56177=CARTESIAN_POINT('Ctrl Pts',(3.60379020123988,-1.,1.37455051379623));
#56178=CARTESIAN_POINT('Ctrl Pts',(3.60379020123988,1.,1.37455051379623));
#56179=CARTESIAN_POINT('Ctrl Pts',(3.61129546591064,-1.,1.37559314436634));
#56180=CARTESIAN_POINT('Ctrl Pts',(3.61129546591064,1.,1.37559314436634));
#56181=CARTESIAN_POINT('Ctrl Pts',(3.6188048116042,-1.,1.37657053403107));
#56182=CARTESIAN_POINT('Ctrl Pts',(3.6188048116042,1.,1.37657053403107));
#56183=CARTESIAN_POINT('Ctrl Pts',(3.62628098665145,-1.,1.37746987919881));
#56184=CARTESIAN_POINT('Ctrl Pts',(3.62628098665145,1.,1.37746987919881));
#56185=CARTESIAN_POINT('Ctrl Pts',(3.63371727442486,-1.,1.37829035457339));
#56186=CARTESIAN_POINT('Ctrl Pts',(3.63371727442486,1.,1.37829035457339));
#56187=CARTESIAN_POINT('Ctrl Pts',(3.64112507791141,-1.,1.37903818567359));
#56188=CARTESIAN_POINT('Ctrl Pts',(3.64112507791141,1.,1.37903818567359));
#56189=CARTESIAN_POINT('Ctrl Pts',(3.64852652756456,-1.,1.37972372481603));
#56190=CARTESIAN_POINT('Ctrl Pts',(3.64852652756456,1.,1.37972372481603));
#56191=CARTESIAN_POINT('Ctrl Pts',(3.6559455440439,-1.,1.38035791051213));
#56192=CARTESIAN_POINT('Ctrl Pts',(3.6559455440439,1.,1.38035791051213));
#56193=CARTESIAN_POINT('Ctrl Pts',(3.66339848520857,-1.,1.38094856333552));
#56194=CARTESIAN_POINT('Ctrl Pts',(3.66339848520857,1.,1.38094856333552));
#56195=CARTESIAN_POINT('Ctrl Pts',(3.67088843112262,-1.,1.38149812653868));
#56196=CARTESIAN_POINT('Ctrl Pts',(3.67088843112262,1.,1.38149812653868));
#56197=CARTESIAN_POINT('Ctrl Pts',(3.67841038482414,-1.,1.3820057429062));
#56198=CARTESIAN_POINT('Ctrl Pts',(3.67841038482414,1.,1.3820057429062));
#56199=CARTESIAN_POINT('Ctrl Pts',(3.68595444983837,-1.,1.38246852827182));
#56200=CARTESIAN_POINT('Ctrl Pts',(3.68595444983837,1.,1.38246852827182));
#56201=CARTESIAN_POINT('Ctrl Pts',(3.69350967899526,-1.,1.38288311171651));
#56202=CARTESIAN_POINT('Ctrl Pts',(3.69350967899526,1.,1.38288311171651));
#56203=CARTESIAN_POINT('Ctrl Pts',(3.701067921679,-1.,1.38324717612865));
#56204=CARTESIAN_POINT('Ctrl Pts',(3.701067921679,1.,1.38324717612865));
#56205=CARTESIAN_POINT('Ctrl Pts',(3.70862680753347,-1.,1.38356065402124));
#56206=CARTESIAN_POINT('Ctrl Pts',(3.70862680753347,1.,1.38356065402124));
#56207=CARTESIAN_POINT('Ctrl Pts',(3.7161876605181,-1.,1.38382489984586));
#56208=CARTESIAN_POINT('Ctrl Pts',(3.7161876605181,1.,1.38382489984586));
#56209=CARTESIAN_POINT('Ctrl Pts',(3.72375409358803,-1.,1.3840421342895));
#56210=CARTESIAN_POINT('Ctrl Pts',(3.72375409358803,1.,1.3840421342895));
#56211=CARTESIAN_POINT('Ctrl Pts',(3.73133035859282,-1.,1.38421479111531));
#56212=CARTESIAN_POINT('Ctrl Pts',(3.73133035859282,1.,1.38421479111531));
#56213=CARTESIAN_POINT('Ctrl Pts',(3.73891976418104,-1.,1.38434489156458));
#56214=CARTESIAN_POINT('Ctrl Pts',(3.73891976418104,1.,1.38434489156458));
#56215=CARTESIAN_POINT('Ctrl Pts',(3.74652317167876,-1.,1.38443344984394));
#56216=CARTESIAN_POINT('Ctrl Pts',(3.74652317167876,1.,1.38443344984394));
#56217=CARTESIAN_POINT('Ctrl Pts',(3.7541397631875,-1.,1.38448077997163));
#56218=CARTESIAN_POINT('Ctrl Pts',(3.7541397631875,1.,1.38448077997163));
#56219=CARTESIAN_POINT('Ctrl Pts',(3.76176768271367,-1.,1.3844867525335));
#56220=CARTESIAN_POINT('Ctrl Pts',(3.76176768271367,1.,1.3844867525335));
#56221=CARTESIAN_POINT('Ctrl Pts',(3.76940473185779,-1.,1.38445107339518));
#56222=CARTESIAN_POINT('Ctrl Pts',(3.76940473185779,1.,1.38445107339518));
#56223=CARTESIAN_POINT('Ctrl Pts',(3.77704902230418,-1.,1.38437354551428));
#56224=CARTESIAN_POINT('Ctrl Pts',(3.77704902230418,1.,1.38437354551428));
#56225=CARTESIAN_POINT('Ctrl Pts',(3.78469969805082,-1.,1.38425435883756));
#56226=CARTESIAN_POINT('Ctrl Pts',(3.78469969805082,1.,1.38425435883756));
#56227=CARTESIAN_POINT('Ctrl Pts',(3.79235669640841,-1.,1.38409399694566));
#56228=CARTESIAN_POINT('Ctrl Pts',(3.79235669640841,1.,1.38409399694566));
#56229=CARTESIAN_POINT('Ctrl Pts',(3.80002044322111,-1.,1.38389311766682));
#56230=CARTESIAN_POINT('Ctrl Pts',(3.80002044322111,1.,1.38389311766682));
#56231=CARTESIAN_POINT('Ctrl Pts',(3.80769156398411,-1.,1.3836524404622));
#56232=CARTESIAN_POINT('Ctrl Pts',(3.80769156398411,1.,1.3836524404622));
#56233=CARTESIAN_POINT('Ctrl Pts',(3.81537060817811,-1.,1.38337263902782));
#56234=CARTESIAN_POINT('Ctrl Pts',(3.81537060817811,1.,1.38337263902782));
#56235=CARTESIAN_POINT('Ctrl Pts',(3.82305771743829,-1.,1.38305421262763));
#56236=CARTESIAN_POINT('Ctrl Pts',(3.82305771743829,1.,1.38305421262763));
#56237=CARTESIAN_POINT('Ctrl Pts',(3.8307526698229,-1.,1.38269750245138));
#56238=CARTESIAN_POINT('Ctrl Pts',(3.8307526698229,1.,1.38269750245138));
#56239=CARTESIAN_POINT('Ctrl Pts',(3.83845502790746,-1.,1.38230274828822));
#56240=CARTESIAN_POINT('Ctrl Pts',(3.83845502790746,1.,1.38230274828822));
#56241=CARTESIAN_POINT('Ctrl Pts',(3.84616425605764,-1.,1.38187013346109));
#56242=CARTESIAN_POINT('Ctrl Pts',(3.84616425605764,1.,1.38187013346109));
#56243=CARTESIAN_POINT('Ctrl Pts',(3.85387983979481,-1.,1.3813998311505));
#56244=CARTESIAN_POINT('Ctrl Pts',(3.85387983979481,1.,1.3813998311505));
#56245=CARTESIAN_POINT('Ctrl Pts',(3.86160143043959,-1.,1.3808920599299));
#56246=CARTESIAN_POINT('Ctrl Pts',(3.86160143043959,1.,1.3808920599299));
#56247=CARTESIAN_POINT('Ctrl Pts',(3.86932885813068,-1.,1.38034709213014));
#56248=CARTESIAN_POINT('Ctrl Pts',(3.86932885813068,1.,1.38034709213014));
#56249=CARTESIAN_POINT('Ctrl Pts',(3.87706205830532,-1.,1.37976523097073));
#56250=CARTESIAN_POINT('Ctrl Pts',(3.87706205830532,1.,1.37976523097073));
#56251=CARTESIAN_POINT('Ctrl Pts',(3.88480102249277,-1.,1.37914679719383));
#56252=CARTESIAN_POINT('Ctrl Pts',(3.88480102249277,1.,1.37914679719383));
#56253=CARTESIAN_POINT('Ctrl Pts',(3.89254574338496,-1.,1.3784921128802));
#56254=CARTESIAN_POINT('Ctrl Pts',(3.89254574338496,1.,1.3784921128802));
#56255=CARTESIAN_POINT('Ctrl Pts',(3.90029615196727,-1.,1.37780148512792));
#56256=CARTESIAN_POINT('Ctrl Pts',(3.90029615196727,1.,1.37780148512792));
#56257=CARTESIAN_POINT('Ctrl Pts',(3.90805209523486,-1.,1.3770751963402));
#56258=CARTESIAN_POINT('Ctrl Pts',(3.90805209523486,1.,1.3770751963402));
#56259=CARTESIAN_POINT('Ctrl Pts',(3.91581337462644,-1.,1.37631350505797));
#56260=CARTESIAN_POINT('Ctrl Pts',(3.91581337462644,1.,1.37631350505797));
#56261=CARTESIAN_POINT('Ctrl Pts',(3.92357976987672,-1.,1.37551664448242));
#56262=CARTESIAN_POINT('Ctrl Pts',(3.92357976987672,1.,1.37551664448242));
#56263=CARTESIAN_POINT('Ctrl Pts',(3.93135106761844,-1.,1.37468482215751));
#56264=CARTESIAN_POINT('Ctrl Pts',(3.93135106761844,1.,1.37468482215751));
#56265=CARTESIAN_POINT('Ctrl Pts',(3.93912709040818,-1.,1.37381821967165));
#56266=CARTESIAN_POINT('Ctrl Pts',(3.93912709040818,1.,1.37381821967165));
#56267=CARTESIAN_POINT('Ctrl Pts',(3.94690771785133,-1.,1.37291699202807));
#56268=CARTESIAN_POINT('Ctrl Pts',(3.94690771785133,1.,1.37291699202807));
#56269=CARTESIAN_POINT('Ctrl Pts',(3.95469287280914,-1.,1.37198126432386));
#56270=CARTESIAN_POINT('Ctrl Pts',(3.95469287280914,1.,1.37198126432386));
#56271=CARTESIAN_POINT('Ctrl Pts',(3.96092458506535,-1.,1.3712051561502));
#56272=CARTESIAN_POINT('Ctrl Pts',(3.96092458506535,1.,1.3712051561502));
#56273=CARTESIAN_POINT('Ctrl Pts',(3.96560037974645,-1.,1.37060761745635));
#56274=CARTESIAN_POINT('Ctrl Pts',(3.96560037974645,1.,1.37060761745635));
#56275=CARTESIAN_POINT('Ctrl Pts',(3.9687184694131,-1.,1.37020239094614));
#56276=CARTESIAN_POINT('Ctrl Pts',(3.9687184694131,1.,1.37020239094614));
#56277=CARTESIAN_POINT('Ctrl Pts',(3.97027773754922,-1.,1.36999806084573));
#56278=CARTESIAN_POINT('Ctrl Pts',(3.97027773754922,1.,1.36999806084573));
#56279=CARTESIAN_POINT('',(3.4984457533445,1.,1.35032489087101));
#56280=CARTESIAN_POINT('Ctrl Pts',(3.4984457533445,-1.,1.35032489087101));
#56281=CARTESIAN_POINT('Ctrl Pts',(3.4984457533445,-0.666666666666667,1.35032489087101));
#56282=CARTESIAN_POINT('Ctrl Pts',(3.4984457533445,-0.333333333333333,1.35032489087101));
#56283=CARTESIAN_POINT('Ctrl Pts',(3.4984457533445,0.333333333333333,1.35032489087101));
#56284=CARTESIAN_POINT('Ctrl Pts',(3.4984457533445,0.666666666666667,1.35032489087101));
#56285=CARTESIAN_POINT('Ctrl Pts',(3.4984457533445,1.,1.35032489087101));
#56286=CARTESIAN_POINT('',(3.97027773754922,1.,1.36999806084573));
#56287=CARTESIAN_POINT('',(3.97027773754922,0.,1.36999806084573));
#56288=CARTESIAN_POINT('Ctrl Pts',(3.4984457533445,1.,1.35032489087101));
#56289=CARTESIAN_POINT('Ctrl Pts',(3.49847119623846,1.,1.35036670892966));
#56290=CARTESIAN_POINT('Ctrl Pts',(3.49861894124827,1.,1.35049736560527));
#56291=CARTESIAN_POINT('Ctrl Pts',(3.49920025459723,1.,1.35080045218587));
#56292=CARTESIAN_POINT('Ctrl Pts',(3.5007660381649,1.,1.35142377279517));
#56293=CARTESIAN_POINT('Ctrl Pts',(3.50408168106261,1.,1.35257032843486));
#56294=CARTESIAN_POINT('Ctrl Pts',(3.50913227059999,1.,1.35419113575956));
#56295=CARTESIAN_POINT('Ctrl Pts',(3.51542230699556,1.,1.35611275237152));
#56296=CARTESIAN_POINT('Ctrl Pts',(3.52261776116748,1.,1.35821701528836));
#56297=CARTESIAN_POINT('Ctrl Pts',(3.530344649616,1.,1.36037259643734));
#56298=CARTESIAN_POINT('Ctrl Pts',(3.53824396424961,1.,1.36245507339307));
#56299=CARTESIAN_POINT('Ctrl Pts',(3.54602591832973,1.,1.36436666257598));
#56300=CARTESIAN_POINT('Ctrl Pts',(3.55353883995949,1.,1.3660614545677));
#56301=CARTESIAN_POINT('Ctrl Pts',(3.56077662028649,1.,1.36754771771233));
#56302=CARTESIAN_POINT('Ctrl Pts',(3.5678208030466,1.,1.36886584973389));
#56303=CARTESIAN_POINT('Ctrl Pts',(3.57479875549486,1.,1.37007229485659));
#56304=CARTESIAN_POINT('Ctrl Pts',(3.58183885982715,1.,1.37122241663062));
#56305=CARTESIAN_POINT('Ctrl Pts',(3.58901853846365,1.,1.37235053660976));
#56306=CARTESIAN_POINT('Ctrl Pts',(3.59634627869048,1.,1.37346320103157));
#56307=CARTESIAN_POINT('Ctrl Pts',(3.60379020123988,1.,1.37455051379623));
#56308=CARTESIAN_POINT('Ctrl Pts',(3.61129546591064,1.,1.37559314436634));
#56309=CARTESIAN_POINT('Ctrl Pts',(3.6188048116042,1.,1.37657053403107));
#56310=CARTESIAN_POINT('Ctrl Pts',(3.62628098665145,1.,1.37746987919881));
#56311=CARTESIAN_POINT('Ctrl Pts',(3.63371727442486,1.,1.37829035457339));
#56312=CARTESIAN_POINT('Ctrl Pts',(3.64112507791141,1.,1.37903818567359));
#56313=CARTESIAN_POINT('Ctrl Pts',(3.64852652756456,1.,1.37972372481603));
#56314=CARTESIAN_POINT('Ctrl Pts',(3.6559455440439,1.,1.38035791051213));
#56315=CARTESIAN_POINT('Ctrl Pts',(3.66339848520857,1.,1.38094856333552));
#56316=CARTESIAN_POINT('Ctrl Pts',(3.67088843112262,1.,1.38149812653868));
#56317=CARTESIAN_POINT('Ctrl Pts',(3.67841038482414,1.,1.3820057429062));
#56318=CARTESIAN_POINT('Ctrl Pts',(3.68595444983837,1.,1.38246852827182));
#56319=CARTESIAN_POINT('Ctrl Pts',(3.69350967899526,1.,1.38288311171651));
#56320=CARTESIAN_POINT('Ctrl Pts',(3.701067921679,1.,1.38324717612865));
#56321=CARTESIAN_POINT('Ctrl Pts',(3.70862680753347,1.,1.38356065402124));
#56322=CARTESIAN_POINT('Ctrl Pts',(3.7161876605181,1.,1.38382489984586));
#56323=CARTESIAN_POINT('Ctrl Pts',(3.72375409358803,1.,1.3840421342895));
#56324=CARTESIAN_POINT('Ctrl Pts',(3.73133035859282,1.,1.38421479111531));
#56325=CARTESIAN_POINT('Ctrl Pts',(3.73891976418104,1.,1.38434489156458));
#56326=CARTESIAN_POINT('Ctrl Pts',(3.74652317167876,1.,1.38443344984394));
#56327=CARTESIAN_POINT('Ctrl Pts',(3.7541397631875,1.,1.38448077997163));
#56328=CARTESIAN_POINT('Ctrl Pts',(3.76176768271367,1.,1.3844867525335));
#56329=CARTESIAN_POINT('Ctrl Pts',(3.76940473185779,1.,1.38445107339518));
#56330=CARTESIAN_POINT('Ctrl Pts',(3.77704902230418,1.,1.38437354551428));
#56331=CARTESIAN_POINT('Ctrl Pts',(3.78469969805082,1.,1.38425435883756));
#56332=CARTESIAN_POINT('Ctrl Pts',(3.79235669640841,1.,1.38409399694566));
#56333=CARTESIAN_POINT('Ctrl Pts',(3.80002044322111,1.,1.38389311766682));
#56334=CARTESIAN_POINT('Ctrl Pts',(3.80769156398411,1.,1.3836524404622));
#56335=CARTESIAN_POINT('Ctrl Pts',(3.81537060817811,1.,1.38337263902782));
#56336=CARTESIAN_POINT('Ctrl Pts',(3.82305771743829,1.,1.38305421262763));
#56337=CARTESIAN_POINT('Ctrl Pts',(3.8307526698229,1.,1.38269750245138));
#56338=CARTESIAN_POINT('Ctrl Pts',(3.83845502790746,1.,1.38230274828822));
#56339=CARTESIAN_POINT('Ctrl Pts',(3.84616425605764,1.,1.38187013346109));
#56340=CARTESIAN_POINT('Ctrl Pts',(3.85387983979481,1.,1.3813998311505));
#56341=CARTESIAN_POINT('Ctrl Pts',(3.86160143043959,1.,1.3808920599299));
#56342=CARTESIAN_POINT('Ctrl Pts',(3.86932885813068,1.,1.38034709213014));
#56343=CARTESIAN_POINT('Ctrl Pts',(3.87706205830532,1.,1.37976523097073));
#56344=CARTESIAN_POINT('Ctrl Pts',(3.88480102249277,1.,1.37914679719383));
#56345=CARTESIAN_POINT('Ctrl Pts',(3.89254574338496,1.,1.3784921128802));
#56346=CARTESIAN_POINT('Ctrl Pts',(3.90029615196727,1.,1.37780148512792));
#56347=CARTESIAN_POINT('Ctrl Pts',(3.90805209523486,1.,1.3770751963402));
#56348=CARTESIAN_POINT('Ctrl Pts',(3.91581337462644,1.,1.37631350505797));
#56349=CARTESIAN_POINT('Ctrl Pts',(3.92357976987672,1.,1.37551664448242));
#56350=CARTESIAN_POINT('Ctrl Pts',(3.93135106761844,1.,1.37468482215751));
#56351=CARTESIAN_POINT('Ctrl Pts',(3.93912709040818,1.,1.37381821967165));
#56352=CARTESIAN_POINT('Ctrl Pts',(3.94690771785133,1.,1.37291699202807));
#56353=CARTESIAN_POINT('Ctrl Pts',(3.95469287280914,1.,1.37198126432386));
#56354=CARTESIAN_POINT('Ctrl Pts',(3.96092458506535,1.,1.3712051561502));
#56355=CARTESIAN_POINT('Ctrl Pts',(3.96560037974645,1.,1.37060761745635));
#56356=CARTESIAN_POINT('Ctrl Pts',(3.9687184694131,1.,1.37020239094614));
#56357=CARTESIAN_POINT('Ctrl Pts',(3.97027773754922,1.,1.36999806084573));
#56358=CARTESIAN_POINT('Origin',(3.97027773754922,0.,1.36999806084573));
#56359=CARTESIAN_POINT('',(4.01728681790024,1.,1.22531898815164));
#56360=CARTESIAN_POINT('Origin',(0.,0.,0.));
#56361=CARTESIAN_POINT('',(3.42859860294378,1.,1.51895082866166));
#56362=CARTESIAN_POINT('Origin',(0.,1.,0.));
#56363=CARTESIAN_POINT('Ctrl Pts',(3.42859860294378,1.,1.51895082866166));
#56364=CARTESIAN_POINT('Ctrl Pts',(3.42859860294378,0.666666666666667,1.51895082866166));
#56365=CARTESIAN_POINT('Ctrl Pts',(3.42859860294378,0.333333333333333,1.51895082866166));
#56366=CARTESIAN_POINT('Ctrl Pts',(3.42859860294378,-0.333333333333333,
1.51895082866166));
#56367=CARTESIAN_POINT('Ctrl Pts',(3.42859860294378,-0.666666666666667,
1.51895082866166));
#56368=CARTESIAN_POINT('Ctrl Pts',(3.42859860294378,-1.,1.51895082866166));
#56369=CARTESIAN_POINT('Ctrl Pts',(3.77614523045147,-1.,1.83867539237861));
#56370=CARTESIAN_POINT('Ctrl Pts',(3.77614523045147,1.,1.83867539237861));
#56371=CARTESIAN_POINT('Ctrl Pts',(3.77518714458232,-1.,1.83742834010821));
#56372=CARTESIAN_POINT('Ctrl Pts',(3.77518714458232,1.,1.83742834010821));
#56373=CARTESIAN_POINT('Ctrl Pts',(3.77326886065484,-1.,1.83493697935064));
#56374=CARTESIAN_POINT('Ctrl Pts',(3.77326886065484,1.,1.83493697935064));
#56375=CARTESIAN_POINT('Ctrl Pts',(3.77038509819777,-1.,1.83120816956515));
#56376=CARTESIAN_POINT('Ctrl Pts',(3.77038509819777,1.,1.83120816956515));
#56377=CARTESIAN_POINT('Ctrl Pts',(3.76652740355856,-1.,1.82625289221933));
#56378=CARTESIAN_POINT('Ctrl Pts',(3.76652740355856,1.,1.82625289221933));
#56379=CARTESIAN_POINT('Ctrl Pts',(3.76168412709652,-1.,1.82008629694924));
#56380=CARTESIAN_POINT('Ctrl Pts',(3.76168412709652,1.,1.82008629694924));
#56381=CARTESIAN_POINT('Ctrl Pts',(3.75681965683995,-1.,1.81394729834032));
#56382=CARTESIAN_POINT('Ctrl Pts',(3.75681965683995,1.,1.81394729834032));
#56383=CARTESIAN_POINT('Ctrl Pts',(3.75193395888069,-1.,1.80783603939662));
#56384=CARTESIAN_POINT('Ctrl Pts',(3.75193395888069,1.,1.80783603939662));
#56385=CARTESIAN_POINT('Ctrl Pts',(3.74702700874954,-1.,1.80175271485519));
#56386=CARTESIAN_POINT('Ctrl Pts',(3.74702700874954,1.,1.80175271485519));
#56387=CARTESIAN_POINT('Ctrl Pts',(3.74209880351667,-1.,1.79569757859041));
#56388=CARTESIAN_POINT('Ctrl Pts',(3.74209880351667,1.,1.79569757859041));
#56389=CARTESIAN_POINT('Ctrl Pts',(3.73714934729962,-1.,1.78967092823139));
#56390=CARTESIAN_POINT('Ctrl Pts',(3.73714934729962,1.,1.78967092823139));
#56391=CARTESIAN_POINT('Ctrl Pts',(3.73217863095022,-1.,1.78367308442682));
#56392=CARTESIAN_POINT('Ctrl Pts',(3.73217863095022,1.,1.78367308442682));
#56393=CARTESIAN_POINT('Ctrl Pts',(3.72718661205504,-1.,1.77770437039606));
#56394=CARTESIAN_POINT('Ctrl Pts',(3.72718661205504,1.,1.77770437039606));
#56395=CARTESIAN_POINT('Ctrl Pts',(3.72217319911429,-1.,1.77176509401846));
#56396=CARTESIAN_POINT('Ctrl Pts',(3.72217319911429,1.,1.77176509401846));
#56397=CARTESIAN_POINT('Ctrl Pts',(3.71713822377675,-1.,1.76585552124549));
#56398=CARTESIAN_POINT('Ctrl Pts',(3.71713822377675,1.,1.76585552124549));
#56399=CARTESIAN_POINT('Ctrl Pts',(3.71208146346454,-1.,1.75997588499021));
#56400=CARTESIAN_POINT('Ctrl Pts',(3.71208146346454,1.,1.75997588499021));
#56401=CARTESIAN_POINT('Ctrl Pts',(3.70700269736876,-1.,1.75412641804148));
#56402=CARTESIAN_POINT('Ctrl Pts',(3.70700269736876,1.,1.75412641804148));
#56403=CARTESIAN_POINT('Ctrl Pts',(3.70190175673422,-1.,1.74830738046092));
#56404=CARTESIAN_POINT('Ctrl Pts',(3.70190175673422,1.,1.74830738046092));
#56405=CARTESIAN_POINT('Ctrl Pts',(3.6967785691046,-1.,1.74251908492589));
#56406=CARTESIAN_POINT('Ctrl Pts',(3.6967785691046,1.,1.74251908492589));
#56407=CARTESIAN_POINT('Ctrl Pts',(3.69163322647906,-1.,1.73676193254493));
#56408=CARTESIAN_POINT('Ctrl Pts',(3.69163322647906,1.,1.73676193254493));
#56409=CARTESIAN_POINT('Ctrl Pts',(3.68646597019188,-1.,1.73103640956647));
#56410=CARTESIAN_POINT('Ctrl Pts',(3.68646597019188,1.,1.73103640956647));
#56411=CARTESIAN_POINT('Ctrl Pts',(3.68127704936472,-1.,1.72534302437003));
#56412=CARTESIAN_POINT('Ctrl Pts',(3.68127704936472,1.,1.72534302437003));
#56413=CARTESIAN_POINT('Ctrl Pts',(3.67606660374665,-1.,1.71968225581787));
#56414=CARTESIAN_POINT('Ctrl Pts',(3.67606660374665,1.,1.71968225581787));
#56415=CARTESIAN_POINT('Ctrl Pts',(3.67083454901629,-1.,1.71405450210392));
#56416=CARTESIAN_POINT('Ctrl Pts',(3.67083454901629,1.,1.71405450210392));
#56417=CARTESIAN_POINT('Ctrl Pts',(3.6655804319893,-1.,1.70846001610983));
#56418=CARTESIAN_POINT('Ctrl Pts',(3.6655804319893,1.,1.70846001610983));
#56419=CARTESIAN_POINT('Ctrl Pts',(3.6603033877491,-1.,1.70289888566904));
#56420=CARTESIAN_POINT('Ctrl Pts',(3.6603033877491,1.,1.70289888566904));
#56421=CARTESIAN_POINT('Ctrl Pts',(3.65500246526798,-1.,1.69737117722559));
#56422=CARTESIAN_POINT('Ctrl Pts',(3.65500246526798,1.,1.69737117722559));
#56423=CARTESIAN_POINT('Ctrl Pts',(3.64967689827393,-1.,1.691877054817));
#56424=CARTESIAN_POINT('Ctrl Pts',(3.64967689827393,1.,1.691877054817));
#56425=CARTESIAN_POINT('Ctrl Pts',(3.64432638915199,-1.,1.68641690471455));
#56426=CARTESIAN_POINT('Ctrl Pts',(3.64432638915199,1.,1.68641690471455));
#56427=CARTESIAN_POINT('Ctrl Pts',(3.63895140887443,-1.,1.68099146651577));
#56428=CARTESIAN_POINT('Ctrl Pts',(3.63895140887443,1.,1.68099146651577));
#56429=CARTESIAN_POINT('Ctrl Pts',(3.63355343201211,-1.,1.67560193613145));
#56430=CARTESIAN_POINT('Ctrl Pts',(3.63355343201211,1.,1.67560193613145));
#56431=CARTESIAN_POINT('Ctrl Pts',(3.62813422105257,-1.,1.67024966008037));
#56432=CARTESIAN_POINT('Ctrl Pts',(3.62813422105257,1.,1.67024966008037));
#56433=CARTESIAN_POINT('Ctrl Pts',(3.62269517989104,-1.,1.66493585923853));
#56434=CARTESIAN_POINT('Ctrl Pts',(3.62269517989104,1.,1.66493585923853));
#56435=CARTESIAN_POINT('Ctrl Pts',(3.61723666482457,-1.,1.65966133399186));
#56436=CARTESIAN_POINT('Ctrl Pts',(3.61723666482457,1.,1.65966133399186));
#56437=CARTESIAN_POINT('Ctrl Pts',(3.61175734965129,-1.,1.65442619244327));
#56438=CARTESIAN_POINT('Ctrl Pts',(3.61175734965129,1.,1.65442619244327));
#56439=CARTESIAN_POINT('Ctrl Pts',(3.60625346556992,-1.,1.64922952425833));
#56440=CARTESIAN_POINT('Ctrl Pts',(3.60625346556992,1.,1.64922952425833));
#56441=CARTESIAN_POINT('Ctrl Pts',(3.6007202851384,-1.,1.6440700438558));
#56442=CARTESIAN_POINT('Ctrl Pts',(3.6007202851384,1.,1.6440700438558));
#56443=CARTESIAN_POINT('Ctrl Pts',(3.59515368334887,-1.,1.63894676675349));
#56444=CARTESIAN_POINT('Ctrl Pts',(3.59515368334887,1.,1.63894676675349));
#56445=CARTESIAN_POINT('Ctrl Pts',(3.58955176627876,-1.,1.63385971451259));
#56446=CARTESIAN_POINT('Ctrl Pts',(3.58955176627876,1.,1.63385971451259));
#56447=CARTESIAN_POINT('Ctrl Pts',(3.5839162577435,-1.,1.62881051550748));
#56448=CARTESIAN_POINT('Ctrl Pts',(3.5839162577435,1.,1.62881051550748));
#56449=CARTESIAN_POINT('Ctrl Pts',(3.57825455954405,-1.,1.62380329464851));
#56450=CARTESIAN_POINT('Ctrl Pts',(3.57825455954405,1.,1.62380329464851));
#56451=CARTESIAN_POINT('Ctrl Pts',(3.57257679609826,-1.,1.61884340915412));
#56452=CARTESIAN_POINT('Ctrl Pts',(3.57257679609826,1.,1.61884340915412));
#56453=CARTESIAN_POINT('Ctrl Pts',(3.56689200468404,-1.,1.61393581747522));
#56454=CARTESIAN_POINT('Ctrl Pts',(3.56689200468404,1.,1.61393581747522));
#56455=CARTESIAN_POINT('Ctrl Pts',(3.56120432482986,-1.,1.60908344685459));
#56456=CARTESIAN_POINT('Ctrl Pts',(3.56120432482986,1.,1.60908344685459));
#56457=CARTESIAN_POINT('Ctrl Pts',(3.55550985096117,-1.,1.60428584699848));
#56458=CARTESIAN_POINT('Ctrl Pts',(3.55550985096117,1.,1.60428584699848));
#56459=CARTESIAN_POINT('Ctrl Pts',(3.54979148634426,-1.,1.59953698113444));
#56460=CARTESIAN_POINT('Ctrl Pts',(3.54979148634426,1.,1.59953698113444));
#56461=CARTESIAN_POINT('Ctrl Pts',(3.544024581823,-1.,1.5948276694975));
#56462=CARTESIAN_POINT('Ctrl Pts',(3.544024581823,1.,1.5948276694975));
#56463=CARTESIAN_POINT('Ctrl Pts',(3.53818616861045,-1.,1.59014958368725));
#56464=CARTESIAN_POINT('Ctrl Pts',(3.53818616861045,1.,1.59014958368725));
#56465=CARTESIAN_POINT('Ctrl Pts',(3.53226378147068,-1.,1.58549906268083));
#56466=CARTESIAN_POINT('Ctrl Pts',(3.53226378147068,1.,1.58549906268083));
#56467=CARTESIAN_POINT('Ctrl Pts',(3.52626275334899,-1.,1.58088027227856));
#56468=CARTESIAN_POINT('Ctrl Pts',(3.52626275334899,1.,1.58088027227856));
#56469=CARTESIAN_POINT('Ctrl Pts',(3.52021847865961,-1.,1.5763104998818));
#56470=CARTESIAN_POINT('Ctrl Pts',(3.52021847865961,1.,1.5763104998818));
#56471=CARTESIAN_POINT('Ctrl Pts',(3.51418598431733,-1.,1.57181569799774));
#56472=CARTESIAN_POINT('Ctrl Pts',(3.51418598431733,1.,1.57181569799774));
#56473=CARTESIAN_POINT('Ctrl Pts',(3.50821771695427,-1.,1.56742097575041));
#56474=CARTESIAN_POINT('Ctrl Pts',(3.50821771695427,1.,1.56742097575041));
#56475=CARTESIAN_POINT('Ctrl Pts',(3.50234321621607,-1.,1.56314187758689));
#56476=CARTESIAN_POINT('Ctrl Pts',(3.50234321621607,1.,1.56314187758689));
#56477=CARTESIAN_POINT('Ctrl Pts',(3.49655185179623,-1.,1.55897703097859));
#56478=CARTESIAN_POINT('Ctrl Pts',(3.49655185179623,1.,1.55897703097859));
#56479=CARTESIAN_POINT('Ctrl Pts',(3.49076460877317,-1.,1.5548959590107));
#56480=CARTESIAN_POINT('Ctrl Pts',(3.49076460877317,1.,1.5548959590107));
#56481=CARTESIAN_POINT('Ctrl Pts',(3.48485155928414,-1.,1.55084702970382));
#56482=CARTESIAN_POINT('Ctrl Pts',(3.48485155928414,1.,1.55084702970382));
#56483=CARTESIAN_POINT('Ctrl Pts',(3.47868272898599,-1.,1.54678009290207));
#56484=CARTESIAN_POINT('Ctrl Pts',(3.47868272898599,1.,1.54678009290207));
#56485=CARTESIAN_POINT('Ctrl Pts',(3.47217189224576,-1.,1.54266605398152));
#56486=CARTESIAN_POINT('Ctrl Pts',(3.47217189224576,1.,1.54266605398152));
#56487=CARTESIAN_POINT('Ctrl Pts',(3.46531752207222,-1.,1.53851507915533));
#56488=CARTESIAN_POINT('Ctrl Pts',(3.46531752207222,1.,1.53851507915533));
#56489=CARTESIAN_POINT('Ctrl Pts',(3.45825932955273,-1.,1.53440195378902));
#56490=CARTESIAN_POINT('Ctrl Pts',(3.45825932955273,1.,1.53440195378902));
#56491=CARTESIAN_POINT('Ctrl Pts',(3.45127136828667,-1.,1.530462444618));
#56492=CARTESIAN_POINT('Ctrl Pts',(3.45127136828667,1.,1.530462444618));
#56493=CARTESIAN_POINT('Ctrl Pts',(3.44469547527,-1.,1.52686242875717));
#56494=CARTESIAN_POINT('Ctrl Pts',(3.44469547527,1.,1.52686242875717));
#56495=CARTESIAN_POINT('Ctrl Pts',(3.43888895974182,-1.,1.52377348950429));
#56496=CARTESIAN_POINT('Ctrl Pts',(3.43888895974182,1.,1.52377348950429));
#56497=CARTESIAN_POINT('Ctrl Pts',(3.43417156977749,-1.,1.52134826724227));
#56498=CARTESIAN_POINT('Ctrl Pts',(3.43417156977749,1.,1.52134826724227));
#56499=CARTESIAN_POINT('Ctrl Pts',(3.43076036253384,-1.,1.51969006980792));
#56500=CARTESIAN_POINT('Ctrl Pts',(3.43076036253384,1.,1.51969006980792));
#56501=CARTESIAN_POINT('Ctrl Pts',(3.42915787669388,-1.,1.51901585838879));
#56502=CARTESIAN_POINT('Ctrl Pts',(3.42915787669388,1.,1.51901585838879));
#56503=CARTESIAN_POINT('Ctrl Pts',(3.42860527148835,-1.,1.51888450659497));
#56504=CARTESIAN_POINT('Ctrl Pts',(3.42860527148835,1.,1.51888450659497));
#56505=CARTESIAN_POINT('Ctrl Pts',(3.42852521763648,-1.,1.51896318668306));
#56506=CARTESIAN_POINT('Ctrl Pts',(3.42852521763648,1.,1.51896318668306));
#56507=CARTESIAN_POINT('Ctrl Pts',(3.42855728381368,-1.,1.519044091397));
#56508=CARTESIAN_POINT('Ctrl Pts',(3.42855728381368,1.,1.519044091397));
#56509=CARTESIAN_POINT('',(3.77614523045147,1.,1.83867539237861));
#56510=CARTESIAN_POINT('Ctrl Pts',(3.77614523045147,1.,1.83867539237861));
#56511=CARTESIAN_POINT('Ctrl Pts',(3.77518714458232,1.,1.83742834010821));
#56512=CARTESIAN_POINT('Ctrl Pts',(3.77326886065484,1.,1.83493697935064));
#56513=CARTESIAN_POINT('Ctrl Pts',(3.77038509819777,1.,1.83120816956515));
#56514=CARTESIAN_POINT('Ctrl Pts',(3.76652740355856,1.,1.82625289221933));
#56515=CARTESIAN_POINT('Ctrl Pts',(3.76168412709652,1.,1.82008629694924));
#56516=CARTESIAN_POINT('Ctrl Pts',(3.75681965683995,1.,1.81394729834032));
#56517=CARTESIAN_POINT('Ctrl Pts',(3.75193395888069,1.,1.80783603939662));
#56518=CARTESIAN_POINT('Ctrl Pts',(3.74702700874954,1.,1.80175271485519));
#56519=CARTESIAN_POINT('Ctrl Pts',(3.74209880351667,1.,1.79569757859041));
#56520=CARTESIAN_POINT('Ctrl Pts',(3.73714934729962,1.,1.78967092823139));
#56521=CARTESIAN_POINT('Ctrl Pts',(3.73217863095022,1.,1.78367308442682));
#56522=CARTESIAN_POINT('Ctrl Pts',(3.72718661205504,1.,1.77770437039606));
#56523=CARTESIAN_POINT('Ctrl Pts',(3.72217319911429,1.,1.77176509401846));
#56524=CARTESIAN_POINT('Ctrl Pts',(3.71713822377675,1.,1.76585552124549));
#56525=CARTESIAN_POINT('Ctrl Pts',(3.71208146346454,1.,1.75997588499021));
#56526=CARTESIAN_POINT('Ctrl Pts',(3.70700269736876,1.,1.75412641804148));
#56527=CARTESIAN_POINT('Ctrl Pts',(3.70190175673422,1.,1.74830738046092));
#56528=CARTESIAN_POINT('Ctrl Pts',(3.6967785691046,1.,1.74251908492589));
#56529=CARTESIAN_POINT('Ctrl Pts',(3.69163322647906,1.,1.73676193254493));
#56530=CARTESIAN_POINT('Ctrl Pts',(3.68646597019188,1.,1.73103640956647));
#56531=CARTESIAN_POINT('Ctrl Pts',(3.68127704936472,1.,1.72534302437003));
#56532=CARTESIAN_POINT('Ctrl Pts',(3.67606660374665,1.,1.71968225581787));
#56533=CARTESIAN_POINT('Ctrl Pts',(3.67083454901629,1.,1.71405450210392));
#56534=CARTESIAN_POINT('Ctrl Pts',(3.6655804319893,1.,1.70846001610983));
#56535=CARTESIAN_POINT('Ctrl Pts',(3.6603033877491,1.,1.70289888566904));
#56536=CARTESIAN_POINT('Ctrl Pts',(3.65500246526798,1.,1.69737117722559));
#56537=CARTESIAN_POINT('Ctrl Pts',(3.64967689827393,1.,1.691877054817));
#56538=CARTESIAN_POINT('Ctrl Pts',(3.64432638915199,1.,1.68641690471455));
#56539=CARTESIAN_POINT('Ctrl Pts',(3.63895140887443,1.,1.68099146651577));
#56540=CARTESIAN_POINT('Ctrl Pts',(3.63355343201211,1.,1.67560193613145));
#56541=CARTESIAN_POINT('Ctrl Pts',(3.62813422105257,1.,1.67024966008037));
#56542=CARTESIAN_POINT('Ctrl Pts',(3.62269517989104,1.,1.66493585923853));
#56543=CARTESIAN_POINT('Ctrl Pts',(3.61723666482457,1.,1.65966133399186));
#56544=CARTESIAN_POINT('Ctrl Pts',(3.61175734965129,1.,1.65442619244327));
#56545=CARTESIAN_POINT('Ctrl Pts',(3.60625346556992,1.,1.64922952425833));
#56546=CARTESIAN_POINT('Ctrl Pts',(3.6007202851384,1.,1.6440700438558));
#56547=CARTESIAN_POINT('Ctrl Pts',(3.59515368334887,1.,1.63894676675349));
#56548=CARTESIAN_POINT('Ctrl Pts',(3.58955176627876,1.,1.63385971451259));
#56549=CARTESIAN_POINT('Ctrl Pts',(3.5839162577435,1.,1.62881051550748));
#56550=CARTESIAN_POINT('Ctrl Pts',(3.57825455954405,1.,1.62380329464851));
#56551=CARTESIAN_POINT('Ctrl Pts',(3.57257679609826,1.,1.61884340915412));
#56552=CARTESIAN_POINT('Ctrl Pts',(3.56689200468404,1.,1.61393581747522));
#56553=CARTESIAN_POINT('Ctrl Pts',(3.56120432482986,1.,1.60908344685459));
#56554=CARTESIAN_POINT('Ctrl Pts',(3.55550985096117,1.,1.60428584699848));
#56555=CARTESIAN_POINT('Ctrl Pts',(3.54979148634426,1.,1.59953698113444));
#56556=CARTESIAN_POINT('Ctrl Pts',(3.544024581823,1.,1.5948276694975));
#56557=CARTESIAN_POINT('Ctrl Pts',(3.53818616861045,1.,1.59014958368725));
#56558=CARTESIAN_POINT('Ctrl Pts',(3.53226378147068,1.,1.58549906268083));
#56559=CARTESIAN_POINT('Ctrl Pts',(3.52626275334899,1.,1.58088027227856));
#56560=CARTESIAN_POINT('Ctrl Pts',(3.52021847865961,1.,1.5763104998818));
#56561=CARTESIAN_POINT('Ctrl Pts',(3.51418598431733,1.,1.57181569799774));
#56562=CARTESIAN_POINT('Ctrl Pts',(3.50821771695427,1.,1.56742097575041));
#56563=CARTESIAN_POINT('Ctrl Pts',(3.50234321621607,1.,1.56314187758689));
#56564=CARTESIAN_POINT('Ctrl Pts',(3.49655185179623,1.,1.55897703097859));
#56565=CARTESIAN_POINT('Ctrl Pts',(3.49076460877317,1.,1.5548959590107));
#56566=CARTESIAN_POINT('Ctrl Pts',(3.48485155928414,1.,1.55084702970382));
#56567=CARTESIAN_POINT('Ctrl Pts',(3.47868272898599,1.,1.54678009290207));
#56568=CARTESIAN_POINT('Ctrl Pts',(3.47217189224576,1.,1.54266605398152));
#56569=CARTESIAN_POINT('Ctrl Pts',(3.46531752207222,1.,1.53851507915533));
#56570=CARTESIAN_POINT('Ctrl Pts',(3.45825932955273,1.,1.53440195378902));
#56571=CARTESIAN_POINT('Ctrl Pts',(3.45127136828667,1.,1.530462444618));
#56572=CARTESIAN_POINT('Ctrl Pts',(3.44469547527,1.,1.52686242875717));
#56573=CARTESIAN_POINT('Ctrl Pts',(3.43888895974182,1.,1.52377348950429));
#56574=CARTESIAN_POINT('Ctrl Pts',(3.43417156977749,1.,1.52134826724227));
#56575=CARTESIAN_POINT('Ctrl Pts',(3.4310163189349,1.,1.5198144909343));
#56576=CARTESIAN_POINT('Ctrl Pts',(3.42946838852728,1.,1.51914806898539));
#56577=CARTESIAN_POINT('Ctrl Pts',(3.42884302333978,1.,1.51895133295017));
#56578=CARTESIAN_POINT('Ctrl Pts',(3.42864616361967,1.,1.51893924967231));
#56579=CARTESIAN_POINT('Ctrl Pts',(3.42859860294378,1.,1.51895082866166));
#56580=CARTESIAN_POINT('',(3.77614523045147,0.,1.83867539237861));
#56581=CARTESIAN_POINT('Ctrl Pts',(3.24418789321065,-1.,1.88088939428811));
#56582=CARTESIAN_POINT('Ctrl Pts',(3.24418789321065,1.,1.88088939428811));
#56583=CARTESIAN_POINT('Ctrl Pts',(3.24410359189733,-1.,1.8809110068042));
#56584=CARTESIAN_POINT('Ctrl Pts',(3.24410359189733,1.,1.8809110068042));
#56585=CARTESIAN_POINT('Ctrl Pts',(3.24408699284449,-1.,1.8810220187274));
#56586=CARTESIAN_POINT('Ctrl Pts',(3.24408699284449,1.,1.8810220187274));
#56587=CARTESIAN_POINT('Ctrl Pts',(3.24451807186964,-1.,1.88139187908347));
#56588=CARTESIAN_POINT('Ctrl Pts',(3.24451807186964,1.,1.88139187908347));
#56589=CARTESIAN_POINT('Ctrl Pts',(3.24600543790876,-1.,1.88229202583187));
#56590=CARTESIAN_POINT('Ctrl Pts',(3.24600543790876,1.,1.88229202583187));
#56591=CARTESIAN_POINT('Ctrl Pts',(3.24935200512055,-1.,1.88407708646435));
#56592=CARTESIAN_POINT('Ctrl Pts',(3.24935200512055,1.,1.88407708646435));
#56593=CARTESIAN_POINT('Ctrl Pts',(3.25408686339298,-1.,1.88646802523372));
#56594=CARTESIAN_POINT('Ctrl Pts',(3.25408686339298,1.,1.88646802523372));
#56595=CARTESIAN_POINT('Ctrl Pts',(3.2599988519361,-1.,1.88934996203508));
#56596=CARTESIAN_POINT('Ctrl Pts',(3.2599988519361,1.,1.88934996203508));
#56597=CARTESIAN_POINT('Ctrl Pts',(3.2667765388833,-1.,1.89255393500769));
#56598=CARTESIAN_POINT('Ctrl Pts',(3.2667765388833,1.,1.89255393500769));
#56599=CARTESIAN_POINT('Ctrl Pts',(3.27407108932908,-1.,1.89589172903662));
#56600=CARTESIAN_POINT('Ctrl Pts',(3.27407108932908,1.,1.89589172903662));
#56601=CARTESIAN_POINT('Ctrl Pts',(3.28154737912287,-1.,1.89918429230425));
#56602=CARTESIAN_POINT('Ctrl Pts',(3.28154737912287,1.,1.89918429230425));
#56603=CARTESIAN_POINT('Ctrl Pts',(3.28893448600364,-1.,1.9022897124757));
#56604=CARTESIAN_POINT('Ctrl Pts',(3.28893448600364,1.,1.9022897124757));
#56605=CARTESIAN_POINT('Ctrl Pts',(3.29608978722258,-1.,1.9051389186417));
#56606=CARTESIAN_POINT('Ctrl Pts',(3.29608978722258,1.,1.9051389186417));
#56607=CARTESIAN_POINT('Ctrl Pts',(3.30300595568341,-1.,1.90773912171424));
#56608=CARTESIAN_POINT('Ctrl Pts',(3.30300595568341,1.,1.90773912171424));
#56609=CARTESIAN_POINT('Ctrl Pts',(3.30975721158694,-1.,1.91014297830502));
#56610=CARTESIAN_POINT('Ctrl Pts',(3.30975721158694,1.,1.91014297830502));
#56611=CARTESIAN_POINT('Ctrl Pts',(3.31646052426395,-1.,1.91242616234459));
#56612=CARTESIAN_POINT('Ctrl Pts',(3.31646052426395,1.,1.91242616234459));
#56613=CARTESIAN_POINT('Ctrl Pts',(3.32323403454507,-1.,1.91466343916612));
#56614=CARTESIAN_POINT('Ctrl Pts',(3.32323403454507,1.,1.91466343916612));
#56615=CARTESIAN_POINT('Ctrl Pts',(3.33014884257812,-1.,1.91690081930297));
#56616=CARTESIAN_POINT('Ctrl Pts',(3.33014884257812,1.,1.91690081930297));
#56617=CARTESIAN_POINT('Ctrl Pts',(3.33721230709948,-1.,1.91914609610173));
#56618=CARTESIAN_POINT('Ctrl Pts',(3.33721230709948,1.,1.91914609610173));
#56619=CARTESIAN_POINT('Ctrl Pts',(3.34439448941915,-1.,1.92138450828378));
#56620=CARTESIAN_POINT('Ctrl Pts',(3.34439448941915,1.,1.92138450828378));
#56621=CARTESIAN_POINT('Ctrl Pts',(3.35164424847206,-1.,1.92358838440518));
#56622=CARTESIAN_POINT('Ctrl Pts',(3.35164424847206,1.,1.92358838440518));
#56623=CARTESIAN_POINT('Ctrl Pts',(3.35890824422976,-1.,1.92572846125763));
#56624=CARTESIAN_POINT('Ctrl Pts',(3.35890824422976,1.,1.92572846125763));
#56625=CARTESIAN_POINT('Ctrl Pts',(3.36615168657597,-1.,1.92778626543803));
#56626=CARTESIAN_POINT('Ctrl Pts',(3.36615168657597,1.,1.92778626543803));
#56627=CARTESIAN_POINT('Ctrl Pts',(3.37336807068078,-1.,1.92975993109897));
#56628=CARTESIAN_POINT('Ctrl Pts',(3.37336807068078,1.,1.92975993109897));
#56629=CARTESIAN_POINT('Ctrl Pts',(3.38056768525577,-1.,1.93165739093292));
#56630=CARTESIAN_POINT('Ctrl Pts',(3.38056768525577,1.,1.93165739093292));
#56631=CARTESIAN_POINT('Ctrl Pts',(3.38777076883267,-1.,1.93349233176794));
#56632=CARTESIAN_POINT('Ctrl Pts',(3.38777076883267,1.,1.93349233176794));
#56633=CARTESIAN_POINT('Ctrl Pts',(3.39499923640789,-1.,1.93527929945982));
#56634=CARTESIAN_POINT('Ctrl Pts',(3.39499923640789,1.,1.93527929945982));
#56635=CARTESIAN_POINT('Ctrl Pts',(3.40226802104093,-1.,1.93702857723089));
#56636=CARTESIAN_POINT('Ctrl Pts',(3.40226802104093,1.,1.93702857723089));
#56637=CARTESIAN_POINT('Ctrl Pts',(3.40957978266622,-1.,1.93874306008132));
#56638=CARTESIAN_POINT('Ctrl Pts',(3.40957978266622,1.,1.93874306008132));
#56639=CARTESIAN_POINT('Ctrl Pts',(3.41692971994082,-1.,1.94042111965237));
#56640=CARTESIAN_POINT('Ctrl Pts',(3.41692971994082,1.,1.94042111965237));
#56641=CARTESIAN_POINT('Ctrl Pts',(3.42430850941497,-1.,1.94205835913692));
#56642=CARTESIAN_POINT('Ctrl Pts',(3.42430850941497,1.,1.94205835913692));
#56643=CARTESIAN_POINT('Ctrl Pts',(3.43170586602436,-1.,1.94364973660285));
#56644=CARTESIAN_POINT('Ctrl Pts',(3.43170586602436,1.,1.94364973660285));
#56645=CARTESIAN_POINT('Ctrl Pts',(3.43911410197693,-1.,1.94519168842883));
#56646=CARTESIAN_POINT('Ctrl Pts',(3.43911410197693,1.,1.94519168842883));
#56647=CARTESIAN_POINT('Ctrl Pts',(3.44653088665685,-1.,1.94668377715332));
#56648=CARTESIAN_POINT('Ctrl Pts',(3.44653088665685,1.,1.94668377715332));
#56649=CARTESIAN_POINT('Ctrl Pts',(3.45395731584051,-1.,1.94812754766524));
#56650=CARTESIAN_POINT('Ctrl Pts',(3.45395731584051,1.,1.94812754766524));
#56651=CARTESIAN_POINT('Ctrl Pts',(3.46139661060959,-1.,1.94952575850196));
#56652=CARTESIAN_POINT('Ctrl Pts',(3.46139661060959,1.,1.94952575850196));
#56653=CARTESIAN_POINT('Ctrl Pts',(3.4688525897419,-1.,1.95088147859876));
#56654=CARTESIAN_POINT('Ctrl Pts',(3.4688525897419,1.,1.95088147859876));
#56655=CARTESIAN_POINT('Ctrl Pts',(3.47632820495926,-1.,1.95219722189878));
#56656=CARTESIAN_POINT('Ctrl Pts',(3.47632820495926,1.,1.95219722189878));
#56657=CARTESIAN_POINT('Ctrl Pts',(3.48382414832648,-1.,1.95347412486316));
#56658=CARTESIAN_POINT('Ctrl Pts',(3.48382414832648,1.,1.95347412486316));
#56659=CARTESIAN_POINT('Ctrl Pts',(3.49133956289154,-1.,1.95471236969653));
#56660=CARTESIAN_POINT('Ctrl Pts',(3.49133956289154,1.,1.95471236969653));
#56661=CARTESIAN_POINT('Ctrl Pts',(3.49887263575602,-1.,1.9559115382367));
#56662=CARTESIAN_POINT('Ctrl Pts',(3.49887263575602,1.,1.9559115382367));
#56663=CARTESIAN_POINT('Ctrl Pts',(3.50642124159913,-1.,1.95707099606514));
#56664=CARTESIAN_POINT('Ctrl Pts',(3.50642124159913,1.,1.95707099606514));
#56665=CARTESIAN_POINT('Ctrl Pts',(3.51398354617772,-1.,1.95819025316768));
#56666=CARTESIAN_POINT('Ctrl Pts',(3.51398354617772,1.,1.95819025316768));
#56667=CARTESIAN_POINT('Ctrl Pts',(3.52155867431438,-1.,1.95926936324436));
#56668=CARTESIAN_POINT('Ctrl Pts',(3.52155867431438,1.,1.95926936324436));
#56669=CARTESIAN_POINT('Ctrl Pts',(3.52914648844289,-1.,1.96030879411534));
#56670=CARTESIAN_POINT('Ctrl Pts',(3.52914648844289,1.,1.96030879411534));
#56671=CARTESIAN_POINT('Ctrl Pts',(3.53674730625759,-1.,1.96130926212661));
#56672=CARTESIAN_POINT('Ctrl Pts',(3.53674730625759,1.,1.96130926212661));
#56673=CARTESIAN_POINT('Ctrl Pts',(3.54436163300425,-1.,1.96227157573058));
#56674=CARTESIAN_POINT('Ctrl Pts',(3.54436163300425,1.,1.96227157573058));
#56675=CARTESIAN_POINT('Ctrl Pts',(3.55198990600929,-1.,1.96319648628667));
#56676=CARTESIAN_POINT('Ctrl Pts',(3.55198990600929,1.,1.96319648628667));
#56677=CARTESIAN_POINT('Ctrl Pts',(3.55963218706201,-1.,1.96408450906868));
#56678=CARTESIAN_POINT('Ctrl Pts',(3.55963218706201,1.,1.96408450906868));
#56679=CARTESIAN_POINT('Ctrl Pts',(3.56728820357933,-1.,1.96493594634643));
#56680=CARTESIAN_POINT('Ctrl Pts',(3.56728820357933,1.,1.96493594634643));
#56681=CARTESIAN_POINT('Ctrl Pts',(3.57495748601088,-1.,1.96575096652857));
#56682=CARTESIAN_POINT('Ctrl Pts',(3.57495748601088,1.,1.96575096652857));
#56683=CARTESIAN_POINT('Ctrl Pts',(3.58263947663884,-1.,1.9665296668894));
#56684=CARTESIAN_POINT('Ctrl Pts',(3.58263947663884,1.,1.9665296668894));
#56685=CARTESIAN_POINT('Ctrl Pts',(3.5903336402273,-1.,1.96727213799507));
#56686=CARTESIAN_POINT('Ctrl Pts',(3.5903336402273,1.,1.96727213799507));
#56687=CARTESIAN_POINT('Ctrl Pts',(3.59803959819725,-1.,1.96797854118257));
#56688=CARTESIAN_POINT('Ctrl Pts',(3.59803959819725,1.,1.96797854118257));
#56689=CARTESIAN_POINT('Ctrl Pts',(3.60575714017676,-1.,1.96864911885775));
#56690=CARTESIAN_POINT('Ctrl Pts',(3.60575714017676,1.,1.96864911885775));
#56691=CARTESIAN_POINT('Ctrl Pts',(3.61348615496393,-1.,1.96928416040712));
#56692=CARTESIAN_POINT('Ctrl Pts',(3.61348615496393,1.,1.96928416040712));
#56693=CARTESIAN_POINT('Ctrl Pts',(3.62122658401722,-1.,1.96988398129888));
#56694=CARTESIAN_POINT('Ctrl Pts',(3.62122658401722,1.,1.96988398129888));
#56695=CARTESIAN_POINT('Ctrl Pts',(3.62897836973397,-1.,1.97044889850518));
#56696=CARTESIAN_POINT('Ctrl Pts',(3.62897836973397,1.,1.97044889850518));
#56697=CARTESIAN_POINT('Ctrl Pts',(3.63674139590853,-1.,1.97097920454698));
#56698=CARTESIAN_POINT('Ctrl Pts',(3.63674139590853,1.,1.97097920454698));
#56699=CARTESIAN_POINT('Ctrl Pts',(3.64451546724221,-1.,1.97147515441539));
#56700=CARTESIAN_POINT('Ctrl Pts',(3.64451546724221,1.,1.97147515441539));
#56701=CARTESIAN_POINT('Ctrl Pts',(3.65230034717364,-1.,1.97193697240645));
#56702=CARTESIAN_POINT('Ctrl Pts',(3.65230034717364,1.,1.97193697240645));
#56703=CARTESIAN_POINT('Ctrl Pts',(3.66009578166865,-1.,1.97236485439317));
#56704=CARTESIAN_POINT('Ctrl Pts',(3.66009578166865,1.,1.97236485439317));
#56705=CARTESIAN_POINT('Ctrl Pts',(3.66790152751984,-1.,1.9727589719863));
#56706=CARTESIAN_POINT('Ctrl Pts',(3.66790152751984,1.,1.9727589719863));
#56707=CARTESIAN_POINT('Ctrl Pts',(3.67571738106175,-1.,1.97311947678035));
#56708=CARTESIAN_POINT('Ctrl Pts',(3.67571738106175,1.,1.97311947678035));
#56709=CARTESIAN_POINT('Ctrl Pts',(3.68354319913416,-1.,1.97344650303631));
#56710=CARTESIAN_POINT('Ctrl Pts',(3.68354319913416,1.,1.97344650303631));
#56711=CARTESIAN_POINT('Ctrl Pts',(3.69137888597855,-1.,1.97374016224397));
#56712=CARTESIAN_POINT('Ctrl Pts',(3.69137888597855,1.,1.97374016224397));
#56713=CARTESIAN_POINT('Ctrl Pts',(3.69765528558292,-1.,1.97394846382289));
#56714=CARTESIAN_POINT('Ctrl Pts',(3.69765528558292,1.,1.97394846382289));
#56715=CARTESIAN_POINT('Ctrl Pts',(3.70236698911837,-1.,1.97408973726149));
#56716=CARTESIAN_POINT('Ctrl Pts',(3.70236698911837,1.,1.97408973726149));
#56717=CARTESIAN_POINT('Ctrl Pts',(3.7055100813194,-1.,1.974177276451));
#56718=CARTESIAN_POINT('Ctrl Pts',(3.7055100813194,1.,1.974177276451));
#56719=CARTESIAN_POINT('Ctrl Pts',(3.70708211654725,-1.,1.97421938526992));
#56720=CARTESIAN_POINT('Ctrl Pts',(3.70708211654725,1.,1.97421938526992));
#56721=CARTESIAN_POINT('',(3.24413672884902,1.,1.88097764062542));
#56722=CARTESIAN_POINT('Ctrl Pts',(3.24413672884902,-1.,1.88097764062542));
#56723=CARTESIAN_POINT('Ctrl Pts',(3.24413672884902,-0.666666666666667,
1.88097764062542));
#56724=CARTESIAN_POINT('Ctrl Pts',(3.24413672884902,-0.333333333333333,
1.88097764062542));
#56725=CARTESIAN_POINT('Ctrl Pts',(3.24413672884902,0.333333333333333,1.88097764062542));
#56726=CARTESIAN_POINT('Ctrl Pts',(3.24413672884902,0.666666666666667,1.88097764062541));
#56727=CARTESIAN_POINT('Ctrl Pts',(3.24413672884902,1.,1.88097764062541));
#56728=CARTESIAN_POINT('',(3.70708211654725,1.,1.97421938526992));
#56729=CARTESIAN_POINT('',(3.70708211654725,0.,1.97421938526992));
#56730=CARTESIAN_POINT('Ctrl Pts',(3.24413672884902,1.,1.88097764062542));
#56731=CARTESIAN_POINT('Ctrl Pts',(3.24415531671311,1.,1.88102292397987));
#56732=CARTESIAN_POINT('Ctrl Pts',(3.24428080352952,1.,1.88117508446657));
#56733=CARTESIAN_POINT('Ctrl Pts',(3.24480754675942,1.,1.88156537699118));
#56734=CARTESIAN_POINT('Ctrl Pts',(3.24625654410705,1.,1.88242596600422));
#56735=CARTESIAN_POINT('Ctrl Pts',(3.24935200512055,1.,1.88407708646435));
#56736=CARTESIAN_POINT('Ctrl Pts',(3.25408686339298,1.,1.88646802523372));
#56737=CARTESIAN_POINT('Ctrl Pts',(3.2599988519361,1.,1.88934996203508));
#56738=CARTESIAN_POINT('Ctrl Pts',(3.2667765388833,1.,1.89255393500769));
#56739=CARTESIAN_POINT('Ctrl Pts',(3.27407108932908,1.,1.89589172903662));
#56740=CARTESIAN_POINT('Ctrl Pts',(3.28154737912287,1.,1.89918429230425));
#56741=CARTESIAN_POINT('Ctrl Pts',(3.28893448600364,1.,1.9022897124757));
#56742=CARTESIAN_POINT('Ctrl Pts',(3.29608978722258,1.,1.9051389186417));
#56743=CARTESIAN_POINT('Ctrl Pts',(3.30300595568341,1.,1.90773912171424));
#56744=CARTESIAN_POINT('Ctrl Pts',(3.30975721158694,1.,1.91014297830502));
#56745=CARTESIAN_POINT('Ctrl Pts',(3.31646052426395,1.,1.91242616234459));
#56746=CARTESIAN_POINT('Ctrl Pts',(3.32323403454507,1.,1.91466343916612));
#56747=CARTESIAN_POINT('Ctrl Pts',(3.33014884257812,1.,1.91690081930297));
#56748=CARTESIAN_POINT('Ctrl Pts',(3.33721230709948,1.,1.91914609610173));
#56749=CARTESIAN_POINT('Ctrl Pts',(3.34439448941915,1.,1.92138450828378));
#56750=CARTESIAN_POINT('Ctrl Pts',(3.35164424847206,1.,1.92358838440518));
#56751=CARTESIAN_POINT('Ctrl Pts',(3.35890824422976,1.,1.92572846125763));
#56752=CARTESIAN_POINT('Ctrl Pts',(3.36615168657597,1.,1.92778626543803));
#56753=CARTESIAN_POINT('Ctrl Pts',(3.37336807068078,1.,1.92975993109897));
#56754=CARTESIAN_POINT('Ctrl Pts',(3.38056768525577,1.,1.93165739093292));
#56755=CARTESIAN_POINT('Ctrl Pts',(3.38777076883267,1.,1.93349233176794));
#56756=CARTESIAN_POINT('Ctrl Pts',(3.39499923640789,1.,1.93527929945982));
#56757=CARTESIAN_POINT('Ctrl Pts',(3.40226802104093,1.,1.93702857723089));
#56758=CARTESIAN_POINT('Ctrl Pts',(3.40957978266622,1.,1.93874306008132));
#56759=CARTESIAN_POINT('Ctrl Pts',(3.41692971994082,1.,1.94042111965237));
#56760=CARTESIAN_POINT('Ctrl Pts',(3.42430850941497,1.,1.94205835913692));
#56761=CARTESIAN_POINT('Ctrl Pts',(3.43170586602436,1.,1.94364973660285));
#56762=CARTESIAN_POINT('Ctrl Pts',(3.43911410197693,1.,1.94519168842883));
#56763=CARTESIAN_POINT('Ctrl Pts',(3.44653088665685,1.,1.94668377715332));
#56764=CARTESIAN_POINT('Ctrl Pts',(3.45395731584051,1.,1.94812754766524));
#56765=CARTESIAN_POINT('Ctrl Pts',(3.46139661060959,1.,1.94952575850196));
#56766=CARTESIAN_POINT('Ctrl Pts',(3.4688525897419,1.,1.95088147859876));
#56767=CARTESIAN_POINT('Ctrl Pts',(3.47632820495926,1.,1.95219722189878));
#56768=CARTESIAN_POINT('Ctrl Pts',(3.48382414832648,1.,1.95347412486316));
#56769=CARTESIAN_POINT('Ctrl Pts',(3.49133956289154,1.,1.95471236969653));
#56770=CARTESIAN_POINT('Ctrl Pts',(3.49887263575602,1.,1.9559115382367));
#56771=CARTESIAN_POINT('Ctrl Pts',(3.50642124159913,1.,1.95707099606514));
#56772=CARTESIAN_POINT('Ctrl Pts',(3.51398354617772,1.,1.95819025316768));
#56773=CARTESIAN_POINT('Ctrl Pts',(3.52155867431438,1.,1.95926936324436));
#56774=CARTESIAN_POINT('Ctrl Pts',(3.52914648844289,1.,1.96030879411534));
#56775=CARTESIAN_POINT('Ctrl Pts',(3.53674730625759,1.,1.96130926212661));
#56776=CARTESIAN_POINT('Ctrl Pts',(3.54436163300425,1.,1.96227157573058));
#56777=CARTESIAN_POINT('Ctrl Pts',(3.55198990600929,1.,1.96319648628667));
#56778=CARTESIAN_POINT('Ctrl Pts',(3.55963218706201,1.,1.96408450906868));
#56779=CARTESIAN_POINT('Ctrl Pts',(3.56728820357933,1.,1.96493594634643));
#56780=CARTESIAN_POINT('Ctrl Pts',(3.57495748601088,1.,1.96575096652857));
#56781=CARTESIAN_POINT('Ctrl Pts',(3.58263947663884,1.,1.9665296668894));
#56782=CARTESIAN_POINT('Ctrl Pts',(3.5903336402273,1.,1.96727213799507));
#56783=CARTESIAN_POINT('Ctrl Pts',(3.59803959819725,1.,1.96797854118257));
#56784=CARTESIAN_POINT('Ctrl Pts',(3.60575714017676,1.,1.96864911885775));
#56785=CARTESIAN_POINT('Ctrl Pts',(3.61348615496393,1.,1.96928416040712));
#56786=CARTESIAN_POINT('Ctrl Pts',(3.62122658401722,1.,1.96988398129888));
#56787=CARTESIAN_POINT('Ctrl Pts',(3.62897836973397,1.,1.97044889850518));
#56788=CARTESIAN_POINT('Ctrl Pts',(3.63674139590853,1.,1.97097920454698));
#56789=CARTESIAN_POINT('Ctrl Pts',(3.64451546724221,1.,1.97147515441539));
#56790=CARTESIAN_POINT('Ctrl Pts',(3.65230034717364,1.,1.97193697240645));
#56791=CARTESIAN_POINT('Ctrl Pts',(3.66009578166865,1.,1.97236485439317));
#56792=CARTESIAN_POINT('Ctrl Pts',(3.66790152751984,1.,1.9727589719863));
#56793=CARTESIAN_POINT('Ctrl Pts',(3.67571738106175,1.,1.97311947678035));
#56794=CARTESIAN_POINT('Ctrl Pts',(3.68354319913416,1.,1.97344650303631));
#56795=CARTESIAN_POINT('Ctrl Pts',(3.69137888597855,1.,1.97374016224397));
#56796=CARTESIAN_POINT('Ctrl Pts',(3.69765528558292,1.,1.97394846382289));
#56797=CARTESIAN_POINT('Ctrl Pts',(3.70236698911837,1.,1.97408973726149));
#56798=CARTESIAN_POINT('Ctrl Pts',(3.7055100813194,1.,1.974177276451));
#56799=CARTESIAN_POINT('Ctrl Pts',(3.70708211654725,1.,1.97421938526992));
#56800=CARTESIAN_POINT('Origin',(3.70708211654725,0.,1.97421938526992));
#56801=CARTESIAN_POINT('',(3.77614523045147,1.,1.83867539237861));
#56802=CARTESIAN_POINT('Origin',(0.,0.,0.));
#56803=CARTESIAN_POINT('',(3.14877060440425,1.,2.03660101169564));
#56804=CARTESIAN_POINT('Origin',(0.,1.,0.));
#56805=CARTESIAN_POINT('Ctrl Pts',(3.14877060440425,1.,2.03660101169564));
#56806=CARTESIAN_POINT('Ctrl Pts',(3.14877060440425,0.666666666666667,2.03660101169564));
#56807=CARTESIAN_POINT('Ctrl Pts',(3.14877060440425,0.333333333333333,2.03660101169564));
#56808=CARTESIAN_POINT('Ctrl Pts',(3.14877060440425,-0.333333333333333,
2.03660101169564));
#56809=CARTESIAN_POINT('Ctrl Pts',(3.14877060440425,-0.666666666666667,
2.03660101169564));
#56810=CARTESIAN_POINT('Ctrl Pts',(3.14877060440425,-1.,2.03660101169564));
#56811=CARTESIAN_POINT('Ctrl Pts',(3.44202241512147,-1.,2.40675750623143));
#56812=CARTESIAN_POINT('Ctrl Pts',(3.44202241512147,1.,2.40675750623143));
#56813=CARTESIAN_POINT('Ctrl Pts',(3.44127120683402,-1.,2.40537592959345));
#56814=CARTESIAN_POINT('Ctrl Pts',(3.44127120683402,1.,2.40537592959345));
#56815=CARTESIAN_POINT('Ctrl Pts',(3.43976627485223,-1.,2.40261515590099));
#56816=CARTESIAN_POINT('Ctrl Pts',(3.43976627485223,1.,2.40261515590099));
#56817=CARTESIAN_POINT('Ctrl Pts',(3.43750133066036,-1.,2.39848113411429));
#56818=CARTESIAN_POINT('Ctrl Pts',(3.43750133066036,1.,2.39848113411429));
#56819=CARTESIAN_POINT('Ctrl Pts',(3.43446630680436,-1.,2.39298338805823));
#56820=CARTESIAN_POINT('Ctrl Pts',(3.43446630680436,1.,2.39298338805823));
#56821=CARTESIAN_POINT('Ctrl Pts',(3.43064732714472,-1.,2.38613505844641));
#56822=CARTESIAN_POINT('Ctrl Pts',(3.43064732714472,1.,2.38613505844641));
#56823=CARTESIAN_POINT('Ctrl Pts',(3.42680309755241,-1.,2.37931067029517));
#56824=CARTESIAN_POINT('Ctrl Pts',(3.42680309755241,1.,2.37931067029517));
#56825=CARTESIAN_POINT('Ctrl Pts',(3.42293356216595,-1.,2.37251035954351));
#56826=CARTESIAN_POINT('Ctrl Pts',(3.42293356216595,1.,2.37251035954351));
#56827=CARTESIAN_POINT('Ctrl Pts',(3.41903866635384,-1.,2.36573431470314));
#56828=CARTESIAN_POINT('Ctrl Pts',(3.41903866635384,1.,2.36573431470314));
#56829=CARTESIAN_POINT('Ctrl Pts',(3.4151183675076,-1.,2.35898278606449));
#56830=CARTESIAN_POINT('Ctrl Pts',(3.4151183675076,1.,2.35898278606449));
#56831=CARTESIAN_POINT('Ctrl Pts',(3.41117262313464,-1.,2.35225606823649));
#56832=CARTESIAN_POINT('Ctrl Pts',(3.41117262313464,1.,2.35225606823649));
#56833=CARTESIAN_POINT('Ctrl Pts',(3.40720137403888,-1.,2.34555447648901));
#56834=CARTESIAN_POINT('Ctrl Pts',(3.40720137403888,1.,2.34555447648901));
#56835=CARTESIAN_POINT('Ctrl Pts',(3.40320452776646,-1.,2.33887832342715));
#56836=CARTESIAN_POINT('Ctrl Pts',(3.40320452776646,1.,2.33887832342715));
#56837=CARTESIAN_POINT('Ctrl Pts',(3.39918194578115,-1.,2.33222789882601));
#56838=CARTESIAN_POINT('Ctrl Pts',(3.39918194578115,1.,2.33222789882601));
#56839=CARTESIAN_POINT('Ctrl Pts',(3.39513342020045,-1.,2.32560343902683));
#56840=CARTESIAN_POINT('Ctrl Pts',(3.39513342020045,1.,2.32560343902683));
#56841=CARTESIAN_POINT('Ctrl Pts',(3.39105869475112,-1.,2.31900513925627));
#56842=CARTESIAN_POINT('Ctrl Pts',(3.39105869475112,1.,2.31900513925627));
#56843=CARTESIAN_POINT('Ctrl Pts',(3.38695751492659,-1.,2.31243319489505));
#56844=CARTESIAN_POINT('Ctrl Pts',(3.38695751492659,1.,2.31243319489505));
#56845=CARTESIAN_POINT('Ctrl Pts',(3.38282967336676,-1.,2.30588783640389));
#56846=CARTESIAN_POINT('Ctrl Pts',(3.38282967336676,1.,2.30588783640389));
#56847=CARTESIAN_POINT('Ctrl Pts',(3.37867504959382,-1.,2.29936936127588));
#56848=CARTESIAN_POINT('Ctrl Pts',(3.37867504959382,1.,2.29936936127588));
#56849=CARTESIAN_POINT('Ctrl Pts',(3.37449367172707,-1.,2.2928781800731));
#56850=CARTESIAN_POINT('Ctrl Pts',(3.37449367172707,1.,2.2928781800731));
#56851=CARTESIAN_POINT('Ctrl Pts',(3.37028570206357,-1.,2.28641481081045));
#56852=CARTESIAN_POINT('Ctrl Pts',(3.37028570206357,1.,2.28641481081045));
#56853=CARTESIAN_POINT('Ctrl Pts',(3.36605130712978,-1.,2.27997979457968));
#56854=CARTESIAN_POINT('Ctrl Pts',(3.36605130712978,1.,2.27997979457968));
#56855=CARTESIAN_POINT('Ctrl Pts',(3.36179055004369,-1.,2.27357362620902));
#56856=CARTESIAN_POINT('Ctrl Pts',(3.36179055004369,1.,2.27357362620902));
#56857=CARTESIAN_POINT('Ctrl Pts',(3.35750328523077,-1.,2.26719668579921));
#56858=CARTESIAN_POINT('Ctrl Pts',(3.35750328523077,1.,2.26719668579921));
#56859=CARTESIAN_POINT('Ctrl Pts',(3.35318902552676,-1.,2.26084915222484));
#56860=CARTESIAN_POINT('Ctrl Pts',(3.35318902552676,1.,2.26084915222484));
#56861=CARTESIAN_POINT('Ctrl Pts',(3.34884690292342,-1.,2.25453097693524));
#56862=CARTESIAN_POINT('Ctrl Pts',(3.34884690292342,1.,2.25453097693524));
#56863=CARTESIAN_POINT('Ctrl Pts',(3.34447596770768,-1.,2.24824207678288));
#56864=CARTESIAN_POINT('Ctrl Pts',(3.34447596770768,1.,2.24824207678288));
#56865=CARTESIAN_POINT('Ctrl Pts',(3.34007543738044,-1.,2.24198249391437));
#56866=CARTESIAN_POINT('Ctrl Pts',(3.34007543738044,1.,2.24198249391437));
#56867=CARTESIAN_POINT('Ctrl Pts',(3.33564495756478,-1.,2.2357525632881));
#56868=CARTESIAN_POINT('Ctrl Pts',(3.33564495756478,1.,2.2357525632881));
#56869=CARTESIAN_POINT('Ctrl Pts',(3.33118487773593,-1.,2.22955308907221));
#56870=CARTESIAN_POINT('Ctrl Pts',(3.33118487773593,1.,2.22955308907221));
#56871=CARTESIAN_POINT('Ctrl Pts',(3.32669646722871,-1.,2.22338548312759));
#56872=CARTESIAN_POINT('Ctrl Pts',(3.32669646722871,1.,2.22338548312759));
#56873=CARTESIAN_POINT('Ctrl Pts',(3.32218125618955,-1.,2.21725135110889));
#56874=CARTESIAN_POINT('Ctrl Pts',(3.32218125618955,1.,2.21725135110889));
#56875=CARTESIAN_POINT('Ctrl Pts',(3.31764044024231,-1.,2.21115211847872));
#56876=CARTESIAN_POINT('Ctrl Pts',(3.31764044024231,1.,2.21115211847872));
#56877=CARTESIAN_POINT('Ctrl Pts',(3.3130742460895,-1.,2.20508863150608));
#56878=CARTESIAN_POINT('Ctrl Pts',(3.3130742460895,1.,2.20508863150608));
#56879=CARTESIAN_POINT('Ctrl Pts',(3.30848134694596,-1.,2.19906078949925));
#56880=CARTESIAN_POINT('Ctrl Pts',(3.30848134694596,1.,2.19906078949925));
#56881=CARTESIAN_POINT('Ctrl Pts',(3.30385816281831,-1.,2.19306710376112));
#56882=CARTESIAN_POINT('Ctrl Pts',(3.30385816281831,1.,2.19306710376112));
#56883=CARTESIAN_POINT('Ctrl Pts',(3.29920022557635,-1.,2.18710556500325));
#56884=CARTESIAN_POINT('Ctrl Pts',(3.29920022557635,1.,2.18710556500325));
#56885=CARTESIAN_POINT('Ctrl Pts',(3.29450361500484,-1.,2.18117455557062));
#56886=CARTESIAN_POINT('Ctrl Pts',(3.29450361500484,1.,2.18117455557062));
#56887=CARTESIAN_POINT('Ctrl Pts',(3.28976645712566,-1.,2.17527380048422));
#56888=CARTESIAN_POINT('Ctrl Pts',(3.28976645712566,1.,2.17527380048422));
#56889=CARTESIAN_POINT('Ctrl Pts',(3.2849901997973,-1.,2.16940517773459));
#56890=CARTESIAN_POINT('Ctrl Pts',(3.2849901997973,1.,2.16940517773459));
#56891=CARTESIAN_POINT('Ctrl Pts',(3.28018150841414,-1.,2.16357391934434));
#56892=CARTESIAN_POINT('Ctrl Pts',(3.28018150841414,1.,2.16357391934434));
#56893=CARTESIAN_POINT('Ctrl Pts',(3.27534954469206,-1.,2.15778690038359));
#56894=CARTESIAN_POINT('Ctrl Pts',(3.27534954469206,1.,2.15778690038359));
#56895=CARTESIAN_POINT('Ctrl Pts',(3.27050245897244,-1.,2.15205043199818));
#56896=CARTESIAN_POINT('Ctrl Pts',(3.27050245897244,1.,2.15205043199818));
#56897=CARTESIAN_POINT('Ctrl Pts',(3.26564388189764,-1.,2.14636805295663));
#56898=CARTESIAN_POINT('Ctrl Pts',(3.26564388189764,1.,2.14636805295663));
#56899=CARTESIAN_POINT('Ctrl Pts',(3.26077002641868,-1.,2.14073870754258));
#56900=CARTESIAN_POINT('Ctrl Pts',(3.26077002641868,1.,2.14073870754258));
#56901=CARTESIAN_POINT('Ctrl Pts',(3.25586495065027,-1.,2.13515375878786));
#56902=CARTESIAN_POINT('Ctrl Pts',(3.25586495065027,1.,2.13515375878786));
#56903=CARTESIAN_POINT('Ctrl Pts',(3.25090574493994,-1.,2.1296002839681));
#56904=CARTESIAN_POINT('Ctrl Pts',(3.25090574493994,1.,2.1296002839681));
#56905=CARTESIAN_POINT('Ctrl Pts',(3.24587102613347,-1.,2.12406646410943));
#56906=CARTESIAN_POINT('Ctrl Pts',(3.24587102613347,1.,2.12406646410943));
#56907=CARTESIAN_POINT('Ctrl Pts',(3.24074905517282,-1.,2.11854673326972));
#56908=CARTESIAN_POINT('Ctrl Pts',(3.24074905517282,1.,2.11854673326972));
#56909=CARTESIAN_POINT('Ctrl Pts',(3.23554444767115,-1.,2.11304604021784));
#56910=CARTESIAN_POINT('Ctrl Pts',(3.23554444767115,1.,2.11304604021784));
#56911=CARTESIAN_POINT('Ctrl Pts',(3.23028945793334,-1.,2.1075869964248));
#56912=CARTESIAN_POINT('Ctrl Pts',(3.23028945793334,1.,2.1075869964248));
#56913=CARTESIAN_POINT('Ctrl Pts',(3.22503437553496,-1.,2.10220384298534));
#56914=CARTESIAN_POINT('Ctrl Pts',(3.22503437553496,1.,2.10220384298534));
#56915=CARTESIAN_POINT('Ctrl Pts',(3.21982707347067,-1.,2.09692958434933));
#56916=CARTESIAN_POINT('Ctrl Pts',(3.21982707347067,1.,2.09692958434933));
#56917=CARTESIAN_POINT('Ctrl Pts',(3.2146942960168,-1.,2.0917841946046));
#56918=CARTESIAN_POINT('Ctrl Pts',(3.2146942960168,1.,2.0917841946046));
#56919=CARTESIAN_POINT('Ctrl Pts',(3.20962575845433,-1.,2.08676465517435));
#56920=CARTESIAN_POINT('Ctrl Pts',(3.20962575845433,1.,2.08676465517435));
#56921=CARTESIAN_POINT('Ctrl Pts',(3.20454818630635,-1.,2.08182850370816));
#56922=CARTESIAN_POINT('Ctrl Pts',(3.20454818630635,1.,2.08182850370816));
#56923=CARTESIAN_POINT('Ctrl Pts',(3.19934132835879,-1.,2.0769044187063));
#56924=CARTESIAN_POINT('Ctrl Pts',(3.19934132835879,1.,2.0769044187063));
#56925=CARTESIAN_POINT('Ctrl Pts',(3.19388465568113,-1.,2.07192253497765));
#56926=CARTESIAN_POINT('Ctrl Pts',(3.19388465568113,1.,2.07192253497765));
#56927=CARTESIAN_POINT('Ctrl Pts',(3.18809755562297,-1.,2.06684062744065));
#56928=CARTESIAN_POINT('Ctrl Pts',(3.18809755562297,1.,2.06684062744065));
#56929=CARTESIAN_POINT('Ctrl Pts',(3.18197692964677,-1.,2.06166849827143));
#56930=CARTESIAN_POINT('Ctrl Pts',(3.18197692964677,1.,2.06166849827143));
#56931=CARTESIAN_POINT('Ctrl Pts',(3.17564906975592,-1.,2.05650186773279));
#56932=CARTESIAN_POINT('Ctrl Pts',(3.17564906975592,1.,2.05650186773279));
#56933=CARTESIAN_POINT('Ctrl Pts',(3.16936341689859,-1.,2.05151770247452));
#56934=CARTESIAN_POINT('Ctrl Pts',(3.16936341689859,1.,2.05151770247452));
#56935=CARTESIAN_POINT('Ctrl Pts',(3.16343165059235,-1.,2.0469333124766));
#56936=CARTESIAN_POINT('Ctrl Pts',(3.16343165059235,1.,2.0469333124766));
#56937=CARTESIAN_POINT('Ctrl Pts',(3.15817983946525,-1.,2.04297406404132));
#56938=CARTESIAN_POINT('Ctrl Pts',(3.15817983946525,1.,2.04297406404132));
#56939=CARTESIAN_POINT('Ctrl Pts',(3.1538999167466,-1.,2.03984073791432));
#56940=CARTESIAN_POINT('Ctrl Pts',(3.1538999167466,1.,2.03984073791432));
#56941=CARTESIAN_POINT('Ctrl Pts',(3.15079010635326,-1.,2.03766932526171));
#56942=CARTESIAN_POINT('Ctrl Pts',(3.15079010635326,1.,2.03766932526171));
#56943=CARTESIAN_POINT('Ctrl Pts',(3.14931281967585,-1.,2.03675273048882));
#56944=CARTESIAN_POINT('Ctrl Pts',(3.14931281967585,1.,2.03675273048882));
#56945=CARTESIAN_POINT('Ctrl Pts',(3.14878756590499,-1.,2.03653654935384));
#56946=CARTESIAN_POINT('Ctrl Pts',(3.14878756590499,1.,2.03653654935384));
#56947=CARTESIAN_POINT('Ctrl Pts',(3.14869618937138,-1.,2.036601737578));
#56948=CARTESIAN_POINT('Ctrl Pts',(3.14869618937138,1.,2.036601737578));
#56949=CARTESIAN_POINT('Ctrl Pts',(3.1487152044751,-1.,2.03668666247593));
#56950=CARTESIAN_POINT('Ctrl Pts',(3.1487152044751,1.,2.03668666247593));
#56951=CARTESIAN_POINT('',(3.44202241512147,1.,2.40675750623143));
#56952=CARTESIAN_POINT('Ctrl Pts',(3.44202241512147,1.,2.40675750623143));
#56953=CARTESIAN_POINT('Ctrl Pts',(3.44127120683402,1.,2.40537592959345));
#56954=CARTESIAN_POINT('Ctrl Pts',(3.43976627485223,1.,2.40261515590099));
#56955=CARTESIAN_POINT('Ctrl Pts',(3.43750133066036,1.,2.39848113411429));
#56956=CARTESIAN_POINT('Ctrl Pts',(3.43446630680436,1.,2.39298338805823));
#56957=CARTESIAN_POINT('Ctrl Pts',(3.43064732714472,1.,2.38613505844641));
#56958=CARTESIAN_POINT('Ctrl Pts',(3.42680309755241,1.,2.37931067029517));
#56959=CARTESIAN_POINT('Ctrl Pts',(3.42293356216595,1.,2.37251035954351));
#56960=CARTESIAN_POINT('Ctrl Pts',(3.41903866635384,1.,2.36573431470314));
#56961=CARTESIAN_POINT('Ctrl Pts',(3.4151183675076,1.,2.35898278606449));
#56962=CARTESIAN_POINT('Ctrl Pts',(3.41117262313464,1.,2.35225606823649));
#56963=CARTESIAN_POINT('Ctrl Pts',(3.40720137403888,1.,2.34555447648901));
#56964=CARTESIAN_POINT('Ctrl Pts',(3.40320452776646,1.,2.33887832342715));
#56965=CARTESIAN_POINT('Ctrl Pts',(3.39918194578115,1.,2.33222789882601));
#56966=CARTESIAN_POINT('Ctrl Pts',(3.39513342020045,1.,2.32560343902683));
#56967=CARTESIAN_POINT('Ctrl Pts',(3.39105869475112,1.,2.31900513925627));
#56968=CARTESIAN_POINT('Ctrl Pts',(3.38695751492659,1.,2.31243319489505));
#56969=CARTESIAN_POINT('Ctrl Pts',(3.38282967336676,1.,2.30588783640389));
#56970=CARTESIAN_POINT('Ctrl Pts',(3.37867504959382,1.,2.29936936127588));
#56971=CARTESIAN_POINT('Ctrl Pts',(3.37449367172707,1.,2.2928781800731));
#56972=CARTESIAN_POINT('Ctrl Pts',(3.37028570206357,1.,2.28641481081045));
#56973=CARTESIAN_POINT('Ctrl Pts',(3.36605130712978,1.,2.27997979457968));
#56974=CARTESIAN_POINT('Ctrl Pts',(3.36179055004369,1.,2.27357362620902));
#56975=CARTESIAN_POINT('Ctrl Pts',(3.35750328523077,1.,2.26719668579921));
#56976=CARTESIAN_POINT('Ctrl Pts',(3.35318902552676,1.,2.26084915222484));
#56977=CARTESIAN_POINT('Ctrl Pts',(3.34884690292342,1.,2.25453097693524));
#56978=CARTESIAN_POINT('Ctrl Pts',(3.34447596770768,1.,2.24824207678288));
#56979=CARTESIAN_POINT('Ctrl Pts',(3.34007543738044,1.,2.24198249391437));
#56980=CARTESIAN_POINT('Ctrl Pts',(3.33564495756478,1.,2.2357525632881));
#56981=CARTESIAN_POINT('Ctrl Pts',(3.33118487773593,1.,2.22955308907221));
#56982=CARTESIAN_POINT('Ctrl Pts',(3.32669646722871,1.,2.22338548312759));
#56983=CARTESIAN_POINT('Ctrl Pts',(3.32218125618955,1.,2.21725135110889));
#56984=CARTESIAN_POINT('Ctrl Pts',(3.31764044024231,1.,2.21115211847872));
#56985=CARTESIAN_POINT('Ctrl Pts',(3.3130742460895,1.,2.20508863150608));
#56986=CARTESIAN_POINT('Ctrl Pts',(3.30848134694596,1.,2.19906078949925));
#56987=CARTESIAN_POINT('Ctrl Pts',(3.30385816281831,1.,2.19306710376112));
#56988=CARTESIAN_POINT('Ctrl Pts',(3.29920022557635,1.,2.18710556500325));
#56989=CARTESIAN_POINT('Ctrl Pts',(3.29450361500484,1.,2.18117455557062));
#56990=CARTESIAN_POINT('Ctrl Pts',(3.28976645712566,1.,2.17527380048422));
#56991=CARTESIAN_POINT('Ctrl Pts',(3.2849901997973,1.,2.16940517773459));
#56992=CARTESIAN_POINT('Ctrl Pts',(3.28018150841414,1.,2.16357391934434));
#56993=CARTESIAN_POINT('Ctrl Pts',(3.27534954469206,1.,2.15778690038359));
#56994=CARTESIAN_POINT('Ctrl Pts',(3.27050245897244,1.,2.15205043199818));
#56995=CARTESIAN_POINT('Ctrl Pts',(3.26564388189764,1.,2.14636805295663));
#56996=CARTESIAN_POINT('Ctrl Pts',(3.26077002641868,1.,2.14073870754258));
#56997=CARTESIAN_POINT('Ctrl Pts',(3.25586495065027,1.,2.13515375878786));
#56998=CARTESIAN_POINT('Ctrl Pts',(3.25090574493994,1.,2.1296002839681));
#56999=CARTESIAN_POINT('Ctrl Pts',(3.24587102613347,1.,2.12406646410943));
#57000=CARTESIAN_POINT('Ctrl Pts',(3.24074905517282,1.,2.11854673326972));
#57001=CARTESIAN_POINT('Ctrl Pts',(3.23554444767115,1.,2.11304604021784));
#57002=CARTESIAN_POINT('Ctrl Pts',(3.23028945793334,1.,2.1075869964248));
#57003=CARTESIAN_POINT('Ctrl Pts',(3.22503437553496,1.,2.10220384298534));
#57004=CARTESIAN_POINT('Ctrl Pts',(3.21982707347067,1.,2.09692958434933));
#57005=CARTESIAN_POINT('Ctrl Pts',(3.2146942960168,1.,2.0917841946046));
#57006=CARTESIAN_POINT('Ctrl Pts',(3.20962575845433,1.,2.08676465517435));
#57007=CARTESIAN_POINT('Ctrl Pts',(3.20454818630635,1.,2.08182850370816));
#57008=CARTESIAN_POINT('Ctrl Pts',(3.19934132835879,1.,2.0769044187063));
#57009=CARTESIAN_POINT('Ctrl Pts',(3.19388465568113,1.,2.07192253497765));
#57010=CARTESIAN_POINT('Ctrl Pts',(3.18809755562297,1.,2.06684062744065));
#57011=CARTESIAN_POINT('Ctrl Pts',(3.18197692964677,1.,2.06166849827143));
#57012=CARTESIAN_POINT('Ctrl Pts',(3.17564906975592,1.,2.05650186773279));
#57013=CARTESIAN_POINT('Ctrl Pts',(3.16936341689859,1.,2.05151770247452));
#57014=CARTESIAN_POINT('Ctrl Pts',(3.16343165059235,1.,2.0469333124766));
#57015=CARTESIAN_POINT('Ctrl Pts',(3.15817983946525,1.,2.04297406404132));
#57016=CARTESIAN_POINT('Ctrl Pts',(3.1538999167466,1.,2.03984073791432));
#57017=CARTESIAN_POINT('Ctrl Pts',(3.15102344775396,1.,2.03783225496023));
#57018=CARTESIAN_POINT('Ctrl Pts',(3.14959882629936,1.,2.03693188810614));
#57019=CARTESIAN_POINT('Ctrl Pts',(3.14901193669147,1.,2.03663974554941));
#57020=CARTESIAN_POINT('Ctrl Pts',(3.1488193908823,1.,2.03659701539175));
#57021=CARTESIAN_POINT('Ctrl Pts',(3.14877060440425,1.,2.03660101169564));
#57022=CARTESIAN_POINT('',(3.44202241512147,0.,2.40675750623143));
#57023=CARTESIAN_POINT('Ctrl Pts',(2.91001063062876,-1.,2.36523532225181));
#57024=CARTESIAN_POINT('Ctrl Pts',(2.91001063062876,1.,2.36523532225181));
#57025=CARTESIAN_POINT('Ctrl Pts',(2.90992398626211,-1.,2.36524348105112));
#57026=CARTESIAN_POINT('Ctrl Pts',(2.90992398626211,1.,2.36524348105112));
#57027=CARTESIAN_POINT('Ctrl Pts',(2.90989022548032,-1.,2.36535052956938));
#57028=CARTESIAN_POINT('Ctrl Pts',(2.90989022548032,1.,2.36535052956938));
#57029=CARTESIAN_POINT('Ctrl Pts',(2.91025813830041,-1.,2.36578327194741));
#57030=CARTESIAN_POINT('Ctrl Pts',(2.91025813830041,1.,2.36578327194741));
#57031=CARTESIAN_POINT('Ctrl Pts',(2.9115863784204,-1.,2.36690501170627));
#57032=CARTESIAN_POINT('Ctrl Pts',(2.9115863784204,1.,2.36690501170627));
#57033=CARTESIAN_POINT('Ctrl Pts',(2.9146124988314,-1.,2.36919161373173));
#57034=CARTESIAN_POINT('Ctrl Pts',(2.9146124988314,1.,2.36919161373173));
#57035=CARTESIAN_POINT('Ctrl Pts',(2.91891503791411,-1.,2.37229381109821));
#57036=CARTESIAN_POINT('Ctrl Pts',(2.91891503791411,1.,2.37229381109821));
#57037=CARTESIAN_POINT('Ctrl Pts',(2.92430340582608,-1.,2.3760651052403));
#57038=CARTESIAN_POINT('Ctrl Pts',(2.92430340582608,1.,2.3760651052403));
#57039=CARTESIAN_POINT('Ctrl Pts',(2.93049643640206,-1.,2.38028989582073));
#57040=CARTESIAN_POINT('Ctrl Pts',(2.93049643640206,1.,2.38028989582073));
#57041=CARTESIAN_POINT('Ctrl Pts',(2.93717903280391,-1.,2.38472771516311));
#57042=CARTESIAN_POINT('Ctrl Pts',(2.93717903280391,1.,2.38472771516311));
#57043=CARTESIAN_POINT('Ctrl Pts',(2.94404820669076,-1.,2.38914929090759));
#57044=CARTESIAN_POINT('Ctrl Pts',(2.94404820669076,1.,2.38914929090759));
#57045=CARTESIAN_POINT('Ctrl Pts',(2.95085857128439,-1.,2.39337207631667));
#57046=CARTESIAN_POINT('Ctrl Pts',(2.95085857128439,1.,2.39337207631667));
#57047=CARTESIAN_POINT('Ctrl Pts',(2.95748006482942,-1.,2.39730553974517));
#57048=CARTESIAN_POINT('Ctrl Pts',(2.95748006482942,1.,2.39730553974517));
#57049=CARTESIAN_POINT('Ctrl Pts',(2.96390432240312,-1.,2.4009556571164));
#57050=CARTESIAN_POINT('Ctrl Pts',(2.96390432240312,1.,2.4009556571164));
#57051=CARTESIAN_POINT('Ctrl Pts',(2.9701964131236,-1.,2.40438604734919));
#57052=CARTESIAN_POINT('Ctrl Pts',(2.9701964131236,1.,2.40438604734919));
#57053=CARTESIAN_POINT('Ctrl Pts',(2.97646002822422,-1.,2.40768975073713));
#57054=CARTESIAN_POINT('Ctrl Pts',(2.97646002822422,1.,2.40768975073713));
#57055=CARTESIAN_POINT('Ctrl Pts',(2.98280015815107,-1.,2.41095909342571));
#57056=CARTESIAN_POINT('Ctrl Pts',(2.98280015815107,1.,2.41095909342571));
#57057=CARTESIAN_POINT('Ctrl Pts',(2.98927983005796,-1.,2.41425064199586));
#57058=CARTESIAN_POINT('Ctrl Pts',(2.98927983005796,1.,2.41425064199586));
#57059=CARTESIAN_POINT('Ctrl Pts',(2.99590509293503,-1.,2.41757324500514));
#57060=CARTESIAN_POINT('Ctrl Pts',(2.99590509293503,1.,2.41757324500514));
#57061=CARTESIAN_POINT('Ctrl Pts',(3.00264868585996,-1.,2.42090763946779));
#57062=CARTESIAN_POINT('Ctrl Pts',(3.00264868585996,1.,2.42090763946779));
#57063=CARTESIAN_POINT('Ctrl Pts',(3.00946442616658,-1.,2.42421849439613));
#57064=CARTESIAN_POINT('Ctrl Pts',(3.00946442616658,1.,2.42421849439613));
#57065=CARTESIAN_POINT('Ctrl Pts',(3.01630420830504,-1.,2.42746856264168));
#57066=CARTESIAN_POINT('Ctrl Pts',(3.01630420830504,1.,2.42746856264168));
#57067=CARTESIAN_POINT('Ctrl Pts',(3.02313656036004,-1.,2.43063415586637));
#57068=CARTESIAN_POINT('Ctrl Pts',(3.02313656036004,1.,2.43063415586637));
#57069=CARTESIAN_POINT('Ctrl Pts',(3.02995534946978,-1.,2.43371241361488));
#57070=CARTESIAN_POINT('Ctrl Pts',(3.02995534946978,1.,2.43371241361488));
#57071=CARTESIAN_POINT('Ctrl Pts',(3.03676949672821,-1.,2.43671278042414));
#57072=CARTESIAN_POINT('Ctrl Pts',(3.03676949672821,1.,2.43671278042414));
#57073=CARTESIAN_POINT('Ctrl Pts',(3.04359685040555,-1.,2.43965194061857));
#57074=CARTESIAN_POINT('Ctrl Pts',(3.04359685040555,1.,2.43965194061857));
#57075=CARTESIAN_POINT('Ctrl Pts',(3.05045678021504,-1.,2.44254768923105));
#57076=CARTESIAN_POINT('Ctrl Pts',(3.05045678021504,1.,2.44254768923105));
#57077=CARTESIAN_POINT('Ctrl Pts',(3.05736242671506,-1.,2.44541251892556));
#57078=CARTESIAN_POINT('Ctrl Pts',(3.05736242671506,1.,2.44541251892556));
#57079=CARTESIAN_POINT('Ctrl Pts',(3.06431596421405,-1.,2.44824970516544));
#57080=CARTESIAN_POINT('Ctrl Pts',(3.06431596421405,1.,2.44824970516544));
#57081=CARTESIAN_POINT('Ctrl Pts',(3.07131290521297,-1.,2.45105688854422));
#57082=CARTESIAN_POINT('Ctrl Pts',(3.07131290521297,1.,2.45105688854422));
#57083=CARTESIAN_POINT('Ctrl Pts',(3.07834472886139,-1.,2.4538282678779));
#57084=CARTESIAN_POINT('Ctrl Pts',(3.07834472886139,1.,2.4538282678779));
#57085=CARTESIAN_POINT('Ctrl Pts',(3.08540206545315,-1.,2.45655725437039));
#57086=CARTESIAN_POINT('Ctrl Pts',(3.08540206545315,1.,2.45655725437039));
#57087=CARTESIAN_POINT('Ctrl Pts',(3.09247787931887,-1.,2.4592391256388));
#57088=CARTESIAN_POINT('Ctrl Pts',(3.09247787931887,1.,2.4592391256388));
#57089=CARTESIAN_POINT('Ctrl Pts',(3.09956993697052,-1.,2.46187308501884));
#57090=CARTESIAN_POINT('Ctrl Pts',(3.09956993697052,1.,2.46187308501884));
#57091=CARTESIAN_POINT('Ctrl Pts',(3.1066790790198,-1.,2.46446082979646));
#57092=CARTESIAN_POINT('Ctrl Pts',(3.1066790790198,1.,2.46446082979646));
#57093=CARTESIAN_POINT('Ctrl Pts',(3.11380805536122,-1.,2.46700558843506));
#57094=CARTESIAN_POINT('Ctrl Pts',(3.11380805536122,1.,2.46700558843506));
#57095=CARTESIAN_POINT('Ctrl Pts',(3.12096015766983,-1.,2.46951098947469));
#57096=CARTESIAN_POINT('Ctrl Pts',(3.12096015766983,1.,2.46951098947469));
#57097=CARTESIAN_POINT('Ctrl Pts',(3.12813790805952,-1.,2.47197997765871));
#57098=CARTESIAN_POINT('Ctrl Pts',(3.12813790805952,1.,2.47197997765871));
#57099=CARTESIAN_POINT('Ctrl Pts',(3.13534181229295,-1.,2.47441378371932));
#57100=CARTESIAN_POINT('Ctrl Pts',(3.13534181229295,1.,2.47441378371932));
#57101=CARTESIAN_POINT('Ctrl Pts',(3.1425709954655,-1.,2.47681245356109));
#57102=CARTESIAN_POINT('Ctrl Pts',(3.1425709954655,1.,2.47681245356109));
#57103=CARTESIAN_POINT('Ctrl Pts',(3.14982373241352,-1.,2.47917529057029));
#57104=CARTESIAN_POINT('Ctrl Pts',(3.14982373241352,1.,2.47917529057029));
#57105=CARTESIAN_POINT('Ctrl Pts',(3.15709802322739,-1.,2.48150133566571));
#57106=CARTESIAN_POINT('Ctrl Pts',(3.15709802322739,1.,2.48150133566571));
#57107=CARTESIAN_POINT('Ctrl Pts',(3.16439213290161,-1.,2.48378981792725));
#57108=CARTESIAN_POINT('Ctrl Pts',(3.16439213290161,1.,2.48378981792725));
#57109=CARTESIAN_POINT('Ctrl Pts',(3.17170518863313,-1.,2.48604065348587));
#57110=CARTESIAN_POINT('Ctrl Pts',(3.17170518863313,1.,2.48604065348587));
#57111=CARTESIAN_POINT('Ctrl Pts',(3.17903698136622,-1.,2.48825428288201));
#57112=CARTESIAN_POINT('Ctrl Pts',(3.17903698136622,1.,2.48825428288201));
#57113=CARTESIAN_POINT('Ctrl Pts',(3.18638771282266,-1.,2.49043146334059));
#57114=CARTESIAN_POINT('Ctrl Pts',(3.18638771282266,1.,2.49043146334059));
#57115=CARTESIAN_POINT('Ctrl Pts',(3.19375775555798,-1.,2.49257307239848));
#57116=CARTESIAN_POINT('Ctrl Pts',(3.19375775555798,1.,2.49257307239848));
#57117=CARTESIAN_POINT('Ctrl Pts',(3.20114742397588,-1.,2.49467992057755));
#57118=CARTESIAN_POINT('Ctrl Pts',(3.20114742397588,1.,2.49467992057755));
#57119=CARTESIAN_POINT('Ctrl Pts',(3.20855669849836,-1.,2.4967525264737));
#57120=CARTESIAN_POINT('Ctrl Pts',(3.20855669849836,1.,2.4967525264737));
#57121=CARTESIAN_POINT('Ctrl Pts',(3.21598526261286,-1.,2.4987911459939));
#57122=CARTESIAN_POINT('Ctrl Pts',(3.21598526261286,1.,2.4987911459939));
#57123=CARTESIAN_POINT('Ctrl Pts',(3.22343262620503,-1.,2.50079587201958));
#57124=CARTESIAN_POINT('Ctrl Pts',(3.22343262620503,1.,2.50079587201958));
#57125=CARTESIAN_POINT('Ctrl Pts',(3.23089822320646,-1.,2.50276671338111));
#57126=CARTESIAN_POINT('Ctrl Pts',(3.23089822320646,1.,2.50276671338111));
#57127=CARTESIAN_POINT('Ctrl Pts',(3.23838151080319,-1.,2.5047036758003));
#57128=CARTESIAN_POINT('Ctrl Pts',(3.23838151080319,1.,2.5047036758003));
#57129=CARTESIAN_POINT('Ctrl Pts',(3.24588208983849,-1.,2.506606859405));
#57130=CARTESIAN_POINT('Ctrl Pts',(3.24588208983849,1.,2.506606859405));
#57131=CARTESIAN_POINT('Ctrl Pts',(3.25339971460982,-1.,2.50847647070723));
#57132=CARTESIAN_POINT('Ctrl Pts',(3.25339971460982,1.,2.50847647070723));
#57133=CARTESIAN_POINT('Ctrl Pts',(3.26093423001434,-1.,2.51031277813486));
#57134=CARTESIAN_POINT('Ctrl Pts',(3.26093423001434,1.,2.51031277813486));
#57135=CARTESIAN_POINT('Ctrl Pts',(3.26848552888115,-1.,2.51211608411423));
#57136=CARTESIAN_POINT('Ctrl Pts',(3.26848552888115,1.,2.51211608411423));
#57137=CARTESIAN_POINT('Ctrl Pts',(3.27605350473142,-1.,2.513886692704));
#57138=CARTESIAN_POINT('Ctrl Pts',(3.27605350473142,1.,2.513886692704));
#57139=CARTESIAN_POINT('Ctrl Pts',(3.28363799702982,-1.,2.51562487464514));
#57140=CARTESIAN_POINT('Ctrl Pts',(3.28363799702982,1.,2.51562487464514));
#57141=CARTESIAN_POINT('Ctrl Pts',(3.2912387729927,-1.,2.51733085123797));
#57142=CARTESIAN_POINT('Ctrl Pts',(3.2912387729927,1.,2.51733085123797));
#57143=CARTESIAN_POINT('Ctrl Pts',(3.29885556388352,-1.,2.51900480701069));
#57144=CARTESIAN_POINT('Ctrl Pts',(3.29885556388352,1.,2.51900480701069));
#57145=CARTESIAN_POINT('Ctrl Pts',(3.30648808815442,-1.,2.52064689568511));
#57146=CARTESIAN_POINT('Ctrl Pts',(3.30648808815442,1.,2.52064689568511));
#57147=CARTESIAN_POINT('Ctrl Pts',(3.31413607874645,-1.,2.52225724871313));
#57148=CARTESIAN_POINT('Ctrl Pts',(3.31413607874645,1.,2.52225724871313));
#57149=CARTESIAN_POINT('Ctrl Pts',(3.32179931078699,-1.,2.5238359839626));
#57150=CARTESIAN_POINT('Ctrl Pts',(3.32179931078699,1.,2.5238359839626));
#57151=CARTESIAN_POINT('Ctrl Pts',(3.32947762187533,-1.,2.52538321164634));
#57152=CARTESIAN_POINT('Ctrl Pts',(3.32947762187533,1.,2.52538321164634));
#57153=CARTESIAN_POINT('Ctrl Pts',(3.33717089999103,-1.,2.52689902690158));
#57154=CARTESIAN_POINT('Ctrl Pts',(3.33717089999103,1.,2.52689902690158));
#57155=CARTESIAN_POINT('Ctrl Pts',(3.34333744115511,-1.,2.52808660915689));
#57156=CARTESIAN_POINT('Ctrl Pts',(3.34333744115511,1.,2.52808660915689));
#57157=CARTESIAN_POINT('Ctrl Pts',(3.34796903576663,-1.,2.52896321610703));
#57158=CARTESIAN_POINT('Ctrl Pts',(3.34796903576663,1.,2.52896321610703));
#57159=CARTESIAN_POINT('Ctrl Pts',(3.35105973714071,-1.,2.5295413654909));
#57160=CARTESIAN_POINT('Ctrl Pts',(3.35105973714071,1.,2.5295413654909));
#57161=CARTESIAN_POINT('Ctrl Pts',(3.35260583073571,-1.,2.52982887637028));
#57162=CARTESIAN_POINT('Ctrl Pts',(3.35260583073571,1.,2.52982887637028));
#57163=CARTESIAN_POINT('',(2.90994629141676,1.,2.36531447826073));
#57164=CARTESIAN_POINT('Ctrl Pts',(2.90994629141676,-1.,2.36531447826073));
#57165=CARTESIAN_POINT('Ctrl Pts',(2.90994629141676,-0.666666666666667,
2.36531447826073));
#57166=CARTESIAN_POINT('Ctrl Pts',(2.90994629141676,-0.333333333333333,
2.36531447826073));
#57167=CARTESIAN_POINT('Ctrl Pts',(2.90994629141676,0.333333333333333,2.36531447826073));
#57168=CARTESIAN_POINT('Ctrl Pts',(2.90994629141676,0.666666666666667,2.36531447826073));
#57169=CARTESIAN_POINT('Ctrl Pts',(2.90994629141676,1.,2.36531447826073));
#57170=CARTESIAN_POINT('',(3.35260583073571,1.,2.52982887637028));
#57171=CARTESIAN_POINT('',(3.35260583073571,0.,2.52982887637028));
#57172=CARTESIAN_POINT('Ctrl Pts',(2.90994629141676,1.,2.36531447826073));
#57173=CARTESIAN_POINT('Ctrl Pts',(2.90995756655606,1.,2.36536211188453));
#57174=CARTESIAN_POINT('Ctrl Pts',(2.91005770527719,1.,2.36553202948613));
#57175=CARTESIAN_POINT('Ctrl Pts',(2.91051690822156,1.,2.36599991765749));
#57176=CARTESIAN_POINT('Ctrl Pts',(2.91181344022548,1.,2.36707658451664));
#57177=CARTESIAN_POINT('Ctrl Pts',(2.9146124988314,1.,2.36919161373173));
#57178=CARTESIAN_POINT('Ctrl Pts',(2.91891503791411,1.,2.37229381109821));
#57179=CARTESIAN_POINT('Ctrl Pts',(2.92430340582608,1.,2.3760651052403));
#57180=CARTESIAN_POINT('Ctrl Pts',(2.93049643640206,1.,2.38028989582073));
#57181=CARTESIAN_POINT('Ctrl Pts',(2.93717903280391,1.,2.38472771516311));
#57182=CARTESIAN_POINT('Ctrl Pts',(2.94404820669076,1.,2.38914929090759));
#57183=CARTESIAN_POINT('Ctrl Pts',(2.95085857128439,1.,2.39337207631667));
#57184=CARTESIAN_POINT('Ctrl Pts',(2.95748006482942,1.,2.39730553974517));
#57185=CARTESIAN_POINT('Ctrl Pts',(2.96390432240312,1.,2.4009556571164));
#57186=CARTESIAN_POINT('Ctrl Pts',(2.9701964131236,1.,2.40438604734919));
#57187=CARTESIAN_POINT('Ctrl Pts',(2.97646002822422,1.,2.40768975073713));
#57188=CARTESIAN_POINT('Ctrl Pts',(2.98280015815107,1.,2.41095909342571));
#57189=CARTESIAN_POINT('Ctrl Pts',(2.98927983005796,1.,2.41425064199586));
#57190=CARTESIAN_POINT('Ctrl Pts',(2.99590509293503,1.,2.41757324500514));
#57191=CARTESIAN_POINT('Ctrl Pts',(3.00264868585996,1.,2.42090763946779));
#57192=CARTESIAN_POINT('Ctrl Pts',(3.00946442616658,1.,2.42421849439613));
#57193=CARTESIAN_POINT('Ctrl Pts',(3.01630420830504,1.,2.42746856264168));
#57194=CARTESIAN_POINT('Ctrl Pts',(3.02313656036004,1.,2.43063415586637));
#57195=CARTESIAN_POINT('Ctrl Pts',(3.02995534946978,1.,2.43371241361488));
#57196=CARTESIAN_POINT('Ctrl Pts',(3.03676949672821,1.,2.43671278042414));
#57197=CARTESIAN_POINT('Ctrl Pts',(3.04359685040555,1.,2.43965194061857));
#57198=CARTESIAN_POINT('Ctrl Pts',(3.05045678021504,1.,2.44254768923105));
#57199=CARTESIAN_POINT('Ctrl Pts',(3.05736242671506,1.,2.44541251892556));
#57200=CARTESIAN_POINT('Ctrl Pts',(3.06431596421405,1.,2.44824970516544));
#57201=CARTESIAN_POINT('Ctrl Pts',(3.07131290521297,1.,2.45105688854422));
#57202=CARTESIAN_POINT('Ctrl Pts',(3.07834472886139,1.,2.4538282678779));
#57203=CARTESIAN_POINT('Ctrl Pts',(3.08540206545315,1.,2.45655725437039));
#57204=CARTESIAN_POINT('Ctrl Pts',(3.09247787931887,1.,2.4592391256388));
#57205=CARTESIAN_POINT('Ctrl Pts',(3.09956993697052,1.,2.46187308501884));
#57206=CARTESIAN_POINT('Ctrl Pts',(3.1066790790198,1.,2.46446082979646));
#57207=CARTESIAN_POINT('Ctrl Pts',(3.11380805536122,1.,2.46700558843506));
#57208=CARTESIAN_POINT('Ctrl Pts',(3.12096015766983,1.,2.46951098947469));
#57209=CARTESIAN_POINT('Ctrl Pts',(3.12813790805952,1.,2.47197997765871));
#57210=CARTESIAN_POINT('Ctrl Pts',(3.13534181229295,1.,2.47441378371932));
#57211=CARTESIAN_POINT('Ctrl Pts',(3.1425709954655,1.,2.47681245356109));
#57212=CARTESIAN_POINT('Ctrl Pts',(3.14982373241352,1.,2.47917529057029));
#57213=CARTESIAN_POINT('Ctrl Pts',(3.15709802322739,1.,2.48150133566571));
#57214=CARTESIAN_POINT('Ctrl Pts',(3.16439213290161,1.,2.48378981792725));
#57215=CARTESIAN_POINT('Ctrl Pts',(3.17170518863313,1.,2.48604065348587));
#57216=CARTESIAN_POINT('Ctrl Pts',(3.17903698136622,1.,2.48825428288201));
#57217=CARTESIAN_POINT('Ctrl Pts',(3.18638771282266,1.,2.49043146334059));
#57218=CARTESIAN_POINT('Ctrl Pts',(3.19375775555798,1.,2.49257307239848));
#57219=CARTESIAN_POINT('Ctrl Pts',(3.20114742397588,1.,2.49467992057755));
#57220=CARTESIAN_POINT('Ctrl Pts',(3.20855669849836,1.,2.4967525264737));
#57221=CARTESIAN_POINT('Ctrl Pts',(3.21598526261286,1.,2.4987911459939));
#57222=CARTESIAN_POINT('Ctrl Pts',(3.22343262620503,1.,2.50079587201958));
#57223=CARTESIAN_POINT('Ctrl Pts',(3.23089822320646,1.,2.50276671338111));
#57224=CARTESIAN_POINT('Ctrl Pts',(3.23838151080319,1.,2.5047036758003));
#57225=CARTESIAN_POINT('Ctrl Pts',(3.24588208983849,1.,2.506606859405));
#57226=CARTESIAN_POINT('Ctrl Pts',(3.25339971460982,1.,2.50847647070723));
#57227=CARTESIAN_POINT('Ctrl Pts',(3.26093423001434,1.,2.51031277813486));
#57228=CARTESIAN_POINT('Ctrl Pts',(3.26848552888115,1.,2.51211608411423));
#57229=CARTESIAN_POINT('Ctrl Pts',(3.27605350473142,1.,2.513886692704));
#57230=CARTESIAN_POINT('Ctrl Pts',(3.28363799702982,1.,2.51562487464514));
#57231=CARTESIAN_POINT('Ctrl Pts',(3.2912387729927,1.,2.51733085123797));
#57232=CARTESIAN_POINT('Ctrl Pts',(3.29885556388352,1.,2.51900480701069));
#57233=CARTESIAN_POINT('Ctrl Pts',(3.30648808815442,1.,2.52064689568511));
#57234=CARTESIAN_POINT('Ctrl Pts',(3.31413607874645,1.,2.52225724871313));
#57235=CARTESIAN_POINT('Ctrl Pts',(3.32179931078699,1.,2.5238359839626));
#57236=CARTESIAN_POINT('Ctrl Pts',(3.32947762187533,1.,2.52538321164634));
#57237=CARTESIAN_POINT('Ctrl Pts',(3.33717089999103,1.,2.52689902690158));
#57238=CARTESIAN_POINT('Ctrl Pts',(3.34333744115511,1.,2.52808660915689));
#57239=CARTESIAN_POINT('Ctrl Pts',(3.34796903576663,1.,2.52896321610703));
#57240=CARTESIAN_POINT('Ctrl Pts',(3.35105973714071,1.,2.5295413654909));
#57241=CARTESIAN_POINT('Ctrl Pts',(3.35260583073571,1.,2.52982887637028));
#57242=CARTESIAN_POINT('Origin',(3.35260583073571,0.,2.52982887637028));
#57243=CARTESIAN_POINT('',(3.44202241512147,1.,2.40675750623143));
#57244=CARTESIAN_POINT('Origin',(0.,0.,0.));
#57245=CARTESIAN_POINT('',(2.79140942341378,1.,2.50410331873042));
#57246=CARTESIAN_POINT('Origin',(0.,1.,0.));
#57247=CARTESIAN_POINT('Ctrl Pts',(2.79140942341378,1.,2.50410331873043));
#57248=CARTESIAN_POINT('Ctrl Pts',(2.79140942341378,0.666666666666667,2.50410331873043));
#57249=CARTESIAN_POINT('Ctrl Pts',(2.79140942341378,0.333333333333333,2.50410331873042));
#57250=CARTESIAN_POINT('Ctrl Pts',(2.79140942341378,-0.333333333333333,
2.50410331873042));
#57251=CARTESIAN_POINT('Ctrl Pts',(2.79140942341378,-0.666666666666667,
2.50410331873042));
#57252=CARTESIAN_POINT('Ctrl Pts',(2.79140942341378,-1.,2.50410331873042));
#57253=CARTESIAN_POINT('Ctrl Pts',(3.02314558451372,-1.,2.91557726271063));
#57254=CARTESIAN_POINT('Ctrl Pts',(3.02314558451372,1.,2.91557726271063));
#57255=CARTESIAN_POINT('Ctrl Pts',(3.02261975104912,-1.,2.91409518070707));
#57256=CARTESIAN_POINT('Ctrl Pts',(3.02261975104912,1.,2.91409518070707));
#57257=CARTESIAN_POINT('Ctrl Pts',(3.02156522743299,-1.,2.91113297349052));
#57258=CARTESIAN_POINT('Ctrl Pts',(3.02156522743299,1.,2.91113297349052));
#57259=CARTESIAN_POINT('Ctrl Pts',(3.01997487194926,-1.,2.90669553303902));
#57260=CARTESIAN_POINT('Ctrl Pts',(3.01997487194926,1.,2.90669553303902));
#57261=CARTESIAN_POINT('Ctrl Pts',(3.01783725123646,-1.,2.90079069102661));
#57262=CARTESIAN_POINT('Ctrl Pts',(3.01783725123646,1.,2.90079069102661));
#57263=CARTESIAN_POINT('Ctrl Pts',(3.01513660433291,-1.,2.8934292556764));
#57264=CARTESIAN_POINT('Ctrl Pts',(3.01513660433291,1.,2.8934292556764));
#57265=CARTESIAN_POINT('Ctrl Pts',(3.01240727309568,-1.,2.88608751706796));
#57266=CARTESIAN_POINT('Ctrl Pts',(3.01240727309568,1.,2.88608751706796));
#57267=CARTESIAN_POINT('Ctrl Pts',(3.0096491810855,-1.,2.87876560072799));
#57268=CARTESIAN_POINT('Ctrl Pts',(3.0096491810855,1.,2.87876560072799));
#57269=CARTESIAN_POINT('Ctrl Pts',(3.00686224485374,-1.,2.87146368430104));
#57270=CARTESIAN_POINT('Ctrl Pts',(3.00686224485374,1.,2.87146368430104));
#57271=CARTESIAN_POINT('Ctrl Pts',(3.00404638316245,-1.,2.86418200833065));
#57272=CARTESIAN_POINT('Ctrl Pts',(3.00404638316245,1.,2.86418200833065));
#57273=CARTESIAN_POINT('Ctrl Pts',(3.0012015079552,-1.,2.85692085715129));
#57274=CARTESIAN_POINT('Ctrl Pts',(3.0012015079552,1.,2.85692085715129));
#57275=CARTESIAN_POINT('Ctrl Pts',(2.99832751144566,-1.,2.84968053289104));
#57276=CARTESIAN_POINT('Ctrl Pts',(2.99832751144566,1.,2.84968053289104));
#57277=CARTESIAN_POINT('Ctrl Pts',(2.995424253416,-1.,2.84246132984334));
#57278=CARTESIAN_POINT('Ctrl Pts',(2.995424253416,1.,2.84246132984334));
#57279=CARTESIAN_POINT('Ctrl Pts',(2.99249155170479,-1.,2.83526351254383));
#57280=CARTESIAN_POINT('Ctrl Pts',(2.99249155170479,1.,2.83526351254383));
#57281=CARTESIAN_POINT('Ctrl Pts',(2.98952916401699,-1.,2.82808728190402));
#57282=CARTESIAN_POINT('Ctrl Pts',(2.98952916401699,1.,2.82808728190402));
#57283=CARTESIAN_POINT('Ctrl Pts',(2.98653680669434,-1.,2.82093279065704));
#57284=CARTESIAN_POINT('Ctrl Pts',(2.98653680669434,1.,2.82093279065704));
#57285=CARTESIAN_POINT('Ctrl Pts',(2.9835141977994,-1.,2.81380019196454));
#57286=CARTESIAN_POINT('Ctrl Pts',(2.9835141977994,1.,2.81380019196454));
#57287=CARTESIAN_POINT('Ctrl Pts',(2.98046109647299,-1.,2.80668968101162));
#57288=CARTESIAN_POINT('Ctrl Pts',(2.98046109647299,1.,2.80668968101162));
#57289=CARTESIAN_POINT('Ctrl Pts',(2.97737733718242,-1.,2.79960153278186));
#57290=CARTESIAN_POINT('Ctrl Pts',(2.97737733718242,1.,2.79960153278186));
#57291=CARTESIAN_POINT('Ctrl Pts',(2.97426288347475,-1.,2.79253615718147));
#57292=CARTESIAN_POINT('Ctrl Pts',(2.97426288347475,1.,2.79253615718147));
#57293=CARTESIAN_POINT('Ctrl Pts',(2.97111781461349,-1.,2.78549409123657));
#57294=CARTESIAN_POINT('Ctrl Pts',(2.97111781461349,1.,2.78549409123657));
#57295=CARTESIAN_POINT('Ctrl Pts',(2.9679422104295,-1.,2.77847589542767));
#57296=CARTESIAN_POINT('Ctrl Pts',(2.9679422104295,1.,2.77847589542767));
#57297=CARTESIAN_POINT('Ctrl Pts',(2.96473605585548,-1.,2.77148206836464));
#57298=CARTESIAN_POINT('Ctrl Pts',(2.96473605585548,1.,2.77148206836464));
#57299=CARTESIAN_POINT('Ctrl Pts',(2.96149914764832,-1.,2.76451296269571));
#57300=CARTESIAN_POINT('Ctrl Pts',(2.96149914764832,1.,2.76451296269571));
#57301=CARTESIAN_POINT('Ctrl Pts',(2.9582309766594,-1.,2.75756867888393));
#57302=CARTESIAN_POINT('Ctrl Pts',(2.9582309766594,1.,2.75756867888393));
#57303=CARTESIAN_POINT('Ctrl Pts',(2.95493069316211,-1.,2.75064903318996));
#57304=CARTESIAN_POINT('Ctrl Pts',(2.95493069316211,1.,2.75064903318996));
#57305=CARTESIAN_POINT('Ctrl Pts',(2.95159737214304,-1.,2.7437537949221));
#57306=CARTESIAN_POINT('Ctrl Pts',(2.95159737214304,1.,2.7437537949221));
#57307=CARTESIAN_POINT('Ctrl Pts',(2.94823023414381,-1.,2.73688288329825));
#57308=CARTESIAN_POINT('Ctrl Pts',(2.94823023414381,1.,2.73688288329825));
#57309=CARTESIAN_POINT('Ctrl Pts',(2.94482887675139,-1.,2.73003657371613));
#57310=CARTESIAN_POINT('Ctrl Pts',(2.94482887675139,1.,2.73003657371613));
#57311=CARTESIAN_POINT('Ctrl Pts',(2.94139351933882,-1.,2.72321571511322));
#57312=CARTESIAN_POINT('Ctrl Pts',(2.94139351933882,1.,2.72321571511322));
#57313=CARTESIAN_POINT('Ctrl Pts',(2.93792519474955,-1.,2.71642190053575));
#57314=CARTESIAN_POINT('Ctrl Pts',(2.93792519474955,1.,2.71642190053575));
#57315=CARTESIAN_POINT('Ctrl Pts',(2.93442516311167,-1.,2.70965695523776));
#57316=CARTESIAN_POINT('Ctrl Pts',(2.93442516311167,1.,2.70965695523776));
#57317=CARTESIAN_POINT('Ctrl Pts',(2.93089438233746,-1.,2.70292247416881));
#57318=CARTESIAN_POINT('Ctrl Pts',(2.93089438233746,1.,2.70292247416881));
#57319=CARTESIAN_POINT('Ctrl Pts',(2.92733294395268,-1.,2.69621932864302));
#57320=CARTESIAN_POINT('Ctrl Pts',(2.92733294395268,1.,2.69621932864302));
#57321=CARTESIAN_POINT('Ctrl Pts',(2.92373955325876,-1.,2.68954721165342));
#57322=CARTESIAN_POINT('Ctrl Pts',(2.92373955325876,1.,2.68954721165342));
#57323=CARTESIAN_POINT('Ctrl Pts',(2.92011090722152,-1.,2.68290409279689));
#57324=CARTESIAN_POINT('Ctrl Pts',(2.92011090722152,1.,2.68290409279689));
#57325=CARTESIAN_POINT('Ctrl Pts',(2.91644290704281,-1.,2.67628728855309));
#57326=CARTESIAN_POINT('Ctrl Pts',(2.91644290704281,1.,2.67628728855309));
#57327=CARTESIAN_POINT('Ctrl Pts',(2.91273193382876,-1.,2.66969458792627));
#57328=CARTESIAN_POINT('Ctrl Pts',(2.91273193382876,1.,2.66969458792627));
#57329=CARTESIAN_POINT('Ctrl Pts',(2.90897617968921,-1.,2.66312542616809));
#57330=CARTESIAN_POINT('Ctrl Pts',(2.90897617968921,1.,2.66312542616809));
#57331=CARTESIAN_POINT('Ctrl Pts',(2.90517678087467,-1.,2.65658188464287));
#57332=CARTESIAN_POINT('Ctrl Pts',(2.90517678087467,1.,2.65658188464287));
#57333=CARTESIAN_POINT('Ctrl Pts',(2.90133950224879,-1.,2.65007017365576));
#57334=CARTESIAN_POINT('Ctrl Pts',(2.90133950224879,1.,2.65007017365576));
#57335=CARTESIAN_POINT('Ctrl Pts',(2.89747231723361,-1.,2.64359851684146));
#57336=CARTESIAN_POINT('Ctrl Pts',(2.89747231723361,1.,2.64359851684146));
#57337=CARTESIAN_POINT('Ctrl Pts',(2.89358228854557,-1.,2.63717442263944));
#57338=CARTESIAN_POINT('Ctrl Pts',(2.89358228854557,1.,2.63717442263944));
#57339=CARTESIAN_POINT('Ctrl Pts',(2.88967244854243,-1.,2.63080195420771));
#57340=CARTESIAN_POINT('Ctrl Pts',(2.88967244854243,1.,2.63080195420771));
#57341=CARTESIAN_POINT('Ctrl Pts',(2.88573922195049,-1.,2.62447947640253));
#57342=CARTESIAN_POINT('Ctrl Pts',(2.88573922195049,1.,2.62447947640253));
#57343=CARTESIAN_POINT('Ctrl Pts',(2.88176821427502,-1.,2.61819596473087));
#57344=CARTESIAN_POINT('Ctrl Pts',(2.88176821427502,1.,2.61819596473087));
#57345=CARTESIAN_POINT('Ctrl Pts',(2.87773881947885,-1.,2.61193507170928));
#57346=CARTESIAN_POINT('Ctrl Pts',(2.87773881947885,1.,2.61193507170928));
#57347=CARTESIAN_POINT('Ctrl Pts',(2.87363176656475,-1.,2.6056817788128));
#57348=CARTESIAN_POINT('Ctrl Pts',(2.87363176656475,1.,2.6056817788128));
#57349=CARTESIAN_POINT('Ctrl Pts',(2.86943633170712,-1.,2.59942875223202));
#57350=CARTESIAN_POINT('Ctrl Pts',(2.86943633170712,1.,2.59942875223202));
#57351=CARTESIAN_POINT('Ctrl Pts',(2.86515629953528,-1.,2.59318160184921));
#57352=CARTESIAN_POINT('Ctrl Pts',(2.86515629953528,1.,2.59318160184921));
#57353=CARTESIAN_POINT('Ctrl Pts',(2.86081999003668,-1.,2.5869677064356));
#57354=CARTESIAN_POINT('Ctrl Pts',(2.86081999003668,1.,2.5869677064356));
#57355=CARTESIAN_POINT('Ctrl Pts',(2.85647171715147,-1.,2.58082875254407));
#57356=CARTESIAN_POINT('Ctrl Pts',(2.85647171715147,1.,2.58082875254407));
#57357=CARTESIAN_POINT('Ctrl Pts',(2.85215360144482,-1.,2.57480482727128));
#57358=CARTESIAN_POINT('Ctrl Pts',(2.85215360144482,1.,2.57480482727128));
#57359=CARTESIAN_POINT('Ctrl Pts',(2.84788893329091,-1.,2.56891984251743));
#57360=CARTESIAN_POINT('Ctrl Pts',(2.84788893329091,1.,2.56891984251743));
#57361=CARTESIAN_POINT('Ctrl Pts',(2.84366802680211,-1.,2.56316920798489));
#57362=CARTESIAN_POINT('Ctrl Pts',(2.84366802680211,1.,2.56316920798489));
#57363=CARTESIAN_POINT('Ctrl Pts',(2.83942515220699,-1.,2.55749952145165));
#57364=CARTESIAN_POINT('Ctrl Pts',(2.83942515220699,1.,2.55749952145165));
#57365=CARTESIAN_POINT('Ctrl Pts',(2.83505269592412,-1.,2.55182152806964));
#57366=CARTESIAN_POINT('Ctrl Pts',(2.83505269592412,1.,2.55182152806964));
#57367=CARTESIAN_POINT('Ctrl Pts',(2.83044254225794,-1.,2.54604736792542));
#57368=CARTESIAN_POINT('Ctrl Pts',(2.83044254225794,1.,2.54604736792542));
#57369=CARTESIAN_POINT('Ctrl Pts',(2.82552167649157,-1.,2.54012272520141));
#57370=CARTESIAN_POINT('Ctrl Pts',(2.82552167649157,1.,2.54012272520141));
#57371=CARTESIAN_POINT('Ctrl Pts',(2.82028550483744,-1.,2.53405679667463));
#57372=CARTESIAN_POINT('Ctrl Pts',(2.82028550483744,1.,2.53405679667463));
#57373=CARTESIAN_POINT('Ctrl Pts',(2.8148437904867,-1.,2.52796388055457));
#57374=CARTESIAN_POINT('Ctrl Pts',(2.8148437904867,1.,2.52796388055457));
#57375=CARTESIAN_POINT('Ctrl Pts',(2.80941521967234,-1.,2.52205778589922));
#57376=CARTESIAN_POINT('Ctrl Pts',(2.80941521967234,1.,2.52205778589922));
#57377=CARTESIAN_POINT('Ctrl Pts',(2.80427363984939,-1.,2.51660190466067));
#57378=CARTESIAN_POINT('Ctrl Pts',(2.80427363984939,1.,2.51660190466067));
#57379=CARTESIAN_POINT('Ctrl Pts',(2.79970585014308,-1.,2.51186983687947));
#57380=CARTESIAN_POINT('Ctrl Pts',(2.79970585014308,1.,2.51186983687947));
#57381=CARTESIAN_POINT('Ctrl Pts',(2.7959687805717,-1.,2.50810555977564));
#57382=CARTESIAN_POINT('Ctrl Pts',(2.7959687805717,1.,2.50810555977564));
#57383=CARTESIAN_POINT('Ctrl Pts',(2.79323694088143,-1.,2.50547439929077));
#57384=CARTESIAN_POINT('Ctrl Pts',(2.79323694088143,1.,2.50547439929077));
#57385=CARTESIAN_POINT('Ctrl Pts',(2.79192122906739,-1.,2.50433799076945));
#57386=CARTESIAN_POINT('Ctrl Pts',(2.79192122906739,1.,2.50433799076945));
#57387=CARTESIAN_POINT('Ctrl Pts',(2.79143626022225,-1.,2.50404230339032));
#57388=CARTESIAN_POINT('Ctrl Pts',(2.79143626022225,1.,2.50404230339032));
#57389=CARTESIAN_POINT('Ctrl Pts',(2.79133581100044,-1.,2.50409239460011));
#57390=CARTESIAN_POINT('Ctrl Pts',(2.79133581100044,1.,2.50409239460011));
#57391=CARTESIAN_POINT('Ctrl Pts',(2.79134130681569,-1.,2.50417924854921));
#57392=CARTESIAN_POINT('Ctrl Pts',(2.79134130681569,1.,2.50417924854921));
#57393=CARTESIAN_POINT('',(3.02314558451372,1.,2.91557726271063));
#57394=CARTESIAN_POINT('Ctrl Pts',(3.02314558451372,1.,2.91557726271063));
#57395=CARTESIAN_POINT('Ctrl Pts',(3.02261975104912,1.,2.91409518070707));
#57396=CARTESIAN_POINT('Ctrl Pts',(3.02156522743299,1.,2.91113297349052));
#57397=CARTESIAN_POINT('Ctrl Pts',(3.01997487194926,1.,2.90669553303902));
#57398=CARTESIAN_POINT('Ctrl Pts',(3.01783725123646,1.,2.90079069102661));
#57399=CARTESIAN_POINT('Ctrl Pts',(3.01513660433291,1.,2.8934292556764));
#57400=CARTESIAN_POINT('Ctrl Pts',(3.01240727309568,1.,2.88608751706796));
#57401=CARTESIAN_POINT('Ctrl Pts',(3.0096491810855,1.,2.87876560072799));
#57402=CARTESIAN_POINT('Ctrl Pts',(3.00686224485374,1.,2.87146368430104));
#57403=CARTESIAN_POINT('Ctrl Pts',(3.00404638316245,1.,2.86418200833065));
#57404=CARTESIAN_POINT('Ctrl Pts',(3.0012015079552,1.,2.85692085715129));
#57405=CARTESIAN_POINT('Ctrl Pts',(2.99832751144566,1.,2.84968053289104));
#57406=CARTESIAN_POINT('Ctrl Pts',(2.995424253416,1.,2.84246132984334));
#57407=CARTESIAN_POINT('Ctrl Pts',(2.99249155170479,1.,2.83526351254383));
#57408=CARTESIAN_POINT('Ctrl Pts',(2.98952916401699,1.,2.82808728190402));
#57409=CARTESIAN_POINT('Ctrl Pts',(2.98653680669434,1.,2.82093279065704));
#57410=CARTESIAN_POINT('Ctrl Pts',(2.9835141977994,1.,2.81380019196454));
#57411=CARTESIAN_POINT('Ctrl Pts',(2.98046109647299,1.,2.80668968101162));
#57412=CARTESIAN_POINT('Ctrl Pts',(2.97737733718242,1.,2.79960153278186));
#57413=CARTESIAN_POINT('Ctrl Pts',(2.97426288347475,1.,2.79253615718147));
#57414=CARTESIAN_POINT('Ctrl Pts',(2.97111781461349,1.,2.78549409123657));
#57415=CARTESIAN_POINT('Ctrl Pts',(2.9679422104295,1.,2.77847589542767));
#57416=CARTESIAN_POINT('Ctrl Pts',(2.96473605585548,1.,2.77148206836464));
#57417=CARTESIAN_POINT('Ctrl Pts',(2.96149914764832,1.,2.76451296269571));
#57418=CARTESIAN_POINT('Ctrl Pts',(2.9582309766594,1.,2.75756867888393));
#57419=CARTESIAN_POINT('Ctrl Pts',(2.95493069316211,1.,2.75064903318996));
#57420=CARTESIAN_POINT('Ctrl Pts',(2.95159737214304,1.,2.7437537949221));
#57421=CARTESIAN_POINT('Ctrl Pts',(2.94823023414381,1.,2.73688288329825));
#57422=CARTESIAN_POINT('Ctrl Pts',(2.94482887675139,1.,2.73003657371613));
#57423=CARTESIAN_POINT('Ctrl Pts',(2.94139351933882,1.,2.72321571511322));
#57424=CARTESIAN_POINT('Ctrl Pts',(2.93792519474955,1.,2.71642190053575));
#57425=CARTESIAN_POINT('Ctrl Pts',(2.93442516311167,1.,2.70965695523776));
#57426=CARTESIAN_POINT('Ctrl Pts',(2.93089438233746,1.,2.70292247416881));
#57427=CARTESIAN_POINT('Ctrl Pts',(2.92733294395268,1.,2.69621932864302));
#57428=CARTESIAN_POINT('Ctrl Pts',(2.92373955325876,1.,2.68954721165342));
#57429=CARTESIAN_POINT('Ctrl Pts',(2.92011090722152,1.,2.68290409279689));
#57430=CARTESIAN_POINT('Ctrl Pts',(2.91644290704281,1.,2.67628728855309));
#57431=CARTESIAN_POINT('Ctrl Pts',(2.91273193382876,1.,2.66969458792627));
#57432=CARTESIAN_POINT('Ctrl Pts',(2.90897617968921,1.,2.66312542616809));
#57433=CARTESIAN_POINT('Ctrl Pts',(2.90517678087467,1.,2.65658188464287));
#57434=CARTESIAN_POINT('Ctrl Pts',(2.90133950224879,1.,2.65007017365576));
#57435=CARTESIAN_POINT('Ctrl Pts',(2.89747231723361,1.,2.64359851684146));
#57436=CARTESIAN_POINT('Ctrl Pts',(2.89358228854557,1.,2.63717442263944));
#57437=CARTESIAN_POINT('Ctrl Pts',(2.88967244854243,1.,2.63080195420771));
#57438=CARTESIAN_POINT('Ctrl Pts',(2.88573922195049,1.,2.62447947640253));
#57439=CARTESIAN_POINT('Ctrl Pts',(2.88176821427502,1.,2.61819596473087));
#57440=CARTESIAN_POINT('Ctrl Pts',(2.87773881947885,1.,2.61193507170928));
#57441=CARTESIAN_POINT('Ctrl Pts',(2.87363176656475,1.,2.6056817788128));
#57442=CARTESIAN_POINT('Ctrl Pts',(2.86943633170712,1.,2.59942875223202));
#57443=CARTESIAN_POINT('Ctrl Pts',(2.86515629953528,1.,2.59318160184921));
#57444=CARTESIAN_POINT('Ctrl Pts',(2.86081999003668,1.,2.5869677064356));
#57445=CARTESIAN_POINT('Ctrl Pts',(2.85647171715147,1.,2.58082875254407));
#57446=CARTESIAN_POINT('Ctrl Pts',(2.85215360144482,1.,2.57480482727128));
#57447=CARTESIAN_POINT('Ctrl Pts',(2.84788893329091,1.,2.56891984251743));
#57448=CARTESIAN_POINT('Ctrl Pts',(2.84366802680211,1.,2.56316920798489));
#57449=CARTESIAN_POINT('Ctrl Pts',(2.83942515220699,1.,2.55749952145165));
#57450=CARTESIAN_POINT('Ctrl Pts',(2.83505269592412,1.,2.55182152806964));
#57451=CARTESIAN_POINT('Ctrl Pts',(2.83044254225794,1.,2.54604736792542));
#57452=CARTESIAN_POINT('Ctrl Pts',(2.82552167649157,1.,2.54012272520141));
#57453=CARTESIAN_POINT('Ctrl Pts',(2.82028550483744,1.,2.53405679667463));
#57454=CARTESIAN_POINT('Ctrl Pts',(2.8148437904867,1.,2.52796388055457));
#57455=CARTESIAN_POINT('Ctrl Pts',(2.80941521967234,1.,2.52205778589922));
#57456=CARTESIAN_POINT('Ctrl Pts',(2.80427363984939,1.,2.51660190466067));
#57457=CARTESIAN_POINT('Ctrl Pts',(2.79970585014308,1.,2.51186983687947));
#57458=CARTESIAN_POINT('Ctrl Pts',(2.7959687805717,1.,2.50810555977564));
#57459=CARTESIAN_POINT('Ctrl Pts',(2.79344192164204,1.,2.50567182569153));
#57460=CARTESIAN_POINT('Ctrl Pts',(2.79217568804874,1.,2.50455968395235));
#57461=CARTESIAN_POINT('Ctrl Pts',(2.79164172519039,1.,2.50417932839344));
#57462=CARTESIAN_POINT('Ctrl Pts',(2.79145823440899,1.,2.50410700351426));
#57463=CARTESIAN_POINT('Ctrl Pts',(2.79140942341378,1.,2.50410331873042));
#57464=CARTESIAN_POINT('',(3.02314558451372,0.,2.91557726271063));
#57465=CARTESIAN_POINT('Ctrl Pts',(2.5041792485492,-1.,2.79134130681569));
#57466=CARTESIAN_POINT('Ctrl Pts',(2.5041792485492,1.,2.79134130681569));
#57467=CARTESIAN_POINT('Ctrl Pts',(2.50409239460108,-1.,2.7913358110015));
#57468=CARTESIAN_POINT('Ctrl Pts',(2.50409239460108,1.,2.7913358110015));
#57469=CARTESIAN_POINT('Ctrl Pts',(2.50404230339286,-1.,2.79143626022503));
#57470=CARTESIAN_POINT('Ctrl Pts',(2.50404230339286,1.,2.79143626022503));
#57471=CARTESIAN_POINT('Ctrl Pts',(2.5043379907732,-1.,2.79192122907148));
#57472=CARTESIAN_POINT('Ctrl Pts',(2.5043379907732,1.,2.79192122907148));
#57473=CARTESIAN_POINT('Ctrl Pts',(2.50547439929414,-1.,2.7932369408851));
#57474=CARTESIAN_POINT('Ctrl Pts',(2.50547439929414,1.,2.7932369408851));
#57475=CARTESIAN_POINT('Ctrl Pts',(2.5081055597767,-1.,2.79596878057287));
#57476=CARTESIAN_POINT('Ctrl Pts',(2.5081055597767,1.,2.79596878057287));
#57477=CARTESIAN_POINT('Ctrl Pts',(2.51186983687818,-1.,2.79970585014168));
#57478=CARTESIAN_POINT('Ctrl Pts',(2.51186983687818,1.,2.79970585014168));
#57479=CARTESIAN_POINT('Ctrl Pts',(2.51660190465805,-1.,2.80427363984653));
#57480=CARTESIAN_POINT('Ctrl Pts',(2.51660190465805,1.,2.80427363984653));
#57481=CARTESIAN_POINT('Ctrl Pts',(2.52205778589653,-1.,2.80941521966941));
#57482=CARTESIAN_POINT('Ctrl Pts',(2.52205778589653,1.,2.80941521966941));
#57483=CARTESIAN_POINT('Ctrl Pts',(2.52796388055278,-1.,2.81484379048475));
#57484=CARTESIAN_POINT('Ctrl Pts',(2.52796388055278,1.,2.81484379048475));
#57485=CARTESIAN_POINT('Ctrl Pts',(2.53405679667412,-1.,2.82028550483689));
#57486=CARTESIAN_POINT('Ctrl Pts',(2.53405679667412,1.,2.82028550483689));
#57487=CARTESIAN_POINT('Ctrl Pts',(2.54012272520199,-1.,2.8255216764922));
#57488=CARTESIAN_POINT('Ctrl Pts',(2.54012272520199,1.,2.8255216764922));
#57489=CARTESIAN_POINT('Ctrl Pts',(2.54604736792655,-1.,2.83044254225917));
#57490=CARTESIAN_POINT('Ctrl Pts',(2.54604736792655,1.,2.83044254225917));
#57491=CARTESIAN_POINT('Ctrl Pts',(2.55182152807077,-1.,2.83505269592536));
#57492=CARTESIAN_POINT('Ctrl Pts',(2.55182152807077,1.,2.83505269592536));
#57493=CARTESIAN_POINT('Ctrl Pts',(2.55749952145241,-1.,2.83942515220782));
#57494=CARTESIAN_POINT('Ctrl Pts',(2.55749952145241,1.,2.83942515220782));
#57495=CARTESIAN_POINT('Ctrl Pts',(2.56316920798513,-1.,2.84366802680237));
#57496=CARTESIAN_POINT('Ctrl Pts',(2.56316920798513,1.,2.84366802680237));
#57497=CARTESIAN_POINT('Ctrl Pts',(2.56891984251721,-1.,2.84788893329067));
#57498=CARTESIAN_POINT('Ctrl Pts',(2.56891984251721,1.,2.84788893329067));
#57499=CARTESIAN_POINT('Ctrl Pts',(2.57480482727081,-1.,2.85215360144431));
#57500=CARTESIAN_POINT('Ctrl Pts',(2.57480482727081,1.,2.85215360144431));
#57501=CARTESIAN_POINT('Ctrl Pts',(2.58082875254357,-1.,2.85647171715092));
#57502=CARTESIAN_POINT('Ctrl Pts',(2.58082875254357,1.,2.85647171715092));
#57503=CARTESIAN_POINT('Ctrl Pts',(2.58696770643524,-1.,2.86081999003629));
#57504=CARTESIAN_POINT('Ctrl Pts',(2.58696770643524,1.,2.86081999003629));
#57505=CARTESIAN_POINT('Ctrl Pts',(2.59318160184908,-1.,2.86515629953513));
#57506=CARTESIAN_POINT('Ctrl Pts',(2.59318160184908,1.,2.86515629953513));
#57507=CARTESIAN_POINT('Ctrl Pts',(2.5994287522321,-1.,2.86943633170722));
#57508=CARTESIAN_POINT('Ctrl Pts',(2.5994287522321,1.,2.86943633170722));
#57509=CARTESIAN_POINT('Ctrl Pts',(2.60568177881303,-1.,2.87363176656501));
#57510=CARTESIAN_POINT('Ctrl Pts',(2.60568177881303,1.,2.87363176656501));
#57511=CARTESIAN_POINT('Ctrl Pts',(2.61193507170955,-1.,2.87773881947916));
#57512=CARTESIAN_POINT('Ctrl Pts',(2.61193507170955,1.,2.87773881947916));
#57513=CARTESIAN_POINT('Ctrl Pts',(2.61819596473108,-1.,2.88176821427525));
#57514=CARTESIAN_POINT('Ctrl Pts',(2.61819596473108,1.,2.88176821427525));
#57515=CARTESIAN_POINT('Ctrl Pts',(2.62447947640262,-1.,2.88573922195059));
#57516=CARTESIAN_POINT('Ctrl Pts',(2.62447947640262,1.,2.88573922195059));
#57517=CARTESIAN_POINT('Ctrl Pts',(2.63080195420767,-1.,2.88967244854239));
#57518=CARTESIAN_POINT('Ctrl Pts',(2.63080195420767,1.,2.88967244854239));
#57519=CARTESIAN_POINT('Ctrl Pts',(2.63717442263932,-1.,2.89358228854544));
#57520=CARTESIAN_POINT('Ctrl Pts',(2.63717442263932,1.,2.89358228854544));
#57521=CARTESIAN_POINT('Ctrl Pts',(2.64359851684131,-1.,2.89747231723345));
#57522=CARTESIAN_POINT('Ctrl Pts',(2.64359851684131,1.,2.89747231723345));
#57523=CARTESIAN_POINT('Ctrl Pts',(2.65007017365564,-1.,2.90133950224867));
#57524=CARTESIAN_POINT('Ctrl Pts',(2.65007017365564,1.,2.90133950224867));
#57525=CARTESIAN_POINT('Ctrl Pts',(2.65658188464282,-1.,2.90517678087461));
#57526=CARTESIAN_POINT('Ctrl Pts',(2.65658188464282,1.,2.90517678087461));
#57527=CARTESIAN_POINT('Ctrl Pts',(2.6631254261681,-1.,2.90897617968923));
#57528=CARTESIAN_POINT('Ctrl Pts',(2.6631254261681,1.,2.90897617968923));
#57529=CARTESIAN_POINT('Ctrl Pts',(2.66969458792631,-1.,2.91273193382882));
#57530=CARTESIAN_POINT('Ctrl Pts',(2.66969458792631,1.,2.91273193382882));
#57531=CARTESIAN_POINT('Ctrl Pts',(2.67628728855312,-1.,2.91644290704285));
#57532=CARTESIAN_POINT('Ctrl Pts',(2.67628728855312,1.,2.91644290704285));
#57533=CARTESIAN_POINT('Ctrl Pts',(2.68290409279688,-1.,2.92011090722152));
#57534=CARTESIAN_POINT('Ctrl Pts',(2.68290409279688,1.,2.92011090722152));
#57535=CARTESIAN_POINT('Ctrl Pts',(2.68954721165339,-1.,2.92373955325875));
#57536=CARTESIAN_POINT('Ctrl Pts',(2.68954721165339,1.,2.92373955325875));
#57537=CARTESIAN_POINT('Ctrl Pts',(2.69621932864301,-1.,2.92733294395267));
#57538=CARTESIAN_POINT('Ctrl Pts',(2.69621932864301,1.,2.92733294395267));
#57539=CARTESIAN_POINT('Ctrl Pts',(2.70292247416885,-1.,2.9308943823375));
#57540=CARTESIAN_POINT('Ctrl Pts',(2.70292247416885,1.,2.9308943823375));
#57541=CARTESIAN_POINT('Ctrl Pts',(2.70965695523787,-1.,2.93442516311179));
#57542=CARTESIAN_POINT('Ctrl Pts',(2.70965695523787,1.,2.93442516311179));
#57543=CARTESIAN_POINT('Ctrl Pts',(2.71642190053592,-1.,2.93792519474972));
#57544=CARTESIAN_POINT('Ctrl Pts',(2.71642190053592,1.,2.93792519474972));
#57545=CARTESIAN_POINT('Ctrl Pts',(2.72321571511337,-1.,2.94139351933897));
#57546=CARTESIAN_POINT('Ctrl Pts',(2.72321571511337,1.,2.94139351933897));
#57547=CARTESIAN_POINT('Ctrl Pts',(2.73003657371616,-1.,2.94482887675143));
#57548=CARTESIAN_POINT('Ctrl Pts',(2.73003657371616,1.,2.94482887675143));
#57549=CARTESIAN_POINT('Ctrl Pts',(2.73688288329808,-1.,2.94823023414364));
#57550=CARTESIAN_POINT('Ctrl Pts',(2.73688288329808,1.,2.94823023414364));
#57551=CARTESIAN_POINT('Ctrl Pts',(2.74375379492172,-1.,2.95159737214266));
#57552=CARTESIAN_POINT('Ctrl Pts',(2.74375379492172,1.,2.95159737214266));
#57553=CARTESIAN_POINT('Ctrl Pts',(2.75064903318947,-1.,2.95493069316161));
#57554=CARTESIAN_POINT('Ctrl Pts',(2.75064903318947,1.,2.95493069316161));
#57555=CARTESIAN_POINT('Ctrl Pts',(2.7575686788835,-1.,2.95823097665896));
#57556=CARTESIAN_POINT('Ctrl Pts',(2.7575686788835,1.,2.95823097665896));
#57557=CARTESIAN_POINT('Ctrl Pts',(2.76451296269557,-1.,2.96149914764818));
#57558=CARTESIAN_POINT('Ctrl Pts',(2.76451296269557,1.,2.96149914764818));
#57559=CARTESIAN_POINT('Ctrl Pts',(2.77148206836498,-1.,2.96473605585583));
#57560=CARTESIAN_POINT('Ctrl Pts',(2.77148206836498,1.,2.96473605585583));
#57561=CARTESIAN_POINT('Ctrl Pts',(2.7784758954285,-1.,2.96794221043036));
#57562=CARTESIAN_POINT('Ctrl Pts',(2.7784758954285,1.,2.96794221043036));
#57563=CARTESIAN_POINT('Ctrl Pts',(2.78549409123769,-1.,2.97111781461465));
#57564=CARTESIAN_POINT('Ctrl Pts',(2.78549409123769,1.,2.97111781461465));
#57565=CARTESIAN_POINT('Ctrl Pts',(2.79253615718248,-1.,2.9742628834758));
#57566=CARTESIAN_POINT('Ctrl Pts',(2.79253615718248,1.,2.9742628834758));
#57567=CARTESIAN_POINT('Ctrl Pts',(2.7996015327823,-1.,2.97737733718287));
#57568=CARTESIAN_POINT('Ctrl Pts',(2.7996015327823,1.,2.97737733718287));
#57569=CARTESIAN_POINT('Ctrl Pts',(2.80668968101106,-1.,2.98046109647241));
#57570=CARTESIAN_POINT('Ctrl Pts',(2.80668968101106,1.,2.98046109647241));
#57571=CARTESIAN_POINT('Ctrl Pts',(2.81380019196286,-1.,2.98351419779767));
#57572=CARTESIAN_POINT('Ctrl Pts',(2.81380019196286,1.,2.98351419779767));
#57573=CARTESIAN_POINT('Ctrl Pts',(2.82093279065457,-1.,2.9865368066918));
#57574=CARTESIAN_POINT('Ctrl Pts',(2.82093279065457,1.,2.9865368066918));
#57575=CARTESIAN_POINT('Ctrl Pts',(2.82808728190157,-1.,2.98952916401446));
#57576=CARTESIAN_POINT('Ctrl Pts',(2.82808728190157,1.,2.98952916401446));
#57577=CARTESIAN_POINT('Ctrl Pts',(2.83526351254248,-1.,2.9924915517034));
#57578=CARTESIAN_POINT('Ctrl Pts',(2.83526351254248,1.,2.9924915517034));
#57579=CARTESIAN_POINT('Ctrl Pts',(2.84246132984415,-1.,2.99542425341685));
#57580=CARTESIAN_POINT('Ctrl Pts',(2.84246132984415,1.,2.99542425341685));
#57581=CARTESIAN_POINT('Ctrl Pts',(2.84968053289451,-1.,2.99832751144925));
#57582=CARTESIAN_POINT('Ctrl Pts',(2.84968053289451,1.,2.99832751144925));
#57583=CARTESIAN_POINT('Ctrl Pts',(2.85692085715685,-1.,3.00120150796095));
#57584=CARTESIAN_POINT('Ctrl Pts',(2.85692085715685,1.,3.00120150796095));
#57585=CARTESIAN_POINT('Ctrl Pts',(2.86418200833667,-1.,3.00404638316867));
#57586=CARTESIAN_POINT('Ctrl Pts',(2.86418200833667,1.,3.00404638316867));
#57587=CARTESIAN_POINT('Ctrl Pts',(2.87146368430501,-1.,3.00686224485784));
#57588=CARTESIAN_POINT('Ctrl Pts',(2.87146368430501,1.,3.00686224485784));
#57589=CARTESIAN_POINT('Ctrl Pts',(2.87876560072727,-1.,3.00964918108476));
#57590=CARTESIAN_POINT('Ctrl Pts',(2.87876560072727,1.,3.00964918108476));
#57591=CARTESIAN_POINT('Ctrl Pts',(2.8860875170608,-1.,3.01240727308829));
#57592=CARTESIAN_POINT('Ctrl Pts',(2.8860875170608,1.,3.01240727308829));
#57593=CARTESIAN_POINT('Ctrl Pts',(2.89342925566321,-1.,3.01513660431928));
#57594=CARTESIAN_POINT('Ctrl Pts',(2.89342925566321,1.,3.01513660431928));
#57595=CARTESIAN_POINT('Ctrl Pts',(2.9007906910105,-1.,3.01783725121981));
#57596=CARTESIAN_POINT('Ctrl Pts',(2.9007906910105,1.,3.01783725121981));
#57597=CARTESIAN_POINT('Ctrl Pts',(2.90669553302526,-1.,3.01997487193503));
#57598=CARTESIAN_POINT('Ctrl Pts',(2.90669553302526,1.,3.01997487193503));
#57599=CARTESIAN_POINT('Ctrl Pts',(2.91113297348212,-1.,3.02156522742431));
#57600=CARTESIAN_POINT('Ctrl Pts',(2.91113297348212,1.,3.02156522742431));
#57601=CARTESIAN_POINT('Ctrl Pts',(2.91409518070399,-1.,3.02261975104593));
#57602=CARTESIAN_POINT('Ctrl Pts',(2.91409518070399,1.,3.02261975104593));
#57603=CARTESIAN_POINT('Ctrl Pts',(2.91557726271063,-1.,3.02314558451372));
#57604=CARTESIAN_POINT('Ctrl Pts',(2.91557726271063,1.,3.02314558451372));
#57605=CARTESIAN_POINT('',(2.50410331873176,1.,2.79140942341258));
#57606=CARTESIAN_POINT('Ctrl Pts',(2.50410331873176,-1.,2.79140942341258));
#57607=CARTESIAN_POINT('Ctrl Pts',(2.50410331873176,-0.666666666666667,
2.79140942341258));
#57608=CARTESIAN_POINT('Ctrl Pts',(2.50410331873176,-0.333333333333333,
2.79140942341258));
#57609=CARTESIAN_POINT('Ctrl Pts',(2.50410331873176,0.333333333333333,2.79140942341258));
#57610=CARTESIAN_POINT('Ctrl Pts',(2.50410331873176,0.666666666666667,2.79140942341258));
#57611=CARTESIAN_POINT('Ctrl Pts',(2.50410331873176,1.,2.79140942341258));
#57612=CARTESIAN_POINT('',(2.91557726271063,1.,3.02314558451372));
#57613=CARTESIAN_POINT('',(2.91557726271063,0.,3.02314558451372));
#57614=CARTESIAN_POINT('Ctrl Pts',(2.50410331873176,1.,2.79140942341258));
#57615=CARTESIAN_POINT('Ctrl Pts',(2.50410700351493,1.,2.79145823440781));
#57616=CARTESIAN_POINT('Ctrl Pts',(2.50417932839313,1.,2.79164172518905));
#57617=CARTESIAN_POINT('Ctrl Pts',(2.50455968395146,1.,2.79217568804755));
#57618=CARTESIAN_POINT('Ctrl Pts',(2.50567182569081,1.,2.79344192164147));
#57619=CARTESIAN_POINT('Ctrl Pts',(2.5081055597767,1.,2.79596878057287));
#57620=CARTESIAN_POINT('Ctrl Pts',(2.51186983687818,1.,2.79970585014168));
#57621=CARTESIAN_POINT('Ctrl Pts',(2.51660190465805,1.,2.80427363984653));
#57622=CARTESIAN_POINT('Ctrl Pts',(2.52205778589653,1.,2.80941521966941));
#57623=CARTESIAN_POINT('Ctrl Pts',(2.52796388055278,1.,2.81484379048475));
#57624=CARTESIAN_POINT('Ctrl Pts',(2.53405679667412,1.,2.82028550483689));
#57625=CARTESIAN_POINT('Ctrl Pts',(2.54012272520199,1.,2.8255216764922));
#57626=CARTESIAN_POINT('Ctrl Pts',(2.54604736792655,1.,2.83044254225917));
#57627=CARTESIAN_POINT('Ctrl Pts',(2.55182152807077,1.,2.83505269592536));
#57628=CARTESIAN_POINT('Ctrl Pts',(2.55749952145241,1.,2.83942515220782));
#57629=CARTESIAN_POINT('Ctrl Pts',(2.56316920798513,1.,2.84366802680237));
#57630=CARTESIAN_POINT('Ctrl Pts',(2.56891984251721,1.,2.84788893329067));
#57631=CARTESIAN_POINT('Ctrl Pts',(2.57480482727081,1.,2.85215360144431));
#57632=CARTESIAN_POINT('Ctrl Pts',(2.58082875254357,1.,2.85647171715092));
#57633=CARTESIAN_POINT('Ctrl Pts',(2.58696770643524,1.,2.86081999003629));
#57634=CARTESIAN_POINT('Ctrl Pts',(2.59318160184908,1.,2.86515629953513));
#57635=CARTESIAN_POINT('Ctrl Pts',(2.5994287522321,1.,2.86943633170722));
#57636=CARTESIAN_POINT('Ctrl Pts',(2.60568177881303,1.,2.87363176656501));
#57637=CARTESIAN_POINT('Ctrl Pts',(2.61193507170955,1.,2.87773881947916));
#57638=CARTESIAN_POINT('Ctrl Pts',(2.61819596473108,1.,2.88176821427525));
#57639=CARTESIAN_POINT('Ctrl Pts',(2.62447947640262,1.,2.88573922195059));
#57640=CARTESIAN_POINT('Ctrl Pts',(2.63080195420767,1.,2.88967244854239));
#57641=CARTESIAN_POINT('Ctrl Pts',(2.63717442263932,1.,2.89358228854544));
#57642=CARTESIAN_POINT('Ctrl Pts',(2.64359851684131,1.,2.89747231723345));
#57643=CARTESIAN_POINT('Ctrl Pts',(2.65007017365564,1.,2.90133950224867));
#57644=CARTESIAN_POINT('Ctrl Pts',(2.65658188464282,1.,2.90517678087461));
#57645=CARTESIAN_POINT('Ctrl Pts',(2.6631254261681,1.,2.90897617968923));
#57646=CARTESIAN_POINT('Ctrl Pts',(2.66969458792631,1.,2.91273193382882));
#57647=CARTESIAN_POINT('Ctrl Pts',(2.67628728855312,1.,2.91644290704285));
#57648=CARTESIAN_POINT('Ctrl Pts',(2.68290409279688,1.,2.92011090722152));
#57649=CARTESIAN_POINT('Ctrl Pts',(2.68954721165339,1.,2.92373955325875));
#57650=CARTESIAN_POINT('Ctrl Pts',(2.69621932864301,1.,2.92733294395267));
#57651=CARTESIAN_POINT('Ctrl Pts',(2.70292247416885,1.,2.9308943823375));
#57652=CARTESIAN_POINT('Ctrl Pts',(2.70965695523787,1.,2.93442516311179));
#57653=CARTESIAN_POINT('Ctrl Pts',(2.71642190053592,1.,2.93792519474972));
#57654=CARTESIAN_POINT('Ctrl Pts',(2.72321571511337,1.,2.94139351933897));
#57655=CARTESIAN_POINT('Ctrl Pts',(2.73003657371616,1.,2.94482887675143));
#57656=CARTESIAN_POINT('Ctrl Pts',(2.73688288329808,1.,2.94823023414364));
#57657=CARTESIAN_POINT('Ctrl Pts',(2.74375379492172,1.,2.95159737214266));
#57658=CARTESIAN_POINT('Ctrl Pts',(2.75064903318947,1.,2.95493069316161));
#57659=CARTESIAN_POINT('Ctrl Pts',(2.7575686788835,1.,2.95823097665896));
#57660=CARTESIAN_POINT('Ctrl Pts',(2.76451296269557,1.,2.96149914764818));
#57661=CARTESIAN_POINT('Ctrl Pts',(2.77148206836498,1.,2.96473605585583));
#57662=CARTESIAN_POINT('Ctrl Pts',(2.7784758954285,1.,2.96794221043036));
#57663=CARTESIAN_POINT('Ctrl Pts',(2.78549409123769,1.,2.97111781461465));
#57664=CARTESIAN_POINT('Ctrl Pts',(2.79253615718248,1.,2.9742628834758));
#57665=CARTESIAN_POINT('Ctrl Pts',(2.7996015327823,1.,2.97737733718287));
#57666=CARTESIAN_POINT('Ctrl Pts',(2.80668968101106,1.,2.98046109647241));
#57667=CARTESIAN_POINT('Ctrl Pts',(2.81380019196286,1.,2.98351419779767));
#57668=CARTESIAN_POINT('Ctrl Pts',(2.82093279065457,1.,2.9865368066918));
#57669=CARTESIAN_POINT('Ctrl Pts',(2.82808728190157,1.,2.98952916401446));
#57670=CARTESIAN_POINT('Ctrl Pts',(2.83526351254248,1.,2.9924915517034));
#57671=CARTESIAN_POINT('Ctrl Pts',(2.84246132984415,1.,2.99542425341685));
#57672=CARTESIAN_POINT('Ctrl Pts',(2.84968053289451,1.,2.99832751144925));
#57673=CARTESIAN_POINT('Ctrl Pts',(2.85692085715685,1.,3.00120150796095));
#57674=CARTESIAN_POINT('Ctrl Pts',(2.86418200833667,1.,3.00404638316867));
#57675=CARTESIAN_POINT('Ctrl Pts',(2.87146368430501,1.,3.00686224485784));
#57676=CARTESIAN_POINT('Ctrl Pts',(2.87876560072727,1.,3.00964918108476));
#57677=CARTESIAN_POINT('Ctrl Pts',(2.8860875170608,1.,3.01240727308829));
#57678=CARTESIAN_POINT('Ctrl Pts',(2.89342925566321,1.,3.01513660431928));
#57679=CARTESIAN_POINT('Ctrl Pts',(2.9007906910105,1.,3.01783725121981));
#57680=CARTESIAN_POINT('Ctrl Pts',(2.90669553302526,1.,3.01997487193503));
#57681=CARTESIAN_POINT('Ctrl Pts',(2.91113297348212,1.,3.02156522742431));
#57682=CARTESIAN_POINT('Ctrl Pts',(2.91409518070399,1.,3.02261975104593));
#57683=CARTESIAN_POINT('Ctrl Pts',(2.91557726271063,1.,3.02314558451372));
#57684=CARTESIAN_POINT('Origin',(2.91557726271063,0.,3.02314558451372));
#57685=CARTESIAN_POINT('',(3.02314558451372,1.,2.91557726271063));
#57686=CARTESIAN_POINT('Origin',(0.,0.,0.));
#57687=CARTESIAN_POINT('',(2.36531447826213,1.,2.90994629141562));
#57688=CARTESIAN_POINT('Origin',(0.,1.,0.));
#57689=CARTESIAN_POINT('Ctrl Pts',(2.36531447826213,1.,2.90994629141563));
#57690=CARTESIAN_POINT('Ctrl Pts',(2.36531447826213,0.666666666666667,2.90994629141563));
#57691=CARTESIAN_POINT('Ctrl Pts',(2.36531447826213,0.333333333333333,2.90994629141563));
#57692=CARTESIAN_POINT('Ctrl Pts',(2.36531447826213,-0.333333333333333,
2.90994629141563));
#57693=CARTESIAN_POINT('Ctrl Pts',(2.36531447826213,-0.666666666666667,
2.90994629141563));
#57694=CARTESIAN_POINT('Ctrl Pts',(2.36531447826213,-1.,2.90994629141563));
#57695=CARTESIAN_POINT('Ctrl Pts',(2.52982887637028,-1.,3.35260583073571));
#57696=CARTESIAN_POINT('Ctrl Pts',(2.52982887637028,1.,3.35260583073571));
#57697=CARTESIAN_POINT('Ctrl Pts',(2.52954136549357,-1.,3.35105973714426));
#57698=CARTESIAN_POINT('Ctrl Pts',(2.52954136549357,1.,3.35105973714426));
#57699=CARTESIAN_POINT('Ctrl Pts',(2.5289632161143,-1.,3.34796903577628));
#57700=CARTESIAN_POINT('Ctrl Pts',(2.5289632161143,1.,3.34796903577628));
#57701=CARTESIAN_POINT('Ctrl Pts',(2.52808660916879,-1.,3.34333744117093));
#57702=CARTESIAN_POINT('Ctrl Pts',(2.52808660916879,1.,3.34333744117093));
#57703=CARTESIAN_POINT('Ctrl Pts',(2.52689902691551,-1.,3.33717090000955));
#57704=CARTESIAN_POINT('Ctrl Pts',(2.52689902691551,1.,3.33717090000955));
#57705=CARTESIAN_POINT('Ctrl Pts',(2.52538321165774,-1.,3.32947762189049));
#57706=CARTESIAN_POINT('Ctrl Pts',(2.52538321165774,1.,3.32947762189049));
#57707=CARTESIAN_POINT('Ctrl Pts',(2.52383598396878,-1.,3.32179931079521));
#57708=CARTESIAN_POINT('Ctrl Pts',(2.52383598396878,1.,3.32179931079521));
#57709=CARTESIAN_POINT('Ctrl Pts',(2.52225724871375,-1.,3.31413607874727));
#57710=CARTESIAN_POINT('Ctrl Pts',(2.52225724871375,1.,3.31413607874727));
#57711=CARTESIAN_POINT('Ctrl Pts',(2.52064689568167,-1.,3.30648808814986));
#57712=CARTESIAN_POINT('Ctrl Pts',(2.52064689568167,1.,3.30648808814986));
#57713=CARTESIAN_POINT('Ctrl Pts',(2.51900480700548,-1.,3.29885556387661));
#57714=CARTESIAN_POINT('Ctrl Pts',(2.51900480700548,1.,3.29885556387661));
#57715=CARTESIAN_POINT('Ctrl Pts',(2.51733085123316,-1.,3.2912387729863));
#57716=CARTESIAN_POINT('Ctrl Pts',(2.51733085123316,1.,3.2912387729863));
#57717=CARTESIAN_POINT('Ctrl Pts',(2.51562487464214,-1.,3.28363799702583));
#57718=CARTESIAN_POINT('Ctrl Pts',(2.51562487464214,1.,3.28363799702583));
#57719=CARTESIAN_POINT('Ctrl Pts',(2.51388669270329,-1.,3.27605350473048));
#57720=CARTESIAN_POINT('Ctrl Pts',(2.51388669270329,1.,3.27605350473048));
#57721=CARTESIAN_POINT('Ctrl Pts',(2.51211608411539,-1.,3.26848552888271));
#57722=CARTESIAN_POINT('Ctrl Pts',(2.51211608411539,1.,3.26848552888271));
#57723=CARTESIAN_POINT('Ctrl Pts',(2.51031277813697,-1.,3.26093423001716));
#57724=CARTESIAN_POINT('Ctrl Pts',(2.51031277813697,1.,3.26093423001716));
#57725=CARTESIAN_POINT('Ctrl Pts',(2.50847647070936,-1.,3.25339971461265));
#57726=CARTESIAN_POINT('Ctrl Pts',(2.50847647070936,1.,3.25339971461265));
#57727=CARTESIAN_POINT('Ctrl Pts',(2.50660685940645,-1.,3.24588208984042));
#57728=CARTESIAN_POINT('Ctrl Pts',(2.50660685940645,1.,3.24588208984042));
#57729=CARTESIAN_POINT('Ctrl Pts',(2.50470367580078,-1.,3.23838151080383));
#57730=CARTESIAN_POINT('Ctrl Pts',(2.50470367580078,1.,3.23838151080383));
#57731=CARTESIAN_POINT('Ctrl Pts',(2.50276671338074,-1.,3.23089822320596));
#57732=CARTESIAN_POINT('Ctrl Pts',(2.50276671338074,1.,3.23089822320596));
#57733=CARTESIAN_POINT('Ctrl Pts',(2.5007958720187,-1.,3.22343262620387));
#57734=CARTESIAN_POINT('Ctrl Pts',(2.5007958720187,1.,3.22343262620387));
#57735=CARTESIAN_POINT('Ctrl Pts',(2.49879114599293,-1.,3.21598526261157));
#57736=CARTESIAN_POINT('Ctrl Pts',(2.49879114599293,1.,3.21598526261157));
#57737=CARTESIAN_POINT('Ctrl Pts',(2.49675252647298,-1.,3.2085566984974));
#57738=CARTESIAN_POINT('Ctrl Pts',(2.49675252647298,1.,3.2085566984974));
#57739=CARTESIAN_POINT('Ctrl Pts',(2.49467992057726,-1.,3.20114742397549));
#57740=CARTESIAN_POINT('Ctrl Pts',(2.49467992057726,1.,3.20114742397549));
#57741=CARTESIAN_POINT('Ctrl Pts',(2.4925730723986,-1.,3.19375775555814));
#57742=CARTESIAN_POINT('Ctrl Pts',(2.4925730723986,1.,3.19375775555814));
#57743=CARTESIAN_POINT('Ctrl Pts',(2.49043146334095,-1.,3.18638771282315));
#57744=CARTESIAN_POINT('Ctrl Pts',(2.49043146334095,1.,3.18638771282315));
#57745=CARTESIAN_POINT('Ctrl Pts',(2.48825428288242,-1.,3.17903698136679));
#57746=CARTESIAN_POINT('Ctrl Pts',(2.48825428288242,1.,3.17903698136679));
#57747=CARTESIAN_POINT('Ctrl Pts',(2.48604065348619,-1.,3.17170518863357));
#57748=CARTESIAN_POINT('Ctrl Pts',(2.48604065348619,1.,3.17170518863357));
#57749=CARTESIAN_POINT('Ctrl Pts',(2.48378981792739,-1.,3.16439213290181));
#57750=CARTESIAN_POINT('Ctrl Pts',(2.48378981792739,1.,3.16439213290181));
#57751=CARTESIAN_POINT('Ctrl Pts',(2.48150133566568,-1.,3.15709802322735));
#57752=CARTESIAN_POINT('Ctrl Pts',(2.48150133566568,1.,3.15709802322735));
#57753=CARTESIAN_POINT('Ctrl Pts',(2.47917529057016,-1.,3.14982373241335));
#57754=CARTESIAN_POINT('Ctrl Pts',(2.47917529057016,1.,3.14982373241335));
#57755=CARTESIAN_POINT('Ctrl Pts',(2.47681245356095,-1.,3.14257099546531));
#57756=CARTESIAN_POINT('Ctrl Pts',(2.47681245356095,1.,3.14257099546531));
#57757=CARTESIAN_POINT('Ctrl Pts',(2.47441378371923,-1.,3.13534181229282));
#57758=CARTESIAN_POINT('Ctrl Pts',(2.47441378371923,1.,3.13534181229282));
#57759=CARTESIAN_POINT('Ctrl Pts',(2.47197997765868,-1.,3.12813790805948));
#57760=CARTESIAN_POINT('Ctrl Pts',(2.47197997765868,1.,3.12813790805948));
#57761=CARTESIAN_POINT('Ctrl Pts',(2.4695109894747,-1.,3.12096015766984));
#57762=CARTESIAN_POINT('Ctrl Pts',(2.4695109894747,1.,3.12096015766984));
#57763=CARTESIAN_POINT('Ctrl Pts',(2.46700558843507,-1.,3.11380805536124));
#57764=CARTESIAN_POINT('Ctrl Pts',(2.46700558843507,1.,3.11380805536124));
#57765=CARTESIAN_POINT('Ctrl Pts',(2.46446082979645,-1.,3.10667907901981));
#57766=CARTESIAN_POINT('Ctrl Pts',(2.46446082979645,1.,3.10667907901981));
#57767=CARTESIAN_POINT('Ctrl Pts',(2.4618730850188,-1.,3.09956993697048));
#57768=CARTESIAN_POINT('Ctrl Pts',(2.4618730850188,1.,3.09956993697048));
#57769=CARTESIAN_POINT('Ctrl Pts',(2.45923912563875,-1.,3.09247787931881));
#57770=CARTESIAN_POINT('Ctrl Pts',(2.45923912563875,1.,3.09247787931881));
#57771=CARTESIAN_POINT('Ctrl Pts',(2.45655725437037,-1.,3.08540206545313));
#57772=CARTESIAN_POINT('Ctrl Pts',(2.45655725437037,1.,3.08540206545313));
#57773=CARTESIAN_POINT('Ctrl Pts',(2.45382826787795,-1.,3.07834472886145));
#57774=CARTESIAN_POINT('Ctrl Pts',(2.45382826787795,1.,3.07834472886145));
#57775=CARTESIAN_POINT('Ctrl Pts',(2.45105688854432,-1.,3.0713129052131));
#57776=CARTESIAN_POINT('Ctrl Pts',(2.45105688854432,1.,3.0713129052131));
#57777=CARTESIAN_POINT('Ctrl Pts',(2.44824970516557,-1.,3.06431596421422));
#57778=CARTESIAN_POINT('Ctrl Pts',(2.44824970516557,1.,3.06431596421422));
#57779=CARTESIAN_POINT('Ctrl Pts',(2.44541251892568,-1.,3.05736242671521));
#57780=CARTESIAN_POINT('Ctrl Pts',(2.44541251892568,1.,3.05736242671521));
#57781=CARTESIAN_POINT('Ctrl Pts',(2.44254768923109,-1.,3.05045678021509));
#57782=CARTESIAN_POINT('Ctrl Pts',(2.44254768923109,1.,3.05045678021509));
#57783=CARTESIAN_POINT('Ctrl Pts',(2.43965194061849,-1.,3.04359685040545));
#57784=CARTESIAN_POINT('Ctrl Pts',(2.43965194061849,1.,3.04359685040545));
#57785=CARTESIAN_POINT('Ctrl Pts',(2.43671278042394,-1.,3.03676949672797));
#57786=CARTESIAN_POINT('Ctrl Pts',(2.43671278042394,1.,3.03676949672797));
#57787=CARTESIAN_POINT('Ctrl Pts',(2.43371241361462,-1.,3.02995534946946));
#57788=CARTESIAN_POINT('Ctrl Pts',(2.43371241361462,1.,3.02995534946946));
#57789=CARTESIAN_POINT('Ctrl Pts',(2.43063415586615,-1.,3.02313656035977));
#57790=CARTESIAN_POINT('Ctrl Pts',(2.43063415586615,1.,3.02313656035977));
#57791=CARTESIAN_POINT('Ctrl Pts',(2.4274685626416,-1.,3.01630420830494));
#57792=CARTESIAN_POINT('Ctrl Pts',(2.4274685626416,1.,3.01630420830494));
#57793=CARTESIAN_POINT('Ctrl Pts',(2.42421849439625,-1.,3.00946442616674));
#57794=CARTESIAN_POINT('Ctrl Pts',(2.42421849439625,1.,3.00946442616674));
#57795=CARTESIAN_POINT('Ctrl Pts',(2.42090763946812,-1.,3.00264868586038));
#57796=CARTESIAN_POINT('Ctrl Pts',(2.42090763946812,1.,3.00264868586038));
#57797=CARTESIAN_POINT('Ctrl Pts',(2.4175732450056,-1.,2.99590509293561));
#57798=CARTESIAN_POINT('Ctrl Pts',(2.4175732450056,1.,2.99590509293561));
#57799=CARTESIAN_POINT('Ctrl Pts',(2.4142506419963,-1.,2.98927983005851));
#57800=CARTESIAN_POINT('Ctrl Pts',(2.4142506419963,1.,2.98927983005851));
#57801=CARTESIAN_POINT('Ctrl Pts',(2.41095909342591,-1.,2.98280015815132));
#57802=CARTESIAN_POINT('Ctrl Pts',(2.41095909342591,1.,2.98280015815132));
#57803=CARTESIAN_POINT('Ctrl Pts',(2.40768975073691,-1.,2.97646002822395));
#57804=CARTESIAN_POINT('Ctrl Pts',(2.40768975073691,1.,2.97646002822395));
#57805=CARTESIAN_POINT('Ctrl Pts',(2.40438604734848,-1.,2.97019641312272));
#57806=CARTESIAN_POINT('Ctrl Pts',(2.40438604734848,1.,2.97019641312272));
#57807=CARTESIAN_POINT('Ctrl Pts',(2.40095565711535,-1.,2.96390432240181));
#57808=CARTESIAN_POINT('Ctrl Pts',(2.40095565711535,1.,2.96390432240181));
#57809=CARTESIAN_POINT('Ctrl Pts',(2.39730553974412,-1.,2.95748006482811));
#57810=CARTESIAN_POINT('Ctrl Pts',(2.39730553974412,1.,2.95748006482811));
#57811=CARTESIAN_POINT('Ctrl Pts',(2.39337207631613,-1.,2.95085857128372));
#57812=CARTESIAN_POINT('Ctrl Pts',(2.39337207631613,1.,2.95085857128372));
#57813=CARTESIAN_POINT('Ctrl Pts',(2.38914929090806,-1.,2.94404820669135));
#57814=CARTESIAN_POINT('Ctrl Pts',(2.38914929090806,1.,2.94404820669135));
#57815=CARTESIAN_POINT('Ctrl Pts',(2.38472771516476,-1.,2.93717903280599));
#57816=CARTESIAN_POINT('Ctrl Pts',(2.38472771516476,1.,2.93717903280599));
#57817=CARTESIAN_POINT('Ctrl Pts',(2.3802898958232,-1.,2.93049643640517));
#57818=CARTESIAN_POINT('Ctrl Pts',(2.3802898958232,1.,2.93049643640517));
#57819=CARTESIAN_POINT('Ctrl Pts',(2.37606510524271,-1.,2.92430340582912));
#57820=CARTESIAN_POINT('Ctrl Pts',(2.37606510524271,1.,2.92430340582912));
#57821=CARTESIAN_POINT('Ctrl Pts',(2.37229381109939,-1.,2.9189150379156));
#57822=CARTESIAN_POINT('Ctrl Pts',(2.37229381109939,1.,2.9189150379156));
#57823=CARTESIAN_POINT('Ctrl Pts',(2.36919161373074,-1.,2.91461249883016));
#57824=CARTESIAN_POINT('Ctrl Pts',(2.36919161373074,1.,2.91461249883016));
#57825=CARTESIAN_POINT('Ctrl Pts',(2.36690501170317,-1.,2.9115863784165));
#57826=CARTESIAN_POINT('Ctrl Pts',(2.36690501170317,1.,2.9115863784165));
#57827=CARTESIAN_POINT('Ctrl Pts',(2.36578327194396,-1.,2.91025813829606));
#57828=CARTESIAN_POINT('Ctrl Pts',(2.36578327194396,1.,2.91025813829606));
#57829=CARTESIAN_POINT('Ctrl Pts',(2.36535052956704,-1.,2.90989022547738));
#57830=CARTESIAN_POINT('Ctrl Pts',(2.36535052956704,1.,2.90989022547738));
#57831=CARTESIAN_POINT('Ctrl Pts',(2.36524348105023,-1.,2.90992398626098));
#57832=CARTESIAN_POINT('Ctrl Pts',(2.36524348105023,1.,2.90992398626098));
#57833=CARTESIAN_POINT('Ctrl Pts',(2.36523532225181,-1.,2.91001063062876));
#57834=CARTESIAN_POINT('Ctrl Pts',(2.36523532225181,1.,2.91001063062876));
#57835=CARTESIAN_POINT('',(2.52982887637028,1.,3.35260583073571));
#57836=CARTESIAN_POINT('Ctrl Pts',(2.52982887637028,1.,3.35260583073571));
#57837=CARTESIAN_POINT('Ctrl Pts',(2.52954136549357,1.,3.35105973714426));
#57838=CARTESIAN_POINT('Ctrl Pts',(2.5289632161143,1.,3.34796903577628));
#57839=CARTESIAN_POINT('Ctrl Pts',(2.52808660916879,1.,3.34333744117093));
#57840=CARTESIAN_POINT('Ctrl Pts',(2.52689902691551,1.,3.33717090000955));
#57841=CARTESIAN_POINT('Ctrl Pts',(2.52538321165774,1.,3.32947762189049));
#57842=CARTESIAN_POINT('Ctrl Pts',(2.52383598396878,1.,3.32179931079521));
#57843=CARTESIAN_POINT('Ctrl Pts',(2.52225724871375,1.,3.31413607874727));
#57844=CARTESIAN_POINT('Ctrl Pts',(2.52064689568167,1.,3.30648808814986));
#57845=CARTESIAN_POINT('Ctrl Pts',(2.51900480700548,1.,3.29885556387661));
#57846=CARTESIAN_POINT('Ctrl Pts',(2.51733085123316,1.,3.2912387729863));
#57847=CARTESIAN_POINT('Ctrl Pts',(2.51562487464214,1.,3.28363799702583));
#57848=CARTESIAN_POINT('Ctrl Pts',(2.51388669270329,1.,3.27605350473048));
#57849=CARTESIAN_POINT('Ctrl Pts',(2.51211608411539,1.,3.26848552888271));
#57850=CARTESIAN_POINT('Ctrl Pts',(2.51031277813697,1.,3.26093423001716));
#57851=CARTESIAN_POINT('Ctrl Pts',(2.50847647070936,1.,3.25339971461265));
#57852=CARTESIAN_POINT('Ctrl Pts',(2.50660685940645,1.,3.24588208984042));
#57853=CARTESIAN_POINT('Ctrl Pts',(2.50470367580078,1.,3.23838151080383));
#57854=CARTESIAN_POINT('Ctrl Pts',(2.50276671338074,1.,3.23089822320596));
#57855=CARTESIAN_POINT('Ctrl Pts',(2.5007958720187,1.,3.22343262620387));
#57856=CARTESIAN_POINT('Ctrl Pts',(2.49879114599293,1.,3.21598526261157));
#57857=CARTESIAN_POINT('Ctrl Pts',(2.49675252647298,1.,3.2085566984974));
#57858=CARTESIAN_POINT('Ctrl Pts',(2.49467992057726,1.,3.20114742397549));
#57859=CARTESIAN_POINT('Ctrl Pts',(2.4925730723986,1.,3.19375775555814));
#57860=CARTESIAN_POINT('Ctrl Pts',(2.49043146334095,1.,3.18638771282315));
#57861=CARTESIAN_POINT('Ctrl Pts',(2.48825428288242,1.,3.17903698136679));
#57862=CARTESIAN_POINT('Ctrl Pts',(2.48604065348619,1.,3.17170518863357));
#57863=CARTESIAN_POINT('Ctrl Pts',(2.48378981792739,1.,3.16439213290181));
#57864=CARTESIAN_POINT('Ctrl Pts',(2.48150133566568,1.,3.15709802322735));
#57865=CARTESIAN_POINT('Ctrl Pts',(2.47917529057016,1.,3.14982373241335));
#57866=CARTESIAN_POINT('Ctrl Pts',(2.47681245356095,1.,3.14257099546531));
#57867=CARTESIAN_POINT('Ctrl Pts',(2.47441378371923,1.,3.13534181229282));
#57868=CARTESIAN_POINT('Ctrl Pts',(2.47197997765868,1.,3.12813790805948));
#57869=CARTESIAN_POINT('Ctrl Pts',(2.4695109894747,1.,3.12096015766984));
#57870=CARTESIAN_POINT('Ctrl Pts',(2.46700558843507,1.,3.11380805536124));
#57871=CARTESIAN_POINT('Ctrl Pts',(2.46446082979645,1.,3.10667907901981));
#57872=CARTESIAN_POINT('Ctrl Pts',(2.4618730850188,1.,3.09956993697048));
#57873=CARTESIAN_POINT('Ctrl Pts',(2.45923912563875,1.,3.09247787931881));
#57874=CARTESIAN_POINT('Ctrl Pts',(2.45655725437037,1.,3.08540206545313));
#57875=CARTESIAN_POINT('Ctrl Pts',(2.45382826787795,1.,3.07834472886145));
#57876=CARTESIAN_POINT('Ctrl Pts',(2.45105688854432,1.,3.0713129052131));
#57877=CARTESIAN_POINT('Ctrl Pts',(2.44824970516557,1.,3.06431596421422));
#57878=CARTESIAN_POINT('Ctrl Pts',(2.44541251892568,1.,3.05736242671521));
#57879=CARTESIAN_POINT('Ctrl Pts',(2.44254768923109,1.,3.05045678021509));
#57880=CARTESIAN_POINT('Ctrl Pts',(2.43965194061849,1.,3.04359685040545));
#57881=CARTESIAN_POINT('Ctrl Pts',(2.43671278042394,1.,3.03676949672797));
#57882=CARTESIAN_POINT('Ctrl Pts',(2.43371241361462,1.,3.02995534946946));
#57883=CARTESIAN_POINT('Ctrl Pts',(2.43063415586615,1.,3.02313656035977));
#57884=CARTESIAN_POINT('Ctrl Pts',(2.4274685626416,1.,3.01630420830494));
#57885=CARTESIAN_POINT('Ctrl Pts',(2.42421849439625,1.,3.00946442616674));
#57886=CARTESIAN_POINT('Ctrl Pts',(2.42090763946812,1.,3.00264868586038));
#57887=CARTESIAN_POINT('Ctrl Pts',(2.4175732450056,1.,2.99590509293561));
#57888=CARTESIAN_POINT('Ctrl Pts',(2.4142506419963,1.,2.98927983005851));
#57889=CARTESIAN_POINT('Ctrl Pts',(2.41095909342591,1.,2.98280015815132));
#57890=CARTESIAN_POINT('Ctrl Pts',(2.40768975073691,1.,2.97646002822395));
#57891=CARTESIAN_POINT('Ctrl Pts',(2.40438604734848,1.,2.97019641312272));
#57892=CARTESIAN_POINT('Ctrl Pts',(2.40095565711535,1.,2.96390432240181));
#57893=CARTESIAN_POINT('Ctrl Pts',(2.39730553974412,1.,2.95748006482811));
#57894=CARTESIAN_POINT('Ctrl Pts',(2.39337207631613,1.,2.95085857128372));
#57895=CARTESIAN_POINT('Ctrl Pts',(2.38914929090806,1.,2.94404820669135));
#57896=CARTESIAN_POINT('Ctrl Pts',(2.38472771516476,1.,2.93717903280599));
#57897=CARTESIAN_POINT('Ctrl Pts',(2.3802898958232,1.,2.93049643640517));
#57898=CARTESIAN_POINT('Ctrl Pts',(2.37606510524271,1.,2.92430340582912));
#57899=CARTESIAN_POINT('Ctrl Pts',(2.37229381109939,1.,2.9189150379156));
#57900=CARTESIAN_POINT('Ctrl Pts',(2.36919161373074,1.,2.91461249883016));
#57901=CARTESIAN_POINT('Ctrl Pts',(2.36707658451709,1.,2.91181344022628));
#57902=CARTESIAN_POINT('Ctrl Pts',(2.36599991765853,1.,2.91051690822262));
#57903=CARTESIAN_POINT('Ctrl Pts',(2.36553202948741,1.,2.91005770527771));
#57904=CARTESIAN_POINT('Ctrl Pts',(2.3653621118858,1.,2.90995756655559));
#57905=CARTESIAN_POINT('Ctrl Pts',(2.36531447826213,1.,2.90994629141563));
#57906=CARTESIAN_POINT('',(2.52982887637028,0.,3.35260583073571));
#57907=CARTESIAN_POINT('Ctrl Pts',(2.03668666247593,-1.,3.1487152044751));
#57908=CARTESIAN_POINT('Ctrl Pts',(2.03668666247593,1.,3.1487152044751));
#57909=CARTESIAN_POINT('Ctrl Pts',(2.03660173757879,-1.,3.14869618937258));
#57910=CARTESIAN_POINT('Ctrl Pts',(2.03660173757879,1.,3.14869618937258));
#57911=CARTESIAN_POINT('Ctrl Pts',(2.03653654935591,-1.,3.14878756590812));
#57912=CARTESIAN_POINT('Ctrl Pts',(2.03653654935591,1.,3.14878756590812));
#57913=CARTESIAN_POINT('Ctrl Pts',(2.03675273049189,-1.,3.14931281968048));
#57914=CARTESIAN_POINT('Ctrl Pts',(2.03675273049189,1.,3.14931281968048));
#57915=CARTESIAN_POINT('Ctrl Pts',(2.03766932526445,-1.,3.15079010635742));
#57916=CARTESIAN_POINT('Ctrl Pts',(2.03766932526445,1.,3.15079010635742));
#57917=CARTESIAN_POINT('Ctrl Pts',(2.03984073791519,-1.,3.15389991674792));
#57918=CARTESIAN_POINT('Ctrl Pts',(2.03984073791519,1.,3.15389991674792));
#57919=CARTESIAN_POINT('Ctrl Pts',(2.04297406404027,-1.,3.15817983946367));
#57920=CARTESIAN_POINT('Ctrl Pts',(2.04297406404027,1.,3.15817983946367));
#57921=CARTESIAN_POINT('Ctrl Pts',(2.04693331247446,-1.,3.16343165058912));
#57922=CARTESIAN_POINT('Ctrl Pts',(2.04693331247446,1.,3.16343165058912));
#57923=CARTESIAN_POINT('Ctrl Pts',(2.05151770247233,-1.,3.16936341689527));
#57924=CARTESIAN_POINT('Ctrl Pts',(2.05151770247233,1.,3.16936341689527));
#57925=CARTESIAN_POINT('Ctrl Pts',(2.05650186773132,-1.,3.17564906975371));
#57926=CARTESIAN_POINT('Ctrl Pts',(2.05650186773132,1.,3.17564906975371));
#57927=CARTESIAN_POINT('Ctrl Pts',(2.06166849827101,-1.,3.18197692964614));
#57928=CARTESIAN_POINT('Ctrl Pts',(2.06166849827101,1.,3.18197692964614));
#57929=CARTESIAN_POINT('Ctrl Pts',(2.06684062744112,-1.,3.18809755562368));
#57930=CARTESIAN_POINT('Ctrl Pts',(2.06684062744112,1.,3.18809755562368));
#57931=CARTESIAN_POINT('Ctrl Pts',(2.07192253497857,-1.,3.19388465568252));
#57932=CARTESIAN_POINT('Ctrl Pts',(2.07192253497857,1.,3.19388465568252));
#57933=CARTESIAN_POINT('Ctrl Pts',(2.07690441870722,-1.,3.19934132836019));
#57934=CARTESIAN_POINT('Ctrl Pts',(2.07690441870722,1.,3.19934132836019));
#57935=CARTESIAN_POINT('Ctrl Pts',(2.08182850370878,-1.,3.2045481863073));
#57936=CARTESIAN_POINT('Ctrl Pts',(2.08182850370878,1.,3.2045481863073));
#57937=CARTESIAN_POINT('Ctrl Pts',(2.08676465517455,-1.,3.20962575845463));
#57938=CARTESIAN_POINT('Ctrl Pts',(2.08676465517455,1.,3.20962575845463));
#57939=CARTESIAN_POINT('Ctrl Pts',(2.09178419460443,-1.,3.21469429601654));
#57940=CARTESIAN_POINT('Ctrl Pts',(2.09178419460443,1.,3.21469429601654));
#57941=CARTESIAN_POINT('Ctrl Pts',(2.09692958434895,-1.,3.21982707347009));
#57942=CARTESIAN_POINT('Ctrl Pts',(2.09692958434895,1.,3.21982707347009));
#57943=CARTESIAN_POINT('Ctrl Pts',(2.10220384298492,-1.,3.22503437553434));
#57944=CARTESIAN_POINT('Ctrl Pts',(2.10220384298492,1.,3.22503437553434));
#57945=CARTESIAN_POINT('Ctrl Pts',(2.10758699642451,-1.,3.23028945793289));
#57946=CARTESIAN_POINT('Ctrl Pts',(2.10758699642451,1.,3.23028945793289));
#57947=CARTESIAN_POINT('Ctrl Pts',(2.11304604021773,-1.,3.23554444767099));
#57948=CARTESIAN_POINT('Ctrl Pts',(2.11304604021773,1.,3.23554444767099));
#57949=CARTESIAN_POINT('Ctrl Pts',(2.11854673326979,-1.,3.24074905517293));
#57950=CARTESIAN_POINT('Ctrl Pts',(2.11854673326979,1.,3.24074905517293));
#57951=CARTESIAN_POINT('Ctrl Pts',(2.12406646410962,-1.,3.24587102613376));
#57952=CARTESIAN_POINT('Ctrl Pts',(2.12406646410962,1.,3.24587102613376));
#57953=CARTESIAN_POINT('Ctrl Pts',(2.12960028396832,-1.,3.25090574494028));
#57954=CARTESIAN_POINT('Ctrl Pts',(2.12960028396832,1.,3.25090574494028));
#57955=CARTESIAN_POINT('Ctrl Pts',(2.13515375878803,-1.,3.25586495065054));
#57956=CARTESIAN_POINT('Ctrl Pts',(2.13515375878803,1.,3.25586495065054));
#57957=CARTESIAN_POINT('Ctrl Pts',(2.14073870754264,-1.,3.26077002641879));
#57958=CARTESIAN_POINT('Ctrl Pts',(2.14073870754264,1.,3.26077002641879));
#57959=CARTESIAN_POINT('Ctrl Pts',(2.1463680529566,-1.,3.26564388189759));
#57960=CARTESIAN_POINT('Ctrl Pts',(2.1463680529566,1.,3.26564388189759));
#57961=CARTESIAN_POINT('Ctrl Pts',(2.15205043199808,-1.,3.27050245897228));
#57962=CARTESIAN_POINT('Ctrl Pts',(2.15205043199808,1.,3.27050245897228));
#57963=CARTESIAN_POINT('Ctrl Pts',(2.15778690038347,-1.,3.27534954469187));
#57964=CARTESIAN_POINT('Ctrl Pts',(2.15778690038347,1.,3.27534954469187));
#57965=CARTESIAN_POINT('Ctrl Pts',(2.16357391934425,-1.,3.280181508414));
#57966=CARTESIAN_POINT('Ctrl Pts',(2.16357391934425,1.,3.280181508414));
#57967=CARTESIAN_POINT('Ctrl Pts',(2.16940517773455,-1.,3.28499019979724));
#57968=CARTESIAN_POINT('Ctrl Pts',(2.16940517773455,1.,3.28499019979724));
#57969=CARTESIAN_POINT('Ctrl Pts',(2.17527380048423,-1.,3.28976645712568));
#57970=CARTESIAN_POINT('Ctrl Pts',(2.17527380048423,1.,3.28976645712568));
#57971=CARTESIAN_POINT('Ctrl Pts',(2.18117455557065,-1.,3.2945036150049));
#57972=CARTESIAN_POINT('Ctrl Pts',(2.18117455557065,1.,3.2945036150049));
#57973=CARTESIAN_POINT('Ctrl Pts',(2.18710556500327,-1.,3.29920022557639));
#57974=CARTESIAN_POINT('Ctrl Pts',(2.18710556500327,1.,3.29920022557639));
#57975=CARTESIAN_POINT('Ctrl Pts',(2.19306710376111,-1.,3.30385816281831));
#57976=CARTESIAN_POINT('Ctrl Pts',(2.19306710376111,1.,3.30385816281831));
#57977=CARTESIAN_POINT('Ctrl Pts',(2.19906078949922,-1.,3.30848134694595));
#57978=CARTESIAN_POINT('Ctrl Pts',(2.19906078949922,1.,3.30848134694595));
#57979=CARTESIAN_POINT('Ctrl Pts',(2.20508863150607,-1.,3.31307424608949));
#57980=CARTESIAN_POINT('Ctrl Pts',(2.20508863150607,1.,3.31307424608949));
#57981=CARTESIAN_POINT('Ctrl Pts',(2.21115211847875,-1.,3.31764044024235));
#57982=CARTESIAN_POINT('Ctrl Pts',(2.21115211847875,1.,3.31764044024235));
#57983=CARTESIAN_POINT('Ctrl Pts',(2.21725135110898,-1.,3.32218125618968));
#57984=CARTESIAN_POINT('Ctrl Pts',(2.21725135110898,1.,3.32218125618968));
#57985=CARTESIAN_POINT('Ctrl Pts',(2.22338548312772,-1.,3.3266964672289));
#57986=CARTESIAN_POINT('Ctrl Pts',(2.22338548312772,1.,3.3266964672289));
#57987=CARTESIAN_POINT('Ctrl Pts',(2.22955308907233,-1.,3.33118487773611));
#57988=CARTESIAN_POINT('Ctrl Pts',(2.22955308907233,1.,3.33118487773611));
#57989=CARTESIAN_POINT('Ctrl Pts',(2.23575256328812,-1.,3.33564495756482));
#57990=CARTESIAN_POINT('Ctrl Pts',(2.23575256328812,1.,3.33564495756482));
#57991=CARTESIAN_POINT('Ctrl Pts',(2.24198249391422,-1.,3.34007543738025));
#57992=CARTESIAN_POINT('Ctrl Pts',(2.24198249391422,1.,3.34007543738025));
#57993=CARTESIAN_POINT('Ctrl Pts',(2.24824207678256,-1.,3.34447596770723));
#57994=CARTESIAN_POINT('Ctrl Pts',(2.24824207678256,1.,3.34447596770723));
#57995=CARTESIAN_POINT('Ctrl Pts',(2.25453097693483,-1.,3.34884690292285));
#57996=CARTESIAN_POINT('Ctrl Pts',(2.25453097693483,1.,3.34884690292285));
#57997=CARTESIAN_POINT('Ctrl Pts',(2.26084915222449,-1.,3.35318902552626));
#57998=CARTESIAN_POINT('Ctrl Pts',(2.26084915222449,1.,3.35318902552626));
#57999=CARTESIAN_POINT('Ctrl Pts',(2.26719668579909,-1.,3.35750328523061));
#58000=CARTESIAN_POINT('Ctrl Pts',(2.26719668579909,1.,3.35750328523061));
#58001=CARTESIAN_POINT('Ctrl Pts',(2.2735736262093,-1.,3.36179055004409));
#58002=CARTESIAN_POINT('Ctrl Pts',(2.2735736262093,1.,3.36179055004409));
#58003=CARTESIAN_POINT('Ctrl Pts',(2.27997979458037,-1.,3.36605130713076));
#58004=CARTESIAN_POINT('Ctrl Pts',(2.27997979458037,1.,3.36605130713076));
#58005=CARTESIAN_POINT('Ctrl Pts',(2.28641481081137,-1.,3.37028570206488));
#58006=CARTESIAN_POINT('Ctrl Pts',(2.28641481081137,1.,3.37028570206488));
#58007=CARTESIAN_POINT('Ctrl Pts',(2.29287818007393,-1.,3.37449367172826));
#58008=CARTESIAN_POINT('Ctrl Pts',(2.29287818007393,1.,3.37449367172826));
#58009=CARTESIAN_POINT('Ctrl Pts',(2.29936936127624,-1.,3.37867504959433));
#58010=CARTESIAN_POINT('Ctrl Pts',(2.29936936127624,1.,3.37867504959433));
#58011=CARTESIAN_POINT('Ctrl Pts',(2.30588783640343,-1.,3.3828296733661));
#58012=CARTESIAN_POINT('Ctrl Pts',(2.30588783640343,1.,3.3828296733661));
#58013=CARTESIAN_POINT('Ctrl Pts',(2.31243319489367,-1.,3.38695751492462));
#58014=CARTESIAN_POINT('Ctrl Pts',(2.31243319489367,1.,3.38695751492462));
#58015=CARTESIAN_POINT('Ctrl Pts',(2.31900513925424,-1.,3.39105869474822));
#58016=CARTESIAN_POINT('Ctrl Pts',(2.31900513925424,1.,3.39105869474822));
#58017=CARTESIAN_POINT('Ctrl Pts',(2.3256034390248,-1.,3.39513342019756));
#58018=CARTESIAN_POINT('Ctrl Pts',(2.3256034390248,1.,3.39513342019756));
#58019=CARTESIAN_POINT('Ctrl Pts',(2.33222789882489,-1.,3.39918194577956));
#58020=CARTESIAN_POINT('Ctrl Pts',(2.33222789882489,1.,3.39918194577956));
#58021=CARTESIAN_POINT('Ctrl Pts',(2.33887832342782,-1.,3.40320452776743));
#58022=CARTESIAN_POINT('Ctrl Pts',(2.33887832342782,1.,3.40320452776743));
#58023=CARTESIAN_POINT('Ctrl Pts',(2.34555447649188,-1.,3.40720137404297));
#58024=CARTESIAN_POINT('Ctrl Pts',(2.34555447649188,1.,3.40720137404297));
#58025=CARTESIAN_POINT('Ctrl Pts',(2.35225606824109,-1.,3.41117262314119));
#58026=CARTESIAN_POINT('Ctrl Pts',(2.35225606824109,1.,3.41117262314119));
#58027=CARTESIAN_POINT('Ctrl Pts',(2.35898278606946,-1.,3.41511836751469));
#58028=CARTESIAN_POINT('Ctrl Pts',(2.35898278606946,1.,3.41511836751469));
#58029=CARTESIAN_POINT('Ctrl Pts',(2.36573431470642,-1.,3.41903866635852));
#58030=CARTESIAN_POINT('Ctrl Pts',(2.36573431470642,1.,3.41903866635852));
#58031=CARTESIAN_POINT('Ctrl Pts',(2.37251035954292,-1.,3.42293356216511));
#58032=CARTESIAN_POINT('Ctrl Pts',(2.37251035954292,1.,3.42293356216511));
#58033=CARTESIAN_POINT('Ctrl Pts',(2.37931067028926,-1.,3.42680309754399));
#58034=CARTESIAN_POINT('Ctrl Pts',(2.37931067028926,1.,3.42680309754399));
#58035=CARTESIAN_POINT('Ctrl Pts',(2.38613505843552,-1.,3.4306473271292));
#58036=CARTESIAN_POINT('Ctrl Pts',(2.38613505843552,1.,3.4306473271292));
#58037=CARTESIAN_POINT('Ctrl Pts',(2.39298338804493,-1.,3.4344663067854));
#58038=CARTESIAN_POINT('Ctrl Pts',(2.39298338804493,1.,3.4344663067854));
#58039=CARTESIAN_POINT('Ctrl Pts',(2.39848113410292,-1.,3.43750133064416));
#58040=CARTESIAN_POINT('Ctrl Pts',(2.39848113410292,1.,3.43750133064416));
#58041=CARTESIAN_POINT('Ctrl Pts',(2.40261515589405,-1.,3.43976627484234));
#58042=CARTESIAN_POINT('Ctrl Pts',(2.40261515589405,1.,3.43976627484234));
#58043=CARTESIAN_POINT('Ctrl Pts',(2.4053759295909,-1.,3.44127120683039));
#58044=CARTESIAN_POINT('Ctrl Pts',(2.4053759295909,1.,3.44127120683039));
#58045=CARTESIAN_POINT('Ctrl Pts',(2.40675750623143,-1.,3.44202241512147));
#58046=CARTESIAN_POINT('Ctrl Pts',(2.40675750623143,1.,3.44202241512147));
#58047=CARTESIAN_POINT('',(2.03660101169714,1.,3.14877060440328));
#58048=CARTESIAN_POINT('Ctrl Pts',(2.03660101169714,-1.,3.14877060440327));
#58049=CARTESIAN_POINT('Ctrl Pts',(2.03660101169714,-0.666666666666667,
3.14877060440327));
#58050=CARTESIAN_POINT('Ctrl Pts',(2.03660101169714,-0.333333333333333,
3.14877060440327));
#58051=CARTESIAN_POINT('Ctrl Pts',(2.03660101169714,0.333333333333333,3.14877060440327));
#58052=CARTESIAN_POINT('Ctrl Pts',(2.03660101169714,0.666666666666667,3.14877060440327));
#58053=CARTESIAN_POINT('Ctrl Pts',(2.03660101169714,1.,3.14877060440327));
#58054=CARTESIAN_POINT('',(2.40675750623143,1.,3.44202241512147));
#58055=CARTESIAN_POINT('',(2.40675750623143,0.,3.44202241512147));
#58056=CARTESIAN_POINT('Ctrl Pts',(2.03660101169714,1.,3.14877060440328));
#58057=CARTESIAN_POINT('Ctrl Pts',(2.03659701539259,1.,3.14881939088124));
#58058=CARTESIAN_POINT('Ctrl Pts',(2.03663974554932,1.,3.1490119366901));
#58059=CARTESIAN_POINT('Ctrl Pts',(2.03693188810545,1.,3.14959882629805));
#58060=CARTESIAN_POINT('Ctrl Pts',(2.03783225495961,1.,3.15102344775328));
#58061=CARTESIAN_POINT('Ctrl Pts',(2.03984073791519,1.,3.15389991674792));
#58062=CARTESIAN_POINT('Ctrl Pts',(2.04297406404027,1.,3.15817983946367));
#58063=CARTESIAN_POINT('Ctrl Pts',(2.04693331247446,1.,3.16343165058912));
#58064=CARTESIAN_POINT('Ctrl Pts',(2.05151770247233,1.,3.16936341689527));
#58065=CARTESIAN_POINT('Ctrl Pts',(2.05650186773132,1.,3.17564906975371));
#58066=CARTESIAN_POINT('Ctrl Pts',(2.06166849827101,1.,3.18197692964614));
#58067=CARTESIAN_POINT('Ctrl Pts',(2.06684062744112,1.,3.18809755562368));
#58068=CARTESIAN_POINT('Ctrl Pts',(2.07192253497857,1.,3.19388465568252));
#58069=CARTESIAN_POINT('Ctrl Pts',(2.07690441870722,1.,3.19934132836019));
#58070=CARTESIAN_POINT('Ctrl Pts',(2.08182850370878,1.,3.2045481863073));
#58071=CARTESIAN_POINT('Ctrl Pts',(2.08676465517455,1.,3.20962575845463));
#58072=CARTESIAN_POINT('Ctrl Pts',(2.09178419460443,1.,3.21469429601654));
#58073=CARTESIAN_POINT('Ctrl Pts',(2.09692958434895,1.,3.21982707347009));
#58074=CARTESIAN_POINT('Ctrl Pts',(2.10220384298492,1.,3.22503437553434));
#58075=CARTESIAN_POINT('Ctrl Pts',(2.10758699642451,1.,3.23028945793289));
#58076=CARTESIAN_POINT('Ctrl Pts',(2.11304604021773,1.,3.23554444767099));
#58077=CARTESIAN_POINT('Ctrl Pts',(2.11854673326979,1.,3.24074905517293));
#58078=CARTESIAN_POINT('Ctrl Pts',(2.12406646410962,1.,3.24587102613376));
#58079=CARTESIAN_POINT('Ctrl Pts',(2.12960028396832,1.,3.25090574494028));
#58080=CARTESIAN_POINT('Ctrl Pts',(2.13515375878803,1.,3.25586495065054));
#58081=CARTESIAN_POINT('Ctrl Pts',(2.14073870754264,1.,3.26077002641879));
#58082=CARTESIAN_POINT('Ctrl Pts',(2.1463680529566,1.,3.26564388189759));
#58083=CARTESIAN_POINT('Ctrl Pts',(2.15205043199808,1.,3.27050245897228));
#58084=CARTESIAN_POINT('Ctrl Pts',(2.15778690038347,1.,3.27534954469187));
#58085=CARTESIAN_POINT('Ctrl Pts',(2.16357391934425,1.,3.280181508414));
#58086=CARTESIAN_POINT('Ctrl Pts',(2.16940517773455,1.,3.28499019979724));
#58087=CARTESIAN_POINT('Ctrl Pts',(2.17527380048423,1.,3.28976645712568));
#58088=CARTESIAN_POINT('Ctrl Pts',(2.18117455557065,1.,3.2945036150049));
#58089=CARTESIAN_POINT('Ctrl Pts',(2.18710556500327,1.,3.29920022557639));
#58090=CARTESIAN_POINT('Ctrl Pts',(2.19306710376111,1.,3.30385816281831));
#58091=CARTESIAN_POINT('Ctrl Pts',(2.19906078949922,1.,3.30848134694595));
#58092=CARTESIAN_POINT('Ctrl Pts',(2.20508863150607,1.,3.31307424608949));
#58093=CARTESIAN_POINT('Ctrl Pts',(2.21115211847875,1.,3.31764044024235));
#58094=CARTESIAN_POINT('Ctrl Pts',(2.21725135110898,1.,3.32218125618968));
#58095=CARTESIAN_POINT('Ctrl Pts',(2.22338548312772,1.,3.3266964672289));
#58096=CARTESIAN_POINT('Ctrl Pts',(2.22955308907233,1.,3.33118487773611));
#58097=CARTESIAN_POINT('Ctrl Pts',(2.23575256328812,1.,3.33564495756482));
#58098=CARTESIAN_POINT('Ctrl Pts',(2.24198249391422,1.,3.34007543738025));
#58099=CARTESIAN_POINT('Ctrl Pts',(2.24824207678256,1.,3.34447596770723));
#58100=CARTESIAN_POINT('Ctrl Pts',(2.25453097693483,1.,3.34884690292285));
#58101=CARTESIAN_POINT('Ctrl Pts',(2.26084915222449,1.,3.35318902552626));
#58102=CARTESIAN_POINT('Ctrl Pts',(2.26719668579909,1.,3.35750328523061));
#58103=CARTESIAN_POINT('Ctrl Pts',(2.2735736262093,1.,3.36179055004409));
#58104=CARTESIAN_POINT('Ctrl Pts',(2.27997979458037,1.,3.36605130713076));
#58105=CARTESIAN_POINT('Ctrl Pts',(2.28641481081137,1.,3.37028570206488));
#58106=CARTESIAN_POINT('Ctrl Pts',(2.29287818007393,1.,3.37449367172826));
#58107=CARTESIAN_POINT('Ctrl Pts',(2.29936936127624,1.,3.37867504959433));
#58108=CARTESIAN_POINT('Ctrl Pts',(2.30588783640343,1.,3.3828296733661));
#58109=CARTESIAN_POINT('Ctrl Pts',(2.31243319489367,1.,3.38695751492462));
#58110=CARTESIAN_POINT('Ctrl Pts',(2.31900513925424,1.,3.39105869474822));
#58111=CARTESIAN_POINT('Ctrl Pts',(2.3256034390248,1.,3.39513342019756));
#58112=CARTESIAN_POINT('Ctrl Pts',(2.33222789882489,1.,3.39918194577956));
#58113=CARTESIAN_POINT('Ctrl Pts',(2.33887832342782,1.,3.40320452776743));
#58114=CARTESIAN_POINT('Ctrl Pts',(2.34555447649188,1.,3.40720137404297));
#58115=CARTESIAN_POINT('Ctrl Pts',(2.35225606824109,1.,3.41117262314119));
#58116=CARTESIAN_POINT('Ctrl Pts',(2.35898278606946,1.,3.41511836751469));
#58117=CARTESIAN_POINT('Ctrl Pts',(2.36573431470642,1.,3.41903866635852));
#58118=CARTESIAN_POINT('Ctrl Pts',(2.37251035954292,1.,3.42293356216511));
#58119=CARTESIAN_POINT('Ctrl Pts',(2.37931067028926,1.,3.42680309754399));
#58120=CARTESIAN_POINT('Ctrl Pts',(2.38613505843552,1.,3.4306473271292));
#58121=CARTESIAN_POINT('Ctrl Pts',(2.39298338804493,1.,3.4344663067854));
#58122=CARTESIAN_POINT('Ctrl Pts',(2.39848113410292,1.,3.43750133064416));
#58123=CARTESIAN_POINT('Ctrl Pts',(2.40261515589405,1.,3.43976627484234));
#58124=CARTESIAN_POINT('Ctrl Pts',(2.4053759295909,1.,3.44127120683039));
#58125=CARTESIAN_POINT('Ctrl Pts',(2.40675750623143,1.,3.44202241512147));
#58126=CARTESIAN_POINT('Origin',(2.40675750623143,0.,3.44202241512147));
#58127=CARTESIAN_POINT('',(2.52982887637028,1.,3.35260583073571));
#58128=CARTESIAN_POINT('Origin',(0.,0.,0.));
#58129=CARTESIAN_POINT('',(1.88097764062697,1.,3.24413672884812));
#58130=CARTESIAN_POINT('Origin',(0.,1.,0.));
#58131=CARTESIAN_POINT('Ctrl Pts',(1.88097764062697,1.,3.24413672884812));
#58132=CARTESIAN_POINT('Ctrl Pts',(1.88097764062697,0.666666666666667,3.24413672884812));
#58133=CARTESIAN_POINT('Ctrl Pts',(1.88097764062697,0.333333333333333,3.24413672884812));
#58134=CARTESIAN_POINT('Ctrl Pts',(1.88097764062697,-0.333333333333333,
3.24413672884812));
#58135=CARTESIAN_POINT('Ctrl Pts',(1.88097764062697,-0.666666666666667,
3.24413672884812));
#58136=CARTESIAN_POINT('Ctrl Pts',(1.88097764062697,-1.,3.24413672884812));
#58137=CARTESIAN_POINT('Ctrl Pts',(1.97421938526992,-1.,3.70708211654725));
#58138=CARTESIAN_POINT('Ctrl Pts',(1.97421938526992,1.,3.70708211654725));
#58139=CARTESIAN_POINT('Ctrl Pts',(1.97417727645308,-1.,3.70551008132332));
#58140=CARTESIAN_POINT('Ctrl Pts',(1.97417727645308,1.,3.70551008132332));
#58141=CARTESIAN_POINT('Ctrl Pts',(1.97408973726715,-1.,3.70236698912904));
#58142=CARTESIAN_POINT('Ctrl Pts',(1.97408973726715,1.,3.70236698912904));
#58143=CARTESIAN_POINT('Ctrl Pts',(1.97394846383216,-1.,3.6976552856004));
#58144=CARTESIAN_POINT('Ctrl Pts',(1.97394846383216,1.,3.6976552856004));
#58145=CARTESIAN_POINT('Ctrl Pts',(1.97374016225483,-1.,3.69137888599902));
#58146=CARTESIAN_POINT('Ctrl Pts',(1.97374016225483,1.,3.69137888599902));
#58147=CARTESIAN_POINT('Ctrl Pts',(1.97344650304519,-1.,3.68354319915092));
#58148=CARTESIAN_POINT('Ctrl Pts',(1.97344650304519,1.,3.68354319915092));
#58149=CARTESIAN_POINT('Ctrl Pts',(1.97311947678516,-1.,3.67571738107084));
#58150=CARTESIAN_POINT('Ctrl Pts',(1.97311947678516,1.,3.67571738107084));
#58151=CARTESIAN_POINT('Ctrl Pts',(1.97275897198678,-1.,3.66790152752075));
#58152=CARTESIAN_POINT('Ctrl Pts',(1.97275897198678,1.,3.66790152752075));
#58153=CARTESIAN_POINT('Ctrl Pts',(1.9723648543905,-1.,3.6600957816636));
#58154=CARTESIAN_POINT('Ctrl Pts',(1.9723648543905,1.,3.6600957816636));
#58155=CARTESIAN_POINT('Ctrl Pts',(1.97193697240239,-1.,3.652300347166));
#58156=CARTESIAN_POINT('Ctrl Pts',(1.97193697240239,1.,3.652300347166));
#58157=CARTESIAN_POINT('Ctrl Pts',(1.97147515441164,-1.,3.64451546723514));
#58158=CARTESIAN_POINT('Ctrl Pts',(1.97147515441164,1.,3.64451546723514));
#58159=CARTESIAN_POINT('Ctrl Pts',(1.97097920454464,-1.,3.63674139590412));
#58160=CARTESIAN_POINT('Ctrl Pts',(1.97097920454464,1.,3.63674139590412));
#58161=CARTESIAN_POINT('Ctrl Pts',(1.97044889850463,-1.,3.62897836973293));
#58162=CARTESIAN_POINT('Ctrl Pts',(1.97044889850463,1.,3.62897836973293));
#58163=CARTESIAN_POINT('Ctrl Pts',(1.96988398129978,-1.,3.62122658401893));
#58164=CARTESIAN_POINT('Ctrl Pts',(1.96988398129978,1.,3.62122658401893));
#58165=CARTESIAN_POINT('Ctrl Pts',(1.96928416040877,-1.,3.61348615496704));
#58166=CARTESIAN_POINT('Ctrl Pts',(1.96928416040877,1.,3.61348615496704));
#58167=CARTESIAN_POINT('Ctrl Pts',(1.9686491188594,-1.,3.60575714017989));
#58168=CARTESIAN_POINT('Ctrl Pts',(1.9686491188594,1.,3.60575714017989));
#58169=CARTESIAN_POINT('Ctrl Pts',(1.96797854118369,-1.,3.59803959819938));
#58170=CARTESIAN_POINT('Ctrl Pts',(1.96797854118369,1.,3.59803959819938));
#58171=CARTESIAN_POINT('Ctrl Pts',(1.96727213799544,-1.,3.59033364022801));
#58172=CARTESIAN_POINT('Ctrl Pts',(1.96727213799544,1.,3.59033364022801));
#58173=CARTESIAN_POINT('Ctrl Pts',(1.96652966688911,-1.,3.58263947663829));
#58174=CARTESIAN_POINT('Ctrl Pts',(1.96652966688911,1.,3.58263947663829));
#58175=CARTESIAN_POINT('Ctrl Pts',(1.96575096652789,-1.,3.57495748600959));
#58176=CARTESIAN_POINT('Ctrl Pts',(1.96575096652789,1.,3.57495748600959));
#58177=CARTESIAN_POINT('Ctrl Pts',(1.96493594634567,-1.,3.56728820357791));
#58178=CARTESIAN_POINT('Ctrl Pts',(1.96493594634567,1.,3.56728820357791));
#58179=CARTESIAN_POINT('Ctrl Pts',(1.96408450906812,-1.,3.55963218706096));
#58180=CARTESIAN_POINT('Ctrl Pts',(1.96408450906812,1.,3.55963218706096));
#58181=CARTESIAN_POINT('Ctrl Pts',(1.96319648628644,-1.,3.55198990600886));
#58182=CARTESIAN_POINT('Ctrl Pts',(1.96319648628644,1.,3.55198990600886));
#58183=CARTESIAN_POINT('Ctrl Pts',(1.96227157573067,-1.,3.54436163300443));
#58184=CARTESIAN_POINT('Ctrl Pts',(1.96227157573067,1.,3.54436163300443));
#58185=CARTESIAN_POINT('Ctrl Pts',(1.96130926212689,-1.,3.53674730625813));
#58186=CARTESIAN_POINT('Ctrl Pts',(1.96130926212689,1.,3.53674730625813));
#58187=CARTESIAN_POINT('Ctrl Pts',(1.96030879411566,-1.,3.52914648844351));
#58188=CARTESIAN_POINT('Ctrl Pts',(1.96030879411566,1.,3.52914648844351));
#58189=CARTESIAN_POINT('Ctrl Pts',(1.95926936324461,-1.,3.52155867431486));
#58190=CARTESIAN_POINT('Ctrl Pts',(1.95926936324461,1.,3.52155867431486));
#58191=CARTESIAN_POINT('Ctrl Pts',(1.95819025316779,-1.,3.51398354617794));
#58192=CARTESIAN_POINT('Ctrl Pts',(1.95819025316779,1.,3.51398354617794));
#58193=CARTESIAN_POINT('Ctrl Pts',(1.95707099606511,-1.,3.50642124159909));
#58194=CARTESIAN_POINT('Ctrl Pts',(1.95707099606511,1.,3.50642124159909));
#58195=CARTESIAN_POINT('Ctrl Pts',(1.95591153823661,-1.,3.49887263575583));
#58196=CARTESIAN_POINT('Ctrl Pts',(1.95591153823661,1.,3.49887263575583));
#58197=CARTESIAN_POINT('Ctrl Pts',(1.95471236969643,-1.,3.49133956289133));
#58198=CARTESIAN_POINT('Ctrl Pts',(1.95471236969643,1.,3.49133956289133));
#58199=CARTESIAN_POINT('Ctrl Pts',(1.95347412486308,-1.,3.48382414832634));
#58200=CARTESIAN_POINT('Ctrl Pts',(1.95347412486308,1.,3.48382414832634));
#58201=CARTESIAN_POINT('Ctrl Pts',(1.95219722189876,-1.,3.47632820495921));
#58202=CARTESIAN_POINT('Ctrl Pts',(1.95219722189876,1.,3.47632820495921));
#58203=CARTESIAN_POINT('Ctrl Pts',(1.95088147859876,-1.,3.46885258974191));
#58204=CARTESIAN_POINT('Ctrl Pts',(1.95088147859876,1.,3.46885258974191));
#58205=CARTESIAN_POINT('Ctrl Pts',(1.94952575850197,-1.,3.46139661060962));
#58206=CARTESIAN_POINT('Ctrl Pts',(1.94952575850197,1.,3.46139661060962));
#58207=CARTESIAN_POINT('Ctrl Pts',(1.94812754766524,-1.,3.45395731584051));
#58208=CARTESIAN_POINT('Ctrl Pts',(1.94812754766524,1.,3.45395731584051));
#58209=CARTESIAN_POINT('Ctrl Pts',(1.94668377715329,-1.,3.44653088665681));
#58210=CARTESIAN_POINT('Ctrl Pts',(1.94668377715329,1.,3.44653088665681));
#58211=CARTESIAN_POINT('Ctrl Pts',(1.94519168842879,-1.,3.43911410197687));
#58212=CARTESIAN_POINT('Ctrl Pts',(1.94519168842879,1.,3.43911410197687));
#58213=CARTESIAN_POINT('Ctrl Pts',(1.94364973660284,-1.,3.43170586602434));
#58214=CARTESIAN_POINT('Ctrl Pts',(1.94364973660284,1.,3.43170586602434));
#58215=CARTESIAN_POINT('Ctrl Pts',(1.94205835913696,-1.,3.42430850941503));
#58216=CARTESIAN_POINT('Ctrl Pts',(1.94205835913696,1.,3.42430850941503));
#58217=CARTESIAN_POINT('Ctrl Pts',(1.94042111965246,-1.,3.41692971994096));
#58218=CARTESIAN_POINT('Ctrl Pts',(1.94042111965246,1.,3.41692971994096));
#58219=CARTESIAN_POINT('Ctrl Pts',(1.93874306008143,-1.,3.40957978266642));
#58220=CARTESIAN_POINT('Ctrl Pts',(1.93874306008143,1.,3.40957978266642));
#58221=CARTESIAN_POINT('Ctrl Pts',(1.93702857723098,-1.,3.40226802104109));
#58222=CARTESIAN_POINT('Ctrl Pts',(1.93702857723098,1.,3.40226802104109));
#58223=CARTESIAN_POINT('Ctrl Pts',(1.93527929945985,-1.,3.39499923640795));
#58224=CARTESIAN_POINT('Ctrl Pts',(1.93527929945985,1.,3.39499923640795));
#58225=CARTESIAN_POINT('Ctrl Pts',(1.93349233176788,-1.,3.38777076883256));
#58226=CARTESIAN_POINT('Ctrl Pts',(1.93349233176788,1.,3.38777076883256));
#58227=CARTESIAN_POINT('Ctrl Pts',(1.93165739093276,-1.,3.3805676852555));
#58228=CARTESIAN_POINT('Ctrl Pts',(1.93165739093276,1.,3.3805676852555));
#58229=CARTESIAN_POINT('Ctrl Pts',(1.92975993109877,-1.,3.37336807068043));
#58230=CARTESIAN_POINT('Ctrl Pts',(1.92975993109877,1.,3.37336807068043));
#58231=CARTESIAN_POINT('Ctrl Pts',(1.92778626543786,-1.,3.36615168657567));
#58232=CARTESIAN_POINT('Ctrl Pts',(1.92778626543786,1.,3.36615168657567));
#58233=CARTESIAN_POINT('Ctrl Pts',(1.92572846125756,-1.,3.35890824422965));
#58234=CARTESIAN_POINT('Ctrl Pts',(1.92572846125756,1.,3.35890824422965));
#58235=CARTESIAN_POINT('Ctrl Pts',(1.92358838440528,-1.,3.35164424847223));
#58236=CARTESIAN_POINT('Ctrl Pts',(1.92358838440528,1.,3.35164424847223));
#58237=CARTESIAN_POINT('Ctrl Pts',(1.92138450828404,-1.,3.34439448941961));
#58238=CARTESIAN_POINT('Ctrl Pts',(1.92138450828404,1.,3.34439448941961));
#58239=CARTESIAN_POINT('Ctrl Pts',(1.9191460961021,-1.,3.33721230710012));
#58240=CARTESIAN_POINT('Ctrl Pts',(1.9191460961021,1.,3.33721230710012));
#58241=CARTESIAN_POINT('Ctrl Pts',(1.91690081930331,-1.,3.33014884257873));
#58242=CARTESIAN_POINT('Ctrl Pts',(1.91690081930331,1.,3.33014884257873));
#58243=CARTESIAN_POINT('Ctrl Pts',(1.91466343916627,-1.,3.32323403454535));
#58244=CARTESIAN_POINT('Ctrl Pts',(1.91466343916627,1.,3.32323403454535));
#58245=CARTESIAN_POINT('Ctrl Pts',(1.91242616234442,-1.,3.31646052426364));
#58246=CARTESIAN_POINT('Ctrl Pts',(1.91242616234442,1.,3.31646052426364));
#58247=CARTESIAN_POINT('Ctrl Pts',(1.91014297830446,-1.,3.30975721158596));
#58248=CARTESIAN_POINT('Ctrl Pts',(1.91014297830446,1.,3.30975721158596));
#58249=CARTESIAN_POINT('Ctrl Pts',(1.90773912171341,-1.,3.30300595568195));
#58250=CARTESIAN_POINT('Ctrl Pts',(1.90773912171341,1.,3.30300595568195));
#58251=CARTESIAN_POINT('Ctrl Pts',(1.90513891864087,-1.,3.29608978722113));
#58252=CARTESIAN_POINT('Ctrl Pts',(1.90513891864087,1.,3.29608978722113));
#58253=CARTESIAN_POINT('Ctrl Pts',(1.90228971247527,-1.,3.2889344860029));
#58254=CARTESIAN_POINT('Ctrl Pts',(1.90228971247527,1.,3.2889344860029));
#58255=CARTESIAN_POINT('Ctrl Pts',(1.89918429230462,-1.,3.28154737912352));
#58256=CARTESIAN_POINT('Ctrl Pts',(1.89918429230462,1.,3.28154737912352));
#58257=CARTESIAN_POINT('Ctrl Pts',(1.89589172903793,-1.,3.27407108933139));
#58258=CARTESIAN_POINT('Ctrl Pts',(1.89589172903793,1.,3.27407108933139));
#58259=CARTESIAN_POINT('Ctrl Pts',(1.89255393500965,-1.,3.26677653888676));
#58260=CARTESIAN_POINT('Ctrl Pts',(1.89255393500965,1.,3.26677653888676));
#58261=CARTESIAN_POINT('Ctrl Pts',(1.88934996203698,-1.,3.25999885193947));
#58262=CARTESIAN_POINT('Ctrl Pts',(1.88934996203698,1.,3.25999885193947));
#58263=CARTESIAN_POINT('Ctrl Pts',(1.88646802523466,-1.,3.25408686339463));
#58264=CARTESIAN_POINT('Ctrl Pts',(1.88646802523466,1.,3.25408686339463));
#58265=CARTESIAN_POINT('Ctrl Pts',(1.88407708646357,-1.,3.24935200511918));
#58266=CARTESIAN_POINT('Ctrl Pts',(1.88407708646357,1.,3.24935200511918));
#58267=CARTESIAN_POINT('Ctrl Pts',(1.88229202582941,-1.,3.24600543790443));
#58268=CARTESIAN_POINT('Ctrl Pts',(1.88229202582941,1.,3.24600543790443));
#58269=CARTESIAN_POINT('Ctrl Pts',(1.88139187908074,-1.,3.24451807186481));
#58270=CARTESIAN_POINT('Ctrl Pts',(1.88139187908074,1.,3.24451807186481));
#58271=CARTESIAN_POINT('Ctrl Pts',(1.88102201872555,-1.,3.24408699284121));
#58272=CARTESIAN_POINT('Ctrl Pts',(1.88102201872555,1.,3.24408699284121));
#58273=CARTESIAN_POINT('Ctrl Pts',(1.88091100680349,-1.,3.24410359189609));
#58274=CARTESIAN_POINT('Ctrl Pts',(1.88091100680349,1.,3.24410359189609));
#58275=CARTESIAN_POINT('Ctrl Pts',(1.8808893942881,-1.,3.24418789321065));
#58276=CARTESIAN_POINT('Ctrl Pts',(1.8808893942881,1.,3.24418789321065));
#58277=CARTESIAN_POINT('',(1.97421938526992,1.,3.70708211654725));
#58278=CARTESIAN_POINT('Ctrl Pts',(1.97421938526992,1.,3.70708211654725));
#58279=CARTESIAN_POINT('Ctrl Pts',(1.97417727645308,1.,3.70551008132332));
#58280=CARTESIAN_POINT('Ctrl Pts',(1.97408973726715,1.,3.70236698912904));
#58281=CARTESIAN_POINT('Ctrl Pts',(1.97394846383216,1.,3.6976552856004));
#58282=CARTESIAN_POINT('Ctrl Pts',(1.97374016225483,1.,3.69137888599902));
#58283=CARTESIAN_POINT('Ctrl Pts',(1.97344650304519,1.,3.68354319915092));
#58284=CARTESIAN_POINT('Ctrl Pts',(1.97311947678516,1.,3.67571738107084));
#58285=CARTESIAN_POINT('Ctrl Pts',(1.97275897198678,1.,3.66790152752075));
#58286=CARTESIAN_POINT('Ctrl Pts',(1.9723648543905,1.,3.6600957816636));
#58287=CARTESIAN_POINT('Ctrl Pts',(1.97193697240239,1.,3.652300347166));
#58288=CARTESIAN_POINT('Ctrl Pts',(1.97147515441164,1.,3.64451546723514));
#58289=CARTESIAN_POINT('Ctrl Pts',(1.97097920454464,1.,3.63674139590412));
#58290=CARTESIAN_POINT('Ctrl Pts',(1.97044889850463,1.,3.62897836973293));
#58291=CARTESIAN_POINT('Ctrl Pts',(1.96988398129978,1.,3.62122658401893));
#58292=CARTESIAN_POINT('Ctrl Pts',(1.96928416040877,1.,3.61348615496704));
#58293=CARTESIAN_POINT('Ctrl Pts',(1.9686491188594,1.,3.60575714017989));
#58294=CARTESIAN_POINT('Ctrl Pts',(1.96797854118369,1.,3.59803959819938));
#58295=CARTESIAN_POINT('Ctrl Pts',(1.96727213799544,1.,3.59033364022801));
#58296=CARTESIAN_POINT('Ctrl Pts',(1.96652966688911,1.,3.58263947663829));
#58297=CARTESIAN_POINT('Ctrl Pts',(1.96575096652789,1.,3.57495748600959));
#58298=CARTESIAN_POINT('Ctrl Pts',(1.96493594634567,1.,3.56728820357791));
#58299=CARTESIAN_POINT('Ctrl Pts',(1.96408450906812,1.,3.55963218706096));
#58300=CARTESIAN_POINT('Ctrl Pts',(1.96319648628644,1.,3.55198990600886));
#58301=CARTESIAN_POINT('Ctrl Pts',(1.96227157573067,1.,3.54436163300443));
#58302=CARTESIAN_POINT('Ctrl Pts',(1.96130926212689,1.,3.53674730625813));
#58303=CARTESIAN_POINT('Ctrl Pts',(1.96030879411566,1.,3.52914648844351));
#58304=CARTESIAN_POINT('Ctrl Pts',(1.95926936324461,1.,3.52155867431486));
#58305=CARTESIAN_POINT('Ctrl Pts',(1.95819025316779,1.,3.51398354617794));
#58306=CARTESIAN_POINT('Ctrl Pts',(1.95707099606511,1.,3.50642124159909));
#58307=CARTESIAN_POINT('Ctrl Pts',(1.95591153823661,1.,3.49887263575583));
#58308=CARTESIAN_POINT('Ctrl Pts',(1.95471236969643,1.,3.49133956289133));
#58309=CARTESIAN_POINT('Ctrl Pts',(1.95347412486308,1.,3.48382414832634));
#58310=CARTESIAN_POINT('Ctrl Pts',(1.95219722189876,1.,3.47632820495921));
#58311=CARTESIAN_POINT('Ctrl Pts',(1.95088147859876,1.,3.46885258974191));
#58312=CARTESIAN_POINT('Ctrl Pts',(1.94952575850197,1.,3.46139661060962));
#58313=CARTESIAN_POINT('Ctrl Pts',(1.94812754766524,1.,3.45395731584051));
#58314=CARTESIAN_POINT('Ctrl Pts',(1.94668377715329,1.,3.44653088665681));
#58315=CARTESIAN_POINT('Ctrl Pts',(1.94519168842879,1.,3.43911410197687));
#58316=CARTESIAN_POINT('Ctrl Pts',(1.94364973660284,1.,3.43170586602434));
#58317=CARTESIAN_POINT('Ctrl Pts',(1.94205835913696,1.,3.42430850941503));
#58318=CARTESIAN_POINT('Ctrl Pts',(1.94042111965246,1.,3.41692971994096));
#58319=CARTESIAN_POINT('Ctrl Pts',(1.93874306008143,1.,3.40957978266642));
#58320=CARTESIAN_POINT('Ctrl Pts',(1.93702857723098,1.,3.40226802104109));
#58321=CARTESIAN_POINT('Ctrl Pts',(1.93527929945985,1.,3.39499923640795));
#58322=CARTESIAN_POINT('Ctrl Pts',(1.93349233176788,1.,3.38777076883256));
#58323=CARTESIAN_POINT('Ctrl Pts',(1.93165739093276,1.,3.3805676852555));
#58324=CARTESIAN_POINT('Ctrl Pts',(1.92975993109877,1.,3.37336807068043));
#58325=CARTESIAN_POINT('Ctrl Pts',(1.92778626543786,1.,3.36615168657567));
#58326=CARTESIAN_POINT('Ctrl Pts',(1.92572846125756,1.,3.35890824422965));
#58327=CARTESIAN_POINT('Ctrl Pts',(1.92358838440528,1.,3.35164424847223));
#58328=CARTESIAN_POINT('Ctrl Pts',(1.92138450828404,1.,3.34439448941961));
#58329=CARTESIAN_POINT('Ctrl Pts',(1.9191460961021,1.,3.33721230710012));
#58330=CARTESIAN_POINT('Ctrl Pts',(1.91690081930331,1.,3.33014884257873));
#58331=CARTESIAN_POINT('Ctrl Pts',(1.91466343916627,1.,3.32323403454535));
#58332=CARTESIAN_POINT('Ctrl Pts',(1.91242616234442,1.,3.31646052426364));
#58333=CARTESIAN_POINT('Ctrl Pts',(1.91014297830446,1.,3.30975721158596));
#58334=CARTESIAN_POINT('Ctrl Pts',(1.90773912171341,1.,3.30300595568195));
#58335=CARTESIAN_POINT('Ctrl Pts',(1.90513891864087,1.,3.29608978722113));
#58336=CARTESIAN_POINT('Ctrl Pts',(1.90228971247527,1.,3.2889344860029));
#58337=CARTESIAN_POINT('Ctrl Pts',(1.89918429230462,1.,3.28154737912352));
#58338=CARTESIAN_POINT('Ctrl Pts',(1.89589172903793,1.,3.27407108933139));
#58339=CARTESIAN_POINT('Ctrl Pts',(1.89255393500965,1.,3.26677653888676));
#58340=CARTESIAN_POINT('Ctrl Pts',(1.88934996203698,1.,3.25999885193947));
#58341=CARTESIAN_POINT('Ctrl Pts',(1.88646802523466,1.,3.25408686339463));
#58342=CARTESIAN_POINT('Ctrl Pts',(1.88407708646357,1.,3.24935200511918));
#58343=CARTESIAN_POINT('Ctrl Pts',(1.88242596600454,1.,3.2462565441079));
#58344=CARTESIAN_POINT('Ctrl Pts',(1.88156537699203,1.,3.24480754676064));
#58345=CARTESIAN_POINT('Ctrl Pts',(1.88117508446775,1.,3.24428080353022));
#58346=CARTESIAN_POINT('Ctrl Pts',(1.8810229239812,1.,3.24415531671284));
#58347=CARTESIAN_POINT('Ctrl Pts',(1.88097764062697,1.,3.24413672884812));
#58348=CARTESIAN_POINT('',(1.97421938526992,0.,3.70708211654725));
#58349=CARTESIAN_POINT('Ctrl Pts',(1.519044091397,-1.,3.42855728381368));
#58350=CARTESIAN_POINT('Ctrl Pts',(1.519044091397,1.,3.42855728381368));
#58351=CARTESIAN_POINT('Ctrl Pts',(1.51896318668366,-1.,3.42852521763778));
#58352=CARTESIAN_POINT('Ctrl Pts',(1.51896318668366,1.,3.42852521763778));
#58353=CARTESIAN_POINT('Ctrl Pts',(1.51888450659652,-1.,3.42860527149177));
#58354=CARTESIAN_POINT('Ctrl Pts',(1.51888450659652,1.,3.42860527149177));
#58355=CARTESIAN_POINT('Ctrl Pts',(1.51901585839109,-1.,3.42915787669893));
#58356=CARTESIAN_POINT('Ctrl Pts',(1.51901585839109,1.,3.42915787669893));
#58357=CARTESIAN_POINT('Ctrl Pts',(1.51969006980999,-1.,3.43076036253837));
#58358=CARTESIAN_POINT('Ctrl Pts',(1.51969006980999,1.,3.43076036253837));
#58359=CARTESIAN_POINT('Ctrl Pts',(1.52134826724292,-1.,3.43417156977893));
#58360=CARTESIAN_POINT('Ctrl Pts',(1.52134826724292,1.,3.43417156977893));
#58361=CARTESIAN_POINT('Ctrl Pts',(1.5237734895035,-1.,3.4388889597401));
#58362=CARTESIAN_POINT('Ctrl Pts',(1.5237734895035,1.,3.4388889597401));
#58363=CARTESIAN_POINT('Ctrl Pts',(1.52686242875556,-1.,3.44469547526647));
#58364=CARTESIAN_POINT('Ctrl Pts',(1.52686242875556,1.,3.44469547526647));
#58365=CARTESIAN_POINT('Ctrl Pts',(1.53046244461635,-1.,3.45127136828305));
#58366=CARTESIAN_POINT('Ctrl Pts',(1.53046244461635,1.,3.45127136828305));
#58367=CARTESIAN_POINT('Ctrl Pts',(1.53440195378792,-1.,3.45825932955032));
#58368=CARTESIAN_POINT('Ctrl Pts',(1.53440195378792,1.,3.45825932955032));
#58369=CARTESIAN_POINT('Ctrl Pts',(1.53851507915502,-1.,3.46531752207153));
#58370=CARTESIAN_POINT('Ctrl Pts',(1.53851507915502,1.,3.46531752207153));
#58371=CARTESIAN_POINT('Ctrl Pts',(1.54266605398187,-1.,3.47217189224653));
#58372=CARTESIAN_POINT('Ctrl Pts',(1.54266605398187,1.,3.47217189224653));
#58373=CARTESIAN_POINT('Ctrl Pts',(1.54678009290276,-1.,3.47868272898751));
#58374=CARTESIAN_POINT('Ctrl Pts',(1.54678009290276,1.,3.47868272898751));
#58375=CARTESIAN_POINT('Ctrl Pts',(1.55084702970452,-1.,3.48485155928567));
#58376=CARTESIAN_POINT('Ctrl Pts',(1.55084702970452,1.,3.48485155928567));
#58377=CARTESIAN_POINT('Ctrl Pts',(1.55489595901116,-1.,3.4907646087742));
#58378=CARTESIAN_POINT('Ctrl Pts',(1.55489595901116,1.,3.4907646087742));
#58379=CARTESIAN_POINT('Ctrl Pts',(1.55897703097874,-1.,3.49655185179655));
#58380=CARTESIAN_POINT('Ctrl Pts',(1.55897703097874,1.,3.49655185179655));
#58381=CARTESIAN_POINT('Ctrl Pts',(1.56314187758675,-1.,3.50234321621578));
#58382=CARTESIAN_POINT('Ctrl Pts',(1.56314187758675,1.,3.50234321621578));
#58383=CARTESIAN_POINT('Ctrl Pts',(1.56742097575012,-1.,3.50821771695363));
#58384=CARTESIAN_POINT('Ctrl Pts',(1.56742097575012,1.,3.50821771695363));
#58385=CARTESIAN_POINT('Ctrl Pts',(1.57181569799743,-1.,3.51418598431665));
#58386=CARTESIAN_POINT('Ctrl Pts',(1.57181569799743,1.,3.51418598431665));
#58387=CARTESIAN_POINT('Ctrl Pts',(1.57631049988158,-1.,3.52021847865912));
#58388=CARTESIAN_POINT('Ctrl Pts',(1.57631049988158,1.,3.52021847865912));
#58389=CARTESIAN_POINT('Ctrl Pts',(1.58088027227848,-1.,3.52626275334881));
#58390=CARTESIAN_POINT('Ctrl Pts',(1.58088027227848,1.,3.52626275334881));
#58391=CARTESIAN_POINT('Ctrl Pts',(1.58549906268088,-1.,3.5322637814708));
#58392=CARTESIAN_POINT('Ctrl Pts',(1.58549906268088,1.,3.5322637814708));
#58393=CARTESIAN_POINT('Ctrl Pts',(1.59014958368739,-1.,3.53818616861077));
#58394=CARTESIAN_POINT('Ctrl Pts',(1.59014958368739,1.,3.53818616861077));
#58395=CARTESIAN_POINT('Ctrl Pts',(1.59482766949766,-1.,3.54402458182337));
#58396=CARTESIAN_POINT('Ctrl Pts',(1.59482766949766,1.,3.54402458182337));
#58397=CARTESIAN_POINT('Ctrl Pts',(1.59953698113457,-1.,3.54979148634454));
#58398=CARTESIAN_POINT('Ctrl Pts',(1.59953698113457,1.,3.54979148634454));
#58399=CARTESIAN_POINT('Ctrl Pts',(1.60428584699853,-1.,3.55550985096129));
#58400=CARTESIAN_POINT('Ctrl Pts',(1.60428584699853,1.,3.55550985096129));
#58401=CARTESIAN_POINT('Ctrl Pts',(1.60908344685457,-1.,3.5612043248298));
#58402=CARTESIAN_POINT('Ctrl Pts',(1.60908344685457,1.,3.5612043248298));
#58403=CARTESIAN_POINT('Ctrl Pts',(1.61393581747514,-1.,3.56689200468387));
#58404=CARTESIAN_POINT('Ctrl Pts',(1.61393581747514,1.,3.56689200468387));
#58405=CARTESIAN_POINT('Ctrl Pts',(1.61884340915404,-1.,3.57257679609806));
#58406=CARTESIAN_POINT('Ctrl Pts',(1.61884340915404,1.,3.57257679609806));
#58407=CARTESIAN_POINT('Ctrl Pts',(1.62380329464844,-1.,3.5782545595439));
#58408=CARTESIAN_POINT('Ctrl Pts',(1.62380329464844,1.,3.5782545595439));
#58409=CARTESIAN_POINT('Ctrl Pts',(1.62881051550745,-1.,3.58391625774343));
#58410=CARTESIAN_POINT('Ctrl Pts',(1.62881051550745,1.,3.58391625774343));
#58411=CARTESIAN_POINT('Ctrl Pts',(1.6338597145126,-1.,3.58955176627879));
#58412=CARTESIAN_POINT('Ctrl Pts',(1.6338597145126,1.,3.58955176627879));
#58413=CARTESIAN_POINT('Ctrl Pts',(1.63894676675352,-1.,3.59515368334893));
#58414=CARTESIAN_POINT('Ctrl Pts',(1.63894676675352,1.,3.59515368334893));
#58415=CARTESIAN_POINT('Ctrl Pts',(1.64407004385582,-1.,3.60072028513845));
#58416=CARTESIAN_POINT('Ctrl Pts',(1.64407004385582,1.,3.60072028513845));
#58417=CARTESIAN_POINT('Ctrl Pts',(1.64922952425832,-1.,3.60625346556992));
#58418=CARTESIAN_POINT('Ctrl Pts',(1.64922952425832,1.,3.60625346556992));
#58419=CARTESIAN_POINT('Ctrl Pts',(1.65442619244325,-1.,3.61175734965127));
#58420=CARTESIAN_POINT('Ctrl Pts',(1.65442619244325,1.,3.61175734965127));
#58421=CARTESIAN_POINT('Ctrl Pts',(1.65966133399186,-1.,3.61723666482456));
#58422=CARTESIAN_POINT('Ctrl Pts',(1.65966133399186,1.,3.61723666482456));
#58423=CARTESIAN_POINT('Ctrl Pts',(1.66493585923855,-1.,3.62269517989109));
#58424=CARTESIAN_POINT('Ctrl Pts',(1.66493585923855,1.,3.62269517989109));
#58425=CARTESIAN_POINT('Ctrl Pts',(1.67024966008044,-1.,3.62813422105271));
#58426=CARTESIAN_POINT('Ctrl Pts',(1.67024966008044,1.,3.62813422105271));
#58427=CARTESIAN_POINT('Ctrl Pts',(1.67560193613156,-1.,3.63355343201232));
#58428=CARTESIAN_POINT('Ctrl Pts',(1.67560193613156,1.,3.63355343201232));
#58429=CARTESIAN_POINT('Ctrl Pts',(1.68099146651586,-1.,3.63895140887462));
#58430=CARTESIAN_POINT('Ctrl Pts',(1.68099146651586,1.,3.63895140887462));
#58431=CARTESIAN_POINT('Ctrl Pts',(1.68641690471457,-1.,3.64432638915203));
#58432=CARTESIAN_POINT('Ctrl Pts',(1.68641690471457,1.,3.64432638915203));
#58433=CARTESIAN_POINT('Ctrl Pts',(1.69187705481689,-1.,3.64967689827371));
#58434=CARTESIAN_POINT('Ctrl Pts',(1.69187705481689,1.,3.64967689827371));
#58435=CARTESIAN_POINT('Ctrl Pts',(1.69737117722534,-1.,3.65500246526749));
#58436=CARTESIAN_POINT('Ctrl Pts',(1.69737117722534,1.,3.65500246526749));
#58437=CARTESIAN_POINT('Ctrl Pts',(1.70289888566873,-1.,3.66030338774847));
#58438=CARTESIAN_POINT('Ctrl Pts',(1.70289888566873,1.,3.66030338774847));
#58439=CARTESIAN_POINT('Ctrl Pts',(1.70846001610956,-1.,3.66558043198876));
#58440=CARTESIAN_POINT('Ctrl Pts',(1.70846001610956,1.,3.66558043198876));
#58441=CARTESIAN_POINT('Ctrl Pts',(1.71405450210383,-1.,3.67083454901611));
#58442=CARTESIAN_POINT('Ctrl Pts',(1.71405450210383,1.,3.67083454901611));
#58443=CARTESIAN_POINT('Ctrl Pts',(1.71968225581808,-1.,3.67606660374709));
#58444=CARTESIAN_POINT('Ctrl Pts',(1.71968225581808,1.,3.67606660374709));
#58445=CARTESIAN_POINT('Ctrl Pts',(1.72534302437056,-1.,3.68127704936579));
#58446=CARTESIAN_POINT('Ctrl Pts',(1.72534302437056,1.,3.68127704936579));
#58447=CARTESIAN_POINT('Ctrl Pts',(1.73103640956717,-1.,3.68646597019332));
#58448=CARTESIAN_POINT('Ctrl Pts',(1.73103640956717,1.,3.68646597019332));
#58449=CARTESIAN_POINT('Ctrl Pts',(1.73676193254557,-1.,3.69163322648036));
#58450=CARTESIAN_POINT('Ctrl Pts',(1.73676193254557,1.,3.69163322648036));
#58451=CARTESIAN_POINT('Ctrl Pts',(1.74251908492617,-1.,3.69677856910517));
#58452=CARTESIAN_POINT('Ctrl Pts',(1.74251908492617,1.,3.69677856910517));
#58453=CARTESIAN_POINT('Ctrl Pts',(1.74830738046057,-1.,3.7019017567335));
#58454=CARTESIAN_POINT('Ctrl Pts',(1.74830738046057,1.,3.7019017567335));
#58455=CARTESIAN_POINT('Ctrl Pts',(1.75412641804042,-1.,3.70700269736659));
#58456=CARTESIAN_POINT('Ctrl Pts',(1.75412641804042,1.,3.70700269736659));
#58457=CARTESIAN_POINT('Ctrl Pts',(1.75997588498865,-1.,3.71208146346136));
#58458=CARTESIAN_POINT('Ctrl Pts',(1.75997588498865,1.,3.71208146346136));
#58459=CARTESIAN_POINT('Ctrl Pts',(1.76585552124394,-1.,3.71713822377359));
#58460=CARTESIAN_POINT('Ctrl Pts',(1.76585552124394,1.,3.71713822377359));
#58461=CARTESIAN_POINT('Ctrl Pts',(1.77176509401761,-1.,3.72217319911254));
#58462=CARTESIAN_POINT('Ctrl Pts',(1.77176509401761,1.,3.72217319911254));
#58463=CARTESIAN_POINT('Ctrl Pts',(1.77770437039658,-1.,3.72718661205609));
#58464=CARTESIAN_POINT('Ctrl Pts',(1.77770437039658,1.,3.72718661205609));
#58465=CARTESIAN_POINT('Ctrl Pts',(1.78367308442901,-1.,3.7321786309547));
#58466=CARTESIAN_POINT('Ctrl Pts',(1.78367308442901,1.,3.7321786309547));
#58467=CARTESIAN_POINT('Ctrl Pts',(1.78967092823491,-1.,3.73714934730681));
#58468=CARTESIAN_POINT('Ctrl Pts',(1.78967092823491,1.,3.73714934730681));
#58469=CARTESIAN_POINT('Ctrl Pts',(1.79569757859422,-1.,3.74209880352445));
#58470=CARTESIAN_POINT('Ctrl Pts',(1.79569757859422,1.,3.74209880352445));
#58471=CARTESIAN_POINT('Ctrl Pts',(1.8017527148577,-1.,3.74702700875467));
#58472=CARTESIAN_POINT('Ctrl Pts',(1.8017527148577,1.,3.74702700875467));
#58473=CARTESIAN_POINT('Ctrl Pts',(1.80783603939617,-1.,3.75193395887977));
#58474=CARTESIAN_POINT('Ctrl Pts',(1.80783603939617,1.,3.75193395887977));
#58475=CARTESIAN_POINT('Ctrl Pts',(1.8139472983358,-1.,3.75681965683071));
#58476=CARTESIAN_POINT('Ctrl Pts',(1.8139472983358,1.,3.75681965683071));
#58477=CARTESIAN_POINT('Ctrl Pts',(1.82008629694091,-1.,3.76168412707948));
#58478=CARTESIAN_POINT('Ctrl Pts',(1.82008629694091,1.,3.76168412707948));
#58479=CARTESIAN_POINT('Ctrl Pts',(1.82625289220915,-1.,3.76652740353775));
#58480=CARTESIAN_POINT('Ctrl Pts',(1.82625289220915,1.,3.76652740353775));
#58481=CARTESIAN_POINT('Ctrl Pts',(1.83120816955645,-1.,3.77038509817999));
#58482=CARTESIAN_POINT('Ctrl Pts',(1.83120816955645,1.,3.77038509817999));
#58483=CARTESIAN_POINT('Ctrl Pts',(1.83493697934534,-1.,3.77326886064398));
#58484=CARTESIAN_POINT('Ctrl Pts',(1.83493697934534,1.,3.77326886064398));
#58485=CARTESIAN_POINT('Ctrl Pts',(1.83742834010626,-1.,3.77518714457833));
#58486=CARTESIAN_POINT('Ctrl Pts',(1.83742834010626,1.,3.77518714457833));
#58487=CARTESIAN_POINT('Ctrl Pts',(1.8386753923786,-1.,3.77614523045147));
#58488=CARTESIAN_POINT('Ctrl Pts',(1.8386753923786,1.,3.77614523045147));
#58489=CARTESIAN_POINT('',(1.5189508286633,1.,3.42859860294306));
#58490=CARTESIAN_POINT('Ctrl Pts',(1.5189508286633,-1.,3.42859860294306));
#58491=CARTESIAN_POINT('Ctrl Pts',(1.5189508286633,-0.666666666666667,3.42859860294306));
#58492=CARTESIAN_POINT('Ctrl Pts',(1.5189508286633,-0.333333333333333,3.42859860294306));
#58493=CARTESIAN_POINT('Ctrl Pts',(1.5189508286633,0.333333333333333,3.42859860294306));
#58494=CARTESIAN_POINT('Ctrl Pts',(1.5189508286633,0.666666666666667,3.42859860294306));
#58495=CARTESIAN_POINT('Ctrl Pts',(1.5189508286633,1.,3.42859860294306));
#58496=CARTESIAN_POINT('',(1.8386753923786,1.,3.77614523045147));
#58497=CARTESIAN_POINT('',(1.8386753923786,0.,3.77614523045147));
#58498=CARTESIAN_POINT('Ctrl Pts',(1.5189508286633,1.,3.42859860294306));
#58499=CARTESIAN_POINT('Ctrl Pts',(1.51893924967331,1.,3.42864616361875));
#58500=CARTESIAN_POINT('Ctrl Pts',(1.5189513329503,1.,3.42884302333841));
#58501=CARTESIAN_POINT('Ctrl Pts',(1.51914806898491,1.,3.42946838852587));
#58502=CARTESIAN_POINT('Ctrl Pts',(1.5198144909338,1.,3.43101631893414));
#58503=CARTESIAN_POINT('Ctrl Pts',(1.52134826724292,1.,3.43417156977893));
#58504=CARTESIAN_POINT('Ctrl Pts',(1.5237734895035,1.,3.4388889597401));
#58505=CARTESIAN_POINT('Ctrl Pts',(1.52686242875556,1.,3.44469547526647));
#58506=CARTESIAN_POINT('Ctrl Pts',(1.53046244461635,1.,3.45127136828305));
#58507=CARTESIAN_POINT('Ctrl Pts',(1.53440195378792,1.,3.45825932955032));
#58508=CARTESIAN_POINT('Ctrl Pts',(1.53851507915502,1.,3.46531752207153));
#58509=CARTESIAN_POINT('Ctrl Pts',(1.54266605398187,1.,3.47217189224653));
#58510=CARTESIAN_POINT('Ctrl Pts',(1.54678009290276,1.,3.47868272898751));
#58511=CARTESIAN_POINT('Ctrl Pts',(1.55084702970452,1.,3.48485155928567));
#58512=CARTESIAN_POINT('Ctrl Pts',(1.55489595901116,1.,3.4907646087742));
#58513=CARTESIAN_POINT('Ctrl Pts',(1.55897703097874,1.,3.49655185179655));
#58514=CARTESIAN_POINT('Ctrl Pts',(1.56314187758675,1.,3.50234321621578));
#58515=CARTESIAN_POINT('Ctrl Pts',(1.56742097575012,1.,3.50821771695363));
#58516=CARTESIAN_POINT('Ctrl Pts',(1.57181569799743,1.,3.51418598431665));
#58517=CARTESIAN_POINT('Ctrl Pts',(1.57631049988158,1.,3.52021847865912));
#58518=CARTESIAN_POINT('Ctrl Pts',(1.58088027227848,1.,3.52626275334881));
#58519=CARTESIAN_POINT('Ctrl Pts',(1.58549906268088,1.,3.5322637814708));
#58520=CARTESIAN_POINT('Ctrl Pts',(1.59014958368739,1.,3.53818616861077));
#58521=CARTESIAN_POINT('Ctrl Pts',(1.59482766949766,1.,3.54402458182337));
#58522=CARTESIAN_POINT('Ctrl Pts',(1.59953698113457,1.,3.54979148634454));
#58523=CARTESIAN_POINT('Ctrl Pts',(1.60428584699853,1.,3.55550985096129));
#58524=CARTESIAN_POINT('Ctrl Pts',(1.60908344685457,1.,3.5612043248298));
#58525=CARTESIAN_POINT('Ctrl Pts',(1.61393581747514,1.,3.56689200468387));
#58526=CARTESIAN_POINT('Ctrl Pts',(1.61884340915404,1.,3.57257679609806));
#58527=CARTESIAN_POINT('Ctrl Pts',(1.62380329464844,1.,3.5782545595439));
#58528=CARTESIAN_POINT('Ctrl Pts',(1.62881051550745,1.,3.58391625774343));
#58529=CARTESIAN_POINT('Ctrl Pts',(1.6338597145126,1.,3.58955176627879));
#58530=CARTESIAN_POINT('Ctrl Pts',(1.63894676675352,1.,3.59515368334893));
#58531=CARTESIAN_POINT('Ctrl Pts',(1.64407004385582,1.,3.60072028513845));
#58532=CARTESIAN_POINT('Ctrl Pts',(1.64922952425832,1.,3.60625346556992));
#58533=CARTESIAN_POINT('Ctrl Pts',(1.65442619244325,1.,3.61175734965127));
#58534=CARTESIAN_POINT('Ctrl Pts',(1.65966133399186,1.,3.61723666482456));
#58535=CARTESIAN_POINT('Ctrl Pts',(1.66493585923855,1.,3.62269517989109));
#58536=CARTESIAN_POINT('Ctrl Pts',(1.67024966008044,1.,3.62813422105271));
#58537=CARTESIAN_POINT('Ctrl Pts',(1.67560193613156,1.,3.63355343201232));
#58538=CARTESIAN_POINT('Ctrl Pts',(1.68099146651586,1.,3.63895140887462));
#58539=CARTESIAN_POINT('Ctrl Pts',(1.68641690471457,1.,3.64432638915203));
#58540=CARTESIAN_POINT('Ctrl Pts',(1.69187705481689,1.,3.64967689827371));
#58541=CARTESIAN_POINT('Ctrl Pts',(1.69737117722534,1.,3.65500246526749));
#58542=CARTESIAN_POINT('Ctrl Pts',(1.70289888566873,1.,3.66030338774847));
#58543=CARTESIAN_POINT('Ctrl Pts',(1.70846001610956,1.,3.66558043198876));
#58544=CARTESIAN_POINT('Ctrl Pts',(1.71405450210383,1.,3.67083454901611));
#58545=CARTESIAN_POINT('Ctrl Pts',(1.71968225581808,1.,3.67606660374709));
#58546=CARTESIAN_POINT('Ctrl Pts',(1.72534302437056,1.,3.68127704936579));
#58547=CARTESIAN_POINT('Ctrl Pts',(1.73103640956717,1.,3.68646597019332));
#58548=CARTESIAN_POINT('Ctrl Pts',(1.73676193254557,1.,3.69163322648036));
#58549=CARTESIAN_POINT('Ctrl Pts',(1.74251908492617,1.,3.69677856910517));
#58550=CARTESIAN_POINT('Ctrl Pts',(1.74830738046057,1.,3.7019017567335));
#58551=CARTESIAN_POINT('Ctrl Pts',(1.75412641804042,1.,3.70700269736659));
#58552=CARTESIAN_POINT('Ctrl Pts',(1.75997588498865,1.,3.71208146346136));
#58553=CARTESIAN_POINT('Ctrl Pts',(1.76585552124394,1.,3.71713822377359));
#58554=CARTESIAN_POINT('Ctrl Pts',(1.77176509401761,1.,3.72217319911254));
#58555=CARTESIAN_POINT('Ctrl Pts',(1.77770437039658,1.,3.72718661205609));
#58556=CARTESIAN_POINT('Ctrl Pts',(1.78367308442901,1.,3.7321786309547));
#58557=CARTESIAN_POINT('Ctrl Pts',(1.78967092823491,1.,3.73714934730681));
#58558=CARTESIAN_POINT('Ctrl Pts',(1.79569757859422,1.,3.74209880352445));
#58559=CARTESIAN_POINT('Ctrl Pts',(1.8017527148577,1.,3.74702700875467));
#58560=CARTESIAN_POINT('Ctrl Pts',(1.80783603939617,1.,3.75193395887977));
#58561=CARTESIAN_POINT('Ctrl Pts',(1.8139472983358,1.,3.75681965683071));
#58562=CARTESIAN_POINT('Ctrl Pts',(1.82008629694091,1.,3.76168412707948));
#58563=CARTESIAN_POINT('Ctrl Pts',(1.82625289220915,1.,3.76652740353775));
#58564=CARTESIAN_POINT('Ctrl Pts',(1.83120816955645,1.,3.77038509817999));
#58565=CARTESIAN_POINT('Ctrl Pts',(1.83493697934534,1.,3.77326886064398));
#58566=CARTESIAN_POINT('Ctrl Pts',(1.83742834010626,1.,3.77518714457833));
#58567=CARTESIAN_POINT('Ctrl Pts',(1.8386753923786,1.,3.77614523045147));
#58568=CARTESIAN_POINT('Origin',(1.8386753923786,0.,3.77614523045147));
#58569=CARTESIAN_POINT('',(1.97421938526992,1.,3.70708211654725));
#58570=CARTESIAN_POINT('Origin',(0.,0.,0.));
#58571=CARTESIAN_POINT('',(1.35032489087269,1.,3.49844575334386));
#58572=CARTESIAN_POINT('Origin',(0.,1.,0.));
#58573=CARTESIAN_POINT('Ctrl Pts',(1.35032489087269,1.,3.49844575334386));
#58574=CARTESIAN_POINT('Ctrl Pts',(1.35032489087269,0.666666666666667,3.49844575334386));
#58575=CARTESIAN_POINT('Ctrl Pts',(1.35032489087269,0.333333333333333,3.49844575334386));
#58576=CARTESIAN_POINT('Ctrl Pts',(1.35032489087269,-0.333333333333333,
3.49844575334386));
#58577=CARTESIAN_POINT('Ctrl Pts',(1.35032489087269,-0.666666666666667,
3.49844575334386));
#58578=CARTESIAN_POINT('Ctrl Pts',(1.35032489087269,-1.,3.49844575334386));
#58579=CARTESIAN_POINT('Ctrl Pts',(1.36999806084572,-1.,3.97027773754922));
#58580=CARTESIAN_POINT('Ctrl Pts',(1.36999806084572,1.,3.97027773754922));
#58581=CARTESIAN_POINT('Ctrl Pts',(1.37020239094758,-1.,3.9687184694173));
#58582=CARTESIAN_POINT('Ctrl Pts',(1.37020239094758,1.,3.9687184694173));
#58583=CARTESIAN_POINT('Ctrl Pts',(1.37060761746027,-1.,3.96560037975788));
#58584=CARTESIAN_POINT('Ctrl Pts',(1.37060761746027,1.,3.96560037975788));
#58585=CARTESIAN_POINT('Ctrl Pts',(1.37120515615663,-1.,3.96092458508407));
#58586=CARTESIAN_POINT('Ctrl Pts',(1.37120515615663,1.,3.96092458508407));
#58587=CARTESIAN_POINT('Ctrl Pts',(1.37198126433139,-1.,3.95469287283105));
#58588=CARTESIAN_POINT('Ctrl Pts',(1.37198126433139,1.,3.95469287283105));
#58589=CARTESIAN_POINT('Ctrl Pts',(1.37291699203423,-1.,3.94690771786926));
#58590=CARTESIAN_POINT('Ctrl Pts',(1.37291699203423,1.,3.94690771786926));
#58591=CARTESIAN_POINT('Ctrl Pts',(1.37381821967499,-1.,3.93912709041791));
#58592=CARTESIAN_POINT('Ctrl Pts',(1.37381821967499,1.,3.93912709041791));
#58593=CARTESIAN_POINT('Ctrl Pts',(1.37468482215784,-1.,3.93135106761941));
#58594=CARTESIAN_POINT('Ctrl Pts',(1.37468482215784,1.,3.93135106761941));
#58595=CARTESIAN_POINT('Ctrl Pts',(1.37551664448057,-1.,3.92357976987132));
#58596=CARTESIAN_POINT('Ctrl Pts',(1.37551664448057,1.,3.92357976987132));
#58597=CARTESIAN_POINT('Ctrl Pts',(1.37631350505516,-1.,3.91581337461825));
#58598=CARTESIAN_POINT('Ctrl Pts',(1.37631350505516,1.,3.91581337461825));
#58599=CARTESIAN_POINT('Ctrl Pts',(1.3770751963376,-1.,3.90805209522729));
#58600=CARTESIAN_POINT('Ctrl Pts',(1.3770751963376,1.,3.90805209522729));
#58601=CARTESIAN_POINT('Ctrl Pts',(1.3778014851263,-1.,3.90029615196255));
#58602=CARTESIAN_POINT('Ctrl Pts',(1.3778014851263,1.,3.90029615196255));
#58603=CARTESIAN_POINT('Ctrl Pts',(1.37849211287981,-1.,3.89254574338385));
#58604=CARTESIAN_POINT('Ctrl Pts',(1.37849211287981,1.,3.89254574338385));
#58605=CARTESIAN_POINT('Ctrl Pts',(1.37914679719446,-1.,3.88480102249461));
#58606=CARTESIAN_POINT('Ctrl Pts',(1.37914679719446,1.,3.88480102249461));
#58607=CARTESIAN_POINT('Ctrl Pts',(1.37976523097187,-1.,3.87706205830865));
#58608=CARTESIAN_POINT('Ctrl Pts',(1.37976523097187,1.,3.87706205830865));
#58609=CARTESIAN_POINT('Ctrl Pts',(1.38034709213129,-1.,3.86932885813403));
#58610=CARTESIAN_POINT('Ctrl Pts',(1.38034709213129,1.,3.86932885813403));
#58611=CARTESIAN_POINT('Ctrl Pts',(1.38089205993067,-1.,3.86160143044187));
#58612=CARTESIAN_POINT('Ctrl Pts',(1.38089205993067,1.,3.86160143044187));
#58613=CARTESIAN_POINT('Ctrl Pts',(1.38139983115075,-1.,3.85387983979557));
#58614=CARTESIAN_POINT('Ctrl Pts',(1.38139983115075,1.,3.85387983979557));
#58615=CARTESIAN_POINT('Ctrl Pts',(1.38187013346089,-1.,3.84616425605705));
#58616=CARTESIAN_POINT('Ctrl Pts',(1.38187013346089,1.,3.84616425605705));
#58617=CARTESIAN_POINT('Ctrl Pts',(1.38230274828774,-1.,3.83845502790609));
#58618=CARTESIAN_POINT('Ctrl Pts',(1.38230274828774,1.,3.83845502790609));
#58619=CARTESIAN_POINT('Ctrl Pts',(1.38269750245086,-1.,3.83075266982138));
#58620=CARTESIAN_POINT('Ctrl Pts',(1.38269750245086,1.,3.83075266982138));
#58621=CARTESIAN_POINT('Ctrl Pts',(1.38305421262724,-1.,3.82305771743715));
#58622=CARTESIAN_POINT('Ctrl Pts',(1.38305421262724,1.,3.82305771743715));
#58623=CARTESIAN_POINT('Ctrl Pts',(1.38337263902766,-1.,3.81537060817765));
#58624=CARTESIAN_POINT('Ctrl Pts',(1.38337263902766,1.,3.81537060817765));
#58625=CARTESIAN_POINT('Ctrl Pts',(1.38365244046226,-1.,3.80769156398429));
#58626=CARTESIAN_POINT('Ctrl Pts',(1.38365244046226,1.,3.80769156398429));
#58627=CARTESIAN_POINT('Ctrl Pts',(1.38389311766701,-1.,3.80002044322169));
#58628=CARTESIAN_POINT('Ctrl Pts',(1.38389311766701,1.,3.80002044322169));
#58629=CARTESIAN_POINT('Ctrl Pts',(1.38409399694588,-1.,3.79235669640907));
#58630=CARTESIAN_POINT('Ctrl Pts',(1.38409399694588,1.,3.79235669640907));
#58631=CARTESIAN_POINT('Ctrl Pts',(1.38425435883773,-1.,3.78469969805134));
#58632=CARTESIAN_POINT('Ctrl Pts',(1.38425435883773,1.,3.78469969805134));
#58633=CARTESIAN_POINT('Ctrl Pts',(1.38437354551435,-1.,3.77704902230441));
#58634=CARTESIAN_POINT('Ctrl Pts',(1.38437354551435,1.,3.77704902230441));
#58635=CARTESIAN_POINT('Ctrl Pts',(1.38445107339517,-1.,3.76940473185775));
#58636=CARTESIAN_POINT('Ctrl Pts',(1.38445107339517,1.,3.76940473185775));
#58637=CARTESIAN_POINT('Ctrl Pts',(1.38448675253343,-1.,3.76176768271347));
#58638=CARTESIAN_POINT('Ctrl Pts',(1.38448675253343,1.,3.76176768271347));
#58639=CARTESIAN_POINT('Ctrl Pts',(1.38448077997155,-1.,3.75413976318727));
#58640=CARTESIAN_POINT('Ctrl Pts',(1.38448077997155,1.,3.75413976318727));
#58641=CARTESIAN_POINT('Ctrl Pts',(1.38443344984389,-1.,3.7465231716786));
#58642=CARTESIAN_POINT('Ctrl Pts',(1.38443344984389,1.,3.7465231716786));
#58643=CARTESIAN_POINT('Ctrl Pts',(1.38434489156456,-1.,3.73891976418099));
#58644=CARTESIAN_POINT('Ctrl Pts',(1.38434489156456,1.,3.73891976418099));
#58645=CARTESIAN_POINT('Ctrl Pts',(1.38421479111531,-1.,3.73133035859283));
#58646=CARTESIAN_POINT('Ctrl Pts',(1.38421479111531,1.,3.73133035859283));
#58647=CARTESIAN_POINT('Ctrl Pts',(1.3840421342895,-1.,3.72375409358805));
#58648=CARTESIAN_POINT('Ctrl Pts',(1.3840421342895,1.,3.72375409358805));
#58649=CARTESIAN_POINT('Ctrl Pts',(1.38382489984585,-1.,3.7161876605181));
#58650=CARTESIAN_POINT('Ctrl Pts',(1.38382489984585,1.,3.7161876605181));
#58651=CARTESIAN_POINT('Ctrl Pts',(1.38356065402122,-1.,3.70862680753343));
#58652=CARTESIAN_POINT('Ctrl Pts',(1.38356065402122,1.,3.70862680753343));
#58653=CARTESIAN_POINT('Ctrl Pts',(1.38324717612862,-1.,3.70106792167894));
#58654=CARTESIAN_POINT('Ctrl Pts',(1.38324717612862,1.,3.70106792167894));
#58655=CARTESIAN_POINT('Ctrl Pts',(1.38288311171649,-1.,3.69350967899523));
#58656=CARTESIAN_POINT('Ctrl Pts',(1.38288311171649,1.,3.69350967899523));
#58657=CARTESIAN_POINT('Ctrl Pts',(1.38246852827185,-1.,3.68595444983844));
#58658=CARTESIAN_POINT('Ctrl Pts',(1.38246852827185,1.,3.68595444983844));
#58659=CARTESIAN_POINT('Ctrl Pts',(1.38200574290626,-1.,3.6784103848243));
#58660=CARTESIAN_POINT('Ctrl Pts',(1.38200574290626,1.,3.6784103848243));
#58661=CARTESIAN_POINT('Ctrl Pts',(1.38149812653876,-1.,3.67088843112282));
#58662=CARTESIAN_POINT('Ctrl Pts',(1.38149812653876,1.,3.67088843112282));
#58663=CARTESIAN_POINT('Ctrl Pts',(1.38094856333558,-1.,3.66339848520874));
#58664=CARTESIAN_POINT('Ctrl Pts',(1.38094856333558,1.,3.66339848520874));
#58665=CARTESIAN_POINT('Ctrl Pts',(1.38035791051215,-1.,3.65594554404396));
#58666=CARTESIAN_POINT('Ctrl Pts',(1.38035791051215,1.,3.65594554404396));
#58667=CARTESIAN_POINT('Ctrl Pts',(1.37972372481598,-1.,3.64852652756444));
#58668=CARTESIAN_POINT('Ctrl Pts',(1.37972372481598,1.,3.64852652756444));
#58669=CARTESIAN_POINT('Ctrl Pts',(1.37903818567347,-1.,3.64112507791112));
#58670=CARTESIAN_POINT('Ctrl Pts',(1.37903818567347,1.,3.64112507791112));
#58671=CARTESIAN_POINT('Ctrl Pts',(1.37829035457324,-1.,3.63371727442448));
#58672=CARTESIAN_POINT('Ctrl Pts',(1.37829035457324,1.,3.63371727442448));
#58673=CARTESIAN_POINT('Ctrl Pts',(1.37746987919868,-1.,3.62628098665112));
#58674=CARTESIAN_POINT('Ctrl Pts',(1.37746987919868,1.,3.62628098665112));
#58675=CARTESIAN_POINT('Ctrl Pts',(1.37657053403102,-1.,3.61880481160408));
#58676=CARTESIAN_POINT('Ctrl Pts',(1.37657053403102,1.,3.61880481160408));
#58677=CARTESIAN_POINT('Ctrl Pts',(1.37559314436641,-1.,3.61129546591082));
#58678=CARTESIAN_POINT('Ctrl Pts',(1.37559314436641,1.,3.61129546591082));
#58679=CARTESIAN_POINT('Ctrl Pts',(1.37455051379642,-1.,3.60379020124038));
#58680=CARTESIAN_POINT('Ctrl Pts',(1.37455051379642,1.,3.60379020124038));
#58681=CARTESIAN_POINT('Ctrl Pts',(1.37346320103184,-1.,3.59634627869117));
#58682=CARTESIAN_POINT('Ctrl Pts',(1.37346320103184,1.,3.59634627869117));
#58683=CARTESIAN_POINT('Ctrl Pts',(1.37235053661,-1.,3.5890185384643));
#58684=CARTESIAN_POINT('Ctrl Pts',(1.37235053661,1.,3.5890185384643));
#58685=CARTESIAN_POINT('Ctrl Pts',(1.37122241663073,-1.,3.58183885982745));
#58686=CARTESIAN_POINT('Ctrl Pts',(1.37122241663073,1.,3.58183885982745));
#58687=CARTESIAN_POINT('Ctrl Pts',(1.37007229485646,-1.,3.57479875549453));
#58688=CARTESIAN_POINT('Ctrl Pts',(1.37007229485646,1.,3.57479875549453));
#58689=CARTESIAN_POINT('Ctrl Pts',(1.36886584973349,-1.,3.56782080304554));
#58690=CARTESIAN_POINT('Ctrl Pts',(1.36886584973349,1.,3.56782080304554));
#58691=CARTESIAN_POINT('Ctrl Pts',(1.36754771771174,-1.,3.56077662028492));
#58692=CARTESIAN_POINT('Ctrl Pts',(1.36754771771174,1.,3.56077662028492));
#58693=CARTESIAN_POINT('Ctrl Pts',(1.36606145456711,-1.,3.55353883995793));
#58694=CARTESIAN_POINT('Ctrl Pts',(1.36606145456711,1.,3.55353883995793));
#58695=CARTESIAN_POINT('Ctrl Pts',(1.36436666257567,-1.,3.54602591832893));
#58696=CARTESIAN_POINT('Ctrl Pts',(1.36436666257567,1.,3.54602591832893));
#58697=CARTESIAN_POINT('Ctrl Pts',(1.36245507339334,-1.,3.53824396425032));
#58698=CARTESIAN_POINT('Ctrl Pts',(1.36245507339334,1.,3.53824396425032));
#58699=CARTESIAN_POINT('Ctrl Pts',(1.36037259643827,-1.,3.53034464961849));
#58700=CARTESIAN_POINT('Ctrl Pts',(1.36037259643827,1.,3.53034464961849));
#58701=CARTESIAN_POINT('Ctrl Pts',(1.35821701528975,-1.,3.52261776117121));
#58702=CARTESIAN_POINT('Ctrl Pts',(1.35821701528975,1.,3.52261776117121));
#58703=CARTESIAN_POINT('Ctrl Pts',(1.35611275237288,-1.,3.51542230699919));
#58704=CARTESIAN_POINT('Ctrl Pts',(1.35611275237288,1.,3.51542230699919));
#58705=CARTESIAN_POINT('Ctrl Pts',(1.35419113576022,-1.,3.50913227060177));
#58706=CARTESIAN_POINT('Ctrl Pts',(1.35419113576022,1.,3.50913227060177));
#58707=CARTESIAN_POINT('Ctrl Pts',(1.3525703284343,-1.,3.50408168106113));
#58708=CARTESIAN_POINT('Ctrl Pts',(1.3525703284343,1.,3.50408168106113));
#58709=CARTESIAN_POINT('Ctrl Pts',(1.35133076331065,-1.,3.50049707063673));
#58710=CARTESIAN_POINT('Ctrl Pts',(1.35133076331065,1.,3.50049707063673));
#58711=CARTESIAN_POINT('Ctrl Pts',(1.35067437417289,-1.,3.49888720256612));
#58712=CARTESIAN_POINT('Ctrl Pts',(1.35067437417289,1.,3.49888720256612));
#58713=CARTESIAN_POINT('Ctrl Pts',(1.35037650302887,-1.,3.49840357193384));
#58714=CARTESIAN_POINT('Ctrl Pts',(1.35037650302887,1.,3.49840357193384));
#58715=CARTESIAN_POINT('Ctrl Pts',(1.35026426118351,-1.,3.49840260053616));
#58716=CARTESIAN_POINT('Ctrl Pts',(1.35026426118351,1.,3.49840260053616));
#58717=CARTESIAN_POINT('Ctrl Pts',(1.35022972712301,-1.,3.49848248301936));
#58718=CARTESIAN_POINT('Ctrl Pts',(1.35022972712301,1.,3.49848248301936));
#58719=CARTESIAN_POINT('',(1.36999806084572,1.,3.97027773754922));
#58720=CARTESIAN_POINT('Ctrl Pts',(1.36999806084572,1.,3.97027773754922));
#58721=CARTESIAN_POINT('Ctrl Pts',(1.37020239094758,1.,3.9687184694173));
#58722=CARTESIAN_POINT('Ctrl Pts',(1.37060761746027,1.,3.96560037975788));
#58723=CARTESIAN_POINT('Ctrl Pts',(1.37120515615663,1.,3.96092458508407));
#58724=CARTESIAN_POINT('Ctrl Pts',(1.37198126433139,1.,3.95469287283105));
#58725=CARTESIAN_POINT('Ctrl Pts',(1.37291699203423,1.,3.94690771786926));
#58726=CARTESIAN_POINT('Ctrl Pts',(1.37381821967499,1.,3.93912709041791));
#58727=CARTESIAN_POINT('Ctrl Pts',(1.37468482215784,1.,3.93135106761941));
#58728=CARTESIAN_POINT('Ctrl Pts',(1.37551664448057,1.,3.92357976987132));
#58729=CARTESIAN_POINT('Ctrl Pts',(1.37631350505516,1.,3.91581337461825));
#58730=CARTESIAN_POINT('Ctrl Pts',(1.3770751963376,1.,3.90805209522729));
#58731=CARTESIAN_POINT('Ctrl Pts',(1.3778014851263,1.,3.90029615196255));
#58732=CARTESIAN_POINT('Ctrl Pts',(1.37849211287981,1.,3.89254574338385));
#58733=CARTESIAN_POINT('Ctrl Pts',(1.37914679719446,1.,3.88480102249461));
#58734=CARTESIAN_POINT('Ctrl Pts',(1.37976523097187,1.,3.87706205830865));
#58735=CARTESIAN_POINT('Ctrl Pts',(1.38034709213129,1.,3.86932885813403));
#58736=CARTESIAN_POINT('Ctrl Pts',(1.38089205993067,1.,3.86160143044187));
#58737=CARTESIAN_POINT('Ctrl Pts',(1.38139983115075,1.,3.85387983979557));
#58738=CARTESIAN_POINT('Ctrl Pts',(1.38187013346089,1.,3.84616425605705));
#58739=CARTESIAN_POINT('Ctrl Pts',(1.38230274828774,1.,3.83845502790609));
#58740=CARTESIAN_POINT('Ctrl Pts',(1.38269750245086,1.,3.83075266982138));
#58741=CARTESIAN_POINT('Ctrl Pts',(1.38305421262724,1.,3.82305771743715));
#58742=CARTESIAN_POINT('Ctrl Pts',(1.38337263902766,1.,3.81537060817765));
#58743=CARTESIAN_POINT('Ctrl Pts',(1.38365244046226,1.,3.80769156398429));
#58744=CARTESIAN_POINT('Ctrl Pts',(1.38389311766701,1.,3.80002044322169));
#58745=CARTESIAN_POINT('Ctrl Pts',(1.38409399694588,1.,3.79235669640907));
#58746=CARTESIAN_POINT('Ctrl Pts',(1.38425435883773,1.,3.78469969805134));
#58747=CARTESIAN_POINT('Ctrl Pts',(1.38437354551435,1.,3.77704902230441));
#58748=CARTESIAN_POINT('Ctrl Pts',(1.38445107339517,1.,3.76940473185775));
#58749=CARTESIAN_POINT('Ctrl Pts',(1.38448675253343,1.,3.76176768271347));
#58750=CARTESIAN_POINT('Ctrl Pts',(1.38448077997155,1.,3.75413976318727));
#58751=CARTESIAN_POINT('Ctrl Pts',(1.38443344984389,1.,3.7465231716786));
#58752=CARTESIAN_POINT('Ctrl Pts',(1.38434489156456,1.,3.73891976418099));
#58753=CARTESIAN_POINT('Ctrl Pts',(1.38421479111531,1.,3.73133035859283));
#58754=CARTESIAN_POINT('Ctrl Pts',(1.3840421342895,1.,3.72375409358805));
#58755=CARTESIAN_POINT('Ctrl Pts',(1.38382489984585,1.,3.7161876605181));
#58756=CARTESIAN_POINT('Ctrl Pts',(1.38356065402122,1.,3.70862680753343));
#58757=CARTESIAN_POINT('Ctrl Pts',(1.38324717612862,1.,3.70106792167894));
#58758=CARTESIAN_POINT('Ctrl Pts',(1.38288311171649,1.,3.69350967899523));
#58759=CARTESIAN_POINT('Ctrl Pts',(1.38246852827185,1.,3.68595444983844));
#58760=CARTESIAN_POINT('Ctrl Pts',(1.38200574290626,1.,3.6784103848243));
#58761=CARTESIAN_POINT('Ctrl Pts',(1.38149812653876,1.,3.67088843112282));
#58762=CARTESIAN_POINT('Ctrl Pts',(1.38094856333558,1.,3.66339848520874));
#58763=CARTESIAN_POINT('Ctrl Pts',(1.38035791051215,1.,3.65594554404396));
#58764=CARTESIAN_POINT('Ctrl Pts',(1.37972372481598,1.,3.64852652756444));
#58765=CARTESIAN_POINT('Ctrl Pts',(1.37903818567347,1.,3.64112507791112));
#58766=CARTESIAN_POINT('Ctrl Pts',(1.37829035457324,1.,3.63371727442448));
#58767=CARTESIAN_POINT('Ctrl Pts',(1.37746987919868,1.,3.62628098665112));
#58768=CARTESIAN_POINT('Ctrl Pts',(1.37657053403102,1.,3.61880481160408));
#58769=CARTESIAN_POINT('Ctrl Pts',(1.37559314436641,1.,3.61129546591082));
#58770=CARTESIAN_POINT('Ctrl Pts',(1.37455051379642,1.,3.60379020124038));
#58771=CARTESIAN_POINT('Ctrl Pts',(1.37346320103184,1.,3.59634627869117));
#58772=CARTESIAN_POINT('Ctrl Pts',(1.37235053661,1.,3.5890185384643));
#58773=CARTESIAN_POINT('Ctrl Pts',(1.37122241663073,1.,3.58183885982745));
#58774=CARTESIAN_POINT('Ctrl Pts',(1.37007229485646,1.,3.57479875549453));
#58775=CARTESIAN_POINT('Ctrl Pts',(1.36886584973349,1.,3.56782080304554));
#58776=CARTESIAN_POINT('Ctrl Pts',(1.36754771771174,1.,3.56077662028492));
#58777=CARTESIAN_POINT('Ctrl Pts',(1.36606145456711,1.,3.55353883995793));
#58778=CARTESIAN_POINT('Ctrl Pts',(1.36436666257567,1.,3.54602591832893));
#58779=CARTESIAN_POINT('Ctrl Pts',(1.36245507339334,1.,3.53824396425032));
#58780=CARTESIAN_POINT('Ctrl Pts',(1.36037259643827,1.,3.53034464961849));
#58781=CARTESIAN_POINT('Ctrl Pts',(1.35821701528975,1.,3.52261776117121));
#58782=CARTESIAN_POINT('Ctrl Pts',(1.35611275237288,1.,3.51542230699919));
#58783=CARTESIAN_POINT('Ctrl Pts',(1.35419113576022,1.,3.50913227060177));
#58784=CARTESIAN_POINT('Ctrl Pts',(1.3525703284343,1.,3.50408168106113));
#58785=CARTESIAN_POINT('Ctrl Pts',(1.35142377279535,1.,3.5007660381658));
#58786=CARTESIAN_POINT('Ctrl Pts',(1.35080045218652,1.,3.49920025459856));
#58787=CARTESIAN_POINT('Ctrl Pts',(1.35049736560633,1.,3.49861894124915));
#58788=CARTESIAN_POINT('Ctrl Pts',(1.35036670893102,1.,3.49847119623841));
#58789=CARTESIAN_POINT('Ctrl Pts',(1.35032489087269,1.,3.49844575334386));
#58790=CARTESIAN_POINT('',(1.36999806084572,0.,3.97027773754922));
#58791=CARTESIAN_POINT('Ctrl Pts',(0.96399761336957,-1.,3.62397690409552));
#58792=CARTESIAN_POINT('Ctrl Pts',(0.96399761336957,1.,3.62397690409552));
#58793=CARTESIAN_POINT('Ctrl Pts',(0.963922720982576,-1.,3.62393257642191));
#58794=CARTESIAN_POINT('Ctrl Pts',(0.963922720982576,1.,3.62393257642191));
#58795=CARTESIAN_POINT('Ctrl Pts',(0.963832486396055,-1.,3.62399933640277));
#58796=CARTESIAN_POINT('Ctrl Pts',(0.963832486396055,1.,3.62399933640277));
#58797=CARTESIAN_POINT('Ctrl Pts',(0.963875774532102,-1.,3.62456568607055));
#58798=CARTESIAN_POINT('Ctrl Pts',(0.963875774532102,1.,3.62456568607055));
#58799=CARTESIAN_POINT('Ctrl Pts',(0.964291001274618,-1.,3.62625391255277));
#58800=CARTESIAN_POINT('Ctrl Pts',(0.964291001274618,1.,3.62625391255277));
#58801=CARTESIAN_POINT('Ctrl Pts',(0.965395153165715,-1.,3.62988252139998));
#58802=CARTESIAN_POINT('Ctrl Pts',(0.965395153165715,1.,3.62988252139998));
#58803=CARTESIAN_POINT('Ctrl Pts',(0.967052554540877,-1.,3.6349212208096));
#58804=CARTESIAN_POINT('Ctrl Pts',(0.967052554540877,1.,3.6349212208096));
#58805=CARTESIAN_POINT('Ctrl Pts',(0.969195124674828,-1.,3.64113946505393));
#58806=CARTESIAN_POINT('Ctrl Pts',(0.969195124674828,1.,3.64113946505393));
#58807=CARTESIAN_POINT('Ctrl Pts',(0.971722122060277,-1.,3.64819756447072));
#58808=CARTESIAN_POINT('Ctrl Pts',(0.971722122060277,1.,3.64819756447072));
#58809=CARTESIAN_POINT('Ctrl Pts',(0.974519971354138,-1.,3.6557157673487));
#58810=CARTESIAN_POINT('Ctrl Pts',(0.974519971354138,1.,3.6557157673487));
#58811=CARTESIAN_POINT('Ctrl Pts',(0.977478312751416,-1.,3.66333049637403));
#58812=CARTESIAN_POINT('Ctrl Pts',(0.977478312751416,1.,3.66333049637403));
#58813=CARTESIAN_POINT('Ctrl Pts',(0.980505922458494,-1.,3.67074983340444));
#58814=CARTESIAN_POINT('Ctrl Pts',(0.980505922458494,1.,3.67074983340444));
#58815=CARTESIAN_POINT('Ctrl Pts',(0.983550791470864,-1.,3.67782408841876));
#58816=CARTESIAN_POINT('Ctrl Pts',(0.983550791470864,1.,3.67782408841876));
#58817=CARTESIAN_POINT('Ctrl Pts',(0.986602639864285,-1.,3.6845531792623));
#58818=CARTESIAN_POINT('Ctrl Pts',(0.986602639864285,1.,3.6845531792623));
#58819=CARTESIAN_POINT('Ctrl Pts',(0.989676715398858,-1.,3.69102682138955));
#58820=CARTESIAN_POINT('Ctrl Pts',(0.989676715398858,1.,3.69102682138955));
#58821=CARTESIAN_POINT('Ctrl Pts',(0.992802218332103,-1.,3.69738123415696));
#58822=CARTESIAN_POINT('Ctrl Pts',(0.992802218332103,1.,3.69738123415696));
#58823=CARTESIAN_POINT('Ctrl Pts',(0.996009819772431,-1.,3.70375282282107));
#58824=CARTESIAN_POINT('Ctrl Pts',(0.996009819772431,1.,3.70375282282107));
#58825=CARTESIAN_POINT('Ctrl Pts',(0.999317260756344,-1.,3.7102243971387));
#58826=CARTESIAN_POINT('Ctrl Pts',(0.999317260756344,1.,3.7102243971387));
#58827=CARTESIAN_POINT('Ctrl Pts',(1.00272423396802,-1.,3.71680667125047));
#58828=CARTESIAN_POINT('Ctrl Pts',(1.00272423396802,1.,3.71680667125047));
#58829=CARTESIAN_POINT('Ctrl Pts',(1.00622000735696,-1.,3.72346803750544));
#58830=CARTESIAN_POINT('Ctrl Pts',(1.00622000735696,1.,3.72346803750544));
#58831=CARTESIAN_POINT('Ctrl Pts',(1.00978798539491,-1.,3.73015276704407));
#58832=CARTESIAN_POINT('Ctrl Pts',(1.00978798539491,1.,3.73015276704407));
#58833=CARTESIAN_POINT('Ctrl Pts',(1.01341114319906,-1.,3.73680245055747));
#58834=CARTESIAN_POINT('Ctrl Pts',(1.01341114319906,1.,3.73680245055747));
#58835=CARTESIAN_POINT('Ctrl Pts',(1.01707794311088,-1.,3.74337942504993));
#58836=CARTESIAN_POINT('Ctrl Pts',(1.01707794311088,1.,3.74337942504993));
#58837=CARTESIAN_POINT('Ctrl Pts',(1.02078510487439,-1.,3.74987777155873));
#58838=CARTESIAN_POINT('Ctrl Pts',(1.02078510487439,1.,3.74987777155873));
#58839=CARTESIAN_POINT('Ctrl Pts',(1.02453429444668,-1.,3.75631037456224));
#58840=CARTESIAN_POINT('Ctrl Pts',(1.02453429444668,1.,3.75631037456224));
#58841=CARTESIAN_POINT('Ctrl Pts',(1.02833014458184,-1.,3.76270122291245));
#58842=CARTESIAN_POINT('Ctrl Pts',(1.02833014458184,1.,3.76270122291245));
#58843=CARTESIAN_POINT('Ctrl Pts',(1.03217786604919,-1.,3.76907609832516));
#58844=CARTESIAN_POINT('Ctrl Pts',(1.03217786604919,1.,3.76907609832516));
#58845=CARTESIAN_POINT('Ctrl Pts',(1.03608074678008,-1.,3.77545283140427));
#58846=CARTESIAN_POINT('Ctrl Pts',(1.03608074678008,1.,3.77545283140427));
#58847=CARTESIAN_POINT('Ctrl Pts',(1.04003862055798,-1.,3.7818353500817));
#58848=CARTESIAN_POINT('Ctrl Pts',(1.04003862055798,1.,3.7818353500817));
#58849=CARTESIAN_POINT('Ctrl Pts',(1.04404924374422,-1.,3.78821910787179));
#58850=CARTESIAN_POINT('Ctrl Pts',(1.04404924374422,1.,3.78821910787179));
#58851=CARTESIAN_POINT('Ctrl Pts',(1.04810913267639,-1.,3.79459440308786));
#58852=CARTESIAN_POINT('Ctrl Pts',(1.04810913267639,1.,3.79459440308786));
#58853=CARTESIAN_POINT('Ctrl Pts',(1.05221457990016,-1.,3.80095039790681));
#58854=CARTESIAN_POINT('Ctrl Pts',(1.05221457990016,1.,3.80095039790681));
#58855=CARTESIAN_POINT('Ctrl Pts',(1.05636266918644,-1.,3.80727913637791));
#58856=CARTESIAN_POINT('Ctrl Pts',(1.05636266918644,1.,3.80727913637791));
#58857=CARTESIAN_POINT('Ctrl Pts',(1.06055206187299,-1.,3.8135786611749));
#58858=CARTESIAN_POINT('Ctrl Pts',(1.06055206187299,1.,3.8135786611749));
#58859=CARTESIAN_POINT('Ctrl Pts',(1.0647824403893,-1.,3.81985083953012));
#58860=CARTESIAN_POINT('Ctrl Pts',(1.0647824403893,1.,3.81985083953012));
#58861=CARTESIAN_POINT('Ctrl Pts',(1.06905413180359,-1.,3.82609989967276));
#58862=CARTESIAN_POINT('Ctrl Pts',(1.06905413180359,1.,3.82609989967276));
#58863=CARTESIAN_POINT('Ctrl Pts',(1.07336766633459,-1.,3.83233071195144));
#58864=CARTESIAN_POINT('Ctrl Pts',(1.07336766633459,1.,3.83233071195144));
#58865=CARTESIAN_POINT('Ctrl Pts',(1.07772335353858,-1.,3.83854714117491));
#58866=CARTESIAN_POINT('Ctrl Pts',(1.07772335353858,1.,3.83854714117491));
#58867=CARTESIAN_POINT('Ctrl Pts',(1.08212087917991,-1.,3.8447504803063));
#58868=CARTESIAN_POINT('Ctrl Pts',(1.08212087917991,1.,3.8447504803063));
#58869=CARTESIAN_POINT('Ctrl Pts',(1.08655950846384,-1.,3.85094025222713));
#58870=CARTESIAN_POINT('Ctrl Pts',(1.08655950846384,1.,3.85094025222713));
#58871=CARTESIAN_POINT('Ctrl Pts',(1.09103825516294,-1.,3.85711487933931));
#58872=CARTESIAN_POINT('Ctrl Pts',(1.09103825516294,1.,3.85711487933931));
#58873=CARTESIAN_POINT('Ctrl Pts',(1.09555606505013,-1.,3.86327241021247));
#58874=CARTESIAN_POINT('Ctrl Pts',(1.09555606505013,1.,3.86327241021247));
#58875=CARTESIAN_POINT('Ctrl Pts',(1.10011198761195,-1.,3.86941120134849));
#58876=CARTESIAN_POINT('Ctrl Pts',(1.10011198761195,1.,3.86941120134849));
#58877=CARTESIAN_POINT('Ctrl Pts',(1.10470536603287,-1.,3.87553067187514));
#58878=CARTESIAN_POINT('Ctrl Pts',(1.10470536603287,1.,3.87553067187514));
#58879=CARTESIAN_POINT('Ctrl Pts',(1.10933577224008,-1.,3.88163105531724));
#58880=CARTESIAN_POINT('Ctrl Pts',(1.10933577224008,1.,3.88163105531724));
#58881=CARTESIAN_POINT('Ctrl Pts',(1.11400292434429,-1.,3.88771308285171));
#58882=CARTESIAN_POINT('Ctrl Pts',(1.11400292434429,1.,3.88771308285171));
#58883=CARTESIAN_POINT('Ctrl Pts',(1.11870660794603,-1.,3.89377768340344));
#58884=CARTESIAN_POINT('Ctrl Pts',(1.11870660794603,1.,3.89377768340344));
#58885=CARTESIAN_POINT('Ctrl Pts',(1.12344660099043,-1.,3.89982569750025));
#58886=CARTESIAN_POINT('Ctrl Pts',(1.12344660099043,1.,3.89982569750025));
#58887=CARTESIAN_POINT('Ctrl Pts',(1.12822258281553,-1.,3.90585753318737));
#58888=CARTESIAN_POINT('Ctrl Pts',(1.12822258281553,1.,3.90585753318737));
#58889=CARTESIAN_POINT('Ctrl Pts',(1.13303414693896,-1.,3.91187321145649));
#58890=CARTESIAN_POINT('Ctrl Pts',(1.13303414693896,1.,3.91187321145649));
#58891=CARTESIAN_POINT('Ctrl Pts',(1.13788084225554,-1.,3.91787251936827));
#58892=CARTESIAN_POINT('Ctrl Pts',(1.13788084225554,1.,3.91787251936827));
#58893=CARTESIAN_POINT('Ctrl Pts',(1.14276220561593,-1.,3.92385513133997));
#58894=CARTESIAN_POINT('Ctrl Pts',(1.14276220561593,1.,3.92385513133997));
#58895=CARTESIAN_POINT('Ctrl Pts',(1.14767779451123,-1.,3.92982073294257));
#58896=CARTESIAN_POINT('Ctrl Pts',(1.14767779451123,1.,3.92982073294257));
#58897=CARTESIAN_POINT('Ctrl Pts',(1.1526272271632,-1.,3.9357691705628));
#58898=CARTESIAN_POINT('Ctrl Pts',(1.1526272271632,1.,3.9357691705628));
#58899=CARTESIAN_POINT('Ctrl Pts',(1.15761018340956,-1.,3.94170046685203));
#58900=CARTESIAN_POINT('Ctrl Pts',(1.15761018340956,1.,3.94170046685203));
#58901=CARTESIAN_POINT('Ctrl Pts',(1.16262637999157,-1.,3.94761474780583));
#58902=CARTESIAN_POINT('Ctrl Pts',(1.16262637999157,1.,3.94761474780583));
#58903=CARTESIAN_POINT('Ctrl Pts',(1.16767555244438,-1.,3.95351219509876));
#58904=CARTESIAN_POINT('Ctrl Pts',(1.16767555244438,1.,3.95351219509876));
#58905=CARTESIAN_POINT('Ctrl Pts',(1.17275743590361,-1.,3.95939299213276));
#58906=CARTESIAN_POINT('Ctrl Pts',(1.17275743590361,1.,3.95939299213276));
#58907=CARTESIAN_POINT('Ctrl Pts',(1.17787174135592,-1.,3.96525726358159));
#58908=CARTESIAN_POINT('Ctrl Pts',(1.17787174135592,1.,3.96525726358159));
#58909=CARTESIAN_POINT('Ctrl Pts',(1.18301815039831,-1.,3.97110505165415));
#58910=CARTESIAN_POINT('Ctrl Pts',(1.18301815039831,1.,3.97110505165415));
#58911=CARTESIAN_POINT('Ctrl Pts',(1.18819633715539,-1.,3.97693634767754));
#58912=CARTESIAN_POINT('Ctrl Pts',(1.18819633715539,1.,3.97693634767754));
#58913=CARTESIAN_POINT('Ctrl Pts',(1.19340598349475,-1.,3.98275111052561));
#58914=CARTESIAN_POINT('Ctrl Pts',(1.19340598349475,1.,3.98275111052561));
#58915=CARTESIAN_POINT('Ctrl Pts',(1.19864679609566,-1.,3.98854928957189));
#58916=CARTESIAN_POINT('Ctrl Pts',(1.19864679609566,1.,3.98854928957189));
#58917=CARTESIAN_POINT('Ctrl Pts',(1.20391852375138,-1.,3.99433084799666));
#58918=CARTESIAN_POINT('Ctrl Pts',(1.20391852375138,1.,3.99433084799666));
#58919=CARTESIAN_POINT('Ctrl Pts',(1.20922097029551,-1.,4.00009577950721));
#58920=CARTESIAN_POINT('Ctrl Pts',(1.20922097029551,1.,4.00009577950721));
#58921=CARTESIAN_POINT('Ctrl Pts',(1.21455398918133,-1.,4.00584409522722));
#58922=CARTESIAN_POINT('Ctrl Pts',(1.21455398918133,1.,4.00584409522722));
#58923=CARTESIAN_POINT('Ctrl Pts',(1.21884478244403,-1.,4.01042947140789));
#58924=CARTESIAN_POINT('Ctrl Pts',(1.21884478244403,1.,4.01042947140789));
#58925=CARTESIAN_POINT('Ctrl Pts',(1.22207656455845,-1.,4.01386104433519));
#58926=CARTESIAN_POINT('Ctrl Pts',(1.22207656455845,1.,4.01386104433519));
#58927=CARTESIAN_POINT('Ctrl Pts',(1.22423716681317,-1.,4.01614544569895));
#58928=CARTESIAN_POINT('Ctrl Pts',(1.22423716681317,1.,4.01614544569895));
#58929=CARTESIAN_POINT('Ctrl Pts',(1.22531898815164,-1.,4.01728681790024));
#58930=CARTESIAN_POINT('Ctrl Pts',(1.22531898815164,1.,4.01728681790024));
#58931=CARTESIAN_POINT('',(0.963899035118985,1.,3.62400312501199));
#58932=CARTESIAN_POINT('Ctrl Pts',(0.963899035118985,-1.,3.62400312501199));
#58933=CARTESIAN_POINT('Ctrl Pts',(0.963899035118985,-0.666666666666667,
3.62400312501199));
#58934=CARTESIAN_POINT('Ctrl Pts',(0.963899035118985,-0.333333333333333,
3.62400312501199));
#58935=CARTESIAN_POINT('Ctrl Pts',(0.963899035118985,0.333333333333333,
3.62400312501199));
#58936=CARTESIAN_POINT('Ctrl Pts',(0.963899035118985,0.666666666666667,
3.62400312501199));
#58937=CARTESIAN_POINT('Ctrl Pts',(0.963899035118985,1.,3.62400312501199));
#58938=CARTESIAN_POINT('',(1.22531898815164,1.,4.01728681790024));
#58939=CARTESIAN_POINT('',(1.22531898815164,0.,4.01728681790024));
#58940=CARTESIAN_POINT('Ctrl Pts',(0.963899035118985,1.,3.62400312501199));
#58941=CARTESIAN_POINT('Ctrl Pts',(0.963880158556712,1.,3.62404828878375));
#58942=CARTESIAN_POINT('Ctrl Pts',(0.963861297423578,1.,3.62424461507455));
#58943=CARTESIAN_POINT('Ctrl Pts',(0.963957782642589,1.,3.62489305727516));
#58944=CARTESIAN_POINT('Ctrl Pts',(0.964373850166081,1.,3.62652618145252));
#58945=CARTESIAN_POINT('Ctrl Pts',(0.965395153165715,1.,3.62988252139998));
#58946=CARTESIAN_POINT('Ctrl Pts',(0.967052554540877,1.,3.6349212208096));
#58947=CARTESIAN_POINT('Ctrl Pts',(0.969195124674828,1.,3.64113946505393));
#58948=CARTESIAN_POINT('Ctrl Pts',(0.971722122060277,1.,3.64819756447072));
#58949=CARTESIAN_POINT('Ctrl Pts',(0.974519971354138,1.,3.6557157673487));
#58950=CARTESIAN_POINT('Ctrl Pts',(0.977478312751416,1.,3.66333049637403));
#58951=CARTESIAN_POINT('Ctrl Pts',(0.980505922458494,1.,3.67074983340444));
#58952=CARTESIAN_POINT('Ctrl Pts',(0.983550791470864,1.,3.67782408841876));
#58953=CARTESIAN_POINT('Ctrl Pts',(0.986602639864285,1.,3.6845531792623));
#58954=CARTESIAN_POINT('Ctrl Pts',(0.989676715398858,1.,3.69102682138955));
#58955=CARTESIAN_POINT('Ctrl Pts',(0.992802218332103,1.,3.69738123415696));
#58956=CARTESIAN_POINT('Ctrl Pts',(0.996009819772431,1.,3.70375282282107));
#58957=CARTESIAN_POINT('Ctrl Pts',(0.999317260756344,1.,3.7102243971387));
#58958=CARTESIAN_POINT('Ctrl Pts',(1.00272423396802,1.,3.71680667125047));
#58959=CARTESIAN_POINT('Ctrl Pts',(1.00622000735696,1.,3.72346803750544));
#58960=CARTESIAN_POINT('Ctrl Pts',(1.00978798539491,1.,3.73015276704407));
#58961=CARTESIAN_POINT('Ctrl Pts',(1.01341114319906,1.,3.73680245055747));
#58962=CARTESIAN_POINT('Ctrl Pts',(1.01707794311088,1.,3.74337942504993));
#58963=CARTESIAN_POINT('Ctrl Pts',(1.02078510487439,1.,3.74987777155873));
#58964=CARTESIAN_POINT('Ctrl Pts',(1.02453429444668,1.,3.75631037456224));
#58965=CARTESIAN_POINT('Ctrl Pts',(1.02833014458184,1.,3.76270122291245));
#58966=CARTESIAN_POINT('Ctrl Pts',(1.03217786604919,1.,3.76907609832516));
#58967=CARTESIAN_POINT('Ctrl Pts',(1.03608074678008,1.,3.77545283140427));
#58968=CARTESIAN_POINT('Ctrl Pts',(1.04003862055798,1.,3.7818353500817));
#58969=CARTESIAN_POINT('Ctrl Pts',(1.04404924374422,1.,3.78821910787179));
#58970=CARTESIAN_POINT('Ctrl Pts',(1.04810913267639,1.,3.79459440308786));
#58971=CARTESIAN_POINT('Ctrl Pts',(1.05221457990016,1.,3.80095039790681));
#58972=CARTESIAN_POINT('Ctrl Pts',(1.05636266918644,1.,3.80727913637791));
#58973=CARTESIAN_POINT('Ctrl Pts',(1.06055206187299,1.,3.8135786611749));
#58974=CARTESIAN_POINT('Ctrl Pts',(1.0647824403893,1.,3.81985083953012));
#58975=CARTESIAN_POINT('Ctrl Pts',(1.06905413180359,1.,3.82609989967276));
#58976=CARTESIAN_POINT('Ctrl Pts',(1.07336766633459,1.,3.83233071195144));
#58977=CARTESIAN_POINT('Ctrl Pts',(1.07772335353858,1.,3.83854714117491));
#58978=CARTESIAN_POINT('Ctrl Pts',(1.08212087917991,1.,3.8447504803063));
#58979=CARTESIAN_POINT('Ctrl Pts',(1.08655950846384,1.,3.85094025222713));
#58980=CARTESIAN_POINT('Ctrl Pts',(1.09103825516294,1.,3.85711487933931));
#58981=CARTESIAN_POINT('Ctrl Pts',(1.09555606505013,1.,3.86327241021247));
#58982=CARTESIAN_POINT('Ctrl Pts',(1.10011198761195,1.,3.86941120134849));
#58983=CARTESIAN_POINT('Ctrl Pts',(1.10470536603287,1.,3.87553067187514));
#58984=CARTESIAN_POINT('Ctrl Pts',(1.10933577224008,1.,3.88163105531724));
#58985=CARTESIAN_POINT('Ctrl Pts',(1.11400292434429,1.,3.88771308285171));
#58986=CARTESIAN_POINT('Ctrl Pts',(1.11870660794603,1.,3.89377768340344));
#58987=CARTESIAN_POINT('Ctrl Pts',(1.12344660099043,1.,3.89982569750025));
#58988=CARTESIAN_POINT('Ctrl Pts',(1.12822258281553,1.,3.90585753318737));
#58989=CARTESIAN_POINT('Ctrl Pts',(1.13303414693896,1.,3.91187321145649));
#58990=CARTESIAN_POINT('Ctrl Pts',(1.13788084225554,1.,3.91787251936827));
#58991=CARTESIAN_POINT('Ctrl Pts',(1.14276220561593,1.,3.92385513133997));
#58992=CARTESIAN_POINT('Ctrl Pts',(1.14767779451123,1.,3.92982073294257));
#58993=CARTESIAN_POINT('Ctrl Pts',(1.1526272271632,1.,3.9357691705628));
#58994=CARTESIAN_POINT('Ctrl Pts',(1.15761018340956,1.,3.94170046685203));
#58995=CARTESIAN_POINT('Ctrl Pts',(1.16262637999157,1.,3.94761474780583));
#58996=CARTESIAN_POINT('Ctrl Pts',(1.16767555244438,1.,3.95351219509876));
#58997=CARTESIAN_POINT('Ctrl Pts',(1.17275743590361,1.,3.95939299213276));
#58998=CARTESIAN_POINT('Ctrl Pts',(1.17787174135592,1.,3.96525726358159));
#58999=CARTESIAN_POINT('Ctrl Pts',(1.18301815039831,1.,3.97110505165415));
#59000=CARTESIAN_POINT('Ctrl Pts',(1.18819633715539,1.,3.97693634767754));
#59001=CARTESIAN_POINT('Ctrl Pts',(1.19340598349475,1.,3.98275111052561));
#59002=CARTESIAN_POINT('Ctrl Pts',(1.19864679609566,1.,3.98854928957189));
#59003=CARTESIAN_POINT('Ctrl Pts',(1.20391852375138,1.,3.99433084799666));
#59004=CARTESIAN_POINT('Ctrl Pts',(1.20922097029551,1.,4.00009577950721));
#59005=CARTESIAN_POINT('Ctrl Pts',(1.21455398918133,1.,4.00584409522722));
#59006=CARTESIAN_POINT('Ctrl Pts',(1.21884478244403,1.,4.01042947140789));
#59007=CARTESIAN_POINT('Ctrl Pts',(1.22207656455845,1.,4.01386104433519));
#59008=CARTESIAN_POINT('Ctrl Pts',(1.22423716681317,1.,4.01614544569895));
#59009=CARTESIAN_POINT('Ctrl Pts',(1.22531898815164,1.,4.01728681790024));
#59010=CARTESIAN_POINT('Origin',(1.22531898815164,0.,4.01728681790024));
#59011=CARTESIAN_POINT('',(1.36999806084572,1.,3.97027773754922));
#59012=CARTESIAN_POINT('Origin',(0.,0.,0.));
#59013=CARTESIAN_POINT('',(0.786422660833742,1.,3.66661143271648));
#59014=CARTESIAN_POINT('Origin',(0.,1.,0.));
#59015=CARTESIAN_POINT('Ctrl Pts',(0.786422660833742,1.,3.66661143271648));
#59016=CARTESIAN_POINT('Ctrl Pts',(0.786422660833742,0.666666666666667,
3.66661143271648));
#59017=CARTESIAN_POINT('Ctrl Pts',(0.786422660833742,0.333333333333333,
3.66661143271648));
#59018=CARTESIAN_POINT('Ctrl Pts',(0.786422660833742,-0.333333333333333,
3.66661143271648));
#59019=CARTESIAN_POINT('Ctrl Pts',(0.786422660833742,-0.666666666666667,
3.66661143271648));
#59020=CARTESIAN_POINT('Ctrl Pts',(0.786422660833742,-1.,3.66661143271648));
#59021=CARTESIAN_POINT('Ctrl Pts',(0.732042837400619,-1.,4.13571194405636));
#59022=CARTESIAN_POINT('Ctrl Pts',(0.732042837400619,1.,4.13571194405636));
#59023=CARTESIAN_POINT('Ctrl Pts',(0.732488575135925,-1.,4.13420383737278));
#59024=CARTESIAN_POINT('Ctrl Pts',(0.732488575135925,1.,4.13420383737278));
#59025=CARTESIAN_POINT('Ctrl Pts',(0.733376589325634,-1.,4.13118752796397));
#59026=CARTESIAN_POINT('Ctrl Pts',(0.733376589325634,1.,4.13118752796397));
#59027=CARTESIAN_POINT('Ctrl Pts',(0.734698226767512,-1.,4.12666277572794));
#59028=CARTESIAN_POINT('Ctrl Pts',(0.734698226767512,1.,4.12666277572794));
#59029=CARTESIAN_POINT('Ctrl Pts',(0.736439634335347,-1.,4.12062919626082));
#59030=CARTESIAN_POINT('Ctrl Pts',(0.736439634335347,1.,4.12062919626082));
#59031=CARTESIAN_POINT('Ctrl Pts',(0.738581708229118,-1.,4.11308626953795));
#59032=CARTESIAN_POINT('Ctrl Pts',(0.738581708229118,1.,4.11308626953795));
#59033=CARTESIAN_POINT('Ctrl Pts',(0.740688998555151,-1.,4.1055424175856));
#59034=CARTESIAN_POINT('Ctrl Pts',(0.740688998555151,1.,4.1055424175856));
#59035=CARTESIAN_POINT('Ctrl Pts',(0.742761369690017,-1.,4.09799769702712));
#59036=CARTESIAN_POINT('Ctrl Pts',(0.742761369690017,1.,4.09799769702712));
#59037=CARTESIAN_POINT('Ctrl Pts',(0.744798649705513,-1.,4.09045220253011));
#59038=CARTESIAN_POINT('Ctrl Pts',(0.744798649705513,1.,4.09045220253011));
#59039=CARTESIAN_POINT('Ctrl Pts',(0.746800631490821,-1.,4.08290608094789));
#59040=CARTESIAN_POINT('Ctrl Pts',(0.746800631490821,1.,4.08290608094789));
#59041=CARTESIAN_POINT('Ctrl Pts',(0.748767076679176,-1.,4.07535951055363));
#59042=CARTESIAN_POINT('Ctrl Pts',(0.748767076679176,1.,4.07535951055363));
#59043=CARTESIAN_POINT('Ctrl Pts',(0.750697720483175,-1.,4.06781267241886));
#59044=CARTESIAN_POINT('Ctrl Pts',(0.750697720483175,1.,4.06781267241886));
#59045=CARTESIAN_POINT('Ctrl Pts',(0.752592276482868,-1.,4.06026572221399));
#59046=CARTESIAN_POINT('Ctrl Pts',(0.752592276482868,1.,4.06026572221399));
#59047=CARTESIAN_POINT('Ctrl Pts',(0.754450441816411,-1.,4.05271876688106));
#59048=CARTESIAN_POINT('Ctrl Pts',(0.754450441816411,1.,4.05271876688106));
#59049=CARTESIAN_POINT('Ctrl Pts',(0.756271902370186,-1.,4.04517182654344));
#59050=CARTESIAN_POINT('Ctrl Pts',(0.756271902370186,1.,4.04517182654344));
#59051=CARTESIAN_POINT('Ctrl Pts',(0.758056338885553,-1.,4.03762485803468));
#59052=CARTESIAN_POINT('Ctrl Pts',(0.758056338885553,1.,4.03762485803468));
#59053=CARTESIAN_POINT('Ctrl Pts',(0.759803433244165,-1.,4.0300778195465));
#59054=CARTESIAN_POINT('Ctrl Pts',(0.759803433244165,1.,4.0300778195465));
#59055=CARTESIAN_POINT('Ctrl Pts',(0.761512875859941,-1.,4.02253072741347));
#59056=CARTESIAN_POINT('Ctrl Pts',(0.761512875859941,1.,4.02253072741347));
#59057=CARTESIAN_POINT('Ctrl Pts',(0.763184371182826,-1.,4.01498370680434));
#59058=CARTESIAN_POINT('Ctrl Pts',(0.763184371182826,1.,4.01498370680434));
#59059=CARTESIAN_POINT('Ctrl Pts',(0.764817648784946,-1.,4.00743706791366));
#59060=CARTESIAN_POINT('Ctrl Pts',(0.764817648784946,1.,4.00743706791366));
#59061=CARTESIAN_POINT('Ctrl Pts',(0.766412457135785,-1.,3.99989129179464));
#59062=CARTESIAN_POINT('Ctrl Pts',(0.766412457135785,1.,3.99989129179464));
#59063=CARTESIAN_POINT('Ctrl Pts',(0.767968531377707,-1.,3.99234687880892));
#59064=CARTESIAN_POINT('Ctrl Pts',(0.767968531377707,1.,3.99234687880892));
#59065=CARTESIAN_POINT('Ctrl Pts',(0.769485566245459,-1.,3.98480422348403));
#59066=CARTESIAN_POINT('Ctrl Pts',(0.769485566245459,1.,3.98480422348403));
#59067=CARTESIAN_POINT('Ctrl Pts',(0.770963190030503,-1.,3.97726349165507));
#59068=CARTESIAN_POINT('Ctrl Pts',(0.770963190030503,1.,3.97726349165507));
#59069=CARTESIAN_POINT('Ctrl Pts',(0.772400931772238,-1.,3.96972446532832));
#59070=CARTESIAN_POINT('Ctrl Pts',(0.772400931772238,1.,3.96972446532832));
#59071=CARTESIAN_POINT('Ctrl Pts',(0.773798212026682,-1.,3.96218649639876));
#59072=CARTESIAN_POINT('Ctrl Pts',(0.773798212026682,1.,3.96218649639876));
#59073=CARTESIAN_POINT('Ctrl Pts',(0.775154418039441,-1.,3.95464885452364));
#59074=CARTESIAN_POINT('Ctrl Pts',(0.775154418039441,1.,3.95464885452364));
#59075=CARTESIAN_POINT('Ctrl Pts',(0.776468966697959,-1.,3.94711101619471));
#59076=CARTESIAN_POINT('Ctrl Pts',(0.776468966697959,1.,3.94711101619471));
#59077=CARTESIAN_POINT('Ctrl Pts',(0.777741370568549,-1.,3.93957296768098));
#59078=CARTESIAN_POINT('Ctrl Pts',(0.777741370568549,1.,3.93957296768098));
#59079=CARTESIAN_POINT('Ctrl Pts',(0.778971308134786,-1.,3.93203552473153));
#59080=CARTESIAN_POINT('Ctrl Pts',(0.778971308134786,1.,3.93203552473153));
#59081=CARTESIAN_POINT('Ctrl Pts',(0.780158678615506,-1.,3.92450058323799));
#59082=CARTESIAN_POINT('Ctrl Pts',(0.780158678615506,1.,3.92450058323799));
#59083=CARTESIAN_POINT('Ctrl Pts',(0.781303428618343,-1.,3.9169703605466));
#59084=CARTESIAN_POINT('Ctrl Pts',(0.781303428618343,1.,3.9169703605466));
#59085=CARTESIAN_POINT('Ctrl Pts',(0.782405395622758,-1.,3.90944671004536));
#59086=CARTESIAN_POINT('Ctrl Pts',(0.782405395622758,1.,3.90944671004536));
#59087=CARTESIAN_POINT('Ctrl Pts',(0.783464141529082,-1.,3.90193039043971));
#59088=CARTESIAN_POINT('Ctrl Pts',(0.783464141529082,1.,3.90193039043971));
#59089=CARTESIAN_POINT('Ctrl Pts',(0.784478799358335,-1.,3.89442039235105));
#59090=CARTESIAN_POINT('Ctrl Pts',(0.784478799358335,1.,3.89442039235105));
#59091=CARTESIAN_POINT('Ctrl Pts',(0.785447890340723,-1.,3.88691313167399));
#59092=CARTESIAN_POINT('Ctrl Pts',(0.785447890340723,1.,3.88691313167399));
#59093=CARTESIAN_POINT('Ctrl Pts',(0.786369675812591,-1.,3.87940402818186));
#59094=CARTESIAN_POINT('Ctrl Pts',(0.786369675812591,1.,3.87940402818186));
#59095=CARTESIAN_POINT('Ctrl Pts',(0.78724252761798,-1.,3.87188916600905));
#59096=CARTESIAN_POINT('Ctrl Pts',(0.78724252761798,1.,3.87188916600905));
#59097=CARTESIAN_POINT('Ctrl Pts',(0.78806531509377,-1.,3.86436702561342));
#59098=CARTESIAN_POINT('Ctrl Pts',(0.78806531509377,1.,3.86436702561342));
#59099=CARTESIAN_POINT('Ctrl Pts',(0.788837734090688,-1.,3.85683995872536));
#59100=CARTESIAN_POINT('Ctrl Pts',(0.788837734090688,1.,3.85683995872536));
#59101=CARTESIAN_POINT('Ctrl Pts',(0.789560798155618,-1.,3.8493163780891));
#59102=CARTESIAN_POINT('Ctrl Pts',(0.789560798155618,1.,3.8493163780891));
#59103=CARTESIAN_POINT('Ctrl Pts',(0.790236124191289,-1.,3.84180762342476));
#59104=CARTESIAN_POINT('Ctrl Pts',(0.790236124191289,1.,3.84180762342476));
#59105=CARTESIAN_POINT('Ctrl Pts',(0.790865012705339,-1.,3.83432392054804));
#59106=CARTESIAN_POINT('Ctrl Pts',(0.790865012705339,1.,3.83432392054804));
#59107=CARTESIAN_POINT('Ctrl Pts',(0.791447528662381,-1.,3.82687033899799));
#59108=CARTESIAN_POINT('Ctrl Pts',(0.791447528662381,1.,3.82687033899799));
#59109=CARTESIAN_POINT('Ctrl Pts',(0.791981740718606,-1.,3.81944345442237));
#59110=CARTESIAN_POINT('Ctrl Pts',(0.791981740718606,1.,3.81944345442237));
#59111=CARTESIAN_POINT('Ctrl Pts',(0.792462483517568,-1.,3.81202588694726));
#59112=CARTESIAN_POINT('Ctrl Pts',(0.792462483517568,1.,3.81202588694726));
#59113=CARTESIAN_POINT('Ctrl Pts',(0.792882695234692,-1.,3.80459229925598));
#59114=CARTESIAN_POINT('Ctrl Pts',(0.792882695234692,1.,3.80459229925598));
#59115=CARTESIAN_POINT('Ctrl Pts',(0.7932356129732,-1.,3.79711921389862));
#59116=CARTESIAN_POINT('Ctrl Pts',(0.7932356129732,1.,3.79711921389862));
#59117=CARTESIAN_POINT('Ctrl Pts',(0.793516871680965,-1.,3.78959439439222));
#59118=CARTESIAN_POINT('Ctrl Pts',(0.793516871680965,1.,3.78959439439222));
#59119=CARTESIAN_POINT('Ctrl Pts',(0.793726235781339,-1.,3.78202460377617));
#59120=CARTESIAN_POINT('Ctrl Pts',(0.793726235781339,1.,3.78202460377617));
#59121=CARTESIAN_POINT('Ctrl Pts',(0.793870523787515,-1.,3.77444863801264));
#59122=CARTESIAN_POINT('Ctrl Pts',(0.793870523787515,1.,3.77444863801264));
#59123=CARTESIAN_POINT('Ctrl Pts',(0.793961083689141,-1.,3.76692626931184));
#59124=CARTESIAN_POINT('Ctrl Pts',(0.793961083689141,1.,3.76692626931184));
#59125=CARTESIAN_POINT('Ctrl Pts',(0.794008429135046,-1.,3.75951468666325));
#59126=CARTESIAN_POINT('Ctrl Pts',(0.794008429135046,1.,3.75951468666325));
#59127=CARTESIAN_POINT('Ctrl Pts',(0.79401734737144,-1.,3.75224692493895));
#59128=CARTESIAN_POINT('Ctrl Pts',(0.79401734737144,1.,3.75224692493895));
#59129=CARTESIAN_POINT('Ctrl Pts',(0.79398270045988,-1.,3.74511357728827));
#59130=CARTESIAN_POINT('Ctrl Pts',(0.79398270045988,1.,3.74511357728827));
#59131=CARTESIAN_POINT('Ctrl Pts',(0.79388270093679,-1.,3.73803280541576));
#59132=CARTESIAN_POINT('Ctrl Pts',(0.79388270093679,1.,3.73803280541576));
#59133=CARTESIAN_POINT('Ctrl Pts',(0.793682750269347,-1.,3.7308691469564));
#59134=CARTESIAN_POINT('Ctrl Pts',(0.793682750269347,1.,3.7308691469564));
#59135=CARTESIAN_POINT('Ctrl Pts',(0.79334702378387,-1.,3.7234879729357));
#59136=CARTESIAN_POINT('Ctrl Pts',(0.79334702378387,1.,3.7234879729357));
#59137=CARTESIAN_POINT('Ctrl Pts',(0.792848377370115,-1.,3.7158024239604));
#59138=CARTESIAN_POINT('Ctrl Pts',(0.792848377370115,1.,3.7158024239604));
#59139=CARTESIAN_POINT('Ctrl Pts',(0.792177688845967,-1.,3.70781724021879));
#59140=CARTESIAN_POINT('Ctrl Pts',(0.792177688845967,1.,3.70781724021879));
#59141=CARTESIAN_POINT('Ctrl Pts',(0.791356575696508,-1.,3.69968940808982));
#59142=CARTESIAN_POINT('Ctrl Pts',(0.791356575696508,1.,3.69968940808982));
#59143=CARTESIAN_POINT('Ctrl Pts',(0.790436284989579,-1.,3.69172044327754));
#59144=CARTESIAN_POINT('Ctrl Pts',(0.790436284989579,1.,3.69172044327754));
#59145=CARTESIAN_POINT('Ctrl Pts',(0.789483546065158,-1.,3.68428439784285));
#59146=CARTESIAN_POINT('Ctrl Pts',(0.789483546065158,1.,3.68428439784285));
#59147=CARTESIAN_POINT('Ctrl Pts',(0.788569566220662,-1.,3.67777119516438));
#59148=CARTESIAN_POINT('Ctrl Pts',(0.788569566220662,1.,3.67777119516438));
#59149=CARTESIAN_POINT('Ctrl Pts',(0.787758799995426,-1.,3.672529236635));
#59150=CARTESIAN_POINT('Ctrl Pts',(0.787758799995426,1.,3.672529236635));
#59151=CARTESIAN_POINT('Ctrl Pts',(0.787095252589507,-1.,3.66879484800625));
#59152=CARTESIAN_POINT('Ctrl Pts',(0.787095252589507,1.,3.66879484800625));
#59153=CARTESIAN_POINT('Ctrl Pts',(0.786698783541657,-1.,3.66710211819938));
#59154=CARTESIAN_POINT('Ctrl Pts',(0.786698783541657,1.,3.66710211819938));
#59155=CARTESIAN_POINT('Ctrl Pts',(0.786480236184947,-1.,3.66657784454965));
#59156=CARTESIAN_POINT('Ctrl Pts',(0.786480236184947,1.,3.66657784454965));
#59157=CARTESIAN_POINT('Ctrl Pts',(0.786369528183039,-1.,3.66655932661846));
#59158=CARTESIAN_POINT('Ctrl Pts',(0.786369528183039,1.,3.66655932661846));
#59159=CARTESIAN_POINT('Ctrl Pts',(0.786322922920599,-1.,3.66663282329846));
#59160=CARTESIAN_POINT('Ctrl Pts',(0.786322922920599,1.,3.66663282329846));
#59161=CARTESIAN_POINT('',(0.732042837400619,1.,4.13571194405636));
#59162=CARTESIAN_POINT('Ctrl Pts',(0.732042837400619,1.,4.13571194405636));
#59163=CARTESIAN_POINT('Ctrl Pts',(0.732488575135925,1.,4.13420383737278));
#59164=CARTESIAN_POINT('Ctrl Pts',(0.733376589325634,1.,4.13118752796397));
#59165=CARTESIAN_POINT('Ctrl Pts',(0.734698226767512,1.,4.12666277572794));
#59166=CARTESIAN_POINT('Ctrl Pts',(0.736439634335347,1.,4.12062919626082));
#59167=CARTESIAN_POINT('Ctrl Pts',(0.738581708229118,1.,4.11308626953795));
#59168=CARTESIAN_POINT('Ctrl Pts',(0.740688998555151,1.,4.1055424175856));
#59169=CARTESIAN_POINT('Ctrl Pts',(0.742761369690017,1.,4.09799769702712));
#59170=CARTESIAN_POINT('Ctrl Pts',(0.744798649705513,1.,4.09045220253011));
#59171=CARTESIAN_POINT('Ctrl Pts',(0.746800631490821,1.,4.08290608094789));
#59172=CARTESIAN_POINT('Ctrl Pts',(0.748767076679176,1.,4.07535951055363));
#59173=CARTESIAN_POINT('Ctrl Pts',(0.750697720483175,1.,4.06781267241886));
#59174=CARTESIAN_POINT('Ctrl Pts',(0.752592276482868,1.,4.06026572221399));
#59175=CARTESIAN_POINT('Ctrl Pts',(0.754450441816411,1.,4.05271876688106));
#59176=CARTESIAN_POINT('Ctrl Pts',(0.756271902370186,1.,4.04517182654344));
#59177=CARTESIAN_POINT('Ctrl Pts',(0.758056338885553,1.,4.03762485803468));
#59178=CARTESIAN_POINT('Ctrl Pts',(0.759803433244165,1.,4.0300778195465));
#59179=CARTESIAN_POINT('Ctrl Pts',(0.761512875859941,1.,4.02253072741347));
#59180=CARTESIAN_POINT('Ctrl Pts',(0.763184371182826,1.,4.01498370680434));
#59181=CARTESIAN_POINT('Ctrl Pts',(0.764817648784946,1.,4.00743706791366));
#59182=CARTESIAN_POINT('Ctrl Pts',(0.766412457135785,1.,3.99989129179464));
#59183=CARTESIAN_POINT('Ctrl Pts',(0.767968531377707,1.,3.99234687880892));
#59184=CARTESIAN_POINT('Ctrl Pts',(0.769485566245459,1.,3.98480422348403));
#59185=CARTESIAN_POINT('Ctrl Pts',(0.770963190030503,1.,3.97726349165507));
#59186=CARTESIAN_POINT('Ctrl Pts',(0.772400931772238,1.,3.96972446532832));
#59187=CARTESIAN_POINT('Ctrl Pts',(0.773798212026682,1.,3.96218649639876));
#59188=CARTESIAN_POINT('Ctrl Pts',(0.775154418039441,1.,3.95464885452364));
#59189=CARTESIAN_POINT('Ctrl Pts',(0.776468966697959,1.,3.94711101619471));
#59190=CARTESIAN_POINT('Ctrl Pts',(0.777741370568549,1.,3.93957296768098));
#59191=CARTESIAN_POINT('Ctrl Pts',(0.778971308134786,1.,3.93203552473153));
#59192=CARTESIAN_POINT('Ctrl Pts',(0.780158678615506,1.,3.92450058323799));
#59193=CARTESIAN_POINT('Ctrl Pts',(0.781303428618343,1.,3.9169703605466));
#59194=CARTESIAN_POINT('Ctrl Pts',(0.782405395622758,1.,3.90944671004536));
#59195=CARTESIAN_POINT('Ctrl Pts',(0.783464141529082,1.,3.90193039043971));
#59196=CARTESIAN_POINT('Ctrl Pts',(0.784478799358335,1.,3.89442039235105));
#59197=CARTESIAN_POINT('Ctrl Pts',(0.785447890340723,1.,3.88691313167399));
#59198=CARTESIAN_POINT('Ctrl Pts',(0.786369675812591,1.,3.87940402818186));
#59199=CARTESIAN_POINT('Ctrl Pts',(0.78724252761798,1.,3.87188916600905));
#59200=CARTESIAN_POINT('Ctrl Pts',(0.78806531509377,1.,3.86436702561342));
#59201=CARTESIAN_POINT('Ctrl Pts',(0.788837734090688,1.,3.85683995872536));
#59202=CARTESIAN_POINT('Ctrl Pts',(0.789560798155618,1.,3.8493163780891));
#59203=CARTESIAN_POINT('Ctrl Pts',(0.790236124191289,1.,3.84180762342476));
#59204=CARTESIAN_POINT('Ctrl Pts',(0.790865012705339,1.,3.83432392054804));
#59205=CARTESIAN_POINT('Ctrl Pts',(0.791447528662381,1.,3.82687033899799));
#59206=CARTESIAN_POINT('Ctrl Pts',(0.791981740718606,1.,3.81944345442237));
#59207=CARTESIAN_POINT('Ctrl Pts',(0.792462483517568,1.,3.81202588694726));
#59208=CARTESIAN_POINT('Ctrl Pts',(0.792882695234692,1.,3.80459229925598));
#59209=CARTESIAN_POINT('Ctrl Pts',(0.7932356129732,1.,3.79711921389862));
#59210=CARTESIAN_POINT('Ctrl Pts',(0.793516871680965,1.,3.78959439439222));
#59211=CARTESIAN_POINT('Ctrl Pts',(0.793726235781339,1.,3.78202460377617));
#59212=CARTESIAN_POINT('Ctrl Pts',(0.793870523787515,1.,3.77444863801264));
#59213=CARTESIAN_POINT('Ctrl Pts',(0.793961083689141,1.,3.76692626931184));
#59214=CARTESIAN_POINT('Ctrl Pts',(0.794008429135046,1.,3.75951468666325));
#59215=CARTESIAN_POINT('Ctrl Pts',(0.79401734737144,1.,3.75224692493895));
#59216=CARTESIAN_POINT('Ctrl Pts',(0.79398270045988,1.,3.74511357728827));
#59217=CARTESIAN_POINT('Ctrl Pts',(0.79388270093679,1.,3.73803280541576));
#59218=CARTESIAN_POINT('Ctrl Pts',(0.793682750269347,1.,3.7308691469564));
#59219=CARTESIAN_POINT('Ctrl Pts',(0.79334702378387,1.,3.7234879729357));
#59220=CARTESIAN_POINT('Ctrl Pts',(0.792848377370115,1.,3.7158024239604));
#59221=CARTESIAN_POINT('Ctrl Pts',(0.792177688845967,1.,3.70781724021879));
#59222=CARTESIAN_POINT('Ctrl Pts',(0.791356575696508,1.,3.69968940808982));
#59223=CARTESIAN_POINT('Ctrl Pts',(0.790436284989579,1.,3.69172044327754));
#59224=CARTESIAN_POINT('Ctrl Pts',(0.789483546065158,1.,3.68428439784285));
#59225=CARTESIAN_POINT('Ctrl Pts',(0.788569566220662,1.,3.67777119516438));
#59226=CARTESIAN_POINT('Ctrl Pts',(0.787758799995426,1.,3.672529236635));
#59227=CARTESIAN_POINT('Ctrl Pts',(0.787145041181588,1.,3.66907505398769));
#59228=CARTESIAN_POINT('Ctrl Pts',(0.786774337198499,1.,3.66743103898844));
#59229=CARTESIAN_POINT('Ctrl Pts',(0.786565919559889,1.,3.66680946938396));
#59230=CARTESIAN_POINT('Ctrl Pts',(0.786459983896781,1.,3.66664310415236));
#59231=CARTESIAN_POINT('Ctrl Pts',(0.786422660833743,1.,3.66661143271648));
#59232=CARTESIAN_POINT('',(0.732042837400619,0.,4.13571194405636));
#59233=CARTESIAN_POINT('Ctrl Pts',(0.385214314776328,-1.,3.73016218570874));
#59234=CARTESIAN_POINT('Ctrl Pts',(0.385214314776328,1.,3.73016218570874));
#59235=CARTESIAN_POINT('Ctrl Pts',(0.385147278814803,-1.,3.73010668803185));
#59236=CARTESIAN_POINT('Ctrl Pts',(0.385147278814803,1.,3.73010668803185));
#59237=CARTESIAN_POINT('Ctrl Pts',(0.385047711603887,-1.,3.73015851028729));
#59238=CARTESIAN_POINT('Ctrl Pts',(0.385047711603887,1.,3.73015851028729));
#59239=CARTESIAN_POINT('Ctrl Pts',(0.385001870183841,-1.,3.73072465900727));
#59240=CARTESIAN_POINT('Ctrl Pts',(0.385001870183841,1.,3.73072465900727));
#59241=CARTESIAN_POINT('Ctrl Pts',(0.385147887989514,-1.,3.73245705639337));
#59242=CARTESIAN_POINT('Ctrl Pts',(0.385147887989514,1.,3.73245705639337));
#59243=CARTESIAN_POINT('Ctrl Pts',(0.385670806454744,-1.,3.73621371845475));
#59244=CARTESIAN_POINT('Ctrl Pts',(0.385670806454744,1.,3.73621371845475));
#59245=CARTESIAN_POINT('Ctrl Pts',(0.386519576222035,-1.,3.74144965781088));
#59246=CARTESIAN_POINT('Ctrl Pts',(0.386519576222035,1.,3.74144965781088));
#59247=CARTESIAN_POINT('Ctrl Pts',(0.387663020050396,-1.,3.74792651696269));
#59248=CARTESIAN_POINT('Ctrl Pts',(0.387663020050396,1.,3.74792651696269));
#59249=CARTESIAN_POINT('Ctrl Pts',(0.38905477589825,-1.,3.75529302894757));
#59250=CARTESIAN_POINT('Ctrl Pts',(0.38905477589825,1.,3.75529302894757));
#59251=CARTESIAN_POINT('Ctrl Pts',(0.390642072979258,-1.,3.76315635032993));
#59252=CARTESIAN_POINT('Ctrl Pts',(0.390642072979258,1.,3.76315635032993));
#59253=CARTESIAN_POINT('Ctrl Pts',(0.392372786223346,-1.,3.77114011595892));
#59254=CARTESIAN_POINT('Ctrl Pts',(0.392372786223346,1.,3.77114011595892));
#59255=CARTESIAN_POINT('Ctrl Pts',(0.394202481011595,-1.,3.77894173114368));
#59256=CARTESIAN_POINT('Ctrl Pts',(0.394202481011595,1.,3.77894173114368));
#59257=CARTESIAN_POINT('Ctrl Pts',(0.396103205335028,-1.,3.78640521279479));
#59258=CARTESIAN_POINT('Ctrl Pts',(0.396103205335028,1.,3.78640521279479));
#59259=CARTESIAN_POINT('Ctrl Pts',(0.398064818684158,-1.,3.79352887163457));
#59260=CARTESIAN_POINT('Ctrl Pts',(0.398064818684158,1.,3.79352887163457));
#59261=CARTESIAN_POINT('Ctrl Pts',(0.400088346504726,-1.,3.80040370384659));
#59262=CARTESIAN_POINT('Ctrl Pts',(0.400088346504726,1.,3.80040370384659));
#59263=CARTESIAN_POINT('Ctrl Pts',(0.402181320148474,-1.,3.80716881962763));
#59264=CARTESIAN_POINT('Ctrl Pts',(0.402181320148474,1.,3.80716881962763));
#59265=CARTESIAN_POINT('Ctrl Pts',(0.404352694628236,-1.,3.81396374287762));
#59266=CARTESIAN_POINT('Ctrl Pts',(0.404352694628236,1.,3.81396374287762));
#59267=CARTESIAN_POINT('Ctrl Pts',(0.406607038258906,-1.,3.82087303913741));
#59268=CARTESIAN_POINT('Ctrl Pts',(0.406607038258906,1.,3.82087303913741));
#59269=CARTESIAN_POINT('Ctrl Pts',(0.408942371447376,-1.,3.82790724256397));
#59270=CARTESIAN_POINT('Ctrl Pts',(0.408942371447376,1.,3.82790724256397));
#59271=CARTESIAN_POINT('Ctrl Pts',(0.411353038798459,-1.,3.83503345578645));
#59272=CARTESIAN_POINT('Ctrl Pts',(0.411353038798459,1.,3.83503345578645));
#59273=CARTESIAN_POINT('Ctrl Pts',(0.413831367016726,-1.,3.84219403994742));
#59274=CARTESIAN_POINT('Ctrl Pts',(0.413831367016726,1.,3.84219403994742));
#59275=CARTESIAN_POINT('Ctrl Pts',(0.41636967805292,-1.,3.8493286415751));
#59276=CARTESIAN_POINT('Ctrl Pts',(0.41636967805292,1.,3.8493286415751));
#59277=CARTESIAN_POINT('Ctrl Pts',(0.418962468086809,-1.,3.85639825648031));
#59278=CARTESIAN_POINT('Ctrl Pts',(0.418962468086809,1.,3.85639825648031));
#59279=CARTESIAN_POINT('Ctrl Pts',(0.421607423177575,-1.,3.86339652542749));
#59280=CARTESIAN_POINT('Ctrl Pts',(0.421607423177575,1.,3.86339652542749));
#59281=CARTESIAN_POINT('Ctrl Pts',(0.424304173195142,-1.,3.87033643487882));
#59282=CARTESIAN_POINT('Ctrl Pts',(0.424304173195142,1.,3.87033643487882));
#59283=CARTESIAN_POINT('Ctrl Pts',(0.427053541173469,-1.,3.87724240306609));
#59284=CARTESIAN_POINT('Ctrl Pts',(0.427053541173469,1.,3.87724240306609));
#59285=CARTESIAN_POINT('Ctrl Pts',(0.429856640579733,-1.,3.88414070943334));
#59286=CARTESIAN_POINT('Ctrl Pts',(0.429856640579733,1.,3.88414070943334));
#59287=CARTESIAN_POINT('Ctrl Pts',(0.432713929544439,-1.,3.89104947940592));
#59288=CARTESIAN_POINT('Ctrl Pts',(0.432713929544439,1.,3.89104947940592));
#59289=CARTESIAN_POINT('Ctrl Pts',(0.435624629433505,-1.,3.8979725665544));
#59290=CARTESIAN_POINT('Ctrl Pts',(0.435624629433505,1.,3.8979725665544));
#59291=CARTESIAN_POINT('Ctrl Pts',(0.438587235458233,-1.,3.90490512938546));
#59292=CARTESIAN_POINT('Ctrl Pts',(0.438587235458233,1.,3.90490512938546));
#59293=CARTESIAN_POINT('Ctrl Pts',(0.441599824524047,-1.,3.91183704069146));
#59294=CARTESIAN_POINT('Ctrl Pts',(0.441599824524047,1.,3.91183704069146));
#59295=CARTESIAN_POINT('Ctrl Pts',(0.444660430230592,-1.,3.91875701610721));
#59296=CARTESIAN_POINT('Ctrl Pts',(0.444660430230592,1.,3.91875701610721));
#59297=CARTESIAN_POINT('Ctrl Pts',(0.447767416837296,-1.,3.92565674143424));
#59298=CARTESIAN_POINT('Ctrl Pts',(0.447767416837296,1.,3.92565674143424));
#59299=CARTESIAN_POINT('Ctrl Pts',(0.450919768356346,-1.,3.93253407403128));
#59300=CARTESIAN_POINT('Ctrl Pts',(0.450919768356346,1.,3.93253407403128));
#59301=CARTESIAN_POINT('Ctrl Pts',(0.454116879027575,-1.,3.93939080846298));
#59302=CARTESIAN_POINT('Ctrl Pts',(0.454116879027575,1.,3.93939080846298));
#59303=CARTESIAN_POINT('Ctrl Pts',(0.457358410451673,-1.,3.94623117206675));
#59304=CARTESIAN_POINT('Ctrl Pts',(0.457358410451673,1.,3.94623117206675));
#59305=CARTESIAN_POINT('Ctrl Pts',(0.460644124429119,-1.,3.95306005817363));
#59306=CARTESIAN_POINT('Ctrl Pts',(0.460644124429119,1.,3.95306005817363));
#59307=CARTESIAN_POINT('Ctrl Pts',(0.463973722115744,-1.,3.95988133243543));
#59308=CARTESIAN_POINT('Ctrl Pts',(0.463973722115744,1.,3.95988133243543));
#59309=CARTESIAN_POINT('Ctrl Pts',(0.467346690880671,-1.,3.96669622273946));
#59310=CARTESIAN_POINT('Ctrl Pts',(0.467346690880671,1.,3.96669622273946));
#59311=CARTESIAN_POINT('Ctrl Pts',(0.470762379613477,-1.,3.97350414289415));
#59312=CARTESIAN_POINT('Ctrl Pts',(0.470762379613477,1.,3.97350414289415));
#59313=CARTESIAN_POINT('Ctrl Pts',(0.474220061019542,-1.,3.9803033804443));
#59314=CARTESIAN_POINT('Ctrl Pts',(0.474220061019542,1.,3.9803033804443));
#59315=CARTESIAN_POINT('Ctrl Pts',(0.477718999122033,-1.,3.98709184306743));
#59316=CARTESIAN_POINT('Ctrl Pts',(0.477718999122033,1.,3.98709184306743));
#59317=CARTESIAN_POINT('Ctrl Pts',(0.481258512209637,-1.,3.99386775880655));
#59318=CARTESIAN_POINT('Ctrl Pts',(0.481258512209637,1.,3.99386775880655));
#59319=CARTESIAN_POINT('Ctrl Pts',(0.484838042421754,-1.,4.00063045119234));
#59320=CARTESIAN_POINT('Ctrl Pts',(0.484838042421754,1.,4.00063045119234));
#59321=CARTESIAN_POINT('Ctrl Pts',(0.48845713042453,-1.,4.0073800839092));
#59322=CARTESIAN_POINT('Ctrl Pts',(0.48845713042453,1.,4.0073800839092));
#59323=CARTESIAN_POINT('Ctrl Pts',(0.49211538341793,-1.,4.01411733503486));
#59324=CARTESIAN_POINT('Ctrl Pts',(0.49211538341793,1.,4.01411733503486));
#59325=CARTESIAN_POINT('Ctrl Pts',(0.495812444326222,-1.,4.02084308851813));
#59326=CARTESIAN_POINT('Ctrl Pts',(0.495812444326222,1.,4.02084308851813));
#59327=CARTESIAN_POINT('Ctrl Pts',(0.499547962340889,-1.,4.0275581398015));
#59328=CARTESIAN_POINT('Ctrl Pts',(0.499547962340889,1.,4.0275581398015));
#59329=CARTESIAN_POINT('Ctrl Pts',(0.503321556915513,-1.,4.0342628417439));
#59330=CARTESIAN_POINT('Ctrl Pts',(0.503321556915513,1.,4.0342628417439));
#59331=CARTESIAN_POINT('Ctrl Pts',(0.507132823288361,-1.,4.04095715149074));
#59332=CARTESIAN_POINT('Ctrl Pts',(0.507132823288361,1.,4.04095715149074));
#59333=CARTESIAN_POINT('Ctrl Pts',(0.510981349219173,-1.,4.04764078815591));
#59334=CARTESIAN_POINT('Ctrl Pts',(0.510981349219173,1.,4.04764078815591));
#59335=CARTESIAN_POINT('Ctrl Pts',(0.514866728193103,-1.,4.05431335771261));
#59336=CARTESIAN_POINT('Ctrl Pts',(0.514866728193103,1.,4.05431335771261));
#59337=CARTESIAN_POINT('Ctrl Pts',(0.518788572336809,-1.,4.06097448037934));
#59338=CARTESIAN_POINT('Ctrl Pts',(0.518788572336809,1.,4.06097448037934));
#59339=CARTESIAN_POINT('Ctrl Pts',(0.522746528602767,-1.,4.06762394471075));
#59340=CARTESIAN_POINT('Ctrl Pts',(0.522746528602767,1.,4.06762394471075));
#59341=CARTESIAN_POINT('Ctrl Pts',(0.526740277226999,-1.,4.07426172299496));
#59342=CARTESIAN_POINT('Ctrl Pts',(0.526740277226999,1.,4.07426172299496));
#59343=CARTESIAN_POINT('Ctrl Pts',(0.530769518728075,-1.,4.08088789536488));
#59344=CARTESIAN_POINT('Ctrl Pts',(0.530769518728075,1.,4.08088789536488));
#59345=CARTESIAN_POINT('Ctrl Pts',(0.534833963476999,-1.,4.08750259988693));
#59346=CARTESIAN_POINT('Ctrl Pts',(0.534833963476999,1.,4.08750259988693));
#59347=CARTESIAN_POINT('Ctrl Pts',(0.53893332117992,-1.,4.09410597627116));
#59348=CARTESIAN_POINT('Ctrl Pts',(0.53893332117992,1.,4.09410597627116));
#59349=CARTESIAN_POINT('Ctrl Pts',(0.543067286878457,-1.,4.10069810244473));
#59350=CARTESIAN_POINT('Ctrl Pts',(0.543067286878457,1.,4.10069810244473));
#59351=CARTESIAN_POINT('Ctrl Pts',(0.547235539486759,-1.,4.1072789702877));
#59352=CARTESIAN_POINT('Ctrl Pts',(0.547235539486759,1.,4.1072789702877));
#59353=CARTESIAN_POINT('Ctrl Pts',(0.551437758498246,-1.,4.11384852025578));
#59354=CARTESIAN_POINT('Ctrl Pts',(0.551437758498246,1.,4.11384852025578));
#59355=CARTESIAN_POINT('Ctrl Pts',(0.555673636130778,-1.,4.1204066619623));
#59356=CARTESIAN_POINT('Ctrl Pts',(0.555673636130778,1.,4.1204066619623));
#59357=CARTESIAN_POINT('Ctrl Pts',(0.559942890594628,-1.,4.12695329951859));
#59358=CARTESIAN_POINT('Ctrl Pts',(0.559942890594628,1.,4.12695329951859));
#59359=CARTESIAN_POINT('Ctrl Pts',(0.564245279535705,-1.,4.13348835726086));
#59360=CARTESIAN_POINT('Ctrl Pts',(0.564245279535705,1.,4.13348835726086));
#59361=CARTESIAN_POINT('Ctrl Pts',(0.568580610187115,-1.,4.14001179828669));
#59362=CARTESIAN_POINT('Ctrl Pts',(0.568580610187115,1.,4.14001179828669));
#59363=CARTESIAN_POINT('Ctrl Pts',(0.572948736066276,-1.,4.14652361065787));
#59364=CARTESIAN_POINT('Ctrl Pts',(0.572948736066276,1.,4.14652361065787));
#59365=CARTESIAN_POINT('Ctrl Pts',(0.576469391673916,-1.,4.1517237611974));
#59366=CARTESIAN_POINT('Ctrl Pts',(0.576469391673916,1.,4.1517237611974));
#59367=CARTESIAN_POINT('Ctrl Pts',(0.579124568912543,-1.,4.15561864787379));
#59368=CARTESIAN_POINT('Ctrl Pts',(0.579124568912543,1.,4.15561864787379));
#59369=CARTESIAN_POINT('Ctrl Pts',(0.580901211462913,-1.,4.15821291712391));
#59370=CARTESIAN_POINT('Ctrl Pts',(0.580901211462913,1.,4.15821291712391));
#59371=CARTESIAN_POINT('Ctrl Pts',(0.581791163835814,-1.,4.15950947128175));
#59372=CARTESIAN_POINT('Ctrl Pts',(0.581791163835814,1.,4.15950947128175));
#59373=CARTESIAN_POINT('',(0.385112848332548,1.,3.73017266276632));
#59374=CARTESIAN_POINT('Ctrl Pts',(0.385112848332548,-1.,3.73017266276632));
#59375=CARTESIAN_POINT('Ctrl Pts',(0.385112848332548,-0.666666666666667,
3.73017266276632));
#59376=CARTESIAN_POINT('Ctrl Pts',(0.385112848332548,-0.333333333333333,
3.73017266276632));
#59377=CARTESIAN_POINT('Ctrl Pts',(0.385112848332548,0.333333333333333,
3.73017266276632));
#59378=CARTESIAN_POINT('Ctrl Pts',(0.385112848332548,0.666666666666667,
3.73017266276632));
#59379=CARTESIAN_POINT('Ctrl Pts',(0.385112848332548,1.,3.73017266276632));
#59380=CARTESIAN_POINT('',(0.581791163835814,1.,4.15950947128175));
#59381=CARTESIAN_POINT('',(0.581791163835814,0.,4.15950947128175));
#59382=CARTESIAN_POINT('Ctrl Pts',(0.385112848332549,1.,3.73017266276632));
#59383=CARTESIAN_POINT('Ctrl Pts',(0.385087139001608,1.,3.73021431755218));
#59384=CARTESIAN_POINT('Ctrl Pts',(0.385037797882046,1.,3.73040527620929));
#59385=CARTESIAN_POINT('Ctrl Pts',(0.385031656499141,1.,3.731060828624));
#59386=CARTESIAN_POINT('Ctrl Pts',(0.385187124633964,1.,3.73273893363318));
#59387=CARTESIAN_POINT('Ctrl Pts',(0.385670806454744,1.,3.73621371845475));
#59388=CARTESIAN_POINT('Ctrl Pts',(0.386519576222035,1.,3.74144965781088));
#59389=CARTESIAN_POINT('Ctrl Pts',(0.387663020050396,1.,3.74792651696269));
#59390=CARTESIAN_POINT('Ctrl Pts',(0.38905477589825,1.,3.75529302894757));
#59391=CARTESIAN_POINT('Ctrl Pts',(0.390642072979258,1.,3.76315635032993));
#59392=CARTESIAN_POINT('Ctrl Pts',(0.392372786223346,1.,3.77114011595892));
#59393=CARTESIAN_POINT('Ctrl Pts',(0.394202481011595,1.,3.77894173114368));
#59394=CARTESIAN_POINT('Ctrl Pts',(0.396103205335028,1.,3.78640521279479));
#59395=CARTESIAN_POINT('Ctrl Pts',(0.398064818684158,1.,3.79352887163457));
#59396=CARTESIAN_POINT('Ctrl Pts',(0.400088346504726,1.,3.80040370384659));
#59397=CARTESIAN_POINT('Ctrl Pts',(0.402181320148474,1.,3.80716881962763));
#59398=CARTESIAN_POINT('Ctrl Pts',(0.404352694628236,1.,3.81396374287762));
#59399=CARTESIAN_POINT('Ctrl Pts',(0.406607038258906,1.,3.82087303913741));
#59400=CARTESIAN_POINT('Ctrl Pts',(0.408942371447376,1.,3.82790724256397));
#59401=CARTESIAN_POINT('Ctrl Pts',(0.411353038798459,1.,3.83503345578645));
#59402=CARTESIAN_POINT('Ctrl Pts',(0.413831367016726,1.,3.84219403994742));
#59403=CARTESIAN_POINT('Ctrl Pts',(0.41636967805292,1.,3.8493286415751));
#59404=CARTESIAN_POINT('Ctrl Pts',(0.418962468086809,1.,3.85639825648031));
#59405=CARTESIAN_POINT('Ctrl Pts',(0.421607423177575,1.,3.86339652542749));
#59406=CARTESIAN_POINT('Ctrl Pts',(0.424304173195142,1.,3.87033643487882));
#59407=CARTESIAN_POINT('Ctrl Pts',(0.427053541173469,1.,3.87724240306609));
#59408=CARTESIAN_POINT('Ctrl Pts',(0.429856640579733,1.,3.88414070943334));
#59409=CARTESIAN_POINT('Ctrl Pts',(0.432713929544439,1.,3.89104947940592));
#59410=CARTESIAN_POINT('Ctrl Pts',(0.435624629433505,1.,3.8979725665544));
#59411=CARTESIAN_POINT('Ctrl Pts',(0.438587235458233,1.,3.90490512938546));
#59412=CARTESIAN_POINT('Ctrl Pts',(0.441599824524047,1.,3.91183704069146));
#59413=CARTESIAN_POINT('Ctrl Pts',(0.444660430230592,1.,3.91875701610721));
#59414=CARTESIAN_POINT('Ctrl Pts',(0.447767416837296,1.,3.92565674143424));
#59415=CARTESIAN_POINT('Ctrl Pts',(0.450919768356346,1.,3.93253407403128));
#59416=CARTESIAN_POINT('Ctrl Pts',(0.454116879027575,1.,3.93939080846298));
#59417=CARTESIAN_POINT('Ctrl Pts',(0.457358410451673,1.,3.94623117206675));
#59418=CARTESIAN_POINT('Ctrl Pts',(0.460644124429119,1.,3.95306005817363));
#59419=CARTESIAN_POINT('Ctrl Pts',(0.463973722115744,1.,3.95988133243543));
#59420=CARTESIAN_POINT('Ctrl Pts',(0.467346690880671,1.,3.96669622273946));
#59421=CARTESIAN_POINT('Ctrl Pts',(0.470762379613477,1.,3.97350414289415));
#59422=CARTESIAN_POINT('Ctrl Pts',(0.474220061019542,1.,3.9803033804443));
#59423=CARTESIAN_POINT('Ctrl Pts',(0.477718999122033,1.,3.98709184306743));
#59424=CARTESIAN_POINT('Ctrl Pts',(0.481258512209637,1.,3.99386775880655));
#59425=CARTESIAN_POINT('Ctrl Pts',(0.484838042421754,1.,4.00063045119234));
#59426=CARTESIAN_POINT('Ctrl Pts',(0.48845713042453,1.,4.0073800839092));
#59427=CARTESIAN_POINT('Ctrl Pts',(0.49211538341793,1.,4.01411733503486));
#59428=CARTESIAN_POINT('Ctrl Pts',(0.495812444326222,1.,4.02084308851813));
#59429=CARTESIAN_POINT('Ctrl Pts',(0.499547962340889,1.,4.0275581398015));
#59430=CARTESIAN_POINT('Ctrl Pts',(0.503321556915513,1.,4.0342628417439));
#59431=CARTESIAN_POINT('Ctrl Pts',(0.507132823288361,1.,4.04095715149074));
#59432=CARTESIAN_POINT('Ctrl Pts',(0.510981349219173,1.,4.04764078815591));
#59433=CARTESIAN_POINT('Ctrl Pts',(0.514866728193103,1.,4.05431335771261));
#59434=CARTESIAN_POINT('Ctrl Pts',(0.518788572336809,1.,4.06097448037934));
#59435=CARTESIAN_POINT('Ctrl Pts',(0.522746528602767,1.,4.06762394471075));
#59436=CARTESIAN_POINT('Ctrl Pts',(0.526740277226999,1.,4.07426172299496));
#59437=CARTESIAN_POINT('Ctrl Pts',(0.530769518728075,1.,4.08088789536488));
#59438=CARTESIAN_POINT('Ctrl Pts',(0.534833963476999,1.,4.08750259988693));
#59439=CARTESIAN_POINT('Ctrl Pts',(0.53893332117992,1.,4.09410597627116));
#59440=CARTESIAN_POINT('Ctrl Pts',(0.543067286878457,1.,4.10069810244473));
#59441=CARTESIAN_POINT('Ctrl Pts',(0.547235539486759,1.,4.1072789702877));
#59442=CARTESIAN_POINT('Ctrl Pts',(0.551437758498246,1.,4.11384852025578));
#59443=CARTESIAN_POINT('Ctrl Pts',(0.555673636130778,1.,4.1204066619623));
#59444=CARTESIAN_POINT('Ctrl Pts',(0.559942890594628,1.,4.12695329951859));
#59445=CARTESIAN_POINT('Ctrl Pts',(0.564245279535705,1.,4.13348835726086));
#59446=CARTESIAN_POINT('Ctrl Pts',(0.568580610187115,1.,4.14001179828669));
#59447=CARTESIAN_POINT('Ctrl Pts',(0.572948736066276,1.,4.14652361065787));
#59448=CARTESIAN_POINT('Ctrl Pts',(0.576469391673916,1.,4.1517237611974));
#59449=CARTESIAN_POINT('Ctrl Pts',(0.579124568912543,1.,4.15561864787379));
#59450=CARTESIAN_POINT('Ctrl Pts',(0.580901211462913,1.,4.15821291712391));
#59451=CARTESIAN_POINT('Ctrl Pts',(0.581791163835814,1.,4.15950947128175));
#59452=CARTESIAN_POINT('Origin',(0.581791163835814,0.,4.15950947128175));
#59453=CARTESIAN_POINT('',(0.732042837400619,1.,4.13571194405636));
#59454=CARTESIAN_POINT('Origin',(0.,0.,0.));
#59455=CARTESIAN_POINT('',(0.203156094897895,1.,3.74449296982994));
#59456=CARTESIAN_POINT('Origin',(0.,1.,0.));
#59457=CARTESIAN_POINT('Ctrl Pts',(0.203156094897895,1.,3.74449296982994));
#59458=CARTESIAN_POINT('Ctrl Pts',(0.203156094897895,0.666666666666667,
3.74449296982994));
#59459=CARTESIAN_POINT('Ctrl Pts',(0.203156094897895,0.333333333333333,
3.74449296982994));
#59460=CARTESIAN_POINT('Ctrl Pts',(0.203156094897895,-0.333333333333333,
3.74449296982994));
#59461=CARTESIAN_POINT('Ctrl Pts',(0.203156094897895,-0.666666666666667,
3.74449296982994));
#59462=CARTESIAN_POINT('Ctrl Pts',(0.203156094897895,-1.,3.74449296982994));
#59463=CARTESIAN_POINT('Ctrl Pts',(0.0760622897878233,-1.,4.19931119685982));
#59464=CARTESIAN_POINT('Ctrl Pts',(0.0760622897878233,1.,4.19931119685982));
#59465=CARTESIAN_POINT('Ctrl Pts',(0.0767384596142192,-1.,4.19789138621624));
#59466=CARTESIAN_POINT('Ctrl Pts',(0.0767384596142192,1.,4.19789138621624));
#59467=CARTESIAN_POINT('Ctrl Pts',(0.0780873956244399,-1.,4.19505112860624));
#59468=CARTESIAN_POINT('Ctrl Pts',(0.0780873956244399,1.,4.19505112860624));
#59469=CARTESIAN_POINT('Ctrl Pts',(0.08010058871176,-1.,4.19078883322483));
#59470=CARTESIAN_POINT('Ctrl Pts',(0.08010058871176,1.,4.19078883322483));
#59471=CARTESIAN_POINT('Ctrl Pts',(0.0827644164389507,-1.,4.1851019532944));
#59472=CARTESIAN_POINT('Ctrl Pts',(0.0827644164389507,1.,4.1851019532944));
#59473=CARTESIAN_POINT('Ctrl Pts',(0.0860600915552512,-1.,4.17798698669991));
#59474=CARTESIAN_POINT('Ctrl Pts',(0.0860600915552512,1.,4.17798698669991));
#59475=CARTESIAN_POINT('Ctrl Pts',(0.0893215560850325,-1.,4.17086566491823));
#59476=CARTESIAN_POINT('Ctrl Pts',(0.0893215560850325,1.,4.17086566491823));
#59477=CARTESIAN_POINT('Ctrl Pts',(0.0925486672167687,-1.,4.16373802265942));
#59478=CARTESIAN_POINT('Ctrl Pts',(0.0925486672167687,1.,4.16373802265942));
#59479=CARTESIAN_POINT('Ctrl Pts',(0.0957412403297065,-1.,4.15660412653006));
#59480=CARTESIAN_POINT('Ctrl Pts',(0.0957412403297065,1.,4.15660412653006));
#59481=CARTESIAN_POINT('Ctrl Pts',(0.0988990478899809,-1.,4.1494640891762));
#59482=CARTESIAN_POINT('Ctrl Pts',(0.0988990478899809,1.,4.1494640891762));
#59483=CARTESIAN_POINT('Ctrl Pts',(0.102021826577453,-1.,4.14231804938737));
#59484=CARTESIAN_POINT('Ctrl Pts',(0.102021826577453,1.,4.14231804938737));
#59485=CARTESIAN_POINT('Ctrl Pts',(0.105109286538864,-1.,4.13516614458396));
#59486=CARTESIAN_POINT('Ctrl Pts',(0.105109286538864,1.,4.13516614458396));
#59487=CARTESIAN_POINT('Ctrl Pts',(0.10816112052835,-1.,4.12800848371386));
#59488=CARTESIAN_POINT('Ctrl Pts',(0.10816112052835,1.,4.12800848371386));
#59489=CARTESIAN_POINT('Ctrl Pts',(0.111177012683377,-1.,4.12084512502444));
#59490=CARTESIAN_POINT('Ctrl Pts',(0.111177012683377,1.,4.12084512502444));
#59491=CARTESIAN_POINT('Ctrl Pts',(0.114156649609601,-1.,4.11367603925313));
#59492=CARTESIAN_POINT('Ctrl Pts',(0.114156649609601,1.,4.11367603925313));
#59493=CARTESIAN_POINT('Ctrl Pts',(0.117099722731704,-1.,4.10650113382187));
#59494=CARTESIAN_POINT('Ctrl Pts',(0.117099722731704,1.,4.10650113382187));
#59495=CARTESIAN_POINT('Ctrl Pts',(0.120005924388162,-1.,4.09932031767243));
#59496=CARTESIAN_POINT('Ctrl Pts',(0.120005924388162,1.,4.09932031767243));
#59497=CARTESIAN_POINT('Ctrl Pts',(0.122874946249119,-1.,4.09213355850836));
#59498=CARTESIAN_POINT('Ctrl Pts',(0.122874946249119,1.,4.09213355850836));
#59499=CARTESIAN_POINT('Ctrl Pts',(0.125706476822529,-1.,4.08494093372315));
#59500=CARTESIAN_POINT('Ctrl Pts',(0.125706476822529,1.,4.08494093372315));
#59501=CARTESIAN_POINT('Ctrl Pts',(0.128500200484813,-1.,4.07774270738809));
#59502=CARTESIAN_POINT('Ctrl Pts',(0.128500200484813,1.,4.07774270738809));
#59503=CARTESIAN_POINT('Ctrl Pts',(0.131255793548914,-1.,4.07053931528579));
#59504=CARTESIAN_POINT('Ctrl Pts',(0.131255793548914,1.,4.07053931528579));
#59505=CARTESIAN_POINT('Ctrl Pts',(0.133972916144225,-1.,4.06333121018476));
#59506=CARTESIAN_POINT('Ctrl Pts',(0.133972916144225,1.,4.06333121018476));
#59507=CARTESIAN_POINT('Ctrl Pts',(0.136651205046111,-1.,4.05611873400122));
#59508=CARTESIAN_POINT('Ctrl Pts',(0.136651205046111,1.,4.05611873400122));
#59509=CARTESIAN_POINT('Ctrl Pts',(0.139290267180059,-1.,4.04890199238056));
#59510=CARTESIAN_POINT('Ctrl Pts',(0.139290267180059,1.,4.04890199238056));
#59511=CARTESIAN_POINT('Ctrl Pts',(0.141889671485507,-1.,4.04168069633842));
#59512=CARTESIAN_POINT('Ctrl Pts',(0.141889671485507,1.,4.04168069633842));
#59513=CARTESIAN_POINT('Ctrl Pts',(0.144448947038352,-1.,4.03445411510403));
#59514=CARTESIAN_POINT('Ctrl Pts',(0.144448947038352,1.,4.03445411510403));
#59515=CARTESIAN_POINT('Ctrl Pts',(0.146967602878998,-1.,4.02722143147048));
#59516=CARTESIAN_POINT('Ctrl Pts',(0.146967602878998,1.,4.02722143147048));
#59517=CARTESIAN_POINT('Ctrl Pts',(0.149445144968707,-1.,4.01998203715588));
#59518=CARTESIAN_POINT('Ctrl Pts',(0.149445144968707,1.,4.01998203715588));
#59519=CARTESIAN_POINT('Ctrl Pts',(0.151881094022909,-1.,4.01273584234684));
#59520=CARTESIAN_POINT('Ctrl Pts',(0.151881094022909,1.,4.01273584234684));
#59521=CARTESIAN_POINT('Ctrl Pts',(0.154275004872309,-1.,4.00548360245297));
#59522=CARTESIAN_POINT('Ctrl Pts',(0.154275004872309,1.,4.00548360245297));
#59523=CARTESIAN_POINT('Ctrl Pts',(0.156626481393735,-1.,3.99822717425869));
#59524=CARTESIAN_POINT('Ctrl Pts',(0.156626481393735,1.,3.99822717425869));
#59525=CARTESIAN_POINT('Ctrl Pts',(0.158935123982796,-1.,3.99096873945862));
#59526=CARTESIAN_POINT('Ctrl Pts',(0.158935123982796,1.,3.99096873945862));
#59527=CARTESIAN_POINT('Ctrl Pts',(0.161200482186087,-1.,3.98371010319866));
#59528=CARTESIAN_POINT('Ctrl Pts',(0.161200482186087,1.,3.98371010319866));
#59529=CARTESIAN_POINT('Ctrl Pts',(0.163422004609998,-1.,3.97645194630944));
#59530=CARTESIAN_POINT('Ctrl Pts',(0.163422004609998,1.,3.97645194630944));
#59531=CARTESIAN_POINT('Ctrl Pts',(0.165598992851097,-1.,3.9691931362141));
#59532=CARTESIAN_POINT('Ctrl Pts',(0.165598992851097,1.,3.9691931362141));
#59533=CARTESIAN_POINT('Ctrl Pts',(0.167730547023312,-1.,3.96192990160296));
#59534=CARTESIAN_POINT('Ctrl Pts',(0.167730547023312,1.,3.96192990160296));
#59535=CARTESIAN_POINT('Ctrl Pts',(0.16981566637413,-1.,3.95465744665263));
#59536=CARTESIAN_POINT('Ctrl Pts',(0.16981566637413,1.,3.95465744665263));
#59537=CARTESIAN_POINT('Ctrl Pts',(0.171853355369232,-1.,3.94737164900861));
#59538=CARTESIAN_POINT('Ctrl Pts',(0.171853355369232,1.,3.94737164900861));
#59539=CARTESIAN_POINT('Ctrl Pts',(0.173842734974607,-1.,3.94007083096214));
#59540=CARTESIAN_POINT('Ctrl Pts',(0.173842734974607,1.,3.94007083096214));
#59541=CARTESIAN_POINT('Ctrl Pts',(0.175783136893872,-1.,3.93275726771049));
#59542=CARTESIAN_POINT('Ctrl Pts',(0.175783136893872,1.,3.93275726771049));
#59543=CARTESIAN_POINT('Ctrl Pts',(0.177674246152328,-1.,3.92543942697672));
#59544=CARTESIAN_POINT('Ctrl Pts',(0.177674246152328,1.,3.92543942697672));
#59545=CARTESIAN_POINT('Ctrl Pts',(0.179515885822894,-1.,3.91812876180948));
#59546=CARTESIAN_POINT('Ctrl Pts',(0.179515885822894,1.,3.91812876180948));
#59547=CARTESIAN_POINT('Ctrl Pts',(0.181307740731795,-1.,3.91083557557193));
#59548=CARTESIAN_POINT('Ctrl Pts',(0.181307740731795,1.,3.91083557557193));
#59549=CARTESIAN_POINT('Ctrl Pts',(0.183049081993193,-1.,3.90356488555138));
#59550=CARTESIAN_POINT('Ctrl Pts',(0.183049081993193,1.,3.90356488555138));
#59551=CARTESIAN_POINT('Ctrl Pts',(0.184738537728034,-1.,3.89631300742633));
#59552=CARTESIAN_POINT('Ctrl Pts',(0.184738537728034,1.,3.89631300742633));
#59553=CARTESIAN_POINT('Ctrl Pts',(0.186373724985263,-1.,3.88906196725817));
#59554=CARTESIAN_POINT('Ctrl Pts',(0.186373724985263,1.,3.88906196725817));
#59555=CARTESIAN_POINT('Ctrl Pts',(0.187951632512663,-1.,3.88178563496187));
#59556=CARTESIAN_POINT('Ctrl Pts',(0.187951632512663,1.,3.88178563496187));
#59557=CARTESIAN_POINT('Ctrl Pts',(0.189469253358254,-1.,3.87445976418377));
#59558=CARTESIAN_POINT('Ctrl Pts',(0.189469253358254,1.,3.87445976418377));
#59559=CARTESIAN_POINT('Ctrl Pts',(0.190924190418612,-1.,3.8670715862477));
#59560=CARTESIAN_POINT('Ctrl Pts',(0.190924190418612,1.,3.8670715862477));
#59561=CARTESIAN_POINT('Ctrl Pts',(0.192315153044979,-1.,3.85962774407652));
#59562=CARTESIAN_POINT('Ctrl Pts',(0.192315153044979,1.,3.85962774407652));
#59563=CARTESIAN_POINT('Ctrl Pts',(0.193642806777747,-1.,3.85216762264019));
#59564=CARTESIAN_POINT('Ctrl Pts',(0.193642806777747,1.,3.85216762264019));
#59565=CARTESIAN_POINT('Ctrl Pts',(0.194909009460254,-1.,3.84475203347052));
#59566=CARTESIAN_POINT('Ctrl Pts',(0.194909009460254,1.,3.84475203347052));
#59567=CARTESIAN_POINT('Ctrl Pts',(0.196115198971889,-1.,3.83743910616265));
#59568=CARTESIAN_POINT('Ctrl Pts',(0.196115198971889,1.,3.83743910616265));
#59569=CARTESIAN_POINT('Ctrl Pts',(0.197260935827375,-1.,3.83026221776488));
#59570=CARTESIAN_POINT('Ctrl Pts',(0.197260935827375,1.,3.83026221776488));
#59571=CARTESIAN_POINT('Ctrl Pts',(0.198342616900469,-1.,3.82321127348981));
#59572=CARTESIAN_POINT('Ctrl Pts',(0.198342616900469,1.,3.82321127348981));
#59573=CARTESIAN_POINT('Ctrl Pts',(0.199351525297396,-1.,3.81620203429702));
#59574=CARTESIAN_POINT('Ctrl Pts',(0.199351525297396,1.,3.81620203429702));
#59575=CARTESIAN_POINT('Ctrl Pts',(0.200274679433289,-1.,3.80909529318501));
#59576=CARTESIAN_POINT('Ctrl Pts',(0.200274679433289,1.,3.80909529318501));
#59577=CARTESIAN_POINT('Ctrl Pts',(0.201097756307251,-1.,3.80175247447171));
#59578=CARTESIAN_POINT('Ctrl Pts',(0.201097756307251,1.,3.80175247447171));
#59579=CARTESIAN_POINT('Ctrl Pts',(0.201807533800798,-1.,3.79408354187274));
#59580=CARTESIAN_POINT('Ctrl Pts',(0.201807533800798,1.,3.79408354187274));
#59581=CARTESIAN_POINT('Ctrl Pts',(0.202394260512192,-1.,3.78609175019317));
#59582=CARTESIAN_POINT('Ctrl Pts',(0.202394260512192,1.,3.78609175019317));
#59583=CARTESIAN_POINT('Ctrl Pts',(0.202854729699196,-1.,3.77793553476879));
#59584=CARTESIAN_POINT('Ctrl Pts',(0.202854729699196,1.,3.77793553476879));
#59585=CARTESIAN_POINT('Ctrl Pts',(0.203192390045337,-1.,3.76992071595267));
#59586=CARTESIAN_POINT('Ctrl Pts',(0.203192390045337,1.,3.76992071595267));
#59587=CARTESIAN_POINT('Ctrl Pts',(0.203414634707646,-1.,3.76242717937273));
#59588=CARTESIAN_POINT('Ctrl Pts',(0.203414634707646,1.,3.76242717937273));
#59589=CARTESIAN_POINT('Ctrl Pts',(0.203530796848403,-1.,3.75585118707924));
#59590=CARTESIAN_POINT('Ctrl Pts',(0.203530796848403,1.,3.75585118707924));
#59591=CARTESIAN_POINT('Ctrl Pts',(0.203550035479096,-1.,3.75054693397716));
#59592=CARTESIAN_POINT('Ctrl Pts',(0.203550035479096,1.,3.75054693397716));
#59593=CARTESIAN_POINT('Ctrl Pts',(0.203478844530229,-1.,3.74675472018582));
#59594=CARTESIAN_POINT('Ctrl Pts',(0.203478844530229,1.,3.74675472018582));
#59595=CARTESIAN_POINT('Ctrl Pts',(0.203352057956055,-1.,3.7450208092684));
#59596=CARTESIAN_POINT('Ctrl Pts',(0.203352057956055,1.,3.7450208092684));
#59597=CARTESIAN_POINT('Ctrl Pts',(0.203218215747894,-1.,3.74446880195845));
#59598=CARTESIAN_POINT('Ctrl Pts',(0.203218215747894,1.,3.74446880195845));
#59599=CARTESIAN_POINT('Ctrl Pts',(0.20311176758786,-1.,3.74443319346666));
#59600=CARTESIAN_POINT('Ctrl Pts',(0.20311176758786,1.,3.74443319346666));
#59601=CARTESIAN_POINT('Ctrl Pts',(0.203054238699719,-1.,3.74449849461127));
#59602=CARTESIAN_POINT('Ctrl Pts',(0.203054238699719,1.,3.74449849461127));
#59603=CARTESIAN_POINT('',(0.0760622897878233,1.,4.19931119685982));
#59604=CARTESIAN_POINT('Ctrl Pts',(0.0760622897878233,1.,4.19931119685982));
#59605=CARTESIAN_POINT('Ctrl Pts',(0.0767384596142192,1.,4.19789138621624));
#59606=CARTESIAN_POINT('Ctrl Pts',(0.0780873956244399,1.,4.19505112860624));
#59607=CARTESIAN_POINT('Ctrl Pts',(0.08010058871176,1.,4.19078883322483));
#59608=CARTESIAN_POINT('Ctrl Pts',(0.0827644164389507,1.,4.1851019532944));
#59609=CARTESIAN_POINT('Ctrl Pts',(0.0860600915552512,1.,4.17798698669991));
#59610=CARTESIAN_POINT('Ctrl Pts',(0.0893215560850325,1.,4.17086566491823));
#59611=CARTESIAN_POINT('Ctrl Pts',(0.0925486672167687,1.,4.16373802265942));
#59612=CARTESIAN_POINT('Ctrl Pts',(0.0957412403297065,1.,4.15660412653006));
#59613=CARTESIAN_POINT('Ctrl Pts',(0.0988990478899809,1.,4.1494640891762));
#59614=CARTESIAN_POINT('Ctrl Pts',(0.102021826577453,1.,4.14231804938737));
#59615=CARTESIAN_POINT('Ctrl Pts',(0.105109286538864,1.,4.13516614458396));
#59616=CARTESIAN_POINT('Ctrl Pts',(0.10816112052835,1.,4.12800848371386));
#59617=CARTESIAN_POINT('Ctrl Pts',(0.111177012683377,1.,4.12084512502444));
#59618=CARTESIAN_POINT('Ctrl Pts',(0.114156649609601,1.,4.11367603925313));
#59619=CARTESIAN_POINT('Ctrl Pts',(0.117099722731704,1.,4.10650113382187));
#59620=CARTESIAN_POINT('Ctrl Pts',(0.120005924388162,1.,4.09932031767243));
#59621=CARTESIAN_POINT('Ctrl Pts',(0.122874946249119,1.,4.09213355850836));
#59622=CARTESIAN_POINT('Ctrl Pts',(0.125706476822529,1.,4.08494093372315));
#59623=CARTESIAN_POINT('Ctrl Pts',(0.128500200484813,1.,4.07774270738809));
#59624=CARTESIAN_POINT('Ctrl Pts',(0.131255793548914,1.,4.07053931528579));
#59625=CARTESIAN_POINT('Ctrl Pts',(0.133972916144225,1.,4.06333121018476));
#59626=CARTESIAN_POINT('Ctrl Pts',(0.136651205046111,1.,4.05611873400122));
#59627=CARTESIAN_POINT('Ctrl Pts',(0.139290267180059,1.,4.04890199238056));
#59628=CARTESIAN_POINT('Ctrl Pts',(0.141889671485507,1.,4.04168069633842));
#59629=CARTESIAN_POINT('Ctrl Pts',(0.144448947038352,1.,4.03445411510403));
#59630=CARTESIAN_POINT('Ctrl Pts',(0.146967602878998,1.,4.02722143147048));
#59631=CARTESIAN_POINT('Ctrl Pts',(0.149445144968707,1.,4.01998203715588));
#59632=CARTESIAN_POINT('Ctrl Pts',(0.151881094022909,1.,4.01273584234684));
#59633=CARTESIAN_POINT('Ctrl Pts',(0.154275004872309,1.,4.00548360245297));
#59634=CARTESIAN_POINT('Ctrl Pts',(0.156626481393735,1.,3.99822717425869));
#59635=CARTESIAN_POINT('Ctrl Pts',(0.158935123982796,1.,3.99096873945862));
#59636=CARTESIAN_POINT('Ctrl Pts',(0.161200482186087,1.,3.98371010319866));
#59637=CARTESIAN_POINT('Ctrl Pts',(0.163422004609998,1.,3.97645194630944));
#59638=CARTESIAN_POINT('Ctrl Pts',(0.165598992851097,1.,3.9691931362141));
#59639=CARTESIAN_POINT('Ctrl Pts',(0.167730547023312,1.,3.96192990160296));
#59640=CARTESIAN_POINT('Ctrl Pts',(0.16981566637413,1.,3.95465744665263));
#59641=CARTESIAN_POINT('Ctrl Pts',(0.171853355369232,1.,3.94737164900861));
#59642=CARTESIAN_POINT('Ctrl Pts',(0.173842734974607,1.,3.94007083096214));
#59643=CARTESIAN_POINT('Ctrl Pts',(0.175783136893872,1.,3.93275726771049));
#59644=CARTESIAN_POINT('Ctrl Pts',(0.177674246152328,1.,3.92543942697672));
#59645=CARTESIAN_POINT('Ctrl Pts',(0.179515885822894,1.,3.91812876180948));
#59646=CARTESIAN_POINT('Ctrl Pts',(0.181307740731795,1.,3.91083557557193));
#59647=CARTESIAN_POINT('Ctrl Pts',(0.183049081993193,1.,3.90356488555138));
#59648=CARTESIAN_POINT('Ctrl Pts',(0.184738537728034,1.,3.89631300742633));
#59649=CARTESIAN_POINT('Ctrl Pts',(0.186373724985263,1.,3.88906196725817));
#59650=CARTESIAN_POINT('Ctrl Pts',(0.187951632512663,1.,3.88178563496187));
#59651=CARTESIAN_POINT('Ctrl Pts',(0.189469253358254,1.,3.87445976418377));
#59652=CARTESIAN_POINT('Ctrl Pts',(0.190924190418612,1.,3.8670715862477));
#59653=CARTESIAN_POINT('Ctrl Pts',(0.192315153044979,1.,3.85962774407652));
#59654=CARTESIAN_POINT('Ctrl Pts',(0.193642806777747,1.,3.85216762264019));
#59655=CARTESIAN_POINT('Ctrl Pts',(0.194909009460254,1.,3.84475203347052));
#59656=CARTESIAN_POINT('Ctrl Pts',(0.196115198971889,1.,3.83743910616265));
#59657=CARTESIAN_POINT('Ctrl Pts',(0.197260935827375,1.,3.83026221776488));
#59658=CARTESIAN_POINT('Ctrl Pts',(0.198342616900469,1.,3.82321127348981));
#59659=CARTESIAN_POINT('Ctrl Pts',(0.199351525297396,1.,3.81620203429702));
#59660=CARTESIAN_POINT('Ctrl Pts',(0.200274679433289,1.,3.80909529318501));
#59661=CARTESIAN_POINT('Ctrl Pts',(0.201097756307251,1.,3.80175247447171));
#59662=CARTESIAN_POINT('Ctrl Pts',(0.201807533800798,1.,3.79408354187274));
#59663=CARTESIAN_POINT('Ctrl Pts',(0.202394260512192,1.,3.78609175019317));
#59664=CARTESIAN_POINT('Ctrl Pts',(0.202854729699196,1.,3.77793553476879));
#59665=CARTESIAN_POINT('Ctrl Pts',(0.203192390045337,1.,3.76992071595267));
#59666=CARTESIAN_POINT('Ctrl Pts',(0.203414634707646,1.,3.76242717937273));
#59667=CARTESIAN_POINT('Ctrl Pts',(0.203530796848403,1.,3.75585118707924));
#59668=CARTESIAN_POINT('Ctrl Pts',(0.203550035479096,1.,3.75054693397716));
#59669=CARTESIAN_POINT('Ctrl Pts',(0.203484186269314,1.,3.74703926501843));
#59670=CARTESIAN_POINT('Ctrl Pts',(0.203375226874331,1.,3.74535749969262));
#59671=CARTESIAN_POINT('Ctrl Pts',(0.203266610111263,1.,3.74471097893961));
#59672=CARTESIAN_POINT('Ctrl Pts',(0.203188003947964,1.,3.74453008995129));
#59673=CARTESIAN_POINT('Ctrl Pts',(0.203156094897895,1.,3.74449296982994));
#59674=CARTESIAN_POINT('',(0.0760622897878233,0.,4.19931119685982));
#59675=CARTESIAN_POINT('Ctrl Pts',(-0.20305423869972,-1.,3.74449849461127));
#59676=CARTESIAN_POINT('Ctrl Pts',(-0.20305423869972,1.,3.74449849461127));
#59677=CARTESIAN_POINT('Ctrl Pts',(-0.203111767587923,-1.,3.7444331934681));
#59678=CARTESIAN_POINT('Ctrl Pts',(-0.203111767587923,1.,3.7444331934681));
#59679=CARTESIAN_POINT('Ctrl Pts',(-0.203218215748059,-1.,3.7444688019622));
#59680=CARTESIAN_POINT('Ctrl Pts',(-0.203218215748059,1.,3.7444688019622));
#59681=CARTESIAN_POINT('Ctrl Pts',(-0.203352057956297,-1.,3.74502080927395));
#59682=CARTESIAN_POINT('Ctrl Pts',(-0.203352057956297,1.,3.74502080927395));
#59683=CARTESIAN_POINT('Ctrl Pts',(-0.203478844530447,-1.,3.7467547201908));
#59684=CARTESIAN_POINT('Ctrl Pts',(-0.203478844530447,1.,3.7467547201908));
#59685=CARTESIAN_POINT('Ctrl Pts',(-0.203550035479166,-1.,3.75054693397875));
#59686=CARTESIAN_POINT('Ctrl Pts',(-0.203550035479166,1.,3.75054693397875));
#59687=CARTESIAN_POINT('Ctrl Pts',(-0.203530796848322,-1.,3.75585118707734));
#59688=CARTESIAN_POINT('Ctrl Pts',(-0.203530796848322,1.,3.75585118707734));
#59689=CARTESIAN_POINT('Ctrl Pts',(-0.203414634707479,-1.,3.76242717936885));
#59690=CARTESIAN_POINT('Ctrl Pts',(-0.203414634707479,1.,3.76242717936885));
#59691=CARTESIAN_POINT('Ctrl Pts',(-0.203192390045165,-1.,3.7699207159487));
#59692=CARTESIAN_POINT('Ctrl Pts',(-0.203192390045165,1.,3.7699207159487));
#59693=CARTESIAN_POINT('Ctrl Pts',(-0.202854729699081,-1.,3.77793553476614));
#59694=CARTESIAN_POINT('Ctrl Pts',(-0.202854729699081,1.,3.77793553476614));
#59695=CARTESIAN_POINT('Ctrl Pts',(-0.20239426051216,-1.,3.78609175019242));
#59696=CARTESIAN_POINT('Ctrl Pts',(-0.20239426051216,1.,3.78609175019242));
#59697=CARTESIAN_POINT('Ctrl Pts',(-0.201807533800837,-1.,3.7940835418736));
#59698=CARTESIAN_POINT('Ctrl Pts',(-0.201807533800837,1.,3.7940835418736));
#59699=CARTESIAN_POINT('Ctrl Pts',(-0.201097756307326,-1.,3.80175247447337));
#59700=CARTESIAN_POINT('Ctrl Pts',(-0.201097756307326,1.,3.80175247447337));
#59701=CARTESIAN_POINT('Ctrl Pts',(-0.200274679433365,-1.,3.80909529318669));
#59702=CARTESIAN_POINT('Ctrl Pts',(-0.200274679433365,1.,3.80909529318669));
#59703=CARTESIAN_POINT('Ctrl Pts',(-0.199351525297447,-1.,3.81620203429815));
#59704=CARTESIAN_POINT('Ctrl Pts',(-0.199351525297447,1.,3.81620203429815));
#59705=CARTESIAN_POINT('Ctrl Pts',(-0.198342616900487,-1.,3.82321127349016));
#59706=CARTESIAN_POINT('Ctrl Pts',(-0.198342616900487,1.,3.82321127349016));
#59707=CARTESIAN_POINT('Ctrl Pts',(-0.197260935827362,-1.,3.83026221776456));
#59708=CARTESIAN_POINT('Ctrl Pts',(-0.197260935827362,1.,3.83026221776456));
#59709=CARTESIAN_POINT('Ctrl Pts',(-0.196115198971859,-1.,3.83743910616195));
#59710=CARTESIAN_POINT('Ctrl Pts',(-0.196115198971859,1.,3.83743910616195));
#59711=CARTESIAN_POINT('Ctrl Pts',(-0.194909009460221,-1.,3.84475203346977));
#59712=CARTESIAN_POINT('Ctrl Pts',(-0.194909009460221,1.,3.84475203346977));
#59713=CARTESIAN_POINT('Ctrl Pts',(-0.193642806777723,-1.,3.85216762263966));
#59714=CARTESIAN_POINT('Ctrl Pts',(-0.193642806777723,1.,3.85216762263966));
#59715=CARTESIAN_POINT('Ctrl Pts',(-0.192315153044971,-1.,3.85962774407633));
#59716=CARTESIAN_POINT('Ctrl Pts',(-0.192315153044971,1.,3.85962774407633));
#59717=CARTESIAN_POINT('Ctrl Pts',(-0.19092419041862,-1.,3.86707158624783));
#59718=CARTESIAN_POINT('Ctrl Pts',(-0.19092419041862,1.,3.86707158624783));
#59719=CARTESIAN_POINT('Ctrl Pts',(-0.189469253358273,-1.,3.87445976418412));
#59720=CARTESIAN_POINT('Ctrl Pts',(-0.189469253358273,1.,3.87445976418412));
#59721=CARTESIAN_POINT('Ctrl Pts',(-0.187951632512685,-1.,3.88178563496228));
#59722=CARTESIAN_POINT('Ctrl Pts',(-0.187951632512685,1.,3.88178563496228));
#59723=CARTESIAN_POINT('Ctrl Pts',(-0.186373724985281,-1.,3.88906196725848));
#59724=CARTESIAN_POINT('Ctrl Pts',(-0.186373724985281,1.,3.88906196725848));
#59725=CARTESIAN_POINT('Ctrl Pts',(-0.184738537728043,-1.,3.89631300742646));
#59726=CARTESIAN_POINT('Ctrl Pts',(-0.184738537728043,1.,3.89631300742646));
#59727=CARTESIAN_POINT('Ctrl Pts',(-0.183049081993191,-1.,3.90356488555132));
#59728=CARTESIAN_POINT('Ctrl Pts',(-0.183049081993191,1.,3.90356488555132));
#59729=CARTESIAN_POINT('Ctrl Pts',(-0.181307740731786,-1.,3.91083557557175));
#59730=CARTESIAN_POINT('Ctrl Pts',(-0.181307740731786,1.,3.91083557557175));
#59731=CARTESIAN_POINT('Ctrl Pts',(-0.179515885822882,-1.,3.91812876180926));
#59732=CARTESIAN_POINT('Ctrl Pts',(-0.179515885822882,1.,3.91812876180926));
#59733=CARTESIAN_POINT('Ctrl Pts',(-0.177674246152318,-1.,3.92543942697655));
#59734=CARTESIAN_POINT('Ctrl Pts',(-0.177674246152318,1.,3.92543942697655));
#59735=CARTESIAN_POINT('Ctrl Pts',(-0.175783136893868,-1.,3.93275726771042));
#59736=CARTESIAN_POINT('Ctrl Pts',(-0.175783136893868,1.,3.93275726771042));
#59737=CARTESIAN_POINT('Ctrl Pts',(-0.17384273497461,-1.,3.94007083096217));
#59738=CARTESIAN_POINT('Ctrl Pts',(-0.17384273497461,1.,3.94007083096217));
#59739=CARTESIAN_POINT('Ctrl Pts',(-0.17185335536924,-1.,3.94737164900868));
#59740=CARTESIAN_POINT('Ctrl Pts',(-0.17185335536924,1.,3.94737164900868));
#59741=CARTESIAN_POINT('Ctrl Pts',(-0.169815666374139,-1.,3.95465744665268));
#59742=CARTESIAN_POINT('Ctrl Pts',(-0.169815666374139,1.,3.95465744665268));
#59743=CARTESIAN_POINT('Ctrl Pts',(-0.16773054702332,-1.,3.96192990160296));
#59744=CARTESIAN_POINT('Ctrl Pts',(-0.16773054702332,1.,3.96192990160296));
#59745=CARTESIAN_POINT('Ctrl Pts',(-0.165598992851102,-1.,3.96919313621407));
#59746=CARTESIAN_POINT('Ctrl Pts',(-0.165598992851102,1.,3.96919313621407));
#59747=CARTESIAN_POINT('Ctrl Pts',(-0.163422004609999,-1.,3.97645194630943));
#59748=CARTESIAN_POINT('Ctrl Pts',(-0.163422004609999,1.,3.97645194630943));
#59749=CARTESIAN_POINT('Ctrl Pts',(-0.161200482186085,-1.,3.98371010319872));
#59750=CARTESIAN_POINT('Ctrl Pts',(-0.161200482186085,1.,3.98371010319872));
#59751=CARTESIAN_POINT('Ctrl Pts',(-0.158935123982793,-1.,3.99096873945878));
#59752=CARTESIAN_POINT('Ctrl Pts',(-0.158935123982793,1.,3.99096873945878));
#59753=CARTESIAN_POINT('Ctrl Pts',(-0.156626481393734,-1.,3.99822717425893));
#59754=CARTESIAN_POINT('Ctrl Pts',(-0.156626481393734,1.,3.99822717425893));
#59755=CARTESIAN_POINT('Ctrl Pts',(-0.154275004872311,-1.,4.00548360245319));
#59756=CARTESIAN_POINT('Ctrl Pts',(-0.154275004872311,1.,4.00548360245319));
#59757=CARTESIAN_POINT('Ctrl Pts',(-0.151881094022911,-1.,4.01273584234689));
#59758=CARTESIAN_POINT('Ctrl Pts',(-0.151881094022911,1.,4.01273584234689));
#59759=CARTESIAN_POINT('Ctrl Pts',(-0.149445144968707,-1.,4.01998203715564));
#59760=CARTESIAN_POINT('Ctrl Pts',(-0.149445144968707,1.,4.01998203715564));
#59761=CARTESIAN_POINT('Ctrl Pts',(-0.146967602878994,-1.,4.02722143146994));
#59762=CARTESIAN_POINT('Ctrl Pts',(-0.146967602878994,1.,4.02722143146994));
#59763=CARTESIAN_POINT('Ctrl Pts',(-0.144448947038345,-1.,4.03445411510333));
#59764=CARTESIAN_POINT('Ctrl Pts',(-0.144448947038345,1.,4.03445411510333));
#59765=CARTESIAN_POINT('Ctrl Pts',(-0.1418896714855,-1.,4.04168069633781));
#59766=CARTESIAN_POINT('Ctrl Pts',(-0.1418896714855,1.,4.04168069633781));
#59767=CARTESIAN_POINT('Ctrl Pts',(-0.139290267180057,-1.,4.04890199238036));
#59768=CARTESIAN_POINT('Ctrl Pts',(-0.139290267180057,1.,4.04890199238036));
#59769=CARTESIAN_POINT('Ctrl Pts',(-0.136651205046119,-1.,4.05611873400172));
#59770=CARTESIAN_POINT('Ctrl Pts',(-0.136651205046119,1.,4.05611873400172));
#59771=CARTESIAN_POINT('Ctrl Pts',(-0.133972916144245,-1.,4.06333121018596));
#59772=CARTESIAN_POINT('Ctrl Pts',(-0.133972916144245,1.,4.06333121018596));
#59773=CARTESIAN_POINT('Ctrl Pts',(-0.131255793548941,-1.,4.0705393152874));
#59774=CARTESIAN_POINT('Ctrl Pts',(-0.131255793548941,1.,4.0705393152874));
#59775=CARTESIAN_POINT('Ctrl Pts',(-0.128500200484838,-1.,4.07774270738954));
#59776=CARTESIAN_POINT('Ctrl Pts',(-0.128500200484838,1.,4.07774270738954));
#59777=CARTESIAN_POINT('Ctrl Pts',(-0.12570647682254,-1.,4.08494093372377));
#59778=CARTESIAN_POINT('Ctrl Pts',(-0.12570647682254,1.,4.08494093372377));
#59779=CARTESIAN_POINT('Ctrl Pts',(-0.122874946249107,-1.,4.09213355850756));
#59780=CARTESIAN_POINT('Ctrl Pts',(-0.122874946249107,1.,4.09213355850756));
#59781=CARTESIAN_POINT('Ctrl Pts',(-0.120005924388124,-1.,4.09932031767002));
#59782=CARTESIAN_POINT('Ctrl Pts',(-0.120005924388124,1.,4.09932031767002));
#59783=CARTESIAN_POINT('Ctrl Pts',(-0.117099722731648,-1.,4.10650113381833));
#59784=CARTESIAN_POINT('Ctrl Pts',(-0.117099722731648,1.,4.10650113381833));
#59785=CARTESIAN_POINT('Ctrl Pts',(-0.114156649609546,-1.,4.11367603924961));
#59786=CARTESIAN_POINT('Ctrl Pts',(-0.114156649609546,1.,4.11367603924961));
#59787=CARTESIAN_POINT('Ctrl Pts',(-0.111177012683347,-1.,4.1208451250225));
#59788=CARTESIAN_POINT('Ctrl Pts',(-0.111177012683347,1.,4.1208451250225));
#59789=CARTESIAN_POINT('Ctrl Pts',(-0.10816112052837,-1.,4.12800848371504));
#59790=CARTESIAN_POINT('Ctrl Pts',(-0.10816112052837,1.,4.12800848371504));
#59791=CARTESIAN_POINT('Ctrl Pts',(-0.105109286538945,-1.,4.13516614458895));
#59792=CARTESIAN_POINT('Ctrl Pts',(-0.105109286538945,1.,4.13516614458895));
#59793=CARTESIAN_POINT('Ctrl Pts',(-0.102021826577584,-1.,4.14231804939538));
#59794=CARTESIAN_POINT('Ctrl Pts',(-0.102021826577584,1.,4.14231804939538));
#59795=CARTESIAN_POINT('Ctrl Pts',(-0.0988990478901228,-1.,4.14946408918485));
#59796=CARTESIAN_POINT('Ctrl Pts',(-0.0988990478901228,1.,4.14946408918485));
#59797=CARTESIAN_POINT('Ctrl Pts',(-0.0957412403298009,-1.,4.15660412653577));
#59798=CARTESIAN_POINT('Ctrl Pts',(-0.0957412403298009,1.,4.15660412653577));
#59799=CARTESIAN_POINT('Ctrl Pts',(-0.0925486672167534,-1.,4.16373802265839));
#59800=CARTESIAN_POINT('Ctrl Pts',(-0.0925486672167534,1.,4.16373802265839));
#59801=CARTESIAN_POINT('Ctrl Pts',(-0.0893215560848652,-1.,4.17086566490794));
#59802=CARTESIAN_POINT('Ctrl Pts',(-0.0893215560848652,1.,4.17086566490794));
#59803=CARTESIAN_POINT('Ctrl Pts',(-0.0860600915549399,-1.,4.17798698668094));
#59804=CARTESIAN_POINT('Ctrl Pts',(-0.0860600915549399,1.,4.17798698668094));
#59805=CARTESIAN_POINT('Ctrl Pts',(-0.0827644164385681,-1.,4.18510195327123));
#59806=CARTESIAN_POINT('Ctrl Pts',(-0.0827644164385681,1.,4.18510195327123));
#59807=CARTESIAN_POINT('Ctrl Pts',(-0.0801005887114322,-1.,4.19078883320504));
#59808=CARTESIAN_POINT('Ctrl Pts',(-0.0801005887114322,1.,4.19078883320504));
#59809=CARTESIAN_POINT('Ctrl Pts',(-0.07808739562424,-1.,4.19505112859416));
#59810=CARTESIAN_POINT('Ctrl Pts',(-0.07808739562424,1.,4.19505112859416));
#59811=CARTESIAN_POINT('Ctrl Pts',(-0.0767384596141467,-1.,4.1978913862118));
#59812=CARTESIAN_POINT('Ctrl Pts',(-0.0767384596141467,1.,4.1978913862118));
#59813=CARTESIAN_POINT('Ctrl Pts',(-0.0760622897878249,-1.,4.19931119685982));
#59814=CARTESIAN_POINT('Ctrl Pts',(-0.0760622897878249,1.,4.19931119685982));
#59815=CARTESIAN_POINT('',(-0.203156094896102,1.,3.74449296983004));
#59816=CARTESIAN_POINT('Ctrl Pts',(-0.203156094896101,-1.,3.74449296983004));
#59817=CARTESIAN_POINT('Ctrl Pts',(-0.203156094896101,-0.666666666666667,
3.74449296983004));
#59818=CARTESIAN_POINT('Ctrl Pts',(-0.203156094896101,-0.333333333333333,
3.74449296983004));
#59819=CARTESIAN_POINT('Ctrl Pts',(-0.203156094896101,0.333333333333333,
3.74449296983004));
#59820=CARTESIAN_POINT('Ctrl Pts',(-0.203156094896101,0.666666666666667,
3.74449296983004));
#59821=CARTESIAN_POINT('Ctrl Pts',(-0.203156094896101,1.,3.74449296983004));
#59822=CARTESIAN_POINT('',(-0.0760622897878249,1.,4.19931119685982));
#59823=CARTESIAN_POINT('',(-0.0760622897878249,0.,4.19931119685982));
#59824=CARTESIAN_POINT('Ctrl Pts',(-0.203156094896101,1.,3.74449296983004));
#59825=CARTESIAN_POINT('Ctrl Pts',(-0.203188003946657,1.,3.74453008995092));
#59826=CARTESIAN_POINT('Ctrl Pts',(-0.203266610110531,1.,3.74471097893845));
#59827=CARTESIAN_POINT('Ctrl Pts',(-0.203375226874122,1.,3.74535749969115));
#59828=CARTESIAN_POINT('Ctrl Pts',(-0.203484186269415,1.,3.74703926501752));
#59829=CARTESIAN_POINT('Ctrl Pts',(-0.203550035479166,1.,3.75054693397875));
#59830=CARTESIAN_POINT('Ctrl Pts',(-0.203530796848322,1.,3.75585118707734));
#59831=CARTESIAN_POINT('Ctrl Pts',(-0.203414634707479,1.,3.76242717936885));
#59832=CARTESIAN_POINT('Ctrl Pts',(-0.203192390045165,1.,3.7699207159487));
#59833=CARTESIAN_POINT('Ctrl Pts',(-0.202854729699081,1.,3.77793553476614));
#59834=CARTESIAN_POINT('Ctrl Pts',(-0.20239426051216,1.,3.78609175019242));
#59835=CARTESIAN_POINT('Ctrl Pts',(-0.201807533800837,1.,3.7940835418736));
#59836=CARTESIAN_POINT('Ctrl Pts',(-0.201097756307326,1.,3.80175247447337));
#59837=CARTESIAN_POINT('Ctrl Pts',(-0.200274679433365,1.,3.80909529318669));
#59838=CARTESIAN_POINT('Ctrl Pts',(-0.199351525297447,1.,3.81620203429815));
#59839=CARTESIAN_POINT('Ctrl Pts',(-0.198342616900487,1.,3.82321127349016));
#59840=CARTESIAN_POINT('Ctrl Pts',(-0.197260935827362,1.,3.83026221776456));
#59841=CARTESIAN_POINT('Ctrl Pts',(-0.196115198971859,1.,3.83743910616195));
#59842=CARTESIAN_POINT('Ctrl Pts',(-0.194909009460221,1.,3.84475203346977));
#59843=CARTESIAN_POINT('Ctrl Pts',(-0.193642806777723,1.,3.85216762263966));
#59844=CARTESIAN_POINT('Ctrl Pts',(-0.192315153044971,1.,3.85962774407633));
#59845=CARTESIAN_POINT('Ctrl Pts',(-0.19092419041862,1.,3.86707158624783));
#59846=CARTESIAN_POINT('Ctrl Pts',(-0.189469253358273,1.,3.87445976418412));
#59847=CARTESIAN_POINT('Ctrl Pts',(-0.187951632512685,1.,3.88178563496228));
#59848=CARTESIAN_POINT('Ctrl Pts',(-0.186373724985281,1.,3.88906196725848));
#59849=CARTESIAN_POINT('Ctrl Pts',(-0.184738537728043,1.,3.89631300742646));
#59850=CARTESIAN_POINT('Ctrl Pts',(-0.183049081993191,1.,3.90356488555132));
#59851=CARTESIAN_POINT('Ctrl Pts',(-0.181307740731786,1.,3.91083557557175));
#59852=CARTESIAN_POINT('Ctrl Pts',(-0.179515885822882,1.,3.91812876180926));
#59853=CARTESIAN_POINT('Ctrl Pts',(-0.177674246152318,1.,3.92543942697655));
#59854=CARTESIAN_POINT('Ctrl Pts',(-0.175783136893868,1.,3.93275726771042));
#59855=CARTESIAN_POINT('Ctrl Pts',(-0.17384273497461,1.,3.94007083096217));
#59856=CARTESIAN_POINT('Ctrl Pts',(-0.17185335536924,1.,3.94737164900868));
#59857=CARTESIAN_POINT('Ctrl Pts',(-0.169815666374139,1.,3.95465744665268));
#59858=CARTESIAN_POINT('Ctrl Pts',(-0.16773054702332,1.,3.96192990160296));
#59859=CARTESIAN_POINT('Ctrl Pts',(-0.165598992851102,1.,3.96919313621407));
#59860=CARTESIAN_POINT('Ctrl Pts',(-0.163422004609999,1.,3.97645194630943));
#59861=CARTESIAN_POINT('Ctrl Pts',(-0.161200482186085,1.,3.98371010319872));
#59862=CARTESIAN_POINT('Ctrl Pts',(-0.158935123982793,1.,3.99096873945878));
#59863=CARTESIAN_POINT('Ctrl Pts',(-0.156626481393734,1.,3.99822717425893));
#59864=CARTESIAN_POINT('Ctrl Pts',(-0.154275004872311,1.,4.00548360245319));
#59865=CARTESIAN_POINT('Ctrl Pts',(-0.151881094022911,1.,4.01273584234689));
#59866=CARTESIAN_POINT('Ctrl Pts',(-0.149445144968707,1.,4.01998203715564));
#59867=CARTESIAN_POINT('Ctrl Pts',(-0.146967602878994,1.,4.02722143146994));
#59868=CARTESIAN_POINT('Ctrl Pts',(-0.144448947038345,1.,4.03445411510333));
#59869=CARTESIAN_POINT('Ctrl Pts',(-0.1418896714855,1.,4.04168069633781));
#59870=CARTESIAN_POINT('Ctrl Pts',(-0.139290267180057,1.,4.04890199238036));
#59871=CARTESIAN_POINT('Ctrl Pts',(-0.136651205046119,1.,4.05611873400172));
#59872=CARTESIAN_POINT('Ctrl Pts',(-0.133972916144245,1.,4.06333121018596));
#59873=CARTESIAN_POINT('Ctrl Pts',(-0.131255793548941,1.,4.0705393152874));
#59874=CARTESIAN_POINT('Ctrl Pts',(-0.128500200484838,1.,4.07774270738954));
#59875=CARTESIAN_POINT('Ctrl Pts',(-0.12570647682254,1.,4.08494093372377));
#59876=CARTESIAN_POINT('Ctrl Pts',(-0.122874946249107,1.,4.09213355850756));
#59877=CARTESIAN_POINT('Ctrl Pts',(-0.120005924388124,1.,4.09932031767002));
#59878=CARTESIAN_POINT('Ctrl Pts',(-0.117099722731648,1.,4.10650113381833));
#59879=CARTESIAN_POINT('Ctrl Pts',(-0.114156649609546,1.,4.11367603924961));
#59880=CARTESIAN_POINT('Ctrl Pts',(-0.111177012683347,1.,4.1208451250225));
#59881=CARTESIAN_POINT('Ctrl Pts',(-0.10816112052837,1.,4.12800848371504));
#59882=CARTESIAN_POINT('Ctrl Pts',(-0.105109286538945,1.,4.13516614458895));
#59883=CARTESIAN_POINT('Ctrl Pts',(-0.102021826577584,1.,4.14231804939538));
#59884=CARTESIAN_POINT('Ctrl Pts',(-0.0988990478901228,1.,4.14946408918485));
#59885=CARTESIAN_POINT('Ctrl Pts',(-0.0957412403298009,1.,4.15660412653577));
#59886=CARTESIAN_POINT('Ctrl Pts',(-0.0925486672167534,1.,4.16373802265839));
#59887=CARTESIAN_POINT('Ctrl Pts',(-0.0893215560848652,1.,4.17086566490794));
#59888=CARTESIAN_POINT('Ctrl Pts',(-0.0860600915549399,1.,4.17798698668094));
#59889=CARTESIAN_POINT('Ctrl Pts',(-0.0827644164385681,1.,4.18510195327123));
#59890=CARTESIAN_POINT('Ctrl Pts',(-0.0801005887114322,1.,4.19078883320504));
#59891=CARTESIAN_POINT('Ctrl Pts',(-0.07808739562424,1.,4.19505112859416));
#59892=CARTESIAN_POINT('Ctrl Pts',(-0.0767384596141467,1.,4.1978913862118));
#59893=CARTESIAN_POINT('Ctrl Pts',(-0.0760622897878249,1.,4.19931119685982));
#59894=CARTESIAN_POINT('Origin',(-0.0760622897878249,0.,4.19931119685982));
#59895=CARTESIAN_POINT('',(0.0760622897878233,1.,4.19931119685982));
#59896=CARTESIAN_POINT('Origin',(0.,0.,0.));
#59897=CARTESIAN_POINT('',(-0.385112848330762,1.,3.73017266276651));
#59898=CARTESIAN_POINT('Origin',(0.,1.,0.));
#59899=CARTESIAN_POINT('Ctrl Pts',(-0.385112848330762,1.,3.73017266276651));
#59900=CARTESIAN_POINT('Ctrl Pts',(-0.385112848330762,0.666666666666667,
3.73017266276651));
#59901=CARTESIAN_POINT('Ctrl Pts',(-0.385112848330762,0.333333333333333,
3.73017266276651));
#59902=CARTESIAN_POINT('Ctrl Pts',(-0.385112848330762,-0.333333333333333,
3.73017266276651));
#59903=CARTESIAN_POINT('Ctrl Pts',(-0.385112848330762,-0.666666666666667,
3.73017266276651));
#59904=CARTESIAN_POINT('Ctrl Pts',(-0.385112848330762,-1.,3.73017266276651));
#59905=CARTESIAN_POINT('Ctrl Pts',(-0.581791163835815,-1.,4.15950947128175));
#59906=CARTESIAN_POINT('Ctrl Pts',(-0.581791163835815,1.,4.15950947128175));
#59907=CARTESIAN_POINT('Ctrl Pts',(-0.580901211463535,-1.,4.1582129171283));
#59908=CARTESIAN_POINT('Ctrl Pts',(-0.580901211463535,1.,4.1582129171283));
#59909=CARTESIAN_POINT('Ctrl Pts',(-0.579124568914235,-1.,4.15561864788576));
#59910=CARTESIAN_POINT('Ctrl Pts',(-0.579124568914235,1.,4.15561864788576));
#59911=CARTESIAN_POINT('Ctrl Pts',(-0.576469391676688,-1.,4.151723761217));
#59912=CARTESIAN_POINT('Ctrl Pts',(-0.576469391676688,1.,4.151723761217));
#59913=CARTESIAN_POINT('Ctrl Pts',(-0.572948736069522,-1.,4.14652361068081));
#59914=CARTESIAN_POINT('Ctrl Pts',(-0.572948736069522,1.,4.14652361068081));
#59915=CARTESIAN_POINT('Ctrl Pts',(-0.568580610189775,-1.,4.14001179830547));
#59916=CARTESIAN_POINT('Ctrl Pts',(-0.568580610189775,1.,4.14001179830547));
#59917=CARTESIAN_POINT('Ctrl Pts',(-0.564245279537149,-1.,4.13348835727104));
#59918=CARTESIAN_POINT('Ctrl Pts',(-0.564245279537149,1.,4.13348835727104));
#59919=CARTESIAN_POINT('Ctrl Pts',(-0.559942890594774,-1.,4.12695329951961));
#59920=CARTESIAN_POINT('Ctrl Pts',(-0.559942890594774,1.,4.12695329951961));
#59921=CARTESIAN_POINT('Ctrl Pts',(-0.555673636129977,-1.,4.12040666195664));
#59922=CARTESIAN_POINT('Ctrl Pts',(-0.555673636129977,1.,4.12040666195664));
#59923=CARTESIAN_POINT('Ctrl Pts',(-0.551437758497033,-1.,4.11384852024721));
#59924=CARTESIAN_POINT('Ctrl Pts',(-0.551437758497033,1.,4.11384852024721));
#59925=CARTESIAN_POINT('Ctrl Pts',(-0.547235539485637,-1.,4.10727897027977));
#59926=CARTESIAN_POINT('Ctrl Pts',(-0.547235539485637,1.,4.10727897027977));
#59927=CARTESIAN_POINT('Ctrl Pts',(-0.543067286877757,-1.,4.10069810243979));
#59928=CARTESIAN_POINT('Ctrl Pts',(-0.543067286877757,1.,4.10069810243979));
#59929=CARTESIAN_POINT('Ctrl Pts',(-0.538933321179756,-1.,4.09410597627));
#59930=CARTESIAN_POINT('Ctrl Pts',(-0.538933321179756,1.,4.09410597627));
#59931=CARTESIAN_POINT('Ctrl Pts',(-0.534833963477273,-1.,4.08750259988885));
#59932=CARTESIAN_POINT('Ctrl Pts',(-0.534833963477273,1.,4.08750259988885));
#59933=CARTESIAN_POINT('Ctrl Pts',(-0.530769518728571,-1.,4.08088789536836));
#59934=CARTESIAN_POINT('Ctrl Pts',(-0.530769518728571,1.,4.08088789536836));
#59935=CARTESIAN_POINT('Ctrl Pts',(-0.526740277227498,-1.,4.07426172299847));
#59936=CARTESIAN_POINT('Ctrl Pts',(-0.526740277227498,1.,4.07426172299847));
#59937=CARTESIAN_POINT('Ctrl Pts',(-0.522746528603107,-1.,4.06762394471314));
#59938=CARTESIAN_POINT('Ctrl Pts',(-0.522746528603107,1.,4.06762394471314));
#59939=CARTESIAN_POINT('Ctrl Pts',(-0.518788572336924,-1.,4.06097448038013));
#59940=CARTESIAN_POINT('Ctrl Pts',(-0.518788572336924,1.,4.06097448038013));
#59941=CARTESIAN_POINT('Ctrl Pts',(-0.514866728193017,-1.,4.05431335771199));
#59942=CARTESIAN_POINT('Ctrl Pts',(-0.514866728193017,1.,4.05431335771199));
#59943=CARTESIAN_POINT('Ctrl Pts',(-0.51098134921897,-1.,4.04764078815447));
#59944=CARTESIAN_POINT('Ctrl Pts',(-0.51098134921897,1.,4.04764078815447));
#59945=CARTESIAN_POINT('Ctrl Pts',(-0.507132823288136,-1.,4.04095715148915));
#59946=CARTESIAN_POINT('Ctrl Pts',(-0.507132823288136,1.,4.04095715148915));
#59947=CARTESIAN_POINT('Ctrl Pts',(-0.503321556915346,-1.,4.03426284174272));
#59948=CARTESIAN_POINT('Ctrl Pts',(-0.503321556915346,1.,4.03426284174272));
#59949=CARTESIAN_POINT('Ctrl Pts',(-0.499547962340821,-1.,4.02755813980101));
#59950=CARTESIAN_POINT('Ctrl Pts',(-0.499547962340821,1.,4.02755813980101));
#59951=CARTESIAN_POINT('Ctrl Pts',(-0.495812444326251,-1.,4.02084308851832));
#59952=CARTESIAN_POINT('Ctrl Pts',(-0.495812444326251,1.,4.02084308851832));
#59953=CARTESIAN_POINT('Ctrl Pts',(-0.492115383418018,-1.,4.01411733503546));
#59954=CARTESIAN_POINT('Ctrl Pts',(-0.492115383418018,1.,4.01411733503546));
#59955=CARTESIAN_POINT('Ctrl Pts',(-0.488457130424633,-1.,4.0073800839099));
#59956=CARTESIAN_POINT('Ctrl Pts',(-0.488457130424633,1.,4.0073800839099));
#59957=CARTESIAN_POINT('Ctrl Pts',(-0.484838042421835,-1.,4.00063045119288));
#59958=CARTESIAN_POINT('Ctrl Pts',(-0.484838042421835,1.,4.00063045119288));
#59959=CARTESIAN_POINT('Ctrl Pts',(-0.481258512209675,-1.,3.99386775880679));
#59960=CARTESIAN_POINT('Ctrl Pts',(-0.481258512209675,1.,3.99386775880679));
#59961=CARTESIAN_POINT('Ctrl Pts',(-0.477718999122027,-1.,3.98709184306738));
#59962=CARTESIAN_POINT('Ctrl Pts',(-0.477718999122027,1.,3.98709184306738));
#59963=CARTESIAN_POINT('Ctrl Pts',(-0.47422006101951,-1.,3.98030338044409));
#59964=CARTESIAN_POINT('Ctrl Pts',(-0.47422006101951,1.,3.98030338044409));
#59965=CARTESIAN_POINT('Ctrl Pts',(-0.470762379613439,-1.,3.97350414289392));
#59966=CARTESIAN_POINT('Ctrl Pts',(-0.470762379613439,1.,3.97350414289392));
#59967=CARTESIAN_POINT('Ctrl Pts',(-0.467346690880643,-1.,3.9666962227393));
#59968=CARTESIAN_POINT('Ctrl Pts',(-0.467346690880643,1.,3.9666962227393));
#59969=CARTESIAN_POINT('Ctrl Pts',(-0.463973722115733,-1.,3.95988133243538));
#59970=CARTESIAN_POINT('Ctrl Pts',(-0.463973722115733,1.,3.95988133243538));
#59971=CARTESIAN_POINT('Ctrl Pts',(-0.460644124429121,-1.,3.95306005817364));
#59972=CARTESIAN_POINT('Ctrl Pts',(-0.460644124429121,1.,3.95306005817364));
#59973=CARTESIAN_POINT('Ctrl Pts',(-0.457358410451683,-1.,3.94623117206678));
#59974=CARTESIAN_POINT('Ctrl Pts',(-0.457358410451683,1.,3.94623117206678));
#59975=CARTESIAN_POINT('Ctrl Pts',(-0.454116879027584,-1.,3.93939080846298));
#59976=CARTESIAN_POINT('Ctrl Pts',(-0.454116879027584,1.,3.93939080846298));
#59977=CARTESIAN_POINT('Ctrl Pts',(-0.450919768356348,-1.,3.93253407403123));
#59978=CARTESIAN_POINT('Ctrl Pts',(-0.450919768356348,1.,3.93253407403123));
#59979=CARTESIAN_POINT('Ctrl Pts',(-0.447767416837293,-1.,3.92565674143416));
#59980=CARTESIAN_POINT('Ctrl Pts',(-0.447767416837293,1.,3.92565674143416));
#59981=CARTESIAN_POINT('Ctrl Pts',(-0.444660430230591,-1.,3.91875701610719));
#59982=CARTESIAN_POINT('Ctrl Pts',(-0.444660430230591,1.,3.91875701610719));
#59983=CARTESIAN_POINT('Ctrl Pts',(-0.441599824524054,-1.,3.91183704069153));
#59984=CARTESIAN_POINT('Ctrl Pts',(-0.441599824524054,1.,3.91183704069153));
#59985=CARTESIAN_POINT('Ctrl Pts',(-0.43858723545825,-1.,3.90490512938563));
#59986=CARTESIAN_POINT('Ctrl Pts',(-0.43858723545825,1.,3.90490512938563));
#59987=CARTESIAN_POINT('Ctrl Pts',(-0.435624629433528,-1.,3.89797256655462));
#59988=CARTESIAN_POINT('Ctrl Pts',(-0.435624629433528,1.,3.89797256655462));
#59989=CARTESIAN_POINT('Ctrl Pts',(-0.432713929544458,-1.,3.89104947940611));
#59990=CARTESIAN_POINT('Ctrl Pts',(-0.432713929544458,1.,3.89104947940611));
#59991=CARTESIAN_POINT('Ctrl Pts',(-0.429856640579741,-1.,3.88414070943341));
#59992=CARTESIAN_POINT('Ctrl Pts',(-0.429856640579741,1.,3.88414070943341));
#59993=CARTESIAN_POINT('Ctrl Pts',(-0.427053541173457,-1.,3.87724240306597));
#59994=CARTESIAN_POINT('Ctrl Pts',(-0.427053541173457,1.,3.87724240306597));
#59995=CARTESIAN_POINT('Ctrl Pts',(-0.424304173195111,-1.,3.87033643487851));
#59996=CARTESIAN_POINT('Ctrl Pts',(-0.424304173195111,1.,3.87033643487851));
#59997=CARTESIAN_POINT('Ctrl Pts',(-0.421607423177534,-1.,3.86339652542709));
#59998=CARTESIAN_POINT('Ctrl Pts',(-0.421607423177534,1.,3.86339652542709));
#59999=CARTESIAN_POINT('Ctrl Pts',(-0.418962468086773,-1.,3.85639825647996));
#60000=CARTESIAN_POINT('Ctrl Pts',(-0.418962468086773,1.,3.85639825647996));
#60001=CARTESIAN_POINT('Ctrl Pts',(-0.416369678052907,-1.,3.84932864157497));
#60002=CARTESIAN_POINT('Ctrl Pts',(-0.416369678052907,1.,3.84932864157497));
#60003=CARTESIAN_POINT('Ctrl Pts',(-0.413831367016748,-1.,3.84219403994762));
#60004=CARTESIAN_POINT('Ctrl Pts',(-0.413831367016748,1.,3.84219403994762));
#60005=CARTESIAN_POINT('Ctrl Pts',(-0.411353038798519,-1.,3.83503345578698));
#60006=CARTESIAN_POINT('Ctrl Pts',(-0.411353038798519,1.,3.83503345578698));
#60007=CARTESIAN_POINT('Ctrl Pts',(-0.40894237144746,-1.,3.82790724256471));
#60008=CARTESIAN_POINT('Ctrl Pts',(-0.40894237144746,1.,3.82790724256471));
#60009=CARTESIAN_POINT('Ctrl Pts',(-0.406607038258985,-1.,3.8208730391381));
#60010=CARTESIAN_POINT('Ctrl Pts',(-0.406607038258985,1.,3.8208730391381));
#60011=CARTESIAN_POINT('Ctrl Pts',(-0.404352694628273,-1.,3.81396374287793));
#60012=CARTESIAN_POINT('Ctrl Pts',(-0.404352694628273,1.,3.81396374287793));
#60013=CARTESIAN_POINT('Ctrl Pts',(-0.402181320148436,-1.,3.80716881962728));
#60014=CARTESIAN_POINT('Ctrl Pts',(-0.402181320148436,1.,3.80716881962728));
#60015=CARTESIAN_POINT('Ctrl Pts',(-0.4000883465046,-1.,3.80040370384546));
#60016=CARTESIAN_POINT('Ctrl Pts',(-0.4000883465046,1.,3.80040370384546));
#60017=CARTESIAN_POINT('Ctrl Pts',(-0.39806481868397,-1.,3.7935288716329));
#60018=CARTESIAN_POINT('Ctrl Pts',(-0.39806481868397,1.,3.7935288716329));
#60019=CARTESIAN_POINT('Ctrl Pts',(-0.396103205334841,-1.,3.78640521279313));
#60020=CARTESIAN_POINT('Ctrl Pts',(-0.396103205334841,1.,3.78640521279313));
#60021=CARTESIAN_POINT('Ctrl Pts',(-0.394202481011499,-1.,3.77894173114283));
#60022=CARTESIAN_POINT('Ctrl Pts',(-0.394202481011499,1.,3.77894173114283));
#60023=CARTESIAN_POINT('Ctrl Pts',(-0.392372786223433,-1.,3.77114011595967));
#60024=CARTESIAN_POINT('Ctrl Pts',(-0.392372786223433,1.,3.77114011595967));
#60025=CARTESIAN_POINT('Ctrl Pts',(-0.39064207297956,-1.,3.76315635033257));
#60026=CARTESIAN_POINT('Ctrl Pts',(-0.39064207297956,1.,3.76315635033257));
#60027=CARTESIAN_POINT('Ctrl Pts',(-0.389054775898702,-1.,3.75529302895152));
#60028=CARTESIAN_POINT('Ctrl Pts',(-0.389054775898702,1.,3.75529302895152));
#60029=CARTESIAN_POINT('Ctrl Pts',(-0.387663020050836,-1.,3.74792651696654));
#60030=CARTESIAN_POINT('Ctrl Pts',(-0.387663020050836,1.,3.74792651696654));
#60031=CARTESIAN_POINT('Ctrl Pts',(-0.386519576222251,-1.,3.74144965781276));
#60032=CARTESIAN_POINT('Ctrl Pts',(-0.386519576222251,1.,3.74144965781276));
#60033=CARTESIAN_POINT('Ctrl Pts',(-0.385670806454566,-1.,3.73621371845318));
#60034=CARTESIAN_POINT('Ctrl Pts',(-0.385670806454566,1.,3.73621371845318));
#60035=CARTESIAN_POINT('Ctrl Pts',(-0.385147887988951,-1.,3.73245705638843));
#60036=CARTESIAN_POINT('Ctrl Pts',(-0.385147887988951,1.,3.73245705638843));
#60037=CARTESIAN_POINT('Ctrl Pts',(-0.385001870183213,-1.,3.73072465900175));
#60038=CARTESIAN_POINT('Ctrl Pts',(-0.385001870183213,1.,3.73072465900175));
#60039=CARTESIAN_POINT('Ctrl Pts',(-0.385047711603462,-1.,3.73015851028356));
#60040=CARTESIAN_POINT('Ctrl Pts',(-0.385047711603462,1.,3.73015851028356));
#60041=CARTESIAN_POINT('Ctrl Pts',(-0.385147278814642,-1.,3.73010668803042));
#60042=CARTESIAN_POINT('Ctrl Pts',(-0.385147278814642,1.,3.73010668803042));
#60043=CARTESIAN_POINT('Ctrl Pts',(-0.38521431477633,-1.,3.73016218570874));
#60044=CARTESIAN_POINT('Ctrl Pts',(-0.38521431477633,1.,3.73016218570874));
#60045=CARTESIAN_POINT('',(-0.581791163835815,1.,4.15950947128175));
#60046=CARTESIAN_POINT('Ctrl Pts',(-0.581791163835815,1.,4.15950947128175));
#60047=CARTESIAN_POINT('Ctrl Pts',(-0.580901211463535,1.,4.1582129171283));
#60048=CARTESIAN_POINT('Ctrl Pts',(-0.579124568914235,1.,4.15561864788576));
#60049=CARTESIAN_POINT('Ctrl Pts',(-0.576469391676688,1.,4.151723761217));
#60050=CARTESIAN_POINT('Ctrl Pts',(-0.572948736069522,1.,4.14652361068081));
#60051=CARTESIAN_POINT('Ctrl Pts',(-0.568580610189775,1.,4.14001179830547));
#60052=CARTESIAN_POINT('Ctrl Pts',(-0.564245279537149,1.,4.13348835727104));
#60053=CARTESIAN_POINT('Ctrl Pts',(-0.559942890594774,1.,4.12695329951961));
#60054=CARTESIAN_POINT('Ctrl Pts',(-0.555673636129977,1.,4.12040666195664));
#60055=CARTESIAN_POINT('Ctrl Pts',(-0.551437758497033,1.,4.11384852024721));
#60056=CARTESIAN_POINT('Ctrl Pts',(-0.547235539485637,1.,4.10727897027977));
#60057=CARTESIAN_POINT('Ctrl Pts',(-0.543067286877757,1.,4.10069810243979));
#60058=CARTESIAN_POINT('Ctrl Pts',(-0.538933321179756,1.,4.09410597627));
#60059=CARTESIAN_POINT('Ctrl Pts',(-0.534833963477273,1.,4.08750259988885));
#60060=CARTESIAN_POINT('Ctrl Pts',(-0.530769518728571,1.,4.08088789536836));
#60061=CARTESIAN_POINT('Ctrl Pts',(-0.526740277227498,1.,4.07426172299847));
#60062=CARTESIAN_POINT('Ctrl Pts',(-0.522746528603107,1.,4.06762394471314));
#60063=CARTESIAN_POINT('Ctrl Pts',(-0.518788572336924,1.,4.06097448038013));
#60064=CARTESIAN_POINT('Ctrl Pts',(-0.514866728193017,1.,4.05431335771199));
#60065=CARTESIAN_POINT('Ctrl Pts',(-0.51098134921897,1.,4.04764078815447));
#60066=CARTESIAN_POINT('Ctrl Pts',(-0.507132823288136,1.,4.04095715148915));
#60067=CARTESIAN_POINT('Ctrl Pts',(-0.503321556915346,1.,4.03426284174272));
#60068=CARTESIAN_POINT('Ctrl Pts',(-0.499547962340821,1.,4.02755813980101));
#60069=CARTESIAN_POINT('Ctrl Pts',(-0.495812444326251,1.,4.02084308851832));
#60070=CARTESIAN_POINT('Ctrl Pts',(-0.492115383418018,1.,4.01411733503546));
#60071=CARTESIAN_POINT('Ctrl Pts',(-0.488457130424633,1.,4.0073800839099));
#60072=CARTESIAN_POINT('Ctrl Pts',(-0.484838042421835,1.,4.00063045119288));
#60073=CARTESIAN_POINT('Ctrl Pts',(-0.481258512209675,1.,3.99386775880679));
#60074=CARTESIAN_POINT('Ctrl Pts',(-0.477718999122027,1.,3.98709184306738));
#60075=CARTESIAN_POINT('Ctrl Pts',(-0.47422006101951,1.,3.98030338044409));
#60076=CARTESIAN_POINT('Ctrl Pts',(-0.470762379613439,1.,3.97350414289392));
#60077=CARTESIAN_POINT('Ctrl Pts',(-0.467346690880643,1.,3.9666962227393));
#60078=CARTESIAN_POINT('Ctrl Pts',(-0.463973722115733,1.,3.95988133243538));
#60079=CARTESIAN_POINT('Ctrl Pts',(-0.460644124429121,1.,3.95306005817364));
#60080=CARTESIAN_POINT('Ctrl Pts',(-0.457358410451683,1.,3.94623117206678));
#60081=CARTESIAN_POINT('Ctrl Pts',(-0.454116879027584,1.,3.93939080846298));
#60082=CARTESIAN_POINT('Ctrl Pts',(-0.450919768356348,1.,3.93253407403123));
#60083=CARTESIAN_POINT('Ctrl Pts',(-0.447767416837293,1.,3.92565674143416));
#60084=CARTESIAN_POINT('Ctrl Pts',(-0.444660430230591,1.,3.91875701610719));
#60085=CARTESIAN_POINT('Ctrl Pts',(-0.441599824524054,1.,3.91183704069153));
#60086=CARTESIAN_POINT('Ctrl Pts',(-0.43858723545825,1.,3.90490512938563));
#60087=CARTESIAN_POINT('Ctrl Pts',(-0.435624629433528,1.,3.89797256655462));
#60088=CARTESIAN_POINT('Ctrl Pts',(-0.432713929544458,1.,3.89104947940611));
#60089=CARTESIAN_POINT('Ctrl Pts',(-0.429856640579741,1.,3.88414070943341));
#60090=CARTESIAN_POINT('Ctrl Pts',(-0.427053541173457,1.,3.87724240306597));
#60091=CARTESIAN_POINT('Ctrl Pts',(-0.424304173195111,1.,3.87033643487851));
#60092=CARTESIAN_POINT('Ctrl Pts',(-0.421607423177534,1.,3.86339652542709));
#60093=CARTESIAN_POINT('Ctrl Pts',(-0.418962468086773,1.,3.85639825647996));
#60094=CARTESIAN_POINT('Ctrl Pts',(-0.416369678052907,1.,3.84932864157497));
#60095=CARTESIAN_POINT('Ctrl Pts',(-0.413831367016748,1.,3.84219403994762));
#60096=CARTESIAN_POINT('Ctrl Pts',(-0.411353038798519,1.,3.83503345578698));
#60097=CARTESIAN_POINT('Ctrl Pts',(-0.40894237144746,1.,3.82790724256471));
#60098=CARTESIAN_POINT('Ctrl Pts',(-0.406607038258985,1.,3.8208730391381));
#60099=CARTESIAN_POINT('Ctrl Pts',(-0.404352694628273,1.,3.81396374287793));
#60100=CARTESIAN_POINT('Ctrl Pts',(-0.402181320148436,1.,3.80716881962728));
#60101=CARTESIAN_POINT('Ctrl Pts',(-0.4000883465046,1.,3.80040370384546));
#60102=CARTESIAN_POINT('Ctrl Pts',(-0.39806481868397,1.,3.7935288716329));
#60103=CARTESIAN_POINT('Ctrl Pts',(-0.396103205334841,1.,3.78640521279313));
#60104=CARTESIAN_POINT('Ctrl Pts',(-0.394202481011499,1.,3.77894173114283));
#60105=CARTESIAN_POINT('Ctrl Pts',(-0.392372786223433,1.,3.77114011595967));
#60106=CARTESIAN_POINT('Ctrl Pts',(-0.39064207297956,1.,3.76315635033257));
#60107=CARTESIAN_POINT('Ctrl Pts',(-0.389054775898702,1.,3.75529302895152));
#60108=CARTESIAN_POINT('Ctrl Pts',(-0.387663020050836,1.,3.74792651696654));
#60109=CARTESIAN_POINT('Ctrl Pts',(-0.386519576222251,1.,3.74144965781276));
#60110=CARTESIAN_POINT('Ctrl Pts',(-0.385670806454566,1.,3.73621371845318));
#60111=CARTESIAN_POINT('Ctrl Pts',(-0.385187124634206,1.,3.73273893363406));
#60112=CARTESIAN_POINT('Ctrl Pts',(-0.385031656499164,1.,3.73106082862548));
#60113=CARTESIAN_POINT('Ctrl Pts',(-0.385037797881504,1.,3.73040527621055));
#60114=CARTESIAN_POINT('Ctrl Pts',(-0.385087139000375,1.,3.73021431755274));
#60115=CARTESIAN_POINT('Ctrl Pts',(-0.385112848330762,1.,3.73017266276651));
#60116=CARTESIAN_POINT('',(-0.581791163835815,0.,4.15950947128175));
#60117=CARTESIAN_POINT('Ctrl Pts',(-0.7863229229206,-1.,3.66663282329846));
#60118=CARTESIAN_POINT('Ctrl Pts',(-0.7863229229206,1.,3.66663282329846));
#60119=CARTESIAN_POINT('Ctrl Pts',(-0.786369528183326,-1.,3.66655932661986));
#60120=CARTESIAN_POINT('Ctrl Pts',(-0.786369528183326,1.,3.66655932661986));
#60121=CARTESIAN_POINT('Ctrl Pts',(-0.786480236185697,-1.,3.66657784455334));
#60122=CARTESIAN_POINT('Ctrl Pts',(-0.786480236185697,1.,3.66657784455334));
#60123=CARTESIAN_POINT('Ctrl Pts',(-0.786698783542764,-1.,3.66710211820482));
#60124=CARTESIAN_POINT('Ctrl Pts',(-0.786698783542764,1.,3.66710211820482));
#60125=CARTESIAN_POINT('Ctrl Pts',(-0.787095252590501,-1.,3.66879484801113));
#60126=CARTESIAN_POINT('Ctrl Pts',(-0.787095252590501,1.,3.66879484801113));
#60127=CARTESIAN_POINT('Ctrl Pts',(-0.787758799995743,-1.,3.67252923663655));
#60128=CARTESIAN_POINT('Ctrl Pts',(-0.787758799995743,1.,3.67252923663655));
#60129=CARTESIAN_POINT('Ctrl Pts',(-0.788569566220285,-1.,3.67777119516252));
#60130=CARTESIAN_POINT('Ctrl Pts',(-0.788569566220285,1.,3.67777119516252));
#60131=CARTESIAN_POINT('Ctrl Pts',(-0.789483546064387,-1.,3.68428439783905));
#60132=CARTESIAN_POINT('Ctrl Pts',(-0.789483546064387,1.,3.68428439783905));
#60133=CARTESIAN_POINT('Ctrl Pts',(-0.790436284988788,-1.,3.69172044327364));
#60134=CARTESIAN_POINT('Ctrl Pts',(-0.790436284988788,1.,3.69172044327364));
#60135=CARTESIAN_POINT('Ctrl Pts',(-0.79135657569598,-1.,3.69968940808721));
#60136=CARTESIAN_POINT('Ctrl Pts',(-0.79135657569598,1.,3.69968940808721));
#60137=CARTESIAN_POINT('Ctrl Pts',(-0.792177688845818,-1.,3.70781724021806));
#60138=CARTESIAN_POINT('Ctrl Pts',(-0.792177688845818,1.,3.70781724021806));
#60139=CARTESIAN_POINT('Ctrl Pts',(-0.792848377370287,-1.,3.71580242396124));
#60140=CARTESIAN_POINT('Ctrl Pts',(-0.792848377370287,1.,3.71580242396124));
#60141=CARTESIAN_POINT('Ctrl Pts',(-0.793347023784205,-1.,3.72348797293734));
#60142=CARTESIAN_POINT('Ctrl Pts',(-0.793347023784205,1.,3.72348797293734));
#60143=CARTESIAN_POINT('Ctrl Pts',(-0.793682750269684,-1.,3.73086914695805));
#60144=CARTESIAN_POINT('Ctrl Pts',(-0.793682750269684,1.,3.73086914695805));
#60145=CARTESIAN_POINT('Ctrl Pts',(-0.793882700937017,-1.,3.73803280541687));
#60146=CARTESIAN_POINT('Ctrl Pts',(-0.793882700937017,1.,3.73803280541687));
#60147=CARTESIAN_POINT('Ctrl Pts',(-0.793982700459952,-1.,3.74511357728861));
#60148=CARTESIAN_POINT('Ctrl Pts',(-0.793982700459952,1.,3.74511357728861));
#60149=CARTESIAN_POINT('Ctrl Pts',(-0.794017347371377,-1.,3.75224692493864));
#60150=CARTESIAN_POINT('Ctrl Pts',(-0.794017347371377,1.,3.75224692493864));
#60151=CARTESIAN_POINT('Ctrl Pts',(-0.794008429134907,-1.,3.75951468666257));
#60152=CARTESIAN_POINT('Ctrl Pts',(-0.794008429134907,1.,3.75951468666257));
#60153=CARTESIAN_POINT('Ctrl Pts',(-0.793961083688992,-1.,3.76692626931111));
#60154=CARTESIAN_POINT('Ctrl Pts',(-0.793961083688992,1.,3.76692626931111));
#60155=CARTESIAN_POINT('Ctrl Pts',(-0.793870523787408,-1.,3.77444863801212));
#60156=CARTESIAN_POINT('Ctrl Pts',(-0.793870523787408,1.,3.77444863801212));
#60157=CARTESIAN_POINT('Ctrl Pts',(-0.7937262357813,-1.,3.78202460377598));
#60158=CARTESIAN_POINT('Ctrl Pts',(-0.7937262357813,1.,3.78202460377598));
#60159=CARTESIAN_POINT('Ctrl Pts',(-0.793516871680993,-1.,3.78959439439235));
#60160=CARTESIAN_POINT('Ctrl Pts',(-0.793516871680993,1.,3.78959439439235));
#60161=CARTESIAN_POINT('Ctrl Pts',(-0.793235612973273,-1.,3.79711921389897));
#60162=CARTESIAN_POINT('Ctrl Pts',(-0.793235612973273,1.,3.79711921389897));
#60163=CARTESIAN_POINT('Ctrl Pts',(-0.792882695234778,-1.,3.80459229925637));
#60164=CARTESIAN_POINT('Ctrl Pts',(-0.792882695234778,1.,3.80459229925637));
#60165=CARTESIAN_POINT('Ctrl Pts',(-0.792462483517634,-1.,3.81202588694756));
#60166=CARTESIAN_POINT('Ctrl Pts',(-0.792462483517634,1.,3.81202588694756));
#60167=CARTESIAN_POINT('Ctrl Pts',(-0.791981740718635,-1.,3.81944345442249));
#60168=CARTESIAN_POINT('Ctrl Pts',(-0.791981740718635,1.,3.81944345442249));
#60169=CARTESIAN_POINT('Ctrl Pts',(-0.791447528662369,-1.,3.82687033899792));
#60170=CARTESIAN_POINT('Ctrl Pts',(-0.791447528662369,1.,3.82687033899792));
#60171=CARTESIAN_POINT('Ctrl Pts',(-0.790865012705301,-1.,3.83432392054786));
#60172=CARTESIAN_POINT('Ctrl Pts',(-0.790865012705301,1.,3.83432392054786));
#60173=CARTESIAN_POINT('Ctrl Pts',(-0.790236124191242,-1.,3.84180762342454));
#60174=CARTESIAN_POINT('Ctrl Pts',(-0.790236124191242,1.,3.84180762342454));
#60175=CARTESIAN_POINT('Ctrl Pts',(-0.789560798155582,-1.,3.84931637808894));
#60176=CARTESIAN_POINT('Ctrl Pts',(-0.789560798155582,1.,3.84931637808894));
#60177=CARTESIAN_POINT('Ctrl Pts',(-0.788837734090672,-1.,3.85683995872529));
#60178=CARTESIAN_POINT('Ctrl Pts',(-0.788837734090672,1.,3.85683995872529));
#60179=CARTESIAN_POINT('Ctrl Pts',(-0.788065315093778,-1.,3.86436702561345));
#60180=CARTESIAN_POINT('Ctrl Pts',(-0.788065315093778,1.,3.86436702561345));
#60181=CARTESIAN_POINT('Ctrl Pts',(-0.787242527617999,-1.,3.87188916600912));
#60182=CARTESIAN_POINT('Ctrl Pts',(-0.787242527617999,1.,3.87188916600912));
#60183=CARTESIAN_POINT('Ctrl Pts',(-0.786369675812609,-1.,3.8794040281819));
#60184=CARTESIAN_POINT('Ctrl Pts',(-0.786369675812609,1.,3.8794040281819));
#60185=CARTESIAN_POINT('Ctrl Pts',(-0.78544789034073,-1.,3.88691313167398));
#60186=CARTESIAN_POINT('Ctrl Pts',(-0.78544789034073,1.,3.88691313167398));
#60187=CARTESIAN_POINT('Ctrl Pts',(-0.784478799358336,-1.,3.89442039235103));
#60188=CARTESIAN_POINT('Ctrl Pts',(-0.784478799358336,1.,3.89442039235103));
#60189=CARTESIAN_POINT('Ctrl Pts',(-0.783464141529081,-1.,3.9019303904397));
#60190=CARTESIAN_POINT('Ctrl Pts',(-0.783464141529081,1.,3.9019303904397));
#60191=CARTESIAN_POINT('Ctrl Pts',(-0.782405395622764,-1.,3.90944671004542));
#60192=CARTESIAN_POINT('Ctrl Pts',(-0.782405395622764,1.,3.90944671004542));
#60193=CARTESIAN_POINT('Ctrl Pts',(-0.781303428618367,-1.,3.91697036054676));
#60194=CARTESIAN_POINT('Ctrl Pts',(-0.781303428618367,1.,3.91697036054676));
#60195=CARTESIAN_POINT('Ctrl Pts',(-0.780158678615543,-1.,3.92450058323823));
#60196=CARTESIAN_POINT('Ctrl Pts',(-0.780158678615543,1.,3.92450058323823));
#60197=CARTESIAN_POINT('Ctrl Pts',(-0.778971308134821,-1.,3.93203552473174));
#60198=CARTESIAN_POINT('Ctrl Pts',(-0.778971308134821,1.,3.93203552473174));
#60199=CARTESIAN_POINT('Ctrl Pts',(-0.777741370568559,-1.,3.93957296768103));
#60200=CARTESIAN_POINT('Ctrl Pts',(-0.777741370568559,1.,3.93957296768103));
#60201=CARTESIAN_POINT('Ctrl Pts',(-0.776468966697921,-1.,3.94711101619447));
#60202=CARTESIAN_POINT('Ctrl Pts',(-0.776468966697921,1.,3.94711101619447));
#60203=CARTESIAN_POINT('Ctrl Pts',(-0.775154418039352,-1.,3.9546488545231));
#60204=CARTESIAN_POINT('Ctrl Pts',(-0.775154418039352,1.,3.9546488545231));
#60205=CARTESIAN_POINT('Ctrl Pts',(-0.773798212026566,-1.,3.96218649639807));
#60206=CARTESIAN_POINT('Ctrl Pts',(-0.773798212026566,1.,3.96218649639807));
#60207=CARTESIAN_POINT('Ctrl Pts',(-0.772400931772136,-1.,3.96972446532772));
#60208=CARTESIAN_POINT('Ctrl Pts',(-0.772400931772136,1.,3.96972446532772));
#60209=CARTESIAN_POINT('Ctrl Pts',(-0.770963190030471,-1.,3.97726349165488));
#60210=CARTESIAN_POINT('Ctrl Pts',(-0.770963190030471,1.,3.97726349165488));
#60211=CARTESIAN_POINT('Ctrl Pts',(-0.769485566245544,-1.,3.98480422348451));
#60212=CARTESIAN_POINT('Ctrl Pts',(-0.769485566245544,1.,3.98480422348451));
#60213=CARTESIAN_POINT('Ctrl Pts',(-0.767968531377915,-1.,3.9923468788101));
#60214=CARTESIAN_POINT('Ctrl Pts',(-0.767968531377915,1.,3.9923468788101));
#60215=CARTESIAN_POINT('Ctrl Pts',(-0.766412457136064,-1.,3.99989129179622));
#60216=CARTESIAN_POINT('Ctrl Pts',(-0.766412457136064,1.,3.99989129179622));
#60217=CARTESIAN_POINT('Ctrl Pts',(-0.764817648785198,-1.,4.00743706791509));
#60218=CARTESIAN_POINT('Ctrl Pts',(-0.764817648785198,1.,4.00743706791509));
#60219=CARTESIAN_POINT('Ctrl Pts',(-0.763184371182935,-1.,4.01498370680496));
#60220=CARTESIAN_POINT('Ctrl Pts',(-0.763184371182935,1.,4.01498370680496));
#60221=CARTESIAN_POINT('Ctrl Pts',(-0.761512875859804,-1.,4.02253072741268));
#60222=CARTESIAN_POINT('Ctrl Pts',(-0.761512875859804,1.,4.02253072741268));
#60223=CARTESIAN_POINT('Ctrl Pts',(-0.759803433243752,-1.,4.03007781954412));
#60224=CARTESIAN_POINT('Ctrl Pts',(-0.759803433243752,1.,4.03007781954412));
#60225=CARTESIAN_POINT('Ctrl Pts',(-0.758056338884944,-1.,4.03762485803119));
#60226=CARTESIAN_POINT('Ctrl Pts',(-0.758056338884944,1.,4.03762485803119));
#60227=CARTESIAN_POINT('Ctrl Pts',(-0.756271902369581,-1.,4.04517182653997));
#60228=CARTESIAN_POINT('Ctrl Pts',(-0.756271902369581,1.,4.04517182653997));
#60229=CARTESIAN_POINT('Ctrl Pts',(-0.754450441816078,-1.,4.05271876687915));
#60230=CARTESIAN_POINT('Ctrl Pts',(-0.754450441816078,1.,4.05271876687915));
#60231=CARTESIAN_POINT('Ctrl Pts',(-0.752592276483072,-1.,4.06026572221515));
#60232=CARTESIAN_POINT('Ctrl Pts',(-0.752592276483072,1.,4.06026572221515));
#60233=CARTESIAN_POINT('Ctrl Pts',(-0.750697720484036,-1.,4.06781267242378));
#60234=CARTESIAN_POINT('Ctrl Pts',(-0.750697720484036,1.,4.06781267242378));
#60235=CARTESIAN_POINT('Ctrl Pts',(-0.748767076680557,-1.,4.07535951056152));
#60236=CARTESIAN_POINT('Ctrl Pts',(-0.748767076680557,1.,4.07535951056152));
#60237=CARTESIAN_POINT('Ctrl Pts',(-0.746800631492315,-1.,4.08290608095642));
#60238=CARTESIAN_POINT('Ctrl Pts',(-0.746800631492315,1.,4.08290608095642));
#60239=CARTESIAN_POINT('Ctrl Pts',(-0.7447986497065,-1.,4.09045220253573));
#60240=CARTESIAN_POINT('Ctrl Pts',(-0.7447986497065,1.,4.09045220253573));
#60241=CARTESIAN_POINT('Ctrl Pts',(-0.742761369689841,-1.,4.09799769702611));
#60242=CARTESIAN_POINT('Ctrl Pts',(-0.742761369689841,1.,4.09799769702611));
#60243=CARTESIAN_POINT('Ctrl Pts',(-0.740688998553377,-1.,4.10554241757547));
#60244=CARTESIAN_POINT('Ctrl Pts',(-0.740688998553377,1.,4.10554241757547));
#60245=CARTESIAN_POINT('Ctrl Pts',(-0.738581708225844,-1.,4.11308626951927));
#60246=CARTESIAN_POINT('Ctrl Pts',(-0.738581708225844,1.,4.11308626951927));
#60247=CARTESIAN_POINT('Ctrl Pts',(-0.736439634331345,-1.,4.120629196238));
#60248=CARTESIAN_POINT('Ctrl Pts',(-0.736439634331345,1.,4.120629196238));
#60249=CARTESIAN_POINT('Ctrl Pts',(-0.734698226764092,-1.,4.12666277570844));
#60250=CARTESIAN_POINT('Ctrl Pts',(-0.734698226764092,1.,4.12666277570844));
#60251=CARTESIAN_POINT('Ctrl Pts',(-0.733376589323546,-1.,4.13118752795207));
#60252=CARTESIAN_POINT('Ctrl Pts',(-0.733376589323546,1.,4.13118752795207));
#60253=CARTESIAN_POINT('Ctrl Pts',(-0.73248857513516,-1.,4.1342038373684));
#60254=CARTESIAN_POINT('Ctrl Pts',(-0.73248857513516,1.,4.1342038373684));
#60255=CARTESIAN_POINT('Ctrl Pts',(-0.73204283740062,-1.,4.13571194405636));
#60256=CARTESIAN_POINT('Ctrl Pts',(-0.73204283740062,1.,4.13571194405636));
#60257=CARTESIAN_POINT('',(-0.786422660831985,1.,3.66661143271685));
#60258=CARTESIAN_POINT('Ctrl Pts',(-0.786422660831985,-1.,3.66661143271685));
#60259=CARTESIAN_POINT('Ctrl Pts',(-0.786422660831985,-0.666666666666667,
3.66661143271685));
#60260=CARTESIAN_POINT('Ctrl Pts',(-0.786422660831985,-0.333333333333333,
3.66661143271685));
#60261=CARTESIAN_POINT('Ctrl Pts',(-0.786422660831985,0.333333333333333,
3.66661143271685));
#60262=CARTESIAN_POINT('Ctrl Pts',(-0.786422660831985,0.666666666666667,
3.66661143271685));
#60263=CARTESIAN_POINT('Ctrl Pts',(-0.786422660831985,1.,3.66661143271685));
#60264=CARTESIAN_POINT('',(-0.73204283740062,1.,4.13571194405636));
#60265=CARTESIAN_POINT('',(-0.73204283740062,0.,4.13571194405636));
#60266=CARTESIAN_POINT('Ctrl Pts',(-0.786422660831985,1.,3.66661143271685));
#60267=CARTESIAN_POINT('Ctrl Pts',(-0.786459983895432,1.,3.6666431041522));
#60268=CARTESIAN_POINT('Ctrl Pts',(-0.786565919558984,1.,3.66680946938292));
#60269=CARTESIAN_POINT('Ctrl Pts',(-0.786774337198062,1.,3.66743103898702));
#60270=CARTESIAN_POINT('Ctrl Pts',(-0.787145041181546,1.,3.66907505398677));
#60271=CARTESIAN_POINT('Ctrl Pts',(-0.787758799995743,1.,3.67252923663655));
#60272=CARTESIAN_POINT('Ctrl Pts',(-0.788569566220285,1.,3.67777119516252));
#60273=CARTESIAN_POINT('Ctrl Pts',(-0.789483546064387,1.,3.68428439783905));
#60274=CARTESIAN_POINT('Ctrl Pts',(-0.790436284988788,1.,3.69172044327364));
#60275=CARTESIAN_POINT('Ctrl Pts',(-0.79135657569598,1.,3.69968940808721));
#60276=CARTESIAN_POINT('Ctrl Pts',(-0.792177688845818,1.,3.70781724021806));
#60277=CARTESIAN_POINT('Ctrl Pts',(-0.792848377370287,1.,3.71580242396124));
#60278=CARTESIAN_POINT('Ctrl Pts',(-0.793347023784205,1.,3.72348797293734));
#60279=CARTESIAN_POINT('Ctrl Pts',(-0.793682750269684,1.,3.73086914695805));
#60280=CARTESIAN_POINT('Ctrl Pts',(-0.793882700937017,1.,3.73803280541687));
#60281=CARTESIAN_POINT('Ctrl Pts',(-0.793982700459952,1.,3.74511357728861));
#60282=CARTESIAN_POINT('Ctrl Pts',(-0.794017347371377,1.,3.75224692493864));
#60283=CARTESIAN_POINT('Ctrl Pts',(-0.794008429134907,1.,3.75951468666257));
#60284=CARTESIAN_POINT('Ctrl Pts',(-0.793961083688992,1.,3.76692626931111));
#60285=CARTESIAN_POINT('Ctrl Pts',(-0.793870523787408,1.,3.77444863801212));
#60286=CARTESIAN_POINT('Ctrl Pts',(-0.7937262357813,1.,3.78202460377598));
#60287=CARTESIAN_POINT('Ctrl Pts',(-0.793516871680993,1.,3.78959439439235));
#60288=CARTESIAN_POINT('Ctrl Pts',(-0.793235612973273,1.,3.79711921389897));
#60289=CARTESIAN_POINT('Ctrl Pts',(-0.792882695234778,1.,3.80459229925637));
#60290=CARTESIAN_POINT('Ctrl Pts',(-0.792462483517634,1.,3.81202588694756));
#60291=CARTESIAN_POINT('Ctrl Pts',(-0.791981740718635,1.,3.81944345442249));
#60292=CARTESIAN_POINT('Ctrl Pts',(-0.791447528662369,1.,3.82687033899792));
#60293=CARTESIAN_POINT('Ctrl Pts',(-0.790865012705301,1.,3.83432392054786));
#60294=CARTESIAN_POINT('Ctrl Pts',(-0.790236124191242,1.,3.84180762342454));
#60295=CARTESIAN_POINT('Ctrl Pts',(-0.789560798155582,1.,3.84931637808894));
#60296=CARTESIAN_POINT('Ctrl Pts',(-0.788837734090672,1.,3.85683995872529));
#60297=CARTESIAN_POINT('Ctrl Pts',(-0.788065315093778,1.,3.86436702561345));
#60298=CARTESIAN_POINT('Ctrl Pts',(-0.787242527617999,1.,3.87188916600912));
#60299=CARTESIAN_POINT('Ctrl Pts',(-0.786369675812609,1.,3.8794040281819));
#60300=CARTESIAN_POINT('Ctrl Pts',(-0.78544789034073,1.,3.88691313167398));
#60301=CARTESIAN_POINT('Ctrl Pts',(-0.784478799358336,1.,3.89442039235103));
#60302=CARTESIAN_POINT('Ctrl Pts',(-0.783464141529081,1.,3.9019303904397));
#60303=CARTESIAN_POINT('Ctrl Pts',(-0.782405395622764,1.,3.90944671004542));
#60304=CARTESIAN_POINT('Ctrl Pts',(-0.781303428618367,1.,3.91697036054676));
#60305=CARTESIAN_POINT('Ctrl Pts',(-0.780158678615543,1.,3.92450058323823));
#60306=CARTESIAN_POINT('Ctrl Pts',(-0.778971308134821,1.,3.93203552473174));
#60307=CARTESIAN_POINT('Ctrl Pts',(-0.777741370568559,1.,3.93957296768103));
#60308=CARTESIAN_POINT('Ctrl Pts',(-0.776468966697921,1.,3.94711101619447));
#60309=CARTESIAN_POINT('Ctrl Pts',(-0.775154418039352,1.,3.9546488545231));
#60310=CARTESIAN_POINT('Ctrl Pts',(-0.773798212026566,1.,3.96218649639807));
#60311=CARTESIAN_POINT('Ctrl Pts',(-0.772400931772136,1.,3.96972446532772));
#60312=CARTESIAN_POINT('Ctrl Pts',(-0.770963190030471,1.,3.97726349165488));
#60313=CARTESIAN_POINT('Ctrl Pts',(-0.769485566245544,1.,3.98480422348451));
#60314=CARTESIAN_POINT('Ctrl Pts',(-0.767968531377915,1.,3.9923468788101));
#60315=CARTESIAN_POINT('Ctrl Pts',(-0.766412457136064,1.,3.99989129179622));
#60316=CARTESIAN_POINT('Ctrl Pts',(-0.764817648785198,1.,4.00743706791509));
#60317=CARTESIAN_POINT('Ctrl Pts',(-0.763184371182935,1.,4.01498370680496));
#60318=CARTESIAN_POINT('Ctrl Pts',(-0.761512875859804,1.,4.02253072741268));
#60319=CARTESIAN_POINT('Ctrl Pts',(-0.759803433243752,1.,4.03007781954412));
#60320=CARTESIAN_POINT('Ctrl Pts',(-0.758056338884944,1.,4.03762485803119));
#60321=CARTESIAN_POINT('Ctrl Pts',(-0.756271902369581,1.,4.04517182653997));
#60322=CARTESIAN_POINT('Ctrl Pts',(-0.754450441816078,1.,4.05271876687915));
#60323=CARTESIAN_POINT('Ctrl Pts',(-0.752592276483072,1.,4.06026572221515));
#60324=CARTESIAN_POINT('Ctrl Pts',(-0.750697720484036,1.,4.06781267242378));
#60325=CARTESIAN_POINT('Ctrl Pts',(-0.748767076680557,1.,4.07535951056152));
#60326=CARTESIAN_POINT('Ctrl Pts',(-0.746800631492315,1.,4.08290608095642));
#60327=CARTESIAN_POINT('Ctrl Pts',(-0.7447986497065,1.,4.09045220253573));
#60328=CARTESIAN_POINT('Ctrl Pts',(-0.742761369689841,1.,4.09799769702611));
#60329=CARTESIAN_POINT('Ctrl Pts',(-0.740688998553377,1.,4.10554241757547));
#60330=CARTESIAN_POINT('Ctrl Pts',(-0.738581708225844,1.,4.11308626951927));
#60331=CARTESIAN_POINT('Ctrl Pts',(-0.736439634331345,1.,4.120629196238));
#60332=CARTESIAN_POINT('Ctrl Pts',(-0.734698226764092,1.,4.12666277570844));
#60333=CARTESIAN_POINT('Ctrl Pts',(-0.733376589323546,1.,4.13118752795207));
#60334=CARTESIAN_POINT('Ctrl Pts',(-0.73248857513516,1.,4.1342038373684));
#60335=CARTESIAN_POINT('Ctrl Pts',(-0.73204283740062,1.,4.13571194405636));
#60336=CARTESIAN_POINT('Origin',(-0.73204283740062,0.,4.13571194405636));
#60337=CARTESIAN_POINT('',(-0.581791163835815,1.,4.15950947128175));
#60338=CARTESIAN_POINT('Origin',(0.,0.,0.));
#60339=CARTESIAN_POINT('',(-0.963899035117249,1.,3.62400312501245));
#60340=CARTESIAN_POINT('Origin',(0.,1.,0.));
#60341=CARTESIAN_POINT('Ctrl Pts',(-0.963899035117249,1.,3.62400312501245));
#60342=CARTESIAN_POINT('Ctrl Pts',(-0.963899035117249,0.666666666666667,
3.62400312501245));
#60343=CARTESIAN_POINT('Ctrl Pts',(-0.963899035117249,0.333333333333333,
3.62400312501245));
#60344=CARTESIAN_POINT('Ctrl Pts',(-0.963899035117249,-0.333333333333333,
3.62400312501245));
#60345=CARTESIAN_POINT('Ctrl Pts',(-0.963899035117249,-0.666666666666667,
3.62400312501245));
#60346=CARTESIAN_POINT('Ctrl Pts',(-0.963899035117249,-1.,3.62400312501245));
#60347=CARTESIAN_POINT('Ctrl Pts',(-1.22531898815164,-1.,4.01728681790024));
#60348=CARTESIAN_POINT('Ctrl Pts',(-1.22531898815164,1.,4.01728681790024));
#60349=CARTESIAN_POINT('Ctrl Pts',(-1.22423716681447,-1.,4.0161454457032));
#60350=CARTESIAN_POINT('Ctrl Pts',(-1.22423716681447,1.,4.0161454457032));
#60351=CARTESIAN_POINT('Ctrl Pts',(-1.22207656456199,-1.,4.01386104434674));
#60352=CARTESIAN_POINT('Ctrl Pts',(-1.22207656456199,1.,4.01386104434674));
#60353=CARTESIAN_POINT('Ctrl Pts',(-1.21884478244983,-1.,4.01042947142681));
#60354=CARTESIAN_POINT('Ctrl Pts',(-1.21884478244983,1.,4.01042947142681));
#60355=CARTESIAN_POINT('Ctrl Pts',(-1.21455398918813,-1.,4.00584409524937));
#60356=CARTESIAN_POINT('Ctrl Pts',(-1.21455398918813,1.,4.00584409524937));
#60357=CARTESIAN_POINT('Ctrl Pts',(-1.20922097030107,-1.,4.00009577952534));
#60358=CARTESIAN_POINT('Ctrl Pts',(-1.20922097030107,1.,4.00009577952534));
#60359=CARTESIAN_POINT('Ctrl Pts',(-1.2039185237544,-1.,3.99433084800649));
#60360=CARTESIAN_POINT('Ctrl Pts',(-1.2039185237544,1.,3.99433084800649));
#60361=CARTESIAN_POINT('Ctrl Pts',(-1.19864679609596,-1.,3.98854928957287));
#60362=CARTESIAN_POINT('Ctrl Pts',(-1.19864679609596,1.,3.98854928957287));
#60363=CARTESIAN_POINT('Ctrl Pts',(-1.19340598349307,-1.,3.98275111052015));
#60364=CARTESIAN_POINT('Ctrl Pts',(-1.19340598349307,1.,3.98275111052015));
#60365=CARTESIAN_POINT('Ctrl Pts',(-1.18819633715285,-1.,3.97693634766926));
#60366=CARTESIAN_POINT('Ctrl Pts',(-1.18819633715285,1.,3.97693634766926));
#60367=CARTESIAN_POINT('Ctrl Pts',(-1.18301815039596,-1.,3.9711050516465));
#60368=CARTESIAN_POINT('Ctrl Pts',(-1.18301815039596,1.,3.9711050516465));
#60369=CARTESIAN_POINT('Ctrl Pts',(-1.17787174135445,-1.,3.96525726357682));
#60370=CARTESIAN_POINT('Ctrl Pts',(-1.17787174135445,1.,3.96525726357682));
#60371=CARTESIAN_POINT('Ctrl Pts',(-1.17275743590327,-1.,3.95939299213164));
#60372=CARTESIAN_POINT('Ctrl Pts',(-1.17275743590327,1.,3.95939299213164));
#60373=CARTESIAN_POINT('Ctrl Pts',(-1.16767555244495,-1.,3.95351219510062));
#60374=CARTESIAN_POINT('Ctrl Pts',(-1.16767555244495,1.,3.95351219510062));
#60375=CARTESIAN_POINT('Ctrl Pts',(-1.16262637999261,-1.,3.9476147478092));
#60376=CARTESIAN_POINT('Ctrl Pts',(-1.16262637999261,1.,3.9476147478092));
#60377=CARTESIAN_POINT('Ctrl Pts',(-1.1576101834106,-1.,3.94170046685542));
#60378=CARTESIAN_POINT('Ctrl Pts',(-1.1576101834106,1.,3.94170046685542));
#60379=CARTESIAN_POINT('Ctrl Pts',(-1.15262722716391,-1.,3.9357691705651));
#60380=CARTESIAN_POINT('Ctrl Pts',(-1.15262722716391,1.,3.9357691705651));
#60381=CARTESIAN_POINT('Ctrl Pts',(-1.14767779451147,-1.,3.92982073294334));
#60382=CARTESIAN_POINT('Ctrl Pts',(-1.14767779451147,1.,3.92982073294334));
#60383=CARTESIAN_POINT('Ctrl Pts',(-1.14276220561575,-1.,3.92385513133937));
#60384=CARTESIAN_POINT('Ctrl Pts',(-1.14276220561575,1.,3.92385513133937));
#60385=CARTESIAN_POINT('Ctrl Pts',(-1.13788084225511,-1.,3.91787251936688));
#60386=CARTESIAN_POINT('Ctrl Pts',(-1.13788084225511,1.,3.91787251936688));
#60387=CARTESIAN_POINT('Ctrl Pts',(-1.13303414693849,-1.,3.91187321145495));
#60388=CARTESIAN_POINT('Ctrl Pts',(-1.13303414693849,1.,3.91187321145495));
#60389=CARTESIAN_POINT('Ctrl Pts',(-1.12822258281518,-1.,3.90585753318622));
#60390=CARTESIAN_POINT('Ctrl Pts',(-1.12822258281518,1.,3.90585753318622));
#60391=CARTESIAN_POINT('Ctrl Pts',(-1.12344660099029,-1.,3.89982569749978));
#60392=CARTESIAN_POINT('Ctrl Pts',(-1.12344660099029,1.,3.89982569749978));
#60393=CARTESIAN_POINT('Ctrl Pts',(-1.11870660794609,-1.,3.89377768340362));
#60394=CARTESIAN_POINT('Ctrl Pts',(-1.11870660794609,1.,3.89377768340362));
#60395=CARTESIAN_POINT('Ctrl Pts',(-1.11400292434447,-1.,3.88771308285229));
#60396=CARTESIAN_POINT('Ctrl Pts',(-1.11400292434447,1.,3.88771308285229));
#60397=CARTESIAN_POINT('Ctrl Pts',(-1.10933577224029,-1.,3.88163105531791));
#60398=CARTESIAN_POINT('Ctrl Pts',(-1.10933577224029,1.,3.88163105531791));
#60399=CARTESIAN_POINT('Ctrl Pts',(-1.10470536603303,-1.,3.87553067187566));
#60400=CARTESIAN_POINT('Ctrl Pts',(-1.10470536603303,1.,3.87553067187566));
#60401=CARTESIAN_POINT('Ctrl Pts',(-1.10011198761202,-1.,3.86941120134872));
#60402=CARTESIAN_POINT('Ctrl Pts',(-1.10011198761202,1.,3.86941120134872));
#60403=CARTESIAN_POINT('Ctrl Pts',(-1.09555606505012,-1.,3.86327241021242));
#60404=CARTESIAN_POINT('Ctrl Pts',(-1.09555606505012,1.,3.86327241021242));
#60405=CARTESIAN_POINT('Ctrl Pts',(-1.09103825516288,-1.,3.85711487933911));
#60406=CARTESIAN_POINT('Ctrl Pts',(-1.09103825516288,1.,3.85711487933911));
#60407=CARTESIAN_POINT('Ctrl Pts',(-1.08655950846377,-1.,3.8509402522269));
#60408=CARTESIAN_POINT('Ctrl Pts',(-1.08655950846377,1.,3.8509402522269));
#60409=CARTESIAN_POINT('Ctrl Pts',(-1.08212087917986,-1.,3.84475048030615));
#60410=CARTESIAN_POINT('Ctrl Pts',(-1.08212087917986,1.,3.84475048030615));
#60411=CARTESIAN_POINT('Ctrl Pts',(-1.07772335353856,-1.,3.83854714117486));
#60412=CARTESIAN_POINT('Ctrl Pts',(-1.07772335353856,1.,3.83854714117486));
#60413=CARTESIAN_POINT('Ctrl Pts',(-1.0733676663346,-1.,3.83233071195145));
#60414=CARTESIAN_POINT('Ctrl Pts',(-1.0733676663346,1.,3.83233071195145));
#60415=CARTESIAN_POINT('Ctrl Pts',(-1.0690541318036,-1.,3.82609989967278));
#60416=CARTESIAN_POINT('Ctrl Pts',(-1.0690541318036,1.,3.82609989967278));
#60417=CARTESIAN_POINT('Ctrl Pts',(-1.06478244038931,-1.,3.81985083953012));
#60418=CARTESIAN_POINT('Ctrl Pts',(-1.06478244038931,1.,3.81985083953012));
#60419=CARTESIAN_POINT('Ctrl Pts',(-1.06055206187298,-1.,3.81357866117485));
#60420=CARTESIAN_POINT('Ctrl Pts',(-1.06055206187298,1.,3.81357866117485));
#60421=CARTESIAN_POINT('Ctrl Pts',(-1.05636266918643,-1.,3.80727913637784));
#60422=CARTESIAN_POINT('Ctrl Pts',(-1.05636266918643,1.,3.80727913637784));
#60423=CARTESIAN_POINT('Ctrl Pts',(-1.05221457990015,-1.,3.80095039790678));
#60424=CARTESIAN_POINT('Ctrl Pts',(-1.05221457990015,1.,3.80095039790678));
#60425=CARTESIAN_POINT('Ctrl Pts',(-1.04810913267641,-1.,3.79459440308793));
#60426=CARTESIAN_POINT('Ctrl Pts',(-1.04810913267641,1.,3.79459440308793));
#60427=CARTESIAN_POINT('Ctrl Pts',(-1.04404924374426,-1.,3.78821910787195));
#60428=CARTESIAN_POINT('Ctrl Pts',(-1.04404924374426,1.,3.78821910787195));
#60429=CARTESIAN_POINT('Ctrl Pts',(-1.04003862055804,-1.,3.78183535008192));
#60430=CARTESIAN_POINT('Ctrl Pts',(-1.04003862055804,1.,3.78183535008192));
#60431=CARTESIAN_POINT('Ctrl Pts',(-1.03608074678013,-1.,3.77545283140445));
#60432=CARTESIAN_POINT('Ctrl Pts',(-1.03608074678013,1.,3.77545283140445));
#60433=CARTESIAN_POINT('Ctrl Pts',(-1.0321778660492,-1.,3.76907609832522));
#60434=CARTESIAN_POINT('Ctrl Pts',(-1.0321778660492,1.,3.76907609832522));
#60435=CARTESIAN_POINT('Ctrl Pts',(-1.02833014458181,-1.,3.76270122291232));
#60436=CARTESIAN_POINT('Ctrl Pts',(-1.02833014458181,1.,3.76270122291232));
#60437=CARTESIAN_POINT('Ctrl Pts',(-1.0245342944466,-1.,3.75631037456194));
#60438=CARTESIAN_POINT('Ctrl Pts',(-1.0245342944466,1.,3.75631037456194));
#60439=CARTESIAN_POINT('Ctrl Pts',(-1.02078510487428,-1.,3.74987777155834));
#60440=CARTESIAN_POINT('Ctrl Pts',(-1.02078510487428,1.,3.74987777155834));
#60441=CARTESIAN_POINT('Ctrl Pts',(-1.01707794311079,-1.,3.74337942504959));
#60442=CARTESIAN_POINT('Ctrl Pts',(-1.01707794311079,1.,3.74337942504959));
#60443=CARTESIAN_POINT('Ctrl Pts',(-1.01341114319903,-1.,3.73680245055734));
#60444=CARTESIAN_POINT('Ctrl Pts',(-1.01341114319903,1.,3.73680245055734));
#60445=CARTESIAN_POINT('Ctrl Pts',(-1.00978798539496,-1.,3.73015276704426));
#60446=CARTESIAN_POINT('Ctrl Pts',(-1.00978798539496,1.,3.73015276704426));
#60447=CARTESIAN_POINT('Ctrl Pts',(-1.0062200073571,-1.,3.72346803750595));
#60448=CARTESIAN_POINT('Ctrl Pts',(-1.0062200073571,1.,3.72346803750595));
#60449=CARTESIAN_POINT('Ctrl Pts',(-1.00272423396822,-1.,3.71680667125118));
#60450=CARTESIAN_POINT('Ctrl Pts',(-1.00272423396822,1.,3.71680667125118));
#60451=CARTESIAN_POINT('Ctrl Pts',(-0.999317260756531,-1.,3.71022439713938));
#60452=CARTESIAN_POINT('Ctrl Pts',(-0.999317260756531,1.,3.71022439713938));
#60453=CARTESIAN_POINT('Ctrl Pts',(-0.996009819772518,-1.,3.70375282282138));
#60454=CARTESIAN_POINT('Ctrl Pts',(-0.996009819772518,1.,3.70375282282138));
#60455=CARTESIAN_POINT('Ctrl Pts',(-0.99280221833201,-1.,3.69738123415662));
#60456=CARTESIAN_POINT('Ctrl Pts',(-0.99280221833201,1.,3.69738123415662));
#60457=CARTESIAN_POINT('Ctrl Pts',(-0.989676715398558,-1.,3.69102682138846));
#60458=CARTESIAN_POINT('Ctrl Pts',(-0.989676715398558,1.,3.69102682138846));
#60459=CARTESIAN_POINT('Ctrl Pts',(-0.986602639863838,-1.,3.68455317926068));
#60460=CARTESIAN_POINT('Ctrl Pts',(-0.986602639863838,1.,3.68455317926068));
#60461=CARTESIAN_POINT('Ctrl Pts',(-0.983550791470419,-1.,3.67782408841715));
#60462=CARTESIAN_POINT('Ctrl Pts',(-0.983550791470419,1.,3.67782408841715));
#60463=CARTESIAN_POINT('Ctrl Pts',(-0.980505922458267,-1.,3.67074983340361));
#60464=CARTESIAN_POINT('Ctrl Pts',(-0.980505922458267,1.,3.67074983340361));
#60465=CARTESIAN_POINT('Ctrl Pts',(-0.977478312751618,-1.,3.66333049637475));
#60466=CARTESIAN_POINT('Ctrl Pts',(-0.977478312751618,1.,3.66333049637475));
#60467=CARTESIAN_POINT('Ctrl Pts',(-0.974519971354848,-1.,3.65571576735126));
#60468=CARTESIAN_POINT('Ctrl Pts',(-0.974519971354848,1.,3.65571576735126));
#60469=CARTESIAN_POINT('Ctrl Pts',(-0.971722122061341,-1.,3.64819756447455));
#60470=CARTESIAN_POINT('Ctrl Pts',(-0.971722122061341,1.,3.64819756447455));
#60471=CARTESIAN_POINT('Ctrl Pts',(-0.969195124675866,-1.,3.64113946505766));
#60472=CARTESIAN_POINT('Ctrl Pts',(-0.969195124675866,1.,3.64113946505766));
#60473=CARTESIAN_POINT('Ctrl Pts',(-0.967052554541386,-1.,3.63492122081143));
#60474=CARTESIAN_POINT('Ctrl Pts',(-0.967052554541386,1.,3.63492122081143));
#60475=CARTESIAN_POINT('Ctrl Pts',(-0.965395153165293,-1.,3.62988252139846));
#60476=CARTESIAN_POINT('Ctrl Pts',(-0.965395153165293,1.,3.62988252139846));
#60477=CARTESIAN_POINT('Ctrl Pts',(-0.964291001273288,-1.,3.62625391254797));
#60478=CARTESIAN_POINT('Ctrl Pts',(-0.964291001273288,1.,3.62625391254797));
#60479=CARTESIAN_POINT('Ctrl Pts',(-0.963875774530619,-1.,3.6245656860652));
#60480=CARTESIAN_POINT('Ctrl Pts',(-0.963875774530619,1.,3.6245656860652));
#60481=CARTESIAN_POINT('Ctrl Pts',(-0.963832486395051,-1.,3.62399933639914));
#60482=CARTESIAN_POINT('Ctrl Pts',(-0.963832486395051,1.,3.62399933639914));
#60483=CARTESIAN_POINT('Ctrl Pts',(-0.963922720982193,-1.,3.62393257642052));
#60484=CARTESIAN_POINT('Ctrl Pts',(-0.963922720982193,1.,3.62393257642052));
#60485=CARTESIAN_POINT('Ctrl Pts',(-0.963997613369571,-1.,3.62397690409552));
#60486=CARTESIAN_POINT('Ctrl Pts',(-0.963997613369571,1.,3.62397690409552));
#60487=CARTESIAN_POINT('',(-1.22531898815164,1.,4.01728681790024));
#60488=CARTESIAN_POINT('Ctrl Pts',(-1.22531898815164,1.,4.01728681790024));
#60489=CARTESIAN_POINT('Ctrl Pts',(-1.22423716681447,1.,4.0161454457032));
#60490=CARTESIAN_POINT('Ctrl Pts',(-1.22207656456199,1.,4.01386104434674));
#60491=CARTESIAN_POINT('Ctrl Pts',(-1.21884478244983,1.,4.01042947142681));
#60492=CARTESIAN_POINT('Ctrl Pts',(-1.21455398918813,1.,4.00584409524937));
#60493=CARTESIAN_POINT('Ctrl Pts',(-1.20922097030107,1.,4.00009577952534));
#60494=CARTESIAN_POINT('Ctrl Pts',(-1.2039185237544,1.,3.99433084800649));
#60495=CARTESIAN_POINT('Ctrl Pts',(-1.19864679609596,1.,3.98854928957287));
#60496=CARTESIAN_POINT('Ctrl Pts',(-1.19340598349307,1.,3.98275111052015));
#60497=CARTESIAN_POINT('Ctrl Pts',(-1.18819633715285,1.,3.97693634766926));
#60498=CARTESIAN_POINT('Ctrl Pts',(-1.18301815039596,1.,3.9711050516465));
#60499=CARTESIAN_POINT('Ctrl Pts',(-1.17787174135445,1.,3.96525726357682));
#60500=CARTESIAN_POINT('Ctrl Pts',(-1.17275743590327,1.,3.95939299213164));
#60501=CARTESIAN_POINT('Ctrl Pts',(-1.16767555244495,1.,3.95351219510062));
#60502=CARTESIAN_POINT('Ctrl Pts',(-1.16262637999261,1.,3.9476147478092));
#60503=CARTESIAN_POINT('Ctrl Pts',(-1.1576101834106,1.,3.94170046685542));
#60504=CARTESIAN_POINT('Ctrl Pts',(-1.15262722716391,1.,3.9357691705651));
#60505=CARTESIAN_POINT('Ctrl Pts',(-1.14767779451147,1.,3.92982073294334));
#60506=CARTESIAN_POINT('Ctrl Pts',(-1.14276220561575,1.,3.92385513133937));
#60507=CARTESIAN_POINT('Ctrl Pts',(-1.13788084225511,1.,3.91787251936688));
#60508=CARTESIAN_POINT('Ctrl Pts',(-1.13303414693849,1.,3.91187321145495));
#60509=CARTESIAN_POINT('Ctrl Pts',(-1.12822258281518,1.,3.90585753318622));
#60510=CARTESIAN_POINT('Ctrl Pts',(-1.12344660099029,1.,3.89982569749978));
#60511=CARTESIAN_POINT('Ctrl Pts',(-1.11870660794609,1.,3.89377768340362));
#60512=CARTESIAN_POINT('Ctrl Pts',(-1.11400292434447,1.,3.88771308285229));
#60513=CARTESIAN_POINT('Ctrl Pts',(-1.10933577224029,1.,3.88163105531791));
#60514=CARTESIAN_POINT('Ctrl Pts',(-1.10470536603303,1.,3.87553067187566));
#60515=CARTESIAN_POINT('Ctrl Pts',(-1.10011198761202,1.,3.86941120134872));
#60516=CARTESIAN_POINT('Ctrl Pts',(-1.09555606505012,1.,3.86327241021242));
#60517=CARTESIAN_POINT('Ctrl Pts',(-1.09103825516288,1.,3.85711487933911));
#60518=CARTESIAN_POINT('Ctrl Pts',(-1.08655950846377,1.,3.8509402522269));
#60519=CARTESIAN_POINT('Ctrl Pts',(-1.08212087917986,1.,3.84475048030615));
#60520=CARTESIAN_POINT('Ctrl Pts',(-1.07772335353856,1.,3.83854714117486));
#60521=CARTESIAN_POINT('Ctrl Pts',(-1.0733676663346,1.,3.83233071195145));
#60522=CARTESIAN_POINT('Ctrl Pts',(-1.0690541318036,1.,3.82609989967278));
#60523=CARTESIAN_POINT('Ctrl Pts',(-1.06478244038931,1.,3.81985083953012));
#60524=CARTESIAN_POINT('Ctrl Pts',(-1.06055206187298,1.,3.81357866117485));
#60525=CARTESIAN_POINT('Ctrl Pts',(-1.05636266918643,1.,3.80727913637784));
#60526=CARTESIAN_POINT('Ctrl Pts',(-1.05221457990015,1.,3.80095039790678));
#60527=CARTESIAN_POINT('Ctrl Pts',(-1.04810913267641,1.,3.79459440308793));
#60528=CARTESIAN_POINT('Ctrl Pts',(-1.04404924374426,1.,3.78821910787195));
#60529=CARTESIAN_POINT('Ctrl Pts',(-1.04003862055804,1.,3.78183535008192));
#60530=CARTESIAN_POINT('Ctrl Pts',(-1.03608074678013,1.,3.77545283140445));
#60531=CARTESIAN_POINT('Ctrl Pts',(-1.0321778660492,1.,3.76907609832522));
#60532=CARTESIAN_POINT('Ctrl Pts',(-1.02833014458181,1.,3.76270122291232));
#60533=CARTESIAN_POINT('Ctrl Pts',(-1.0245342944466,1.,3.75631037456194));
#60534=CARTESIAN_POINT('Ctrl Pts',(-1.02078510487428,1.,3.74987777155834));
#60535=CARTESIAN_POINT('Ctrl Pts',(-1.01707794311079,1.,3.74337942504959));
#60536=CARTESIAN_POINT('Ctrl Pts',(-1.01341114319903,1.,3.73680245055734));
#60537=CARTESIAN_POINT('Ctrl Pts',(-1.00978798539496,1.,3.73015276704426));
#60538=CARTESIAN_POINT('Ctrl Pts',(-1.0062200073571,1.,3.72346803750595));
#60539=CARTESIAN_POINT('Ctrl Pts',(-1.00272423396822,1.,3.71680667125118));
#60540=CARTESIAN_POINT('Ctrl Pts',(-0.999317260756531,1.,3.71022439713938));
#60541=CARTESIAN_POINT('Ctrl Pts',(-0.996009819772518,1.,3.70375282282138));
#60542=CARTESIAN_POINT('Ctrl Pts',(-0.99280221833201,1.,3.69738123415662));
#60543=CARTESIAN_POINT('Ctrl Pts',(-0.989676715398558,1.,3.69102682138846));
#60544=CARTESIAN_POINT('Ctrl Pts',(-0.986602639863838,1.,3.68455317926068));
#60545=CARTESIAN_POINT('Ctrl Pts',(-0.983550791470419,1.,3.67782408841715));
#60546=CARTESIAN_POINT('Ctrl Pts',(-0.980505922458267,1.,3.67074983340361));
#60547=CARTESIAN_POINT('Ctrl Pts',(-0.977478312751618,1.,3.66333049637475));
#60548=CARTESIAN_POINT('Ctrl Pts',(-0.974519971354848,1.,3.65571576735126));
#60549=CARTESIAN_POINT('Ctrl Pts',(-0.971722122061341,1.,3.64819756447455));
#60550=CARTESIAN_POINT('Ctrl Pts',(-0.969195124675866,1.,3.64113946505766));
#60551=CARTESIAN_POINT('Ctrl Pts',(-0.967052554541386,1.,3.63492122081143));
#60552=CARTESIAN_POINT('Ctrl Pts',(-0.965395153165293,1.,3.62988252139846));
#60553=CARTESIAN_POINT('Ctrl Pts',(-0.964373850166457,1.,3.62652618145335));
#60554=CARTESIAN_POINT('Ctrl Pts',(-0.963957782642843,1.,3.62489305727662));
#60555=CARTESIAN_POINT('Ctrl Pts',(-0.963861297423241,1.,3.62424461507588));
#60556=CARTESIAN_POINT('Ctrl Pts',(-0.963880158555582,1.,3.6240482887845));
#60557=CARTESIAN_POINT('Ctrl Pts',(-0.963899035117249,1.,3.62400312501245));
#60558=CARTESIAN_POINT('',(-1.22531898815164,0.,4.01728681790024));
#60559=CARTESIAN_POINT('Ctrl Pts',(-1.35022972712301,-1.,3.49848248301936));
#60560=CARTESIAN_POINT('Ctrl Pts',(-1.35022972712301,1.,3.49848248301936));
#60561=CARTESIAN_POINT('Ctrl Pts',(-1.35026426118402,-1.,3.4984026005375));
#60562=CARTESIAN_POINT('Ctrl Pts',(-1.35026426118402,1.,3.4984026005375));
#60563=CARTESIAN_POINT('Ctrl Pts',(-1.35037650303019,-1.,3.49840357193736));
#60564=CARTESIAN_POINT('Ctrl Pts',(-1.35037650303019,1.,3.49840357193736));
#60565=CARTESIAN_POINT('Ctrl Pts',(-1.35067437417483,-1.,3.49888720257132));
#60566=CARTESIAN_POINT('Ctrl Pts',(-1.35067437417483,1.,3.49888720257132));
#60567=CARTESIAN_POINT('Ctrl Pts',(-1.3513307633124,-1.,3.5004970706414));
#60568=CARTESIAN_POINT('Ctrl Pts',(-1.3513307633124,1.,3.5004970706414));
#60569=CARTESIAN_POINT('Ctrl Pts',(-1.35257032843486,-1.,3.50408168106261));
#60570=CARTESIAN_POINT('Ctrl Pts',(-1.35257032843486,1.,3.50408168106261));
#60571=CARTESIAN_POINT('Ctrl Pts',(-1.35419113575956,-1.,3.50913227059999));
#60572=CARTESIAN_POINT('Ctrl Pts',(-1.35419113575956,1.,3.50913227059999));
#60573=CARTESIAN_POINT('Ctrl Pts',(-1.35611275237152,-1.,3.51542230699556));
#60574=CARTESIAN_POINT('Ctrl Pts',(-1.35611275237152,1.,3.51542230699556));
#60575=CARTESIAN_POINT('Ctrl Pts',(-1.35821701528836,-1.,3.52261776116748));
#60576=CARTESIAN_POINT('Ctrl Pts',(-1.35821701528836,1.,3.52261776116748));
#60577=CARTESIAN_POINT('Ctrl Pts',(-1.36037259643734,-1.,3.530344649616));
#60578=CARTESIAN_POINT('Ctrl Pts',(-1.36037259643734,1.,3.530344649616));
#60579=CARTESIAN_POINT('Ctrl Pts',(-1.36245507339307,-1.,3.53824396424961));
#60580=CARTESIAN_POINT('Ctrl Pts',(-1.36245507339307,1.,3.53824396424961));
#60581=CARTESIAN_POINT('Ctrl Pts',(-1.36436666257598,-1.,3.54602591832973));
#60582=CARTESIAN_POINT('Ctrl Pts',(-1.36436666257598,1.,3.54602591832973));
#60583=CARTESIAN_POINT('Ctrl Pts',(-1.3660614545677,-1.,3.55353883995949));
#60584=CARTESIAN_POINT('Ctrl Pts',(-1.3660614545677,1.,3.55353883995949));
#60585=CARTESIAN_POINT('Ctrl Pts',(-1.36754771771233,-1.,3.56077662028649));
#60586=CARTESIAN_POINT('Ctrl Pts',(-1.36754771771233,1.,3.56077662028649));
#60587=CARTESIAN_POINT('Ctrl Pts',(-1.36886584973389,-1.,3.5678208030466));
#60588=CARTESIAN_POINT('Ctrl Pts',(-1.36886584973389,1.,3.5678208030466));
#60589=CARTESIAN_POINT('Ctrl Pts',(-1.37007229485659,-1.,3.57479875549486));
#60590=CARTESIAN_POINT('Ctrl Pts',(-1.37007229485659,1.,3.57479875549486));
#60591=CARTESIAN_POINT('Ctrl Pts',(-1.37122241663062,-1.,3.58183885982715));
#60592=CARTESIAN_POINT('Ctrl Pts',(-1.37122241663062,1.,3.58183885982715));
#60593=CARTESIAN_POINT('Ctrl Pts',(-1.37235053660976,-1.,3.58901853846365));
#60594=CARTESIAN_POINT('Ctrl Pts',(-1.37235053660976,1.,3.58901853846365));
#60595=CARTESIAN_POINT('Ctrl Pts',(-1.37346320103157,-1.,3.59634627869048));
#60596=CARTESIAN_POINT('Ctrl Pts',(-1.37346320103157,1.,3.59634627869048));
#60597=CARTESIAN_POINT('Ctrl Pts',(-1.37455051379623,-1.,3.60379020123988));
#60598=CARTESIAN_POINT('Ctrl Pts',(-1.37455051379623,1.,3.60379020123988));
#60599=CARTESIAN_POINT('Ctrl Pts',(-1.37559314436634,-1.,3.61129546591064));
#60600=CARTESIAN_POINT('Ctrl Pts',(-1.37559314436634,1.,3.61129546591064));
#60601=CARTESIAN_POINT('Ctrl Pts',(-1.37657053403107,-1.,3.6188048116042));
#60602=CARTESIAN_POINT('Ctrl Pts',(-1.37657053403107,1.,3.6188048116042));
#60603=CARTESIAN_POINT('Ctrl Pts',(-1.37746987919881,-1.,3.62628098665145));
#60604=CARTESIAN_POINT('Ctrl Pts',(-1.37746987919881,1.,3.62628098665145));
#60605=CARTESIAN_POINT('Ctrl Pts',(-1.37829035457339,-1.,3.63371727442486));
#60606=CARTESIAN_POINT('Ctrl Pts',(-1.37829035457339,1.,3.63371727442486));
#60607=CARTESIAN_POINT('Ctrl Pts',(-1.37903818567359,-1.,3.64112507791141));
#60608=CARTESIAN_POINT('Ctrl Pts',(-1.37903818567359,1.,3.64112507791141));
#60609=CARTESIAN_POINT('Ctrl Pts',(-1.37972372481603,-1.,3.64852652756456));
#60610=CARTESIAN_POINT('Ctrl Pts',(-1.37972372481603,1.,3.64852652756456));
#60611=CARTESIAN_POINT('Ctrl Pts',(-1.38035791051213,-1.,3.6559455440439));
#60612=CARTESIAN_POINT('Ctrl Pts',(-1.38035791051213,1.,3.6559455440439));
#60613=CARTESIAN_POINT('Ctrl Pts',(-1.38094856333552,-1.,3.66339848520857));
#60614=CARTESIAN_POINT('Ctrl Pts',(-1.38094856333552,1.,3.66339848520857));
#60615=CARTESIAN_POINT('Ctrl Pts',(-1.38149812653868,-1.,3.67088843112262));
#60616=CARTESIAN_POINT('Ctrl Pts',(-1.38149812653868,1.,3.67088843112262));
#60617=CARTESIAN_POINT('Ctrl Pts',(-1.3820057429062,-1.,3.67841038482414));
#60618=CARTESIAN_POINT('Ctrl Pts',(-1.3820057429062,1.,3.67841038482414));
#60619=CARTESIAN_POINT('Ctrl Pts',(-1.38246852827182,-1.,3.68595444983837));
#60620=CARTESIAN_POINT('Ctrl Pts',(-1.38246852827182,1.,3.68595444983837));
#60621=CARTESIAN_POINT('Ctrl Pts',(-1.38288311171651,-1.,3.69350967899526));
#60622=CARTESIAN_POINT('Ctrl Pts',(-1.38288311171651,1.,3.69350967899526));
#60623=CARTESIAN_POINT('Ctrl Pts',(-1.38324717612865,-1.,3.701067921679));
#60624=CARTESIAN_POINT('Ctrl Pts',(-1.38324717612865,1.,3.701067921679));
#60625=CARTESIAN_POINT('Ctrl Pts',(-1.38356065402124,-1.,3.70862680753347));
#60626=CARTESIAN_POINT('Ctrl Pts',(-1.38356065402124,1.,3.70862680753347));
#60627=CARTESIAN_POINT('Ctrl Pts',(-1.38382489984586,-1.,3.7161876605181));
#60628=CARTESIAN_POINT('Ctrl Pts',(-1.38382489984586,1.,3.7161876605181));
#60629=CARTESIAN_POINT('Ctrl Pts',(-1.3840421342895,-1.,3.72375409358803));
#60630=CARTESIAN_POINT('Ctrl Pts',(-1.3840421342895,1.,3.72375409358803));
#60631=CARTESIAN_POINT('Ctrl Pts',(-1.38421479111531,-1.,3.73133035859282));
#60632=CARTESIAN_POINT('Ctrl Pts',(-1.38421479111531,1.,3.73133035859282));
#60633=CARTESIAN_POINT('Ctrl Pts',(-1.38434489156458,-1.,3.73891976418104));
#60634=CARTESIAN_POINT('Ctrl Pts',(-1.38434489156458,1.,3.73891976418104));
#60635=CARTESIAN_POINT('Ctrl Pts',(-1.38443344984394,-1.,3.74652317167876));
#60636=CARTESIAN_POINT('Ctrl Pts',(-1.38443344984394,1.,3.74652317167876));
#60637=CARTESIAN_POINT('Ctrl Pts',(-1.38448077997163,-1.,3.7541397631875));
#60638=CARTESIAN_POINT('Ctrl Pts',(-1.38448077997163,1.,3.7541397631875));
#60639=CARTESIAN_POINT('Ctrl Pts',(-1.3844867525335,-1.,3.76176768271367));
#60640=CARTESIAN_POINT('Ctrl Pts',(-1.3844867525335,1.,3.76176768271367));
#60641=CARTESIAN_POINT('Ctrl Pts',(-1.38445107339518,-1.,3.76940473185779));
#60642=CARTESIAN_POINT('Ctrl Pts',(-1.38445107339518,1.,3.76940473185779));
#60643=CARTESIAN_POINT('Ctrl Pts',(-1.38437354551428,-1.,3.77704902230418));
#60644=CARTESIAN_POINT('Ctrl Pts',(-1.38437354551428,1.,3.77704902230418));
#60645=CARTESIAN_POINT('Ctrl Pts',(-1.38425435883756,-1.,3.78469969805082));
#60646=CARTESIAN_POINT('Ctrl Pts',(-1.38425435883756,1.,3.78469969805082));
#60647=CARTESIAN_POINT('Ctrl Pts',(-1.38409399694566,-1.,3.79235669640841));
#60648=CARTESIAN_POINT('Ctrl Pts',(-1.38409399694566,1.,3.79235669640841));
#60649=CARTESIAN_POINT('Ctrl Pts',(-1.38389311766682,-1.,3.80002044322111));
#60650=CARTESIAN_POINT('Ctrl Pts',(-1.38389311766682,1.,3.80002044322111));
#60651=CARTESIAN_POINT('Ctrl Pts',(-1.3836524404622,-1.,3.80769156398411));
#60652=CARTESIAN_POINT('Ctrl Pts',(-1.3836524404622,1.,3.80769156398411));
#60653=CARTESIAN_POINT('Ctrl Pts',(-1.38337263902782,-1.,3.81537060817811));
#60654=CARTESIAN_POINT('Ctrl Pts',(-1.38337263902782,1.,3.81537060817811));
#60655=CARTESIAN_POINT('Ctrl Pts',(-1.38305421262763,-1.,3.82305771743829));
#60656=CARTESIAN_POINT('Ctrl Pts',(-1.38305421262763,1.,3.82305771743829));
#60657=CARTESIAN_POINT('Ctrl Pts',(-1.38269750245138,-1.,3.8307526698229));
#60658=CARTESIAN_POINT('Ctrl Pts',(-1.38269750245138,1.,3.8307526698229));
#60659=CARTESIAN_POINT('Ctrl Pts',(-1.38230274828822,-1.,3.83845502790746));
#60660=CARTESIAN_POINT('Ctrl Pts',(-1.38230274828822,1.,3.83845502790746));
#60661=CARTESIAN_POINT('Ctrl Pts',(-1.38187013346109,-1.,3.84616425605764));
#60662=CARTESIAN_POINT('Ctrl Pts',(-1.38187013346109,1.,3.84616425605764));
#60663=CARTESIAN_POINT('Ctrl Pts',(-1.38139983115049,-1.,3.85387983979481));
#60664=CARTESIAN_POINT('Ctrl Pts',(-1.38139983115049,1.,3.85387983979481));
#60665=CARTESIAN_POINT('Ctrl Pts',(-1.38089205992989,-1.,3.86160143043959));
#60666=CARTESIAN_POINT('Ctrl Pts',(-1.38089205992989,1.,3.86160143043959));
#60667=CARTESIAN_POINT('Ctrl Pts',(-1.38034709213014,-1.,3.86932885813068));
#60668=CARTESIAN_POINT('Ctrl Pts',(-1.38034709213014,1.,3.86932885813068));
#60669=CARTESIAN_POINT('Ctrl Pts',(-1.37976523097073,-1.,3.87706205830532));
#60670=CARTESIAN_POINT('Ctrl Pts',(-1.37976523097073,1.,3.87706205830532));
#60671=CARTESIAN_POINT('Ctrl Pts',(-1.37914679719383,-1.,3.88480102249277));
#60672=CARTESIAN_POINT('Ctrl Pts',(-1.37914679719383,1.,3.88480102249277));
#60673=CARTESIAN_POINT('Ctrl Pts',(-1.3784921128802,-1.,3.89254574338496));
#60674=CARTESIAN_POINT('Ctrl Pts',(-1.3784921128802,1.,3.89254574338496));
#60675=CARTESIAN_POINT('Ctrl Pts',(-1.37780148512792,-1.,3.90029615196727));
#60676=CARTESIAN_POINT('Ctrl Pts',(-1.37780148512792,1.,3.90029615196727));
#60677=CARTESIAN_POINT('Ctrl Pts',(-1.3770751963402,-1.,3.90805209523486));
#60678=CARTESIAN_POINT('Ctrl Pts',(-1.3770751963402,1.,3.90805209523486));
#60679=CARTESIAN_POINT('Ctrl Pts',(-1.37631350505797,-1.,3.91581337462644));
#60680=CARTESIAN_POINT('Ctrl Pts',(-1.37631350505797,1.,3.91581337462644));
#60681=CARTESIAN_POINT('Ctrl Pts',(-1.37551664448242,-1.,3.92357976987672));
#60682=CARTESIAN_POINT('Ctrl Pts',(-1.37551664448242,1.,3.92357976987672));
#60683=CARTESIAN_POINT('Ctrl Pts',(-1.37468482215751,-1.,3.93135106761844));
#60684=CARTESIAN_POINT('Ctrl Pts',(-1.37468482215751,1.,3.93135106761844));
#60685=CARTESIAN_POINT('Ctrl Pts',(-1.37381821967165,-1.,3.93912709040818));
#60686=CARTESIAN_POINT('Ctrl Pts',(-1.37381821967165,1.,3.93912709040818));
#60687=CARTESIAN_POINT('Ctrl Pts',(-1.37291699202807,-1.,3.94690771785133));
#60688=CARTESIAN_POINT('Ctrl Pts',(-1.37291699202807,1.,3.94690771785133));
#60689=CARTESIAN_POINT('Ctrl Pts',(-1.37198126432386,-1.,3.95469287280914));
#60690=CARTESIAN_POINT('Ctrl Pts',(-1.37198126432386,1.,3.95469287280914));
#60691=CARTESIAN_POINT('Ctrl Pts',(-1.3712051561502,-1.,3.96092458506535));
#60692=CARTESIAN_POINT('Ctrl Pts',(-1.3712051561502,1.,3.96092458506535));
#60693=CARTESIAN_POINT('Ctrl Pts',(-1.37060761745635,-1.,3.96560037974645));
#60694=CARTESIAN_POINT('Ctrl Pts',(-1.37060761745635,1.,3.96560037974645));
#60695=CARTESIAN_POINT('Ctrl Pts',(-1.37020239094614,-1.,3.9687184694131));
#60696=CARTESIAN_POINT('Ctrl Pts',(-1.37020239094614,1.,3.9687184694131));
#60697=CARTESIAN_POINT('Ctrl Pts',(-1.36999806084572,-1.,3.97027773754922));
#60698=CARTESIAN_POINT('Ctrl Pts',(-1.36999806084572,1.,3.97027773754922));
#60699=CARTESIAN_POINT('',(-1.35032489087101,1.,3.4984457533445));
#60700=CARTESIAN_POINT('Ctrl Pts',(-1.35032489087101,-1.,3.4984457533445));
#60701=CARTESIAN_POINT('Ctrl Pts',(-1.35032489087101,-0.666666666666667,
3.4984457533445));
#60702=CARTESIAN_POINT('Ctrl Pts',(-1.35032489087101,-0.333333333333333,
3.4984457533445));
#60703=CARTESIAN_POINT('Ctrl Pts',(-1.35032489087101,0.333333333333333,
3.4984457533445));
#60704=CARTESIAN_POINT('Ctrl Pts',(-1.35032489087101,0.666666666666667,
3.4984457533445));
#60705=CARTESIAN_POINT('Ctrl Pts',(-1.35032489087101,1.,3.4984457533445));
#60706=CARTESIAN_POINT('',(-1.36999806084572,1.,3.97027773754922));
#60707=CARTESIAN_POINT('',(-1.36999806084572,0.,3.97027773754922));
#60708=CARTESIAN_POINT('Ctrl Pts',(-1.35032489087101,1.,3.4984457533445));
#60709=CARTESIAN_POINT('Ctrl Pts',(-1.35036670892966,1.,3.49847119623846));
#60710=CARTESIAN_POINT('Ctrl Pts',(-1.35049736560527,1.,3.49861894124827));
#60711=CARTESIAN_POINT('Ctrl Pts',(-1.35080045218587,1.,3.49920025459723));
#60712=CARTESIAN_POINT('Ctrl Pts',(-1.35142377279517,1.,3.5007660381649));
#60713=CARTESIAN_POINT('Ctrl Pts',(-1.35257032843486,1.,3.50408168106261));
#60714=CARTESIAN_POINT('Ctrl Pts',(-1.35419113575956,1.,3.50913227059999));
#60715=CARTESIAN_POINT('Ctrl Pts',(-1.35611275237152,1.,3.51542230699556));
#60716=CARTESIAN_POINT('Ctrl Pts',(-1.35821701528836,1.,3.52261776116748));
#60717=CARTESIAN_POINT('Ctrl Pts',(-1.36037259643734,1.,3.530344649616));
#60718=CARTESIAN_POINT('Ctrl Pts',(-1.36245507339307,1.,3.53824396424961));
#60719=CARTESIAN_POINT('Ctrl Pts',(-1.36436666257598,1.,3.54602591832973));
#60720=CARTESIAN_POINT('Ctrl Pts',(-1.3660614545677,1.,3.55353883995949));
#60721=CARTESIAN_POINT('Ctrl Pts',(-1.36754771771233,1.,3.56077662028649));
#60722=CARTESIAN_POINT('Ctrl Pts',(-1.36886584973389,1.,3.5678208030466));
#60723=CARTESIAN_POINT('Ctrl Pts',(-1.37007229485659,1.,3.57479875549486));
#60724=CARTESIAN_POINT('Ctrl Pts',(-1.37122241663062,1.,3.58183885982715));
#60725=CARTESIAN_POINT('Ctrl Pts',(-1.37235053660976,1.,3.58901853846365));
#60726=CARTESIAN_POINT('Ctrl Pts',(-1.37346320103157,1.,3.59634627869048));
#60727=CARTESIAN_POINT('Ctrl Pts',(-1.37455051379623,1.,3.60379020123988));
#60728=CARTESIAN_POINT('Ctrl Pts',(-1.37559314436634,1.,3.61129546591064));
#60729=CARTESIAN_POINT('Ctrl Pts',(-1.37657053403107,1.,3.6188048116042));
#60730=CARTESIAN_POINT('Ctrl Pts',(-1.37746987919881,1.,3.62628098665145));
#60731=CARTESIAN_POINT('Ctrl Pts',(-1.37829035457339,1.,3.63371727442486));
#60732=CARTESIAN_POINT('Ctrl Pts',(-1.37903818567359,1.,3.64112507791141));
#60733=CARTESIAN_POINT('Ctrl Pts',(-1.37972372481603,1.,3.64852652756456));
#60734=CARTESIAN_POINT('Ctrl Pts',(-1.38035791051213,1.,3.6559455440439));
#60735=CARTESIAN_POINT('Ctrl Pts',(-1.38094856333552,1.,3.66339848520857));
#60736=CARTESIAN_POINT('Ctrl Pts',(-1.38149812653868,1.,3.67088843112262));
#60737=CARTESIAN_POINT('Ctrl Pts',(-1.3820057429062,1.,3.67841038482414));
#60738=CARTESIAN_POINT('Ctrl Pts',(-1.38246852827182,1.,3.68595444983837));
#60739=CARTESIAN_POINT('Ctrl Pts',(-1.38288311171651,1.,3.69350967899526));
#60740=CARTESIAN_POINT('Ctrl Pts',(-1.38324717612865,1.,3.701067921679));
#60741=CARTESIAN_POINT('Ctrl Pts',(-1.38356065402124,1.,3.70862680753347));
#60742=CARTESIAN_POINT('Ctrl Pts',(-1.38382489984586,1.,3.7161876605181));
#60743=CARTESIAN_POINT('Ctrl Pts',(-1.3840421342895,1.,3.72375409358803));
#60744=CARTESIAN_POINT('Ctrl Pts',(-1.38421479111531,1.,3.73133035859282));
#60745=CARTESIAN_POINT('Ctrl Pts',(-1.38434489156458,1.,3.73891976418104));
#60746=CARTESIAN_POINT('Ctrl Pts',(-1.38443344984394,1.,3.74652317167876));
#60747=CARTESIAN_POINT('Ctrl Pts',(-1.38448077997163,1.,3.7541397631875));
#60748=CARTESIAN_POINT('Ctrl Pts',(-1.3844867525335,1.,3.76176768271367));
#60749=CARTESIAN_POINT('Ctrl Pts',(-1.38445107339518,1.,3.76940473185779));
#60750=CARTESIAN_POINT('Ctrl Pts',(-1.38437354551428,1.,3.77704902230418));
#60751=CARTESIAN_POINT('Ctrl Pts',(-1.38425435883756,1.,3.78469969805082));
#60752=CARTESIAN_POINT('Ctrl Pts',(-1.38409399694566,1.,3.79235669640841));
#60753=CARTESIAN_POINT('Ctrl Pts',(-1.38389311766682,1.,3.80002044322111));
#60754=CARTESIAN_POINT('Ctrl Pts',(-1.3836524404622,1.,3.80769156398411));
#60755=CARTESIAN_POINT('Ctrl Pts',(-1.38337263902782,1.,3.81537060817811));
#60756=CARTESIAN_POINT('Ctrl Pts',(-1.38305421262763,1.,3.82305771743829));
#60757=CARTESIAN_POINT('Ctrl Pts',(-1.38269750245138,1.,3.8307526698229));
#60758=CARTESIAN_POINT('Ctrl Pts',(-1.38230274828822,1.,3.83845502790746));
#60759=CARTESIAN_POINT('Ctrl Pts',(-1.38187013346109,1.,3.84616425605764));
#60760=CARTESIAN_POINT('Ctrl Pts',(-1.38139983115049,1.,3.85387983979481));
#60761=CARTESIAN_POINT('Ctrl Pts',(-1.38089205992989,1.,3.86160143043959));
#60762=CARTESIAN_POINT('Ctrl Pts',(-1.38034709213014,1.,3.86932885813068));
#60763=CARTESIAN_POINT('Ctrl Pts',(-1.37976523097073,1.,3.87706205830532));
#60764=CARTESIAN_POINT('Ctrl Pts',(-1.37914679719383,1.,3.88480102249277));
#60765=CARTESIAN_POINT('Ctrl Pts',(-1.3784921128802,1.,3.89254574338496));
#60766=CARTESIAN_POINT('Ctrl Pts',(-1.37780148512792,1.,3.90029615196727));
#60767=CARTESIAN_POINT('Ctrl Pts',(-1.3770751963402,1.,3.90805209523486));
#60768=CARTESIAN_POINT('Ctrl Pts',(-1.37631350505797,1.,3.91581337462644));
#60769=CARTESIAN_POINT('Ctrl Pts',(-1.37551664448242,1.,3.92357976987672));
#60770=CARTESIAN_POINT('Ctrl Pts',(-1.37468482215751,1.,3.93135106761844));
#60771=CARTESIAN_POINT('Ctrl Pts',(-1.37381821967165,1.,3.93912709040818));
#60772=CARTESIAN_POINT('Ctrl Pts',(-1.37291699202807,1.,3.94690771785133));
#60773=CARTESIAN_POINT('Ctrl Pts',(-1.37198126432386,1.,3.95469287280914));
#60774=CARTESIAN_POINT('Ctrl Pts',(-1.3712051561502,1.,3.96092458506535));
#60775=CARTESIAN_POINT('Ctrl Pts',(-1.37060761745635,1.,3.96560037974645));
#60776=CARTESIAN_POINT('Ctrl Pts',(-1.37020239094614,1.,3.9687184694131));
#60777=CARTESIAN_POINT('Ctrl Pts',(-1.36999806084572,1.,3.97027773754922));
#60778=CARTESIAN_POINT('Origin',(-1.36999806084572,0.,3.97027773754922));
#60779=CARTESIAN_POINT('',(-1.22531898815164,1.,4.01728681790024));
#60780=CARTESIAN_POINT('Origin',(0.,0.,0.));
#60781=CARTESIAN_POINT('',(-1.51895082866166,1.,3.42859860294378));
#60782=CARTESIAN_POINT('Origin',(0.,1.,0.));
#60783=CARTESIAN_POINT('Ctrl Pts',(-1.51895082866166,1.,3.42859860294378));
#60784=CARTESIAN_POINT('Ctrl Pts',(-1.51895082866166,0.666666666666667,
3.42859860294378));
#60785=CARTESIAN_POINT('Ctrl Pts',(-1.51895082866166,0.333333333333333,
3.42859860294378));
#60786=CARTESIAN_POINT('Ctrl Pts',(-1.51895082866166,-0.333333333333333,
3.42859860294378));
#60787=CARTESIAN_POINT('Ctrl Pts',(-1.51895082866166,-0.666666666666667,
3.42859860294378));
#60788=CARTESIAN_POINT('Ctrl Pts',(-1.51895082866166,-1.,3.42859860294378));
#60789=CARTESIAN_POINT('Ctrl Pts',(-1.83867539237861,-1.,3.77614523045147));
#60790=CARTESIAN_POINT('Ctrl Pts',(-1.83867539237861,1.,3.77614523045147));
#60791=CARTESIAN_POINT('Ctrl Pts',(-1.83742834010821,-1.,3.77518714458232));
#60792=CARTESIAN_POINT('Ctrl Pts',(-1.83742834010821,1.,3.77518714458232));
#60793=CARTESIAN_POINT('Ctrl Pts',(-1.83493697935064,-1.,3.77326886065484));
#60794=CARTESIAN_POINT('Ctrl Pts',(-1.83493697935064,1.,3.77326886065484));
#60795=CARTESIAN_POINT('Ctrl Pts',(-1.83120816956515,-1.,3.77038509819777));
#60796=CARTESIAN_POINT('Ctrl Pts',(-1.83120816956515,1.,3.77038509819777));
#60797=CARTESIAN_POINT('Ctrl Pts',(-1.82625289221933,-1.,3.76652740355856));
#60798=CARTESIAN_POINT('Ctrl Pts',(-1.82625289221933,1.,3.76652740355856));
#60799=CARTESIAN_POINT('Ctrl Pts',(-1.82008629694924,-1.,3.76168412709652));
#60800=CARTESIAN_POINT('Ctrl Pts',(-1.82008629694924,1.,3.76168412709652));
#60801=CARTESIAN_POINT('Ctrl Pts',(-1.81394729834032,-1.,3.75681965683995));
#60802=CARTESIAN_POINT('Ctrl Pts',(-1.81394729834032,1.,3.75681965683995));
#60803=CARTESIAN_POINT('Ctrl Pts',(-1.80783603939662,-1.,3.75193395888069));
#60804=CARTESIAN_POINT('Ctrl Pts',(-1.80783603939662,1.,3.75193395888069));
#60805=CARTESIAN_POINT('Ctrl Pts',(-1.80175271485519,-1.,3.74702700874954));
#60806=CARTESIAN_POINT('Ctrl Pts',(-1.80175271485519,1.,3.74702700874954));
#60807=CARTESIAN_POINT('Ctrl Pts',(-1.79569757859041,-1.,3.74209880351667));
#60808=CARTESIAN_POINT('Ctrl Pts',(-1.79569757859041,1.,3.74209880351667));
#60809=CARTESIAN_POINT('Ctrl Pts',(-1.78967092823139,-1.,3.73714934729962));
#60810=CARTESIAN_POINT('Ctrl Pts',(-1.78967092823139,1.,3.73714934729962));
#60811=CARTESIAN_POINT('Ctrl Pts',(-1.78367308442682,-1.,3.73217863095022));
#60812=CARTESIAN_POINT('Ctrl Pts',(-1.78367308442682,1.,3.73217863095022));
#60813=CARTESIAN_POINT('Ctrl Pts',(-1.77770437039606,-1.,3.72718661205504));
#60814=CARTESIAN_POINT('Ctrl Pts',(-1.77770437039606,1.,3.72718661205504));
#60815=CARTESIAN_POINT('Ctrl Pts',(-1.77176509401846,-1.,3.72217319911429));
#60816=CARTESIAN_POINT('Ctrl Pts',(-1.77176509401846,1.,3.72217319911429));
#60817=CARTESIAN_POINT('Ctrl Pts',(-1.76585552124549,-1.,3.71713822377675));
#60818=CARTESIAN_POINT('Ctrl Pts',(-1.76585552124549,1.,3.71713822377675));
#60819=CARTESIAN_POINT('Ctrl Pts',(-1.75997588499021,-1.,3.71208146346454));
#60820=CARTESIAN_POINT('Ctrl Pts',(-1.75997588499021,1.,3.71208146346454));
#60821=CARTESIAN_POINT('Ctrl Pts',(-1.75412641804148,-1.,3.70700269736876));
#60822=CARTESIAN_POINT('Ctrl Pts',(-1.75412641804148,1.,3.70700269736876));
#60823=CARTESIAN_POINT('Ctrl Pts',(-1.74830738046092,-1.,3.70190175673422));
#60824=CARTESIAN_POINT('Ctrl Pts',(-1.74830738046092,1.,3.70190175673422));
#60825=CARTESIAN_POINT('Ctrl Pts',(-1.74251908492589,-1.,3.6967785691046));
#60826=CARTESIAN_POINT('Ctrl Pts',(-1.74251908492589,1.,3.6967785691046));
#60827=CARTESIAN_POINT('Ctrl Pts',(-1.73676193254493,-1.,3.69163322647906));
#60828=CARTESIAN_POINT('Ctrl Pts',(-1.73676193254493,1.,3.69163322647906));
#60829=CARTESIAN_POINT('Ctrl Pts',(-1.73103640956647,-1.,3.68646597019188));
#60830=CARTESIAN_POINT('Ctrl Pts',(-1.73103640956647,1.,3.68646597019188));
#60831=CARTESIAN_POINT('Ctrl Pts',(-1.72534302437003,-1.,3.68127704936472));
#60832=CARTESIAN_POINT('Ctrl Pts',(-1.72534302437003,1.,3.68127704936472));
#60833=CARTESIAN_POINT('Ctrl Pts',(-1.71968225581787,-1.,3.67606660374665));
#60834=CARTESIAN_POINT('Ctrl Pts',(-1.71968225581787,1.,3.67606660374665));
#60835=CARTESIAN_POINT('Ctrl Pts',(-1.71405450210392,-1.,3.67083454901629));
#60836=CARTESIAN_POINT('Ctrl Pts',(-1.71405450210392,1.,3.67083454901629));
#60837=CARTESIAN_POINT('Ctrl Pts',(-1.70846001610983,-1.,3.6655804319893));
#60838=CARTESIAN_POINT('Ctrl Pts',(-1.70846001610983,1.,3.6655804319893));
#60839=CARTESIAN_POINT('Ctrl Pts',(-1.70289888566904,-1.,3.6603033877491));
#60840=CARTESIAN_POINT('Ctrl Pts',(-1.70289888566904,1.,3.6603033877491));
#60841=CARTESIAN_POINT('Ctrl Pts',(-1.69737117722559,-1.,3.65500246526798));
#60842=CARTESIAN_POINT('Ctrl Pts',(-1.69737117722559,1.,3.65500246526798));
#60843=CARTESIAN_POINT('Ctrl Pts',(-1.691877054817,-1.,3.64967689827393));
#60844=CARTESIAN_POINT('Ctrl Pts',(-1.691877054817,1.,3.64967689827393));
#60845=CARTESIAN_POINT('Ctrl Pts',(-1.68641690471455,-1.,3.64432638915199));
#60846=CARTESIAN_POINT('Ctrl Pts',(-1.68641690471455,1.,3.64432638915199));
#60847=CARTESIAN_POINT('Ctrl Pts',(-1.68099146651577,-1.,3.63895140887443));
#60848=CARTESIAN_POINT('Ctrl Pts',(-1.68099146651577,1.,3.63895140887443));
#60849=CARTESIAN_POINT('Ctrl Pts',(-1.67560193613145,-1.,3.63355343201211));
#60850=CARTESIAN_POINT('Ctrl Pts',(-1.67560193613145,1.,3.63355343201211));
#60851=CARTESIAN_POINT('Ctrl Pts',(-1.67024966008037,-1.,3.62813422105257));
#60852=CARTESIAN_POINT('Ctrl Pts',(-1.67024966008037,1.,3.62813422105257));
#60853=CARTESIAN_POINT('Ctrl Pts',(-1.66493585923853,-1.,3.62269517989104));
#60854=CARTESIAN_POINT('Ctrl Pts',(-1.66493585923853,1.,3.62269517989104));
#60855=CARTESIAN_POINT('Ctrl Pts',(-1.65966133399186,-1.,3.61723666482457));
#60856=CARTESIAN_POINT('Ctrl Pts',(-1.65966133399186,1.,3.61723666482457));
#60857=CARTESIAN_POINT('Ctrl Pts',(-1.65442619244327,-1.,3.61175734965129));
#60858=CARTESIAN_POINT('Ctrl Pts',(-1.65442619244327,1.,3.61175734965129));
#60859=CARTESIAN_POINT('Ctrl Pts',(-1.64922952425833,-1.,3.60625346556992));
#60860=CARTESIAN_POINT('Ctrl Pts',(-1.64922952425833,1.,3.60625346556992));
#60861=CARTESIAN_POINT('Ctrl Pts',(-1.6440700438558,-1.,3.6007202851384));
#60862=CARTESIAN_POINT('Ctrl Pts',(-1.6440700438558,1.,3.6007202851384));
#60863=CARTESIAN_POINT('Ctrl Pts',(-1.63894676675349,-1.,3.59515368334887));
#60864=CARTESIAN_POINT('Ctrl Pts',(-1.63894676675349,1.,3.59515368334887));
#60865=CARTESIAN_POINT('Ctrl Pts',(-1.63385971451259,-1.,3.58955176627876));
#60866=CARTESIAN_POINT('Ctrl Pts',(-1.63385971451259,1.,3.58955176627876));
#60867=CARTESIAN_POINT('Ctrl Pts',(-1.62881051550748,-1.,3.5839162577435));
#60868=CARTESIAN_POINT('Ctrl Pts',(-1.62881051550748,1.,3.5839162577435));
#60869=CARTESIAN_POINT('Ctrl Pts',(-1.62380329464851,-1.,3.57825455954405));
#60870=CARTESIAN_POINT('Ctrl Pts',(-1.62380329464851,1.,3.57825455954405));
#60871=CARTESIAN_POINT('Ctrl Pts',(-1.61884340915412,-1.,3.57257679609826));
#60872=CARTESIAN_POINT('Ctrl Pts',(-1.61884340915412,1.,3.57257679609826));
#60873=CARTESIAN_POINT('Ctrl Pts',(-1.61393581747522,-1.,3.56689200468404));
#60874=CARTESIAN_POINT('Ctrl Pts',(-1.61393581747522,1.,3.56689200468404));
#60875=CARTESIAN_POINT('Ctrl Pts',(-1.60908344685459,-1.,3.56120432482986));
#60876=CARTESIAN_POINT('Ctrl Pts',(-1.60908344685459,1.,3.56120432482986));
#60877=CARTESIAN_POINT('Ctrl Pts',(-1.60428584699848,-1.,3.55550985096117));
#60878=CARTESIAN_POINT('Ctrl Pts',(-1.60428584699848,1.,3.55550985096117));
#60879=CARTESIAN_POINT('Ctrl Pts',(-1.59953698113444,-1.,3.54979148634426));
#60880=CARTESIAN_POINT('Ctrl Pts',(-1.59953698113444,1.,3.54979148634426));
#60881=CARTESIAN_POINT('Ctrl Pts',(-1.5948276694975,-1.,3.544024581823));
#60882=CARTESIAN_POINT('Ctrl Pts',(-1.5948276694975,1.,3.544024581823));
#60883=CARTESIAN_POINT('Ctrl Pts',(-1.59014958368725,-1.,3.53818616861045));
#60884=CARTESIAN_POINT('Ctrl Pts',(-1.59014958368725,1.,3.53818616861045));
#60885=CARTESIAN_POINT('Ctrl Pts',(-1.58549906268083,-1.,3.53226378147068));
#60886=CARTESIAN_POINT('Ctrl Pts',(-1.58549906268083,1.,3.53226378147068));
#60887=CARTESIAN_POINT('Ctrl Pts',(-1.58088027227856,-1.,3.52626275334899));
#60888=CARTESIAN_POINT('Ctrl Pts',(-1.58088027227856,1.,3.52626275334899));
#60889=CARTESIAN_POINT('Ctrl Pts',(-1.5763104998818,-1.,3.52021847865961));
#60890=CARTESIAN_POINT('Ctrl Pts',(-1.5763104998818,1.,3.52021847865961));
#60891=CARTESIAN_POINT('Ctrl Pts',(-1.57181569799774,-1.,3.51418598431733));
#60892=CARTESIAN_POINT('Ctrl Pts',(-1.57181569799774,1.,3.51418598431733));
#60893=CARTESIAN_POINT('Ctrl Pts',(-1.56742097575041,-1.,3.50821771695427));
#60894=CARTESIAN_POINT('Ctrl Pts',(-1.56742097575041,1.,3.50821771695427));
#60895=CARTESIAN_POINT('Ctrl Pts',(-1.56314187758689,-1.,3.50234321621607));
#60896=CARTESIAN_POINT('Ctrl Pts',(-1.56314187758689,1.,3.50234321621607));
#60897=CARTESIAN_POINT('Ctrl Pts',(-1.55897703097859,-1.,3.49655185179623));
#60898=CARTESIAN_POINT('Ctrl Pts',(-1.55897703097859,1.,3.49655185179623));
#60899=CARTESIAN_POINT('Ctrl Pts',(-1.5548959590107,-1.,3.49076460877317));
#60900=CARTESIAN_POINT('Ctrl Pts',(-1.5548959590107,1.,3.49076460877317));
#60901=CARTESIAN_POINT('Ctrl Pts',(-1.55084702970382,-1.,3.48485155928414));
#60902=CARTESIAN_POINT('Ctrl Pts',(-1.55084702970382,1.,3.48485155928414));
#60903=CARTESIAN_POINT('Ctrl Pts',(-1.54678009290207,-1.,3.47868272898599));
#60904=CARTESIAN_POINT('Ctrl Pts',(-1.54678009290207,1.,3.47868272898599));
#60905=CARTESIAN_POINT('Ctrl Pts',(-1.54266605398152,-1.,3.47217189224576));
#60906=CARTESIAN_POINT('Ctrl Pts',(-1.54266605398152,1.,3.47217189224576));
#60907=CARTESIAN_POINT('Ctrl Pts',(-1.53851507915533,-1.,3.46531752207222));
#60908=CARTESIAN_POINT('Ctrl Pts',(-1.53851507915533,1.,3.46531752207222));
#60909=CARTESIAN_POINT('Ctrl Pts',(-1.53440195378902,-1.,3.45825932955273));
#60910=CARTESIAN_POINT('Ctrl Pts',(-1.53440195378902,1.,3.45825932955273));
#60911=CARTESIAN_POINT('Ctrl Pts',(-1.530462444618,-1.,3.45127136828667));
#60912=CARTESIAN_POINT('Ctrl Pts',(-1.530462444618,1.,3.45127136828667));
#60913=CARTESIAN_POINT('Ctrl Pts',(-1.52686242875717,-1.,3.44469547527));
#60914=CARTESIAN_POINT('Ctrl Pts',(-1.52686242875717,1.,3.44469547527));
#60915=CARTESIAN_POINT('Ctrl Pts',(-1.52377348950429,-1.,3.43888895974182));
#60916=CARTESIAN_POINT('Ctrl Pts',(-1.52377348950429,1.,3.43888895974182));
#60917=CARTESIAN_POINT('Ctrl Pts',(-1.52134826724227,-1.,3.43417156977749));
#60918=CARTESIAN_POINT('Ctrl Pts',(-1.52134826724227,1.,3.43417156977749));
#60919=CARTESIAN_POINT('Ctrl Pts',(-1.51969006980792,-1.,3.43076036253384));
#60920=CARTESIAN_POINT('Ctrl Pts',(-1.51969006980792,1.,3.43076036253384));
#60921=CARTESIAN_POINT('Ctrl Pts',(-1.51901585838879,-1.,3.42915787669388));
#60922=CARTESIAN_POINT('Ctrl Pts',(-1.51901585838879,1.,3.42915787669388));
#60923=CARTESIAN_POINT('Ctrl Pts',(-1.51888450659497,-1.,3.42860527148835));
#60924=CARTESIAN_POINT('Ctrl Pts',(-1.51888450659497,1.,3.42860527148835));
#60925=CARTESIAN_POINT('Ctrl Pts',(-1.51896318668306,-1.,3.42852521763648));
#60926=CARTESIAN_POINT('Ctrl Pts',(-1.51896318668306,1.,3.42852521763648));
#60927=CARTESIAN_POINT('Ctrl Pts',(-1.519044091397,-1.,3.42855728381368));
#60928=CARTESIAN_POINT('Ctrl Pts',(-1.519044091397,1.,3.42855728381368));
#60929=CARTESIAN_POINT('',(-1.83867539237861,1.,3.77614523045147));
#60930=CARTESIAN_POINT('Ctrl Pts',(-1.83867539237861,1.,3.77614523045147));
#60931=CARTESIAN_POINT('Ctrl Pts',(-1.83742834010821,1.,3.77518714458232));
#60932=CARTESIAN_POINT('Ctrl Pts',(-1.83493697935064,1.,3.77326886065484));
#60933=CARTESIAN_POINT('Ctrl Pts',(-1.83120816956515,1.,3.77038509819777));
#60934=CARTESIAN_POINT('Ctrl Pts',(-1.82625289221933,1.,3.76652740355856));
#60935=CARTESIAN_POINT('Ctrl Pts',(-1.82008629694924,1.,3.76168412709652));
#60936=CARTESIAN_POINT('Ctrl Pts',(-1.81394729834032,1.,3.75681965683995));
#60937=CARTESIAN_POINT('Ctrl Pts',(-1.80783603939662,1.,3.75193395888069));
#60938=CARTESIAN_POINT('Ctrl Pts',(-1.80175271485519,1.,3.74702700874954));
#60939=CARTESIAN_POINT('Ctrl Pts',(-1.79569757859041,1.,3.74209880351667));
#60940=CARTESIAN_POINT('Ctrl Pts',(-1.78967092823139,1.,3.73714934729962));
#60941=CARTESIAN_POINT('Ctrl Pts',(-1.78367308442682,1.,3.73217863095022));
#60942=CARTESIAN_POINT('Ctrl Pts',(-1.77770437039606,1.,3.72718661205504));
#60943=CARTESIAN_POINT('Ctrl Pts',(-1.77176509401846,1.,3.72217319911429));
#60944=CARTESIAN_POINT('Ctrl Pts',(-1.76585552124549,1.,3.71713822377675));
#60945=CARTESIAN_POINT('Ctrl Pts',(-1.75997588499021,1.,3.71208146346454));
#60946=CARTESIAN_POINT('Ctrl Pts',(-1.75412641804148,1.,3.70700269736876));
#60947=CARTESIAN_POINT('Ctrl Pts',(-1.74830738046092,1.,3.70190175673422));
#60948=CARTESIAN_POINT('Ctrl Pts',(-1.74251908492589,1.,3.6967785691046));
#60949=CARTESIAN_POINT('Ctrl Pts',(-1.73676193254493,1.,3.69163322647906));
#60950=CARTESIAN_POINT('Ctrl Pts',(-1.73103640956647,1.,3.68646597019188));
#60951=CARTESIAN_POINT('Ctrl Pts',(-1.72534302437003,1.,3.68127704936472));
#60952=CARTESIAN_POINT('Ctrl Pts',(-1.71968225581787,1.,3.67606660374665));
#60953=CARTESIAN_POINT('Ctrl Pts',(-1.71405450210392,1.,3.67083454901629));
#60954=CARTESIAN_POINT('Ctrl Pts',(-1.70846001610983,1.,3.6655804319893));
#60955=CARTESIAN_POINT('Ctrl Pts',(-1.70289888566904,1.,3.6603033877491));
#60956=CARTESIAN_POINT('Ctrl Pts',(-1.69737117722559,1.,3.65500246526798));
#60957=CARTESIAN_POINT('Ctrl Pts',(-1.691877054817,1.,3.64967689827393));
#60958=CARTESIAN_POINT('Ctrl Pts',(-1.68641690471455,1.,3.64432638915199));
#60959=CARTESIAN_POINT('Ctrl Pts',(-1.68099146651577,1.,3.63895140887443));
#60960=CARTESIAN_POINT('Ctrl Pts',(-1.67560193613145,1.,3.63355343201211));
#60961=CARTESIAN_POINT('Ctrl Pts',(-1.67024966008037,1.,3.62813422105257));
#60962=CARTESIAN_POINT('Ctrl Pts',(-1.66493585923853,1.,3.62269517989104));
#60963=CARTESIAN_POINT('Ctrl Pts',(-1.65966133399186,1.,3.61723666482457));
#60964=CARTESIAN_POINT('Ctrl Pts',(-1.65442619244327,1.,3.61175734965129));
#60965=CARTESIAN_POINT('Ctrl Pts',(-1.64922952425833,1.,3.60625346556992));
#60966=CARTESIAN_POINT('Ctrl Pts',(-1.6440700438558,1.,3.6007202851384));
#60967=CARTESIAN_POINT('Ctrl Pts',(-1.63894676675349,1.,3.59515368334887));
#60968=CARTESIAN_POINT('Ctrl Pts',(-1.63385971451259,1.,3.58955176627876));
#60969=CARTESIAN_POINT('Ctrl Pts',(-1.62881051550748,1.,3.5839162577435));
#60970=CARTESIAN_POINT('Ctrl Pts',(-1.62380329464851,1.,3.57825455954405));
#60971=CARTESIAN_POINT('Ctrl Pts',(-1.61884340915412,1.,3.57257679609826));
#60972=CARTESIAN_POINT('Ctrl Pts',(-1.61393581747522,1.,3.56689200468404));
#60973=CARTESIAN_POINT('Ctrl Pts',(-1.60908344685459,1.,3.56120432482986));
#60974=CARTESIAN_POINT('Ctrl Pts',(-1.60428584699848,1.,3.55550985096117));
#60975=CARTESIAN_POINT('Ctrl Pts',(-1.59953698113444,1.,3.54979148634426));
#60976=CARTESIAN_POINT('Ctrl Pts',(-1.5948276694975,1.,3.544024581823));
#60977=CARTESIAN_POINT('Ctrl Pts',(-1.59014958368725,1.,3.53818616861045));
#60978=CARTESIAN_POINT('Ctrl Pts',(-1.58549906268083,1.,3.53226378147068));
#60979=CARTESIAN_POINT('Ctrl Pts',(-1.58088027227856,1.,3.52626275334899));
#60980=CARTESIAN_POINT('Ctrl Pts',(-1.5763104998818,1.,3.52021847865961));
#60981=CARTESIAN_POINT('Ctrl Pts',(-1.57181569799774,1.,3.51418598431733));
#60982=CARTESIAN_POINT('Ctrl Pts',(-1.56742097575041,1.,3.50821771695427));
#60983=CARTESIAN_POINT('Ctrl Pts',(-1.56314187758689,1.,3.50234321621607));
#60984=CARTESIAN_POINT('Ctrl Pts',(-1.55897703097859,1.,3.49655185179623));
#60985=CARTESIAN_POINT('Ctrl Pts',(-1.5548959590107,1.,3.49076460877317));
#60986=CARTESIAN_POINT('Ctrl Pts',(-1.55084702970382,1.,3.48485155928414));
#60987=CARTESIAN_POINT('Ctrl Pts',(-1.54678009290207,1.,3.47868272898599));
#60988=CARTESIAN_POINT('Ctrl Pts',(-1.54266605398152,1.,3.47217189224576));
#60989=CARTESIAN_POINT('Ctrl Pts',(-1.53851507915533,1.,3.46531752207222));
#60990=CARTESIAN_POINT('Ctrl Pts',(-1.53440195378902,1.,3.45825932955273));
#60991=CARTESIAN_POINT('Ctrl Pts',(-1.530462444618,1.,3.45127136828667));
#60992=CARTESIAN_POINT('Ctrl Pts',(-1.52686242875717,1.,3.44469547527));
#60993=CARTESIAN_POINT('Ctrl Pts',(-1.52377348950429,1.,3.43888895974182));
#60994=CARTESIAN_POINT('Ctrl Pts',(-1.52134826724227,1.,3.43417156977749));
#60995=CARTESIAN_POINT('Ctrl Pts',(-1.5198144909343,1.,3.4310163189349));
#60996=CARTESIAN_POINT('Ctrl Pts',(-1.51914806898539,1.,3.42946838852728));
#60997=CARTESIAN_POINT('Ctrl Pts',(-1.51895133295017,1.,3.42884302333978));
#60998=CARTESIAN_POINT('Ctrl Pts',(-1.51893924967231,1.,3.42864616361967));
#60999=CARTESIAN_POINT('Ctrl Pts',(-1.51895082866166,1.,3.42859860294378));
#61000=CARTESIAN_POINT('',(-1.83867539237861,0.,3.77614523045147));
#61001=CARTESIAN_POINT('Ctrl Pts',(-1.88088939428811,-1.,3.24418789321065));
#61002=CARTESIAN_POINT('Ctrl Pts',(-1.88088939428811,1.,3.24418789321065));
#61003=CARTESIAN_POINT('Ctrl Pts',(-1.8809110068042,-1.,3.24410359189733));
#61004=CARTESIAN_POINT('Ctrl Pts',(-1.8809110068042,1.,3.24410359189733));
#61005=CARTESIAN_POINT('Ctrl Pts',(-1.8810220187274,-1.,3.24408699284449));
#61006=CARTESIAN_POINT('Ctrl Pts',(-1.8810220187274,1.,3.24408699284449));
#61007=CARTESIAN_POINT('Ctrl Pts',(-1.88139187908347,-1.,3.24451807186964));
#61008=CARTESIAN_POINT('Ctrl Pts',(-1.88139187908347,1.,3.24451807186964));
#61009=CARTESIAN_POINT('Ctrl Pts',(-1.88229202583187,-1.,3.24600543790876));
#61010=CARTESIAN_POINT('Ctrl Pts',(-1.88229202583187,1.,3.24600543790876));
#61011=CARTESIAN_POINT('Ctrl Pts',(-1.88407708646435,-1.,3.24935200512055));
#61012=CARTESIAN_POINT('Ctrl Pts',(-1.88407708646435,1.,3.24935200512055));
#61013=CARTESIAN_POINT('Ctrl Pts',(-1.88646802523372,-1.,3.25408686339298));
#61014=CARTESIAN_POINT('Ctrl Pts',(-1.88646802523372,1.,3.25408686339298));
#61015=CARTESIAN_POINT('Ctrl Pts',(-1.88934996203508,-1.,3.2599988519361));
#61016=CARTESIAN_POINT('Ctrl Pts',(-1.88934996203508,1.,3.2599988519361));
#61017=CARTESIAN_POINT('Ctrl Pts',(-1.89255393500769,-1.,3.2667765388833));
#61018=CARTESIAN_POINT('Ctrl Pts',(-1.89255393500769,1.,3.2667765388833));
#61019=CARTESIAN_POINT('Ctrl Pts',(-1.89589172903662,-1.,3.27407108932908));
#61020=CARTESIAN_POINT('Ctrl Pts',(-1.89589172903662,1.,3.27407108932908));
#61021=CARTESIAN_POINT('Ctrl Pts',(-1.89918429230425,-1.,3.28154737912287));
#61022=CARTESIAN_POINT('Ctrl Pts',(-1.89918429230425,1.,3.28154737912287));
#61023=CARTESIAN_POINT('Ctrl Pts',(-1.9022897124757,-1.,3.28893448600364));
#61024=CARTESIAN_POINT('Ctrl Pts',(-1.9022897124757,1.,3.28893448600364));
#61025=CARTESIAN_POINT('Ctrl Pts',(-1.9051389186417,-1.,3.29608978722258));
#61026=CARTESIAN_POINT('Ctrl Pts',(-1.9051389186417,1.,3.29608978722258));
#61027=CARTESIAN_POINT('Ctrl Pts',(-1.90773912171424,-1.,3.30300595568341));
#61028=CARTESIAN_POINT('Ctrl Pts',(-1.90773912171424,1.,3.30300595568341));
#61029=CARTESIAN_POINT('Ctrl Pts',(-1.91014297830502,-1.,3.30975721158694));
#61030=CARTESIAN_POINT('Ctrl Pts',(-1.91014297830502,1.,3.30975721158694));
#61031=CARTESIAN_POINT('Ctrl Pts',(-1.91242616234459,-1.,3.31646052426395));
#61032=CARTESIAN_POINT('Ctrl Pts',(-1.91242616234459,1.,3.31646052426395));
#61033=CARTESIAN_POINT('Ctrl Pts',(-1.91466343916612,-1.,3.32323403454507));
#61034=CARTESIAN_POINT('Ctrl Pts',(-1.91466343916612,1.,3.32323403454507));
#61035=CARTESIAN_POINT('Ctrl Pts',(-1.91690081930297,-1.,3.33014884257812));
#61036=CARTESIAN_POINT('Ctrl Pts',(-1.91690081930297,1.,3.33014884257812));
#61037=CARTESIAN_POINT('Ctrl Pts',(-1.91914609610173,-1.,3.33721230709948));
#61038=CARTESIAN_POINT('Ctrl Pts',(-1.91914609610173,1.,3.33721230709948));
#61039=CARTESIAN_POINT('Ctrl Pts',(-1.92138450828378,-1.,3.34439448941915));
#61040=CARTESIAN_POINT('Ctrl Pts',(-1.92138450828378,1.,3.34439448941915));
#61041=CARTESIAN_POINT('Ctrl Pts',(-1.92358838440518,-1.,3.35164424847206));
#61042=CARTESIAN_POINT('Ctrl Pts',(-1.92358838440518,1.,3.35164424847206));
#61043=CARTESIAN_POINT('Ctrl Pts',(-1.92572846125763,-1.,3.35890824422976));
#61044=CARTESIAN_POINT('Ctrl Pts',(-1.92572846125763,1.,3.35890824422976));
#61045=CARTESIAN_POINT('Ctrl Pts',(-1.92778626543803,-1.,3.36615168657597));
#61046=CARTESIAN_POINT('Ctrl Pts',(-1.92778626543803,1.,3.36615168657597));
#61047=CARTESIAN_POINT('Ctrl Pts',(-1.92975993109897,-1.,3.37336807068078));
#61048=CARTESIAN_POINT('Ctrl Pts',(-1.92975993109897,1.,3.37336807068078));
#61049=CARTESIAN_POINT('Ctrl Pts',(-1.93165739093292,-1.,3.38056768525577));
#61050=CARTESIAN_POINT('Ctrl Pts',(-1.93165739093292,1.,3.38056768525577));
#61051=CARTESIAN_POINT('Ctrl Pts',(-1.93349233176794,-1.,3.38777076883267));
#61052=CARTESIAN_POINT('Ctrl Pts',(-1.93349233176794,1.,3.38777076883267));
#61053=CARTESIAN_POINT('Ctrl Pts',(-1.93527929945982,-1.,3.39499923640789));
#61054=CARTESIAN_POINT('Ctrl Pts',(-1.93527929945982,1.,3.39499923640789));
#61055=CARTESIAN_POINT('Ctrl Pts',(-1.93702857723089,-1.,3.40226802104093));
#61056=CARTESIAN_POINT('Ctrl Pts',(-1.93702857723089,1.,3.40226802104093));
#61057=CARTESIAN_POINT('Ctrl Pts',(-1.93874306008132,-1.,3.40957978266622));
#61058=CARTESIAN_POINT('Ctrl Pts',(-1.93874306008132,1.,3.40957978266622));
#61059=CARTESIAN_POINT('Ctrl Pts',(-1.94042111965237,-1.,3.41692971994082));
#61060=CARTESIAN_POINT('Ctrl Pts',(-1.94042111965237,1.,3.41692971994082));
#61061=CARTESIAN_POINT('Ctrl Pts',(-1.94205835913692,-1.,3.42430850941497));
#61062=CARTESIAN_POINT('Ctrl Pts',(-1.94205835913692,1.,3.42430850941497));
#61063=CARTESIAN_POINT('Ctrl Pts',(-1.94364973660285,-1.,3.43170586602436));
#61064=CARTESIAN_POINT('Ctrl Pts',(-1.94364973660285,1.,3.43170586602436));
#61065=CARTESIAN_POINT('Ctrl Pts',(-1.94519168842883,-1.,3.43911410197693));
#61066=CARTESIAN_POINT('Ctrl Pts',(-1.94519168842883,1.,3.43911410197693));
#61067=CARTESIAN_POINT('Ctrl Pts',(-1.94668377715332,-1.,3.44653088665685));
#61068=CARTESIAN_POINT('Ctrl Pts',(-1.94668377715332,1.,3.44653088665685));
#61069=CARTESIAN_POINT('Ctrl Pts',(-1.94812754766524,-1.,3.45395731584051));
#61070=CARTESIAN_POINT('Ctrl Pts',(-1.94812754766524,1.,3.45395731584051));
#61071=CARTESIAN_POINT('Ctrl Pts',(-1.94952575850196,-1.,3.46139661060959));
#61072=CARTESIAN_POINT('Ctrl Pts',(-1.94952575850196,1.,3.46139661060959));
#61073=CARTESIAN_POINT('Ctrl Pts',(-1.95088147859876,-1.,3.4688525897419));
#61074=CARTESIAN_POINT('Ctrl Pts',(-1.95088147859876,1.,3.4688525897419));
#61075=CARTESIAN_POINT('Ctrl Pts',(-1.95219722189878,-1.,3.47632820495926));
#61076=CARTESIAN_POINT('Ctrl Pts',(-1.95219722189878,1.,3.47632820495926));
#61077=CARTESIAN_POINT('Ctrl Pts',(-1.95347412486316,-1.,3.48382414832648));
#61078=CARTESIAN_POINT('Ctrl Pts',(-1.95347412486316,1.,3.48382414832648));
#61079=CARTESIAN_POINT('Ctrl Pts',(-1.95471236969653,-1.,3.49133956289154));
#61080=CARTESIAN_POINT('Ctrl Pts',(-1.95471236969653,1.,3.49133956289154));
#61081=CARTESIAN_POINT('Ctrl Pts',(-1.9559115382367,-1.,3.49887263575602));
#61082=CARTESIAN_POINT('Ctrl Pts',(-1.9559115382367,1.,3.49887263575602));
#61083=CARTESIAN_POINT('Ctrl Pts',(-1.95707099606514,-1.,3.50642124159913));
#61084=CARTESIAN_POINT('Ctrl Pts',(-1.95707099606514,1.,3.50642124159913));
#61085=CARTESIAN_POINT('Ctrl Pts',(-1.95819025316768,-1.,3.51398354617772));
#61086=CARTESIAN_POINT('Ctrl Pts',(-1.95819025316768,1.,3.51398354617772));
#61087=CARTESIAN_POINT('Ctrl Pts',(-1.95926936324436,-1.,3.52155867431438));
#61088=CARTESIAN_POINT('Ctrl Pts',(-1.95926936324436,1.,3.52155867431438));
#61089=CARTESIAN_POINT('Ctrl Pts',(-1.96030879411534,-1.,3.52914648844289));
#61090=CARTESIAN_POINT('Ctrl Pts',(-1.96030879411534,1.,3.52914648844289));
#61091=CARTESIAN_POINT('Ctrl Pts',(-1.96130926212661,-1.,3.53674730625759));
#61092=CARTESIAN_POINT('Ctrl Pts',(-1.96130926212661,1.,3.53674730625759));
#61093=CARTESIAN_POINT('Ctrl Pts',(-1.96227157573058,-1.,3.54436163300425));
#61094=CARTESIAN_POINT('Ctrl Pts',(-1.96227157573058,1.,3.54436163300425));
#61095=CARTESIAN_POINT('Ctrl Pts',(-1.96319648628667,-1.,3.55198990600929));
#61096=CARTESIAN_POINT('Ctrl Pts',(-1.96319648628667,1.,3.55198990600929));
#61097=CARTESIAN_POINT('Ctrl Pts',(-1.96408450906868,-1.,3.55963218706201));
#61098=CARTESIAN_POINT('Ctrl Pts',(-1.96408450906868,1.,3.55963218706201));
#61099=CARTESIAN_POINT('Ctrl Pts',(-1.96493594634643,-1.,3.56728820357933));
#61100=CARTESIAN_POINT('Ctrl Pts',(-1.96493594634643,1.,3.56728820357933));
#61101=CARTESIAN_POINT('Ctrl Pts',(-1.96575096652857,-1.,3.57495748601088));
#61102=CARTESIAN_POINT('Ctrl Pts',(-1.96575096652857,1.,3.57495748601088));
#61103=CARTESIAN_POINT('Ctrl Pts',(-1.9665296668894,-1.,3.58263947663884));
#61104=CARTESIAN_POINT('Ctrl Pts',(-1.9665296668894,1.,3.58263947663884));
#61105=CARTESIAN_POINT('Ctrl Pts',(-1.96727213799507,-1.,3.5903336402273));
#61106=CARTESIAN_POINT('Ctrl Pts',(-1.96727213799507,1.,3.5903336402273));
#61107=CARTESIAN_POINT('Ctrl Pts',(-1.96797854118257,-1.,3.59803959819725));
#61108=CARTESIAN_POINT('Ctrl Pts',(-1.96797854118257,1.,3.59803959819725));
#61109=CARTESIAN_POINT('Ctrl Pts',(-1.96864911885775,-1.,3.60575714017676));
#61110=CARTESIAN_POINT('Ctrl Pts',(-1.96864911885775,1.,3.60575714017676));
#61111=CARTESIAN_POINT('Ctrl Pts',(-1.96928416040712,-1.,3.61348615496393));
#61112=CARTESIAN_POINT('Ctrl Pts',(-1.96928416040712,1.,3.61348615496393));
#61113=CARTESIAN_POINT('Ctrl Pts',(-1.96988398129888,-1.,3.62122658401722));
#61114=CARTESIAN_POINT('Ctrl Pts',(-1.96988398129888,1.,3.62122658401722));
#61115=CARTESIAN_POINT('Ctrl Pts',(-1.97044889850518,-1.,3.62897836973397));
#61116=CARTESIAN_POINT('Ctrl Pts',(-1.97044889850518,1.,3.62897836973397));
#61117=CARTESIAN_POINT('Ctrl Pts',(-1.97097920454698,-1.,3.63674139590853));
#61118=CARTESIAN_POINT('Ctrl Pts',(-1.97097920454698,1.,3.63674139590853));
#61119=CARTESIAN_POINT('Ctrl Pts',(-1.97147515441539,-1.,3.64451546724221));
#61120=CARTESIAN_POINT('Ctrl Pts',(-1.97147515441539,1.,3.64451546724221));
#61121=CARTESIAN_POINT('Ctrl Pts',(-1.97193697240645,-1.,3.65230034717364));
#61122=CARTESIAN_POINT('Ctrl Pts',(-1.97193697240645,1.,3.65230034717364));
#61123=CARTESIAN_POINT('Ctrl Pts',(-1.97236485439317,-1.,3.66009578166865));
#61124=CARTESIAN_POINT('Ctrl Pts',(-1.97236485439317,1.,3.66009578166865));
#61125=CARTESIAN_POINT('Ctrl Pts',(-1.9727589719863,-1.,3.66790152751984));
#61126=CARTESIAN_POINT('Ctrl Pts',(-1.9727589719863,1.,3.66790152751984));
#61127=CARTESIAN_POINT('Ctrl Pts',(-1.97311947678035,-1.,3.67571738106175));
#61128=CARTESIAN_POINT('Ctrl Pts',(-1.97311947678035,1.,3.67571738106175));
#61129=CARTESIAN_POINT('Ctrl Pts',(-1.97344650303631,-1.,3.68354319913416));
#61130=CARTESIAN_POINT('Ctrl Pts',(-1.97344650303631,1.,3.68354319913416));
#61131=CARTESIAN_POINT('Ctrl Pts',(-1.97374016224397,-1.,3.69137888597855));
#61132=CARTESIAN_POINT('Ctrl Pts',(-1.97374016224397,1.,3.69137888597855));
#61133=CARTESIAN_POINT('Ctrl Pts',(-1.97394846382289,-1.,3.69765528558292));
#61134=CARTESIAN_POINT('Ctrl Pts',(-1.97394846382289,1.,3.69765528558292));
#61135=CARTESIAN_POINT('Ctrl Pts',(-1.97408973726149,-1.,3.70236698911837));
#61136=CARTESIAN_POINT('Ctrl Pts',(-1.97408973726149,1.,3.70236698911837));
#61137=CARTESIAN_POINT('Ctrl Pts',(-1.974177276451,-1.,3.7055100813194));
#61138=CARTESIAN_POINT('Ctrl Pts',(-1.974177276451,1.,3.7055100813194));
#61139=CARTESIAN_POINT('Ctrl Pts',(-1.97421938526992,-1.,3.70708211654725));
#61140=CARTESIAN_POINT('Ctrl Pts',(-1.97421938526992,1.,3.70708211654725));
#61141=CARTESIAN_POINT('',(-1.88097764062542,1.,3.24413672884902));
#61142=CARTESIAN_POINT('Ctrl Pts',(-1.88097764062542,-1.,3.24413672884902));
#61143=CARTESIAN_POINT('Ctrl Pts',(-1.88097764062542,-0.666666666666667,
3.24413672884902));
#61144=CARTESIAN_POINT('Ctrl Pts',(-1.88097764062542,-0.333333333333333,
3.24413672884902));
#61145=CARTESIAN_POINT('Ctrl Pts',(-1.88097764062542,0.333333333333333,
3.24413672884902));
#61146=CARTESIAN_POINT('Ctrl Pts',(-1.88097764062542,0.666666666666667,
3.24413672884902));
#61147=CARTESIAN_POINT('Ctrl Pts',(-1.88097764062542,1.,3.24413672884902));
#61148=CARTESIAN_POINT('',(-1.97421938526992,1.,3.70708211654725));
#61149=CARTESIAN_POINT('',(-1.97421938526992,0.,3.70708211654725));
#61150=CARTESIAN_POINT('Ctrl Pts',(-1.88097764062542,1.,3.24413672884902));
#61151=CARTESIAN_POINT('Ctrl Pts',(-1.88102292397987,1.,3.24415531671311));
#61152=CARTESIAN_POINT('Ctrl Pts',(-1.88117508446657,1.,3.24428080352952));
#61153=CARTESIAN_POINT('Ctrl Pts',(-1.88156537699118,1.,3.24480754675942));
#61154=CARTESIAN_POINT('Ctrl Pts',(-1.88242596600422,1.,3.24625654410705));
#61155=CARTESIAN_POINT('Ctrl Pts',(-1.88407708646435,1.,3.24935200512055));
#61156=CARTESIAN_POINT('Ctrl Pts',(-1.88646802523372,1.,3.25408686339298));
#61157=CARTESIAN_POINT('Ctrl Pts',(-1.88934996203508,1.,3.2599988519361));
#61158=CARTESIAN_POINT('Ctrl Pts',(-1.89255393500769,1.,3.2667765388833));
#61159=CARTESIAN_POINT('Ctrl Pts',(-1.89589172903662,1.,3.27407108932908));
#61160=CARTESIAN_POINT('Ctrl Pts',(-1.89918429230425,1.,3.28154737912287));
#61161=CARTESIAN_POINT('Ctrl Pts',(-1.9022897124757,1.,3.28893448600364));
#61162=CARTESIAN_POINT('Ctrl Pts',(-1.9051389186417,1.,3.29608978722258));
#61163=CARTESIAN_POINT('Ctrl Pts',(-1.90773912171424,1.,3.30300595568341));
#61164=CARTESIAN_POINT('Ctrl Pts',(-1.91014297830502,1.,3.30975721158694));
#61165=CARTESIAN_POINT('Ctrl Pts',(-1.91242616234459,1.,3.31646052426395));
#61166=CARTESIAN_POINT('Ctrl Pts',(-1.91466343916612,1.,3.32323403454507));
#61167=CARTESIAN_POINT('Ctrl Pts',(-1.91690081930297,1.,3.33014884257812));
#61168=CARTESIAN_POINT('Ctrl Pts',(-1.91914609610173,1.,3.33721230709948));
#61169=CARTESIAN_POINT('Ctrl Pts',(-1.92138450828378,1.,3.34439448941915));
#61170=CARTESIAN_POINT('Ctrl Pts',(-1.92358838440518,1.,3.35164424847206));
#61171=CARTESIAN_POINT('Ctrl Pts',(-1.92572846125763,1.,3.35890824422976));
#61172=CARTESIAN_POINT('Ctrl Pts',(-1.92778626543803,1.,3.36615168657597));
#61173=CARTESIAN_POINT('Ctrl Pts',(-1.92975993109897,1.,3.37336807068078));
#61174=CARTESIAN_POINT('Ctrl Pts',(-1.93165739093292,1.,3.38056768525577));
#61175=CARTESIAN_POINT('Ctrl Pts',(-1.93349233176794,1.,3.38777076883267));
#61176=CARTESIAN_POINT('Ctrl Pts',(-1.93527929945982,1.,3.39499923640789));
#61177=CARTESIAN_POINT('Ctrl Pts',(-1.93702857723089,1.,3.40226802104093));
#61178=CARTESIAN_POINT('Ctrl Pts',(-1.93874306008132,1.,3.40957978266622));
#61179=CARTESIAN_POINT('Ctrl Pts',(-1.94042111965237,1.,3.41692971994082));
#61180=CARTESIAN_POINT('Ctrl Pts',(-1.94205835913692,1.,3.42430850941497));
#61181=CARTESIAN_POINT('Ctrl Pts',(-1.94364973660285,1.,3.43170586602436));
#61182=CARTESIAN_POINT('Ctrl Pts',(-1.94519168842883,1.,3.43911410197693));
#61183=CARTESIAN_POINT('Ctrl Pts',(-1.94668377715332,1.,3.44653088665685));
#61184=CARTESIAN_POINT('Ctrl Pts',(-1.94812754766524,1.,3.45395731584051));
#61185=CARTESIAN_POINT('Ctrl Pts',(-1.94952575850196,1.,3.46139661060959));
#61186=CARTESIAN_POINT('Ctrl Pts',(-1.95088147859876,1.,3.4688525897419));
#61187=CARTESIAN_POINT('Ctrl Pts',(-1.95219722189878,1.,3.47632820495926));
#61188=CARTESIAN_POINT('Ctrl Pts',(-1.95347412486316,1.,3.48382414832648));
#61189=CARTESIAN_POINT('Ctrl Pts',(-1.95471236969653,1.,3.49133956289154));
#61190=CARTESIAN_POINT('Ctrl Pts',(-1.9559115382367,1.,3.49887263575602));
#61191=CARTESIAN_POINT('Ctrl Pts',(-1.95707099606514,1.,3.50642124159913));
#61192=CARTESIAN_POINT('Ctrl Pts',(-1.95819025316768,1.,3.51398354617772));
#61193=CARTESIAN_POINT('Ctrl Pts',(-1.95926936324436,1.,3.52155867431438));
#61194=CARTESIAN_POINT('Ctrl Pts',(-1.96030879411534,1.,3.52914648844289));
#61195=CARTESIAN_POINT('Ctrl Pts',(-1.96130926212661,1.,3.53674730625759));
#61196=CARTESIAN_POINT('Ctrl Pts',(-1.96227157573058,1.,3.54436163300425));
#61197=CARTESIAN_POINT('Ctrl Pts',(-1.96319648628667,1.,3.55198990600929));
#61198=CARTESIAN_POINT('Ctrl Pts',(-1.96408450906868,1.,3.55963218706201));
#61199=CARTESIAN_POINT('Ctrl Pts',(-1.96493594634643,1.,3.56728820357933));
#61200=CARTESIAN_POINT('Ctrl Pts',(-1.96575096652857,1.,3.57495748601088));
#61201=CARTESIAN_POINT('Ctrl Pts',(-1.9665296668894,1.,3.58263947663884));
#61202=CARTESIAN_POINT('Ctrl Pts',(-1.96727213799507,1.,3.5903336402273));
#61203=CARTESIAN_POINT('Ctrl Pts',(-1.96797854118257,1.,3.59803959819725));
#61204=CARTESIAN_POINT('Ctrl Pts',(-1.96864911885775,1.,3.60575714017676));
#61205=CARTESIAN_POINT('Ctrl Pts',(-1.96928416040712,1.,3.61348615496393));
#61206=CARTESIAN_POINT('Ctrl Pts',(-1.96988398129888,1.,3.62122658401722));
#61207=CARTESIAN_POINT('Ctrl Pts',(-1.97044889850518,1.,3.62897836973397));
#61208=CARTESIAN_POINT('Ctrl Pts',(-1.97097920454698,1.,3.63674139590853));
#61209=CARTESIAN_POINT('Ctrl Pts',(-1.97147515441539,1.,3.64451546724221));
#61210=CARTESIAN_POINT('Ctrl Pts',(-1.97193697240645,1.,3.65230034717364));
#61211=CARTESIAN_POINT('Ctrl Pts',(-1.97236485439317,1.,3.66009578166865));
#61212=CARTESIAN_POINT('Ctrl Pts',(-1.9727589719863,1.,3.66790152751984));
#61213=CARTESIAN_POINT('Ctrl Pts',(-1.97311947678035,1.,3.67571738106175));
#61214=CARTESIAN_POINT('Ctrl Pts',(-1.97344650303631,1.,3.68354319913416));
#61215=CARTESIAN_POINT('Ctrl Pts',(-1.97374016224397,1.,3.69137888597855));
#61216=CARTESIAN_POINT('Ctrl Pts',(-1.97394846382289,1.,3.69765528558292));
#61217=CARTESIAN_POINT('Ctrl Pts',(-1.97408973726149,1.,3.70236698911837));
#61218=CARTESIAN_POINT('Ctrl Pts',(-1.974177276451,1.,3.7055100813194));
#61219=CARTESIAN_POINT('Ctrl Pts',(-1.97421938526992,1.,3.70708211654725));
#61220=CARTESIAN_POINT('Origin',(-1.97421938526992,0.,3.70708211654725));
#61221=CARTESIAN_POINT('',(-1.83867539237861,1.,3.77614523045147));
#61222=CARTESIAN_POINT('Origin',(0.,0.,0.));
#61223=CARTESIAN_POINT('',(-2.03660101169564,1.,3.14877060440425));
#61224=CARTESIAN_POINT('Origin',(0.,1.,0.));
#61225=CARTESIAN_POINT('Ctrl Pts',(-2.03660101169564,1.,3.14877060440425));
#61226=CARTESIAN_POINT('Ctrl Pts',(-2.03660101169564,0.666666666666667,
3.14877060440425));
#61227=CARTESIAN_POINT('Ctrl Pts',(-2.03660101169564,0.333333333333333,
3.14877060440425));
#61228=CARTESIAN_POINT('Ctrl Pts',(-2.03660101169564,-0.333333333333333,
3.14877060440425));
#61229=CARTESIAN_POINT('Ctrl Pts',(-2.03660101169564,-0.666666666666667,
3.14877060440425));
#61230=CARTESIAN_POINT('Ctrl Pts',(-2.03660101169564,-1.,3.14877060440425));
#61231=CARTESIAN_POINT('Ctrl Pts',(-2.40675750623143,-1.,3.44202241512147));
#61232=CARTESIAN_POINT('Ctrl Pts',(-2.40675750623143,1.,3.44202241512147));
#61233=CARTESIAN_POINT('Ctrl Pts',(-2.40537592959345,-1.,3.44127120683402));
#61234=CARTESIAN_POINT('Ctrl Pts',(-2.40537592959345,1.,3.44127120683402));
#61235=CARTESIAN_POINT('Ctrl Pts',(-2.40261515590099,-1.,3.43976627485223));
#61236=CARTESIAN_POINT('Ctrl Pts',(-2.40261515590099,1.,3.43976627485223));
#61237=CARTESIAN_POINT('Ctrl Pts',(-2.39848113411429,-1.,3.43750133066036));
#61238=CARTESIAN_POINT('Ctrl Pts',(-2.39848113411429,1.,3.43750133066036));
#61239=CARTESIAN_POINT('Ctrl Pts',(-2.39298338805823,-1.,3.43446630680436));
#61240=CARTESIAN_POINT('Ctrl Pts',(-2.39298338805823,1.,3.43446630680436));
#61241=CARTESIAN_POINT('Ctrl Pts',(-2.38613505844641,-1.,3.43064732714472));
#61242=CARTESIAN_POINT('Ctrl Pts',(-2.38613505844641,1.,3.43064732714472));
#61243=CARTESIAN_POINT('Ctrl Pts',(-2.37931067029517,-1.,3.42680309755241));
#61244=CARTESIAN_POINT('Ctrl Pts',(-2.37931067029517,1.,3.42680309755241));
#61245=CARTESIAN_POINT('Ctrl Pts',(-2.37251035954351,-1.,3.42293356216595));
#61246=CARTESIAN_POINT('Ctrl Pts',(-2.37251035954351,1.,3.42293356216595));
#61247=CARTESIAN_POINT('Ctrl Pts',(-2.36573431470314,-1.,3.41903866635384));
#61248=CARTESIAN_POINT('Ctrl Pts',(-2.36573431470314,1.,3.41903866635384));
#61249=CARTESIAN_POINT('Ctrl Pts',(-2.35898278606449,-1.,3.4151183675076));
#61250=CARTESIAN_POINT('Ctrl Pts',(-2.35898278606449,1.,3.4151183675076));
#61251=CARTESIAN_POINT('Ctrl Pts',(-2.35225606823649,-1.,3.41117262313464));
#61252=CARTESIAN_POINT('Ctrl Pts',(-2.35225606823649,1.,3.41117262313464));
#61253=CARTESIAN_POINT('Ctrl Pts',(-2.34555447648901,-1.,3.40720137403888));
#61254=CARTESIAN_POINT('Ctrl Pts',(-2.34555447648901,1.,3.40720137403888));
#61255=CARTESIAN_POINT('Ctrl Pts',(-2.33887832342715,-1.,3.40320452776646));
#61256=CARTESIAN_POINT('Ctrl Pts',(-2.33887832342715,1.,3.40320452776646));
#61257=CARTESIAN_POINT('Ctrl Pts',(-2.33222789882601,-1.,3.39918194578115));
#61258=CARTESIAN_POINT('Ctrl Pts',(-2.33222789882601,1.,3.39918194578115));
#61259=CARTESIAN_POINT('Ctrl Pts',(-2.32560343902683,-1.,3.39513342020045));
#61260=CARTESIAN_POINT('Ctrl Pts',(-2.32560343902683,1.,3.39513342020045));
#61261=CARTESIAN_POINT('Ctrl Pts',(-2.31900513925627,-1.,3.39105869475112));
#61262=CARTESIAN_POINT('Ctrl Pts',(-2.31900513925627,1.,3.39105869475112));
#61263=CARTESIAN_POINT('Ctrl Pts',(-2.31243319489505,-1.,3.38695751492659));
#61264=CARTESIAN_POINT('Ctrl Pts',(-2.31243319489505,1.,3.38695751492659));
#61265=CARTESIAN_POINT('Ctrl Pts',(-2.30588783640389,-1.,3.38282967336676));
#61266=CARTESIAN_POINT('Ctrl Pts',(-2.30588783640389,1.,3.38282967336676));
#61267=CARTESIAN_POINT('Ctrl Pts',(-2.29936936127588,-1.,3.37867504959382));
#61268=CARTESIAN_POINT('Ctrl Pts',(-2.29936936127588,1.,3.37867504959382));
#61269=CARTESIAN_POINT('Ctrl Pts',(-2.2928781800731,-1.,3.37449367172707));
#61270=CARTESIAN_POINT('Ctrl Pts',(-2.2928781800731,1.,3.37449367172707));
#61271=CARTESIAN_POINT('Ctrl Pts',(-2.28641481081045,-1.,3.37028570206357));
#61272=CARTESIAN_POINT('Ctrl Pts',(-2.28641481081045,1.,3.37028570206357));
#61273=CARTESIAN_POINT('Ctrl Pts',(-2.27997979457968,-1.,3.36605130712978));
#61274=CARTESIAN_POINT('Ctrl Pts',(-2.27997979457968,1.,3.36605130712978));
#61275=CARTESIAN_POINT('Ctrl Pts',(-2.27357362620902,-1.,3.36179055004369));
#61276=CARTESIAN_POINT('Ctrl Pts',(-2.27357362620902,1.,3.36179055004369));
#61277=CARTESIAN_POINT('Ctrl Pts',(-2.26719668579921,-1.,3.35750328523077));
#61278=CARTESIAN_POINT('Ctrl Pts',(-2.26719668579921,1.,3.35750328523077));
#61279=CARTESIAN_POINT('Ctrl Pts',(-2.26084915222484,-1.,3.35318902552676));
#61280=CARTESIAN_POINT('Ctrl Pts',(-2.26084915222484,1.,3.35318902552676));
#61281=CARTESIAN_POINT('Ctrl Pts',(-2.25453097693524,-1.,3.34884690292342));
#61282=CARTESIAN_POINT('Ctrl Pts',(-2.25453097693524,1.,3.34884690292342));
#61283=CARTESIAN_POINT('Ctrl Pts',(-2.24824207678288,-1.,3.34447596770768));
#61284=CARTESIAN_POINT('Ctrl Pts',(-2.24824207678288,1.,3.34447596770768));
#61285=CARTESIAN_POINT('Ctrl Pts',(-2.24198249391437,-1.,3.34007543738044));
#61286=CARTESIAN_POINT('Ctrl Pts',(-2.24198249391437,1.,3.34007543738044));
#61287=CARTESIAN_POINT('Ctrl Pts',(-2.2357525632881,-1.,3.33564495756478));
#61288=CARTESIAN_POINT('Ctrl Pts',(-2.2357525632881,1.,3.33564495756478));
#61289=CARTESIAN_POINT('Ctrl Pts',(-2.22955308907221,-1.,3.33118487773593));
#61290=CARTESIAN_POINT('Ctrl Pts',(-2.22955308907221,1.,3.33118487773593));
#61291=CARTESIAN_POINT('Ctrl Pts',(-2.22338548312758,-1.,3.32669646722871));
#61292=CARTESIAN_POINT('Ctrl Pts',(-2.22338548312758,1.,3.32669646722871));
#61293=CARTESIAN_POINT('Ctrl Pts',(-2.21725135110889,-1.,3.32218125618955));
#61294=CARTESIAN_POINT('Ctrl Pts',(-2.21725135110889,1.,3.32218125618955));
#61295=CARTESIAN_POINT('Ctrl Pts',(-2.21115211847872,-1.,3.31764044024231));
#61296=CARTESIAN_POINT('Ctrl Pts',(-2.21115211847872,1.,3.31764044024231));
#61297=CARTESIAN_POINT('Ctrl Pts',(-2.20508863150608,-1.,3.3130742460895));
#61298=CARTESIAN_POINT('Ctrl Pts',(-2.20508863150608,1.,3.3130742460895));
#61299=CARTESIAN_POINT('Ctrl Pts',(-2.19906078949924,-1.,3.30848134694596));
#61300=CARTESIAN_POINT('Ctrl Pts',(-2.19906078949924,1.,3.30848134694596));
#61301=CARTESIAN_POINT('Ctrl Pts',(-2.19306710376112,-1.,3.30385816281831));
#61302=CARTESIAN_POINT('Ctrl Pts',(-2.19306710376112,1.,3.30385816281831));
#61303=CARTESIAN_POINT('Ctrl Pts',(-2.18710556500325,-1.,3.29920022557635));
#61304=CARTESIAN_POINT('Ctrl Pts',(-2.18710556500325,1.,3.29920022557635));
#61305=CARTESIAN_POINT('Ctrl Pts',(-2.18117455557062,-1.,3.29450361500484));
#61306=CARTESIAN_POINT('Ctrl Pts',(-2.18117455557062,1.,3.29450361500484));
#61307=CARTESIAN_POINT('Ctrl Pts',(-2.17527380048422,-1.,3.28976645712566));
#61308=CARTESIAN_POINT('Ctrl Pts',(-2.17527380048422,1.,3.28976645712566));
#61309=CARTESIAN_POINT('Ctrl Pts',(-2.16940517773459,-1.,3.2849901997973));
#61310=CARTESIAN_POINT('Ctrl Pts',(-2.16940517773459,1.,3.2849901997973));
#61311=CARTESIAN_POINT('Ctrl Pts',(-2.16357391934434,-1.,3.28018150841414));
#61312=CARTESIAN_POINT('Ctrl Pts',(-2.16357391934434,1.,3.28018150841414));
#61313=CARTESIAN_POINT('Ctrl Pts',(-2.15778690038359,-1.,3.27534954469206));
#61314=CARTESIAN_POINT('Ctrl Pts',(-2.15778690038359,1.,3.27534954469206));
#61315=CARTESIAN_POINT('Ctrl Pts',(-2.15205043199818,-1.,3.27050245897244));
#61316=CARTESIAN_POINT('Ctrl Pts',(-2.15205043199818,1.,3.27050245897244));
#61317=CARTESIAN_POINT('Ctrl Pts',(-2.14636805295663,-1.,3.26564388189764));
#61318=CARTESIAN_POINT('Ctrl Pts',(-2.14636805295663,1.,3.26564388189764));
#61319=CARTESIAN_POINT('Ctrl Pts',(-2.14073870754257,-1.,3.26077002641868));
#61320=CARTESIAN_POINT('Ctrl Pts',(-2.14073870754257,1.,3.26077002641868));
#61321=CARTESIAN_POINT('Ctrl Pts',(-2.13515375878786,-1.,3.25586495065027));
#61322=CARTESIAN_POINT('Ctrl Pts',(-2.13515375878786,1.,3.25586495065027));
#61323=CARTESIAN_POINT('Ctrl Pts',(-2.1296002839681,-1.,3.25090574493994));
#61324=CARTESIAN_POINT('Ctrl Pts',(-2.1296002839681,1.,3.25090574493994));
#61325=CARTESIAN_POINT('Ctrl Pts',(-2.12406646410943,-1.,3.24587102613347));
#61326=CARTESIAN_POINT('Ctrl Pts',(-2.12406646410943,1.,3.24587102613347));
#61327=CARTESIAN_POINT('Ctrl Pts',(-2.11854673326972,-1.,3.24074905517282));
#61328=CARTESIAN_POINT('Ctrl Pts',(-2.11854673326972,1.,3.24074905517282));
#61329=CARTESIAN_POINT('Ctrl Pts',(-2.11304604021784,-1.,3.23554444767115));
#61330=CARTESIAN_POINT('Ctrl Pts',(-2.11304604021784,1.,3.23554444767115));
#61331=CARTESIAN_POINT('Ctrl Pts',(-2.1075869964248,-1.,3.23028945793334));
#61332=CARTESIAN_POINT('Ctrl Pts',(-2.1075869964248,1.,3.23028945793334));
#61333=CARTESIAN_POINT('Ctrl Pts',(-2.10220384298533,-1.,3.22503437553496));
#61334=CARTESIAN_POINT('Ctrl Pts',(-2.10220384298533,1.,3.22503437553496));
#61335=CARTESIAN_POINT('Ctrl Pts',(-2.09692958434933,-1.,3.21982707347067));
#61336=CARTESIAN_POINT('Ctrl Pts',(-2.09692958434933,1.,3.21982707347067));
#61337=CARTESIAN_POINT('Ctrl Pts',(-2.0917841946046,-1.,3.2146942960168));
#61338=CARTESIAN_POINT('Ctrl Pts',(-2.0917841946046,1.,3.2146942960168));
#61339=CARTESIAN_POINT('Ctrl Pts',(-2.08676465517435,-1.,3.20962575845433));
#61340=CARTESIAN_POINT('Ctrl Pts',(-2.08676465517435,1.,3.20962575845433));
#61341=CARTESIAN_POINT('Ctrl Pts',(-2.08182850370816,-1.,3.20454818630635));
#61342=CARTESIAN_POINT('Ctrl Pts',(-2.08182850370816,1.,3.20454818630635));
#61343=CARTESIAN_POINT('Ctrl Pts',(-2.0769044187063,-1.,3.19934132835879));
#61344=CARTESIAN_POINT('Ctrl Pts',(-2.0769044187063,1.,3.19934132835879));
#61345=CARTESIAN_POINT('Ctrl Pts',(-2.07192253497765,-1.,3.19388465568113));
#61346=CARTESIAN_POINT('Ctrl Pts',(-2.07192253497765,1.,3.19388465568113));
#61347=CARTESIAN_POINT('Ctrl Pts',(-2.06684062744065,-1.,3.18809755562297));
#61348=CARTESIAN_POINT('Ctrl Pts',(-2.06684062744065,1.,3.18809755562297));
#61349=CARTESIAN_POINT('Ctrl Pts',(-2.06166849827143,-1.,3.18197692964677));
#61350=CARTESIAN_POINT('Ctrl Pts',(-2.06166849827143,1.,3.18197692964677));
#61351=CARTESIAN_POINT('Ctrl Pts',(-2.05650186773279,-1.,3.17564906975592));
#61352=CARTESIAN_POINT('Ctrl Pts',(-2.05650186773279,1.,3.17564906975592));
#61353=CARTESIAN_POINT('Ctrl Pts',(-2.05151770247452,-1.,3.16936341689859));
#61354=CARTESIAN_POINT('Ctrl Pts',(-2.05151770247452,1.,3.16936341689859));
#61355=CARTESIAN_POINT('Ctrl Pts',(-2.0469333124766,-1.,3.16343165059235));
#61356=CARTESIAN_POINT('Ctrl Pts',(-2.0469333124766,1.,3.16343165059235));
#61357=CARTESIAN_POINT('Ctrl Pts',(-2.04297406404132,-1.,3.15817983946525));
#61358=CARTESIAN_POINT('Ctrl Pts',(-2.04297406404132,1.,3.15817983946525));
#61359=CARTESIAN_POINT('Ctrl Pts',(-2.03984073791432,-1.,3.1538999167466));
#61360=CARTESIAN_POINT('Ctrl Pts',(-2.03984073791432,1.,3.1538999167466));
#61361=CARTESIAN_POINT('Ctrl Pts',(-2.03766932526171,-1.,3.15079010635326));
#61362=CARTESIAN_POINT('Ctrl Pts',(-2.03766932526171,1.,3.15079010635326));
#61363=CARTESIAN_POINT('Ctrl Pts',(-2.03675273048882,-1.,3.14931281967585));
#61364=CARTESIAN_POINT('Ctrl Pts',(-2.03675273048882,1.,3.14931281967585));
#61365=CARTESIAN_POINT('Ctrl Pts',(-2.03653654935384,-1.,3.14878756590499));
#61366=CARTESIAN_POINT('Ctrl Pts',(-2.03653654935384,1.,3.14878756590499));
#61367=CARTESIAN_POINT('Ctrl Pts',(-2.036601737578,-1.,3.14869618937138));
#61368=CARTESIAN_POINT('Ctrl Pts',(-2.036601737578,1.,3.14869618937138));
#61369=CARTESIAN_POINT('Ctrl Pts',(-2.03668666247593,-1.,3.1487152044751));
#61370=CARTESIAN_POINT('Ctrl Pts',(-2.03668666247593,1.,3.1487152044751));
#61371=CARTESIAN_POINT('',(-2.40675750623143,1.,3.44202241512147));
#61372=CARTESIAN_POINT('Ctrl Pts',(-2.40675750623143,1.,3.44202241512147));
#61373=CARTESIAN_POINT('Ctrl Pts',(-2.40537592959345,1.,3.44127120683402));
#61374=CARTESIAN_POINT('Ctrl Pts',(-2.40261515590099,1.,3.43976627485223));
#61375=CARTESIAN_POINT('Ctrl Pts',(-2.39848113411429,1.,3.43750133066036));
#61376=CARTESIAN_POINT('Ctrl Pts',(-2.39298338805823,1.,3.43446630680436));
#61377=CARTESIAN_POINT('Ctrl Pts',(-2.38613505844641,1.,3.43064732714472));
#61378=CARTESIAN_POINT('Ctrl Pts',(-2.37931067029517,1.,3.42680309755241));
#61379=CARTESIAN_POINT('Ctrl Pts',(-2.37251035954351,1.,3.42293356216595));
#61380=CARTESIAN_POINT('Ctrl Pts',(-2.36573431470314,1.,3.41903866635384));
#61381=CARTESIAN_POINT('Ctrl Pts',(-2.35898278606449,1.,3.4151183675076));
#61382=CARTESIAN_POINT('Ctrl Pts',(-2.35225606823649,1.,3.41117262313464));
#61383=CARTESIAN_POINT('Ctrl Pts',(-2.34555447648901,1.,3.40720137403888));
#61384=CARTESIAN_POINT('Ctrl Pts',(-2.33887832342715,1.,3.40320452776646));
#61385=CARTESIAN_POINT('Ctrl Pts',(-2.33222789882601,1.,3.39918194578115));
#61386=CARTESIAN_POINT('Ctrl Pts',(-2.32560343902683,1.,3.39513342020045));
#61387=CARTESIAN_POINT('Ctrl Pts',(-2.31900513925627,1.,3.39105869475112));
#61388=CARTESIAN_POINT('Ctrl Pts',(-2.31243319489505,1.,3.38695751492659));
#61389=CARTESIAN_POINT('Ctrl Pts',(-2.30588783640389,1.,3.38282967336676));
#61390=CARTESIAN_POINT('Ctrl Pts',(-2.29936936127588,1.,3.37867504959382));
#61391=CARTESIAN_POINT('Ctrl Pts',(-2.2928781800731,1.,3.37449367172707));
#61392=CARTESIAN_POINT('Ctrl Pts',(-2.28641481081045,1.,3.37028570206357));
#61393=CARTESIAN_POINT('Ctrl Pts',(-2.27997979457968,1.,3.36605130712978));
#61394=CARTESIAN_POINT('Ctrl Pts',(-2.27357362620902,1.,3.36179055004369));
#61395=CARTESIAN_POINT('Ctrl Pts',(-2.26719668579921,1.,3.35750328523077));
#61396=CARTESIAN_POINT('Ctrl Pts',(-2.26084915222484,1.,3.35318902552676));
#61397=CARTESIAN_POINT('Ctrl Pts',(-2.25453097693524,1.,3.34884690292342));
#61398=CARTESIAN_POINT('Ctrl Pts',(-2.24824207678288,1.,3.34447596770768));
#61399=CARTESIAN_POINT('Ctrl Pts',(-2.24198249391437,1.,3.34007543738044));
#61400=CARTESIAN_POINT('Ctrl Pts',(-2.2357525632881,1.,3.33564495756478));
#61401=CARTESIAN_POINT('Ctrl Pts',(-2.22955308907221,1.,3.33118487773593));
#61402=CARTESIAN_POINT('Ctrl Pts',(-2.22338548312758,1.,3.32669646722871));
#61403=CARTESIAN_POINT('Ctrl Pts',(-2.21725135110889,1.,3.32218125618955));
#61404=CARTESIAN_POINT('Ctrl Pts',(-2.21115211847872,1.,3.31764044024231));
#61405=CARTESIAN_POINT('Ctrl Pts',(-2.20508863150608,1.,3.3130742460895));
#61406=CARTESIAN_POINT('Ctrl Pts',(-2.19906078949924,1.,3.30848134694596));
#61407=CARTESIAN_POINT('Ctrl Pts',(-2.19306710376112,1.,3.30385816281831));
#61408=CARTESIAN_POINT('Ctrl Pts',(-2.18710556500325,1.,3.29920022557635));
#61409=CARTESIAN_POINT('Ctrl Pts',(-2.18117455557062,1.,3.29450361500484));
#61410=CARTESIAN_POINT('Ctrl Pts',(-2.17527380048422,1.,3.28976645712566));
#61411=CARTESIAN_POINT('Ctrl Pts',(-2.16940517773459,1.,3.2849901997973));
#61412=CARTESIAN_POINT('Ctrl Pts',(-2.16357391934434,1.,3.28018150841414));
#61413=CARTESIAN_POINT('Ctrl Pts',(-2.15778690038359,1.,3.27534954469206));
#61414=CARTESIAN_POINT('Ctrl Pts',(-2.15205043199818,1.,3.27050245897244));
#61415=CARTESIAN_POINT('Ctrl Pts',(-2.14636805295663,1.,3.26564388189764));
#61416=CARTESIAN_POINT('Ctrl Pts',(-2.14073870754257,1.,3.26077002641868));
#61417=CARTESIAN_POINT('Ctrl Pts',(-2.13515375878786,1.,3.25586495065027));
#61418=CARTESIAN_POINT('Ctrl Pts',(-2.1296002839681,1.,3.25090574493994));
#61419=CARTESIAN_POINT('Ctrl Pts',(-2.12406646410943,1.,3.24587102613347));
#61420=CARTESIAN_POINT('Ctrl Pts',(-2.11854673326972,1.,3.24074905517282));
#61421=CARTESIAN_POINT('Ctrl Pts',(-2.11304604021784,1.,3.23554444767115));
#61422=CARTESIAN_POINT('Ctrl Pts',(-2.1075869964248,1.,3.23028945793334));
#61423=CARTESIAN_POINT('Ctrl Pts',(-2.10220384298533,1.,3.22503437553496));
#61424=CARTESIAN_POINT('Ctrl Pts',(-2.09692958434933,1.,3.21982707347067));
#61425=CARTESIAN_POINT('Ctrl Pts',(-2.0917841946046,1.,3.2146942960168));
#61426=CARTESIAN_POINT('Ctrl Pts',(-2.08676465517435,1.,3.20962575845433));
#61427=CARTESIAN_POINT('Ctrl Pts',(-2.08182850370816,1.,3.20454818630635));
#61428=CARTESIAN_POINT('Ctrl Pts',(-2.0769044187063,1.,3.19934132835879));
#61429=CARTESIAN_POINT('Ctrl Pts',(-2.07192253497765,1.,3.19388465568113));
#61430=CARTESIAN_POINT('Ctrl Pts',(-2.06684062744065,1.,3.18809755562297));
#61431=CARTESIAN_POINT('Ctrl Pts',(-2.06166849827143,1.,3.18197692964677));
#61432=CARTESIAN_POINT('Ctrl Pts',(-2.05650186773279,1.,3.17564906975592));
#61433=CARTESIAN_POINT('Ctrl Pts',(-2.05151770247452,1.,3.16936341689859));
#61434=CARTESIAN_POINT('Ctrl Pts',(-2.0469333124766,1.,3.16343165059235));
#61435=CARTESIAN_POINT('Ctrl Pts',(-2.04297406404132,1.,3.15817983946525));
#61436=CARTESIAN_POINT('Ctrl Pts',(-2.03984073791432,1.,3.1538999167466));
#61437=CARTESIAN_POINT('Ctrl Pts',(-2.03783225496023,1.,3.15102344775396));
#61438=CARTESIAN_POINT('Ctrl Pts',(-2.03693188810614,1.,3.14959882629936));
#61439=CARTESIAN_POINT('Ctrl Pts',(-2.03663974554941,1.,3.14901193669147));
#61440=CARTESIAN_POINT('Ctrl Pts',(-2.03659701539175,1.,3.1488193908823));
#61441=CARTESIAN_POINT('Ctrl Pts',(-2.03660101169564,1.,3.14877060440425));
#61442=CARTESIAN_POINT('',(-2.40675750623143,0.,3.44202241512147));
#61443=CARTESIAN_POINT('Ctrl Pts',(-2.36523532225181,-1.,2.91001063062876));
#61444=CARTESIAN_POINT('Ctrl Pts',(-2.36523532225181,1.,2.91001063062876));
#61445=CARTESIAN_POINT('Ctrl Pts',(-2.36524348105112,-1.,2.90992398626211));
#61446=CARTESIAN_POINT('Ctrl Pts',(-2.36524348105112,1.,2.90992398626211));
#61447=CARTESIAN_POINT('Ctrl Pts',(-2.36535052956938,-1.,2.90989022548032));
#61448=CARTESIAN_POINT('Ctrl Pts',(-2.36535052956938,1.,2.90989022548032));
#61449=CARTESIAN_POINT('Ctrl Pts',(-2.36578327194741,-1.,2.91025813830041));
#61450=CARTESIAN_POINT('Ctrl Pts',(-2.36578327194741,1.,2.91025813830041));
#61451=CARTESIAN_POINT('Ctrl Pts',(-2.36690501170627,-1.,2.9115863784204));
#61452=CARTESIAN_POINT('Ctrl Pts',(-2.36690501170627,1.,2.9115863784204));
#61453=CARTESIAN_POINT('Ctrl Pts',(-2.36919161373173,-1.,2.9146124988314));
#61454=CARTESIAN_POINT('Ctrl Pts',(-2.36919161373173,1.,2.9146124988314));
#61455=CARTESIAN_POINT('Ctrl Pts',(-2.37229381109821,-1.,2.91891503791411));
#61456=CARTESIAN_POINT('Ctrl Pts',(-2.37229381109821,1.,2.91891503791411));
#61457=CARTESIAN_POINT('Ctrl Pts',(-2.3760651052403,-1.,2.92430340582608));
#61458=CARTESIAN_POINT('Ctrl Pts',(-2.3760651052403,1.,2.92430340582608));
#61459=CARTESIAN_POINT('Ctrl Pts',(-2.38028989582073,-1.,2.93049643640206));
#61460=CARTESIAN_POINT('Ctrl Pts',(-2.38028989582073,1.,2.93049643640206));
#61461=CARTESIAN_POINT('Ctrl Pts',(-2.38472771516311,-1.,2.93717903280391));
#61462=CARTESIAN_POINT('Ctrl Pts',(-2.38472771516311,1.,2.93717903280391));
#61463=CARTESIAN_POINT('Ctrl Pts',(-2.38914929090759,-1.,2.94404820669076));
#61464=CARTESIAN_POINT('Ctrl Pts',(-2.38914929090759,1.,2.94404820669076));
#61465=CARTESIAN_POINT('Ctrl Pts',(-2.39337207631667,-1.,2.95085857128439));
#61466=CARTESIAN_POINT('Ctrl Pts',(-2.39337207631667,1.,2.95085857128439));
#61467=CARTESIAN_POINT('Ctrl Pts',(-2.39730553974517,-1.,2.95748006482942));
#61468=CARTESIAN_POINT('Ctrl Pts',(-2.39730553974517,1.,2.95748006482942));
#61469=CARTESIAN_POINT('Ctrl Pts',(-2.4009556571164,-1.,2.96390432240312));
#61470=CARTESIAN_POINT('Ctrl Pts',(-2.4009556571164,1.,2.96390432240312));
#61471=CARTESIAN_POINT('Ctrl Pts',(-2.40438604734919,-1.,2.9701964131236));
#61472=CARTESIAN_POINT('Ctrl Pts',(-2.40438604734919,1.,2.9701964131236));
#61473=CARTESIAN_POINT('Ctrl Pts',(-2.40768975073713,-1.,2.97646002822422));
#61474=CARTESIAN_POINT('Ctrl Pts',(-2.40768975073713,1.,2.97646002822422));
#61475=CARTESIAN_POINT('Ctrl Pts',(-2.41095909342571,-1.,2.98280015815107));
#61476=CARTESIAN_POINT('Ctrl Pts',(-2.41095909342571,1.,2.98280015815107));
#61477=CARTESIAN_POINT('Ctrl Pts',(-2.41425064199586,-1.,2.98927983005796));
#61478=CARTESIAN_POINT('Ctrl Pts',(-2.41425064199586,1.,2.98927983005796));
#61479=CARTESIAN_POINT('Ctrl Pts',(-2.41757324500514,-1.,2.99590509293503));
#61480=CARTESIAN_POINT('Ctrl Pts',(-2.41757324500514,1.,2.99590509293503));
#61481=CARTESIAN_POINT('Ctrl Pts',(-2.42090763946779,-1.,3.00264868585996));
#61482=CARTESIAN_POINT('Ctrl Pts',(-2.42090763946779,1.,3.00264868585996));
#61483=CARTESIAN_POINT('Ctrl Pts',(-2.42421849439613,-1.,3.00946442616658));
#61484=CARTESIAN_POINT('Ctrl Pts',(-2.42421849439613,1.,3.00946442616658));
#61485=CARTESIAN_POINT('Ctrl Pts',(-2.42746856264168,-1.,3.01630420830504));
#61486=CARTESIAN_POINT('Ctrl Pts',(-2.42746856264168,1.,3.01630420830504));
#61487=CARTESIAN_POINT('Ctrl Pts',(-2.43063415586637,-1.,3.02313656036004));
#61488=CARTESIAN_POINT('Ctrl Pts',(-2.43063415586637,1.,3.02313656036004));
#61489=CARTESIAN_POINT('Ctrl Pts',(-2.43371241361488,-1.,3.02995534946978));
#61490=CARTESIAN_POINT('Ctrl Pts',(-2.43371241361488,1.,3.02995534946978));
#61491=CARTESIAN_POINT('Ctrl Pts',(-2.43671278042414,-1.,3.03676949672821));
#61492=CARTESIAN_POINT('Ctrl Pts',(-2.43671278042414,1.,3.03676949672821));
#61493=CARTESIAN_POINT('Ctrl Pts',(-2.43965194061857,-1.,3.04359685040555));
#61494=CARTESIAN_POINT('Ctrl Pts',(-2.43965194061857,1.,3.04359685040555));
#61495=CARTESIAN_POINT('Ctrl Pts',(-2.44254768923105,-1.,3.05045678021504));
#61496=CARTESIAN_POINT('Ctrl Pts',(-2.44254768923105,1.,3.05045678021504));
#61497=CARTESIAN_POINT('Ctrl Pts',(-2.44541251892556,-1.,3.05736242671506));
#61498=CARTESIAN_POINT('Ctrl Pts',(-2.44541251892556,1.,3.05736242671506));
#61499=CARTESIAN_POINT('Ctrl Pts',(-2.44824970516544,-1.,3.06431596421405));
#61500=CARTESIAN_POINT('Ctrl Pts',(-2.44824970516544,1.,3.06431596421405));
#61501=CARTESIAN_POINT('Ctrl Pts',(-2.45105688854422,-1.,3.07131290521297));
#61502=CARTESIAN_POINT('Ctrl Pts',(-2.45105688854422,1.,3.07131290521297));
#61503=CARTESIAN_POINT('Ctrl Pts',(-2.4538282678779,-1.,3.07834472886139));
#61504=CARTESIAN_POINT('Ctrl Pts',(-2.4538282678779,1.,3.07834472886139));
#61505=CARTESIAN_POINT('Ctrl Pts',(-2.45655725437039,-1.,3.08540206545315));
#61506=CARTESIAN_POINT('Ctrl Pts',(-2.45655725437039,1.,3.08540206545315));
#61507=CARTESIAN_POINT('Ctrl Pts',(-2.4592391256388,-1.,3.09247787931887));
#61508=CARTESIAN_POINT('Ctrl Pts',(-2.4592391256388,1.,3.09247787931887));
#61509=CARTESIAN_POINT('Ctrl Pts',(-2.46187308501884,-1.,3.09956993697052));
#61510=CARTESIAN_POINT('Ctrl Pts',(-2.46187308501884,1.,3.09956993697052));
#61511=CARTESIAN_POINT('Ctrl Pts',(-2.46446082979646,-1.,3.1066790790198));
#61512=CARTESIAN_POINT('Ctrl Pts',(-2.46446082979646,1.,3.1066790790198));
#61513=CARTESIAN_POINT('Ctrl Pts',(-2.46700558843506,-1.,3.11380805536122));
#61514=CARTESIAN_POINT('Ctrl Pts',(-2.46700558843506,1.,3.11380805536122));
#61515=CARTESIAN_POINT('Ctrl Pts',(-2.46951098947469,-1.,3.12096015766983));
#61516=CARTESIAN_POINT('Ctrl Pts',(-2.46951098947469,1.,3.12096015766983));
#61517=CARTESIAN_POINT('Ctrl Pts',(-2.47197997765871,-1.,3.12813790805952));
#61518=CARTESIAN_POINT('Ctrl Pts',(-2.47197997765871,1.,3.12813790805952));
#61519=CARTESIAN_POINT('Ctrl Pts',(-2.47441378371932,-1.,3.13534181229295));
#61520=CARTESIAN_POINT('Ctrl Pts',(-2.47441378371932,1.,3.13534181229295));
#61521=CARTESIAN_POINT('Ctrl Pts',(-2.47681245356109,-1.,3.1425709954655));
#61522=CARTESIAN_POINT('Ctrl Pts',(-2.47681245356109,1.,3.1425709954655));
#61523=CARTESIAN_POINT('Ctrl Pts',(-2.47917529057029,-1.,3.14982373241352));
#61524=CARTESIAN_POINT('Ctrl Pts',(-2.47917529057029,1.,3.14982373241352));
#61525=CARTESIAN_POINT('Ctrl Pts',(-2.48150133566571,-1.,3.15709802322739));
#61526=CARTESIAN_POINT('Ctrl Pts',(-2.48150133566571,1.,3.15709802322739));
#61527=CARTESIAN_POINT('Ctrl Pts',(-2.48378981792725,-1.,3.16439213290161));
#61528=CARTESIAN_POINT('Ctrl Pts',(-2.48378981792725,1.,3.16439213290161));
#61529=CARTESIAN_POINT('Ctrl Pts',(-2.48604065348587,-1.,3.17170518863313));
#61530=CARTESIAN_POINT('Ctrl Pts',(-2.48604065348587,1.,3.17170518863313));
#61531=CARTESIAN_POINT('Ctrl Pts',(-2.48825428288201,-1.,3.17903698136622));
#61532=CARTESIAN_POINT('Ctrl Pts',(-2.48825428288201,1.,3.17903698136622));
#61533=CARTESIAN_POINT('Ctrl Pts',(-2.49043146334059,-1.,3.18638771282266));
#61534=CARTESIAN_POINT('Ctrl Pts',(-2.49043146334059,1.,3.18638771282266));
#61535=CARTESIAN_POINT('Ctrl Pts',(-2.49257307239848,-1.,3.19375775555798));
#61536=CARTESIAN_POINT('Ctrl Pts',(-2.49257307239848,1.,3.19375775555798));
#61537=CARTESIAN_POINT('Ctrl Pts',(-2.49467992057755,-1.,3.20114742397588));
#61538=CARTESIAN_POINT('Ctrl Pts',(-2.49467992057755,1.,3.20114742397588));
#61539=CARTESIAN_POINT('Ctrl Pts',(-2.4967525264737,-1.,3.20855669849836));
#61540=CARTESIAN_POINT('Ctrl Pts',(-2.4967525264737,1.,3.20855669849836));
#61541=CARTESIAN_POINT('Ctrl Pts',(-2.4987911459939,-1.,3.21598526261286));
#61542=CARTESIAN_POINT('Ctrl Pts',(-2.4987911459939,1.,3.21598526261286));
#61543=CARTESIAN_POINT('Ctrl Pts',(-2.50079587201957,-1.,3.22343262620503));
#61544=CARTESIAN_POINT('Ctrl Pts',(-2.50079587201957,1.,3.22343262620503));
#61545=CARTESIAN_POINT('Ctrl Pts',(-2.50276671338111,-1.,3.23089822320646));
#61546=CARTESIAN_POINT('Ctrl Pts',(-2.50276671338111,1.,3.23089822320646));
#61547=CARTESIAN_POINT('Ctrl Pts',(-2.5047036758003,-1.,3.23838151080319));
#61548=CARTESIAN_POINT('Ctrl Pts',(-2.5047036758003,1.,3.23838151080319));
#61549=CARTESIAN_POINT('Ctrl Pts',(-2.506606859405,-1.,3.24588208983849));
#61550=CARTESIAN_POINT('Ctrl Pts',(-2.506606859405,1.,3.24588208983849));
#61551=CARTESIAN_POINT('Ctrl Pts',(-2.50847647070723,-1.,3.25339971460982));
#61552=CARTESIAN_POINT('Ctrl Pts',(-2.50847647070723,1.,3.25339971460982));
#61553=CARTESIAN_POINT('Ctrl Pts',(-2.51031277813486,-1.,3.26093423001434));
#61554=CARTESIAN_POINT('Ctrl Pts',(-2.51031277813486,1.,3.26093423001434));
#61555=CARTESIAN_POINT('Ctrl Pts',(-2.51211608411423,-1.,3.26848552888115));
#61556=CARTESIAN_POINT('Ctrl Pts',(-2.51211608411423,1.,3.26848552888115));
#61557=CARTESIAN_POINT('Ctrl Pts',(-2.513886692704,-1.,3.27605350473142));
#61558=CARTESIAN_POINT('Ctrl Pts',(-2.513886692704,1.,3.27605350473142));
#61559=CARTESIAN_POINT('Ctrl Pts',(-2.51562487464514,-1.,3.28363799702982));
#61560=CARTESIAN_POINT('Ctrl Pts',(-2.51562487464514,1.,3.28363799702982));
#61561=CARTESIAN_POINT('Ctrl Pts',(-2.51733085123797,-1.,3.2912387729927));
#61562=CARTESIAN_POINT('Ctrl Pts',(-2.51733085123797,1.,3.2912387729927));
#61563=CARTESIAN_POINT('Ctrl Pts',(-2.51900480701069,-1.,3.29885556388352));
#61564=CARTESIAN_POINT('Ctrl Pts',(-2.51900480701069,1.,3.29885556388352));
#61565=CARTESIAN_POINT('Ctrl Pts',(-2.52064689568511,-1.,3.30648808815442));
#61566=CARTESIAN_POINT('Ctrl Pts',(-2.52064689568511,1.,3.30648808815442));
#61567=CARTESIAN_POINT('Ctrl Pts',(-2.52225724871313,-1.,3.31413607874645));
#61568=CARTESIAN_POINT('Ctrl Pts',(-2.52225724871313,1.,3.31413607874645));
#61569=CARTESIAN_POINT('Ctrl Pts',(-2.5238359839626,-1.,3.32179931078699));
#61570=CARTESIAN_POINT('Ctrl Pts',(-2.5238359839626,1.,3.32179931078699));
#61571=CARTESIAN_POINT('Ctrl Pts',(-2.52538321164634,-1.,3.32947762187533));
#61572=CARTESIAN_POINT('Ctrl Pts',(-2.52538321164634,1.,3.32947762187533));
#61573=CARTESIAN_POINT('Ctrl Pts',(-2.52689902690158,-1.,3.33717089999103));
#61574=CARTESIAN_POINT('Ctrl Pts',(-2.52689902690158,1.,3.33717089999103));
#61575=CARTESIAN_POINT('Ctrl Pts',(-2.52808660915689,-1.,3.34333744115511));
#61576=CARTESIAN_POINT('Ctrl Pts',(-2.52808660915689,1.,3.34333744115511));
#61577=CARTESIAN_POINT('Ctrl Pts',(-2.52896321610703,-1.,3.34796903576663));
#61578=CARTESIAN_POINT('Ctrl Pts',(-2.52896321610703,1.,3.34796903576663));
#61579=CARTESIAN_POINT('Ctrl Pts',(-2.5295413654909,-1.,3.35105973714071));
#61580=CARTESIAN_POINT('Ctrl Pts',(-2.5295413654909,1.,3.35105973714071));
#61581=CARTESIAN_POINT('Ctrl Pts',(-2.52982887637028,-1.,3.35260583073571));
#61582=CARTESIAN_POINT('Ctrl Pts',(-2.52982887637028,1.,3.35260583073571));
#61583=CARTESIAN_POINT('',(-2.36531447826073,1.,2.90994629141676));
#61584=CARTESIAN_POINT('Ctrl Pts',(-2.36531447826073,-1.,2.90994629141676));
#61585=CARTESIAN_POINT('Ctrl Pts',(-2.36531447826073,-0.666666666666667,
2.90994629141676));
#61586=CARTESIAN_POINT('Ctrl Pts',(-2.36531447826073,-0.333333333333333,
2.90994629141676));
#61587=CARTESIAN_POINT('Ctrl Pts',(-2.36531447826073,0.333333333333333,
2.90994629141676));
#61588=CARTESIAN_POINT('Ctrl Pts',(-2.36531447826073,0.666666666666667,
2.90994629141676));
#61589=CARTESIAN_POINT('Ctrl Pts',(-2.36531447826073,1.,2.90994629141676));
#61590=CARTESIAN_POINT('',(-2.52982887637028,1.,3.35260583073571));
#61591=CARTESIAN_POINT('',(-2.52982887637028,0.,3.35260583073571));
#61592=CARTESIAN_POINT('Ctrl Pts',(-2.36531447826073,1.,2.90994629141676));
#61593=CARTESIAN_POINT('Ctrl Pts',(-2.36536211188453,1.,2.90995756655606));
#61594=CARTESIAN_POINT('Ctrl Pts',(-2.36553202948613,1.,2.91005770527719));
#61595=CARTESIAN_POINT('Ctrl Pts',(-2.36599991765749,1.,2.91051690822156));
#61596=CARTESIAN_POINT('Ctrl Pts',(-2.36707658451664,1.,2.91181344022549));
#61597=CARTESIAN_POINT('Ctrl Pts',(-2.36919161373173,1.,2.9146124988314));
#61598=CARTESIAN_POINT('Ctrl Pts',(-2.37229381109821,1.,2.91891503791411));
#61599=CARTESIAN_POINT('Ctrl Pts',(-2.3760651052403,1.,2.92430340582608));
#61600=CARTESIAN_POINT('Ctrl Pts',(-2.38028989582073,1.,2.93049643640206));
#61601=CARTESIAN_POINT('Ctrl Pts',(-2.38472771516311,1.,2.93717903280391));
#61602=CARTESIAN_POINT('Ctrl Pts',(-2.38914929090759,1.,2.94404820669076));
#61603=CARTESIAN_POINT('Ctrl Pts',(-2.39337207631667,1.,2.95085857128439));
#61604=CARTESIAN_POINT('Ctrl Pts',(-2.39730553974517,1.,2.95748006482942));
#61605=CARTESIAN_POINT('Ctrl Pts',(-2.4009556571164,1.,2.96390432240312));
#61606=CARTESIAN_POINT('Ctrl Pts',(-2.40438604734919,1.,2.9701964131236));
#61607=CARTESIAN_POINT('Ctrl Pts',(-2.40768975073713,1.,2.97646002822422));
#61608=CARTESIAN_POINT('Ctrl Pts',(-2.41095909342571,1.,2.98280015815107));
#61609=CARTESIAN_POINT('Ctrl Pts',(-2.41425064199586,1.,2.98927983005796));
#61610=CARTESIAN_POINT('Ctrl Pts',(-2.41757324500514,1.,2.99590509293503));
#61611=CARTESIAN_POINT('Ctrl Pts',(-2.42090763946779,1.,3.00264868585996));
#61612=CARTESIAN_POINT('Ctrl Pts',(-2.42421849439613,1.,3.00946442616658));
#61613=CARTESIAN_POINT('Ctrl Pts',(-2.42746856264168,1.,3.01630420830504));
#61614=CARTESIAN_POINT('Ctrl Pts',(-2.43063415586637,1.,3.02313656036004));
#61615=CARTESIAN_POINT('Ctrl Pts',(-2.43371241361488,1.,3.02995534946978));
#61616=CARTESIAN_POINT('Ctrl Pts',(-2.43671278042414,1.,3.03676949672821));
#61617=CARTESIAN_POINT('Ctrl Pts',(-2.43965194061857,1.,3.04359685040555));
#61618=CARTESIAN_POINT('Ctrl Pts',(-2.44254768923105,1.,3.05045678021504));
#61619=CARTESIAN_POINT('Ctrl Pts',(-2.44541251892556,1.,3.05736242671506));
#61620=CARTESIAN_POINT('Ctrl Pts',(-2.44824970516544,1.,3.06431596421405));
#61621=CARTESIAN_POINT('Ctrl Pts',(-2.45105688854422,1.,3.07131290521297));
#61622=CARTESIAN_POINT('Ctrl Pts',(-2.4538282678779,1.,3.07834472886139));
#61623=CARTESIAN_POINT('Ctrl Pts',(-2.45655725437039,1.,3.08540206545315));
#61624=CARTESIAN_POINT('Ctrl Pts',(-2.4592391256388,1.,3.09247787931887));
#61625=CARTESIAN_POINT('Ctrl Pts',(-2.46187308501884,1.,3.09956993697052));
#61626=CARTESIAN_POINT('Ctrl Pts',(-2.46446082979646,1.,3.1066790790198));
#61627=CARTESIAN_POINT('Ctrl Pts',(-2.46700558843506,1.,3.11380805536122));
#61628=CARTESIAN_POINT('Ctrl Pts',(-2.46951098947469,1.,3.12096015766983));
#61629=CARTESIAN_POINT('Ctrl Pts',(-2.47197997765871,1.,3.12813790805952));
#61630=CARTESIAN_POINT('Ctrl Pts',(-2.47441378371932,1.,3.13534181229295));
#61631=CARTESIAN_POINT('Ctrl Pts',(-2.47681245356109,1.,3.1425709954655));
#61632=CARTESIAN_POINT('Ctrl Pts',(-2.47917529057029,1.,3.14982373241352));
#61633=CARTESIAN_POINT('Ctrl Pts',(-2.48150133566571,1.,3.15709802322739));
#61634=CARTESIAN_POINT('Ctrl Pts',(-2.48378981792725,1.,3.16439213290161));
#61635=CARTESIAN_POINT('Ctrl Pts',(-2.48604065348587,1.,3.17170518863313));
#61636=CARTESIAN_POINT('Ctrl Pts',(-2.48825428288201,1.,3.17903698136622));
#61637=CARTESIAN_POINT('Ctrl Pts',(-2.49043146334059,1.,3.18638771282266));
#61638=CARTESIAN_POINT('Ctrl Pts',(-2.49257307239848,1.,3.19375775555798));
#61639=CARTESIAN_POINT('Ctrl Pts',(-2.49467992057755,1.,3.20114742397588));
#61640=CARTESIAN_POINT('Ctrl Pts',(-2.4967525264737,1.,3.20855669849836));
#61641=CARTESIAN_POINT('Ctrl Pts',(-2.4987911459939,1.,3.21598526261286));
#61642=CARTESIAN_POINT('Ctrl Pts',(-2.50079587201957,1.,3.22343262620503));
#61643=CARTESIAN_POINT('Ctrl Pts',(-2.50276671338111,1.,3.23089822320646));
#61644=CARTESIAN_POINT('Ctrl Pts',(-2.5047036758003,1.,3.23838151080319));
#61645=CARTESIAN_POINT('Ctrl Pts',(-2.506606859405,1.,3.24588208983849));
#61646=CARTESIAN_POINT('Ctrl Pts',(-2.50847647070723,1.,3.25339971460982));
#61647=CARTESIAN_POINT('Ctrl Pts',(-2.51031277813486,1.,3.26093423001434));
#61648=CARTESIAN_POINT('Ctrl Pts',(-2.51211608411423,1.,3.26848552888115));
#61649=CARTESIAN_POINT('Ctrl Pts',(-2.513886692704,1.,3.27605350473142));
#61650=CARTESIAN_POINT('Ctrl Pts',(-2.51562487464514,1.,3.28363799702982));
#61651=CARTESIAN_POINT('Ctrl Pts',(-2.51733085123797,1.,3.2912387729927));
#61652=CARTESIAN_POINT('Ctrl Pts',(-2.51900480701069,1.,3.29885556388352));
#61653=CARTESIAN_POINT('Ctrl Pts',(-2.52064689568511,1.,3.30648808815442));
#61654=CARTESIAN_POINT('Ctrl Pts',(-2.52225724871313,1.,3.31413607874645));
#61655=CARTESIAN_POINT('Ctrl Pts',(-2.5238359839626,1.,3.32179931078699));
#61656=CARTESIAN_POINT('Ctrl Pts',(-2.52538321164634,1.,3.32947762187533));
#61657=CARTESIAN_POINT('Ctrl Pts',(-2.52689902690158,1.,3.33717089999103));
#61658=CARTESIAN_POINT('Ctrl Pts',(-2.52808660915689,1.,3.34333744115511));
#61659=CARTESIAN_POINT('Ctrl Pts',(-2.52896321610703,1.,3.34796903576663));
#61660=CARTESIAN_POINT('Ctrl Pts',(-2.5295413654909,1.,3.35105973714071));
#61661=CARTESIAN_POINT('Ctrl Pts',(-2.52982887637028,1.,3.35260583073571));
#61662=CARTESIAN_POINT('Origin',(-2.52982887637028,0.,3.35260583073571));
#61663=CARTESIAN_POINT('',(-2.40675750623143,1.,3.44202241512147));
#61664=CARTESIAN_POINT('Origin',(0.,0.,0.));
#61665=CARTESIAN_POINT('',(-2.50410331873042,1.,2.79140942341378));
#61666=CARTESIAN_POINT('Origin',(0.,1.,0.));
#61667=CARTESIAN_POINT('Ctrl Pts',(-2.50410331873042,1.,2.79140942341378));
#61668=CARTESIAN_POINT('Ctrl Pts',(-2.50410331873042,0.666666666666667,
2.79140942341378));
#61669=CARTESIAN_POINT('Ctrl Pts',(-2.50410331873043,0.333333333333333,
2.79140942341378));
#61670=CARTESIAN_POINT('Ctrl Pts',(-2.50410331873043,-0.333333333333333,
2.79140942341378));
#61671=CARTESIAN_POINT('Ctrl Pts',(-2.50410331873043,-0.666666666666667,
2.79140942341378));
#61672=CARTESIAN_POINT('Ctrl Pts',(-2.50410331873043,-1.,2.79140942341378));
#61673=CARTESIAN_POINT('Ctrl Pts',(-2.91557726271063,-1.,3.02314558451372));
#61674=CARTESIAN_POINT('Ctrl Pts',(-2.91557726271063,1.,3.02314558451372));
#61675=CARTESIAN_POINT('Ctrl Pts',(-2.91409518070707,-1.,3.02261975104912));
#61676=CARTESIAN_POINT('Ctrl Pts',(-2.91409518070707,1.,3.02261975104912));
#61677=CARTESIAN_POINT('Ctrl Pts',(-2.91113297349052,-1.,3.02156522743299));
#61678=CARTESIAN_POINT('Ctrl Pts',(-2.91113297349052,1.,3.02156522743299));
#61679=CARTESIAN_POINT('Ctrl Pts',(-2.90669553303902,-1.,3.01997487194926));
#61680=CARTESIAN_POINT('Ctrl Pts',(-2.90669553303902,1.,3.01997487194926));
#61681=CARTESIAN_POINT('Ctrl Pts',(-2.90079069102661,-1.,3.01783725123646));
#61682=CARTESIAN_POINT('Ctrl Pts',(-2.90079069102661,1.,3.01783725123646));
#61683=CARTESIAN_POINT('Ctrl Pts',(-2.8934292556764,-1.,3.01513660433291));
#61684=CARTESIAN_POINT('Ctrl Pts',(-2.8934292556764,1.,3.01513660433291));
#61685=CARTESIAN_POINT('Ctrl Pts',(-2.88608751706796,-1.,3.01240727309568));
#61686=CARTESIAN_POINT('Ctrl Pts',(-2.88608751706796,1.,3.01240727309568));
#61687=CARTESIAN_POINT('Ctrl Pts',(-2.87876560072799,-1.,3.0096491810855));
#61688=CARTESIAN_POINT('Ctrl Pts',(-2.87876560072799,1.,3.0096491810855));
#61689=CARTESIAN_POINT('Ctrl Pts',(-2.87146368430104,-1.,3.00686224485374));
#61690=CARTESIAN_POINT('Ctrl Pts',(-2.87146368430104,1.,3.00686224485374));
#61691=CARTESIAN_POINT('Ctrl Pts',(-2.86418200833065,-1.,3.00404638316245));
#61692=CARTESIAN_POINT('Ctrl Pts',(-2.86418200833065,1.,3.00404638316245));
#61693=CARTESIAN_POINT('Ctrl Pts',(-2.85692085715129,-1.,3.0012015079552));
#61694=CARTESIAN_POINT('Ctrl Pts',(-2.85692085715129,1.,3.0012015079552));
#61695=CARTESIAN_POINT('Ctrl Pts',(-2.84968053289104,-1.,2.99832751144566));
#61696=CARTESIAN_POINT('Ctrl Pts',(-2.84968053289104,1.,2.99832751144566));
#61697=CARTESIAN_POINT('Ctrl Pts',(-2.84246132984334,-1.,2.995424253416));
#61698=CARTESIAN_POINT('Ctrl Pts',(-2.84246132984334,1.,2.995424253416));
#61699=CARTESIAN_POINT('Ctrl Pts',(-2.83526351254383,-1.,2.99249155170479));
#61700=CARTESIAN_POINT('Ctrl Pts',(-2.83526351254383,1.,2.99249155170479));
#61701=CARTESIAN_POINT('Ctrl Pts',(-2.82808728190402,-1.,2.98952916401699));
#61702=CARTESIAN_POINT('Ctrl Pts',(-2.82808728190402,1.,2.98952916401699));
#61703=CARTESIAN_POINT('Ctrl Pts',(-2.82093279065704,-1.,2.98653680669434));
#61704=CARTESIAN_POINT('Ctrl Pts',(-2.82093279065704,1.,2.98653680669434));
#61705=CARTESIAN_POINT('Ctrl Pts',(-2.81380019196454,-1.,2.9835141977994));
#61706=CARTESIAN_POINT('Ctrl Pts',(-2.81380019196454,1.,2.9835141977994));
#61707=CARTESIAN_POINT('Ctrl Pts',(-2.80668968101162,-1.,2.98046109647299));
#61708=CARTESIAN_POINT('Ctrl Pts',(-2.80668968101162,1.,2.98046109647299));
#61709=CARTESIAN_POINT('Ctrl Pts',(-2.79960153278186,-1.,2.97737733718242));
#61710=CARTESIAN_POINT('Ctrl Pts',(-2.79960153278186,1.,2.97737733718242));
#61711=CARTESIAN_POINT('Ctrl Pts',(-2.79253615718147,-1.,2.97426288347475));
#61712=CARTESIAN_POINT('Ctrl Pts',(-2.79253615718147,1.,2.97426288347475));
#61713=CARTESIAN_POINT('Ctrl Pts',(-2.78549409123657,-1.,2.97111781461349));
#61714=CARTESIAN_POINT('Ctrl Pts',(-2.78549409123657,1.,2.97111781461349));
#61715=CARTESIAN_POINT('Ctrl Pts',(-2.77847589542767,-1.,2.9679422104295));
#61716=CARTESIAN_POINT('Ctrl Pts',(-2.77847589542767,1.,2.9679422104295));
#61717=CARTESIAN_POINT('Ctrl Pts',(-2.77148206836464,-1.,2.96473605585548));
#61718=CARTESIAN_POINT('Ctrl Pts',(-2.77148206836464,1.,2.96473605585548));
#61719=CARTESIAN_POINT('Ctrl Pts',(-2.76451296269571,-1.,2.96149914764832));
#61720=CARTESIAN_POINT('Ctrl Pts',(-2.76451296269571,1.,2.96149914764832));
#61721=CARTESIAN_POINT('Ctrl Pts',(-2.75756867888393,-1.,2.9582309766594));
#61722=CARTESIAN_POINT('Ctrl Pts',(-2.75756867888393,1.,2.9582309766594));
#61723=CARTESIAN_POINT('Ctrl Pts',(-2.75064903318996,-1.,2.95493069316211));
#61724=CARTESIAN_POINT('Ctrl Pts',(-2.75064903318996,1.,2.95493069316211));
#61725=CARTESIAN_POINT('Ctrl Pts',(-2.7437537949221,-1.,2.95159737214305));
#61726=CARTESIAN_POINT('Ctrl Pts',(-2.7437537949221,1.,2.95159737214305));
#61727=CARTESIAN_POINT('Ctrl Pts',(-2.73688288329825,-1.,2.94823023414381));
#61728=CARTESIAN_POINT('Ctrl Pts',(-2.73688288329825,1.,2.94823023414381));
#61729=CARTESIAN_POINT('Ctrl Pts',(-2.73003657371613,-1.,2.94482887675139));
#61730=CARTESIAN_POINT('Ctrl Pts',(-2.73003657371613,1.,2.94482887675139));
#61731=CARTESIAN_POINT('Ctrl Pts',(-2.72321571511322,-1.,2.94139351933882));
#61732=CARTESIAN_POINT('Ctrl Pts',(-2.72321571511322,1.,2.94139351933882));
#61733=CARTESIAN_POINT('Ctrl Pts',(-2.71642190053575,-1.,2.93792519474955));
#61734=CARTESIAN_POINT('Ctrl Pts',(-2.71642190053575,1.,2.93792519474955));
#61735=CARTESIAN_POINT('Ctrl Pts',(-2.70965695523776,-1.,2.93442516311168));
#61736=CARTESIAN_POINT('Ctrl Pts',(-2.70965695523776,1.,2.93442516311168));
#61737=CARTESIAN_POINT('Ctrl Pts',(-2.70292247416881,-1.,2.93089438233746));
#61738=CARTESIAN_POINT('Ctrl Pts',(-2.70292247416881,1.,2.93089438233746));
#61739=CARTESIAN_POINT('Ctrl Pts',(-2.69621932864302,-1.,2.92733294395268));
#61740=CARTESIAN_POINT('Ctrl Pts',(-2.69621932864302,1.,2.92733294395268));
#61741=CARTESIAN_POINT('Ctrl Pts',(-2.68954721165342,-1.,2.92373955325876));
#61742=CARTESIAN_POINT('Ctrl Pts',(-2.68954721165342,1.,2.92373955325876));
#61743=CARTESIAN_POINT('Ctrl Pts',(-2.68290409279689,-1.,2.92011090722152));
#61744=CARTESIAN_POINT('Ctrl Pts',(-2.68290409279689,1.,2.92011090722152));
#61745=CARTESIAN_POINT('Ctrl Pts',(-2.67628728855309,-1.,2.91644290704281));
#61746=CARTESIAN_POINT('Ctrl Pts',(-2.67628728855309,1.,2.91644290704281));
#61747=CARTESIAN_POINT('Ctrl Pts',(-2.66969458792627,-1.,2.91273193382876));
#61748=CARTESIAN_POINT('Ctrl Pts',(-2.66969458792627,1.,2.91273193382876));
#61749=CARTESIAN_POINT('Ctrl Pts',(-2.66312542616809,-1.,2.90897617968921));
#61750=CARTESIAN_POINT('Ctrl Pts',(-2.66312542616809,1.,2.90897617968921));
#61751=CARTESIAN_POINT('Ctrl Pts',(-2.65658188464287,-1.,2.90517678087467));
#61752=CARTESIAN_POINT('Ctrl Pts',(-2.65658188464287,1.,2.90517678087467));
#61753=CARTESIAN_POINT('Ctrl Pts',(-2.65007017365576,-1.,2.90133950224879));
#61754=CARTESIAN_POINT('Ctrl Pts',(-2.65007017365576,1.,2.90133950224879));
#61755=CARTESIAN_POINT('Ctrl Pts',(-2.64359851684146,-1.,2.89747231723361));
#61756=CARTESIAN_POINT('Ctrl Pts',(-2.64359851684146,1.,2.89747231723361));
#61757=CARTESIAN_POINT('Ctrl Pts',(-2.63717442263944,-1.,2.89358228854557));
#61758=CARTESIAN_POINT('Ctrl Pts',(-2.63717442263944,1.,2.89358228854557));
#61759=CARTESIAN_POINT('Ctrl Pts',(-2.63080195420771,-1.,2.88967244854243));
#61760=CARTESIAN_POINT('Ctrl Pts',(-2.63080195420771,1.,2.88967244854243));
#61761=CARTESIAN_POINT('Ctrl Pts',(-2.62447947640253,-1.,2.88573922195049));
#61762=CARTESIAN_POINT('Ctrl Pts',(-2.62447947640253,1.,2.88573922195049));
#61763=CARTESIAN_POINT('Ctrl Pts',(-2.61819596473087,-1.,2.88176821427502));
#61764=CARTESIAN_POINT('Ctrl Pts',(-2.61819596473087,1.,2.88176821427502));
#61765=CARTESIAN_POINT('Ctrl Pts',(-2.61193507170928,-1.,2.87773881947885));
#61766=CARTESIAN_POINT('Ctrl Pts',(-2.61193507170928,1.,2.87773881947885));
#61767=CARTESIAN_POINT('Ctrl Pts',(-2.6056817788128,-1.,2.87363176656475));
#61768=CARTESIAN_POINT('Ctrl Pts',(-2.6056817788128,1.,2.87363176656475));
#61769=CARTESIAN_POINT('Ctrl Pts',(-2.59942875223202,-1.,2.86943633170712));
#61770=CARTESIAN_POINT('Ctrl Pts',(-2.59942875223202,1.,2.86943633170712));
#61771=CARTESIAN_POINT('Ctrl Pts',(-2.59318160184921,-1.,2.86515629953528));
#61772=CARTESIAN_POINT('Ctrl Pts',(-2.59318160184921,1.,2.86515629953528));
#61773=CARTESIAN_POINT('Ctrl Pts',(-2.5869677064356,-1.,2.86081999003668));
#61774=CARTESIAN_POINT('Ctrl Pts',(-2.5869677064356,1.,2.86081999003668));
#61775=CARTESIAN_POINT('Ctrl Pts',(-2.58082875254407,-1.,2.85647171715147));
#61776=CARTESIAN_POINT('Ctrl Pts',(-2.58082875254407,1.,2.85647171715147));
#61777=CARTESIAN_POINT('Ctrl Pts',(-2.57480482727128,-1.,2.85215360144483));
#61778=CARTESIAN_POINT('Ctrl Pts',(-2.57480482727128,1.,2.85215360144483));
#61779=CARTESIAN_POINT('Ctrl Pts',(-2.56891984251743,-1.,2.84788893329091));
#61780=CARTESIAN_POINT('Ctrl Pts',(-2.56891984251743,1.,2.84788893329091));
#61781=CARTESIAN_POINT('Ctrl Pts',(-2.56316920798489,-1.,2.84366802680211));
#61782=CARTESIAN_POINT('Ctrl Pts',(-2.56316920798489,1.,2.84366802680211));
#61783=CARTESIAN_POINT('Ctrl Pts',(-2.55749952145165,-1.,2.83942515220699));
#61784=CARTESIAN_POINT('Ctrl Pts',(-2.55749952145165,1.,2.83942515220699));
#61785=CARTESIAN_POINT('Ctrl Pts',(-2.55182152806964,-1.,2.83505269592412));
#61786=CARTESIAN_POINT('Ctrl Pts',(-2.55182152806964,1.,2.83505269592412));
#61787=CARTESIAN_POINT('Ctrl Pts',(-2.54604736792542,-1.,2.83044254225794));
#61788=CARTESIAN_POINT('Ctrl Pts',(-2.54604736792542,1.,2.83044254225794));
#61789=CARTESIAN_POINT('Ctrl Pts',(-2.54012272520141,-1.,2.82552167649157));
#61790=CARTESIAN_POINT('Ctrl Pts',(-2.54012272520141,1.,2.82552167649157));
#61791=CARTESIAN_POINT('Ctrl Pts',(-2.53405679667463,-1.,2.82028550483744));
#61792=CARTESIAN_POINT('Ctrl Pts',(-2.53405679667463,1.,2.82028550483744));
#61793=CARTESIAN_POINT('Ctrl Pts',(-2.52796388055457,-1.,2.8148437904867));
#61794=CARTESIAN_POINT('Ctrl Pts',(-2.52796388055457,1.,2.8148437904867));
#61795=CARTESIAN_POINT('Ctrl Pts',(-2.52205778589922,-1.,2.80941521967234));
#61796=CARTESIAN_POINT('Ctrl Pts',(-2.52205778589922,1.,2.80941521967234));
#61797=CARTESIAN_POINT('Ctrl Pts',(-2.51660190466067,-1.,2.80427363984939));
#61798=CARTESIAN_POINT('Ctrl Pts',(-2.51660190466067,1.,2.80427363984939));
#61799=CARTESIAN_POINT('Ctrl Pts',(-2.51186983687947,-1.,2.79970585014308));
#61800=CARTESIAN_POINT('Ctrl Pts',(-2.51186983687947,1.,2.79970585014308));
#61801=CARTESIAN_POINT('Ctrl Pts',(-2.50810555977564,-1.,2.7959687805717));
#61802=CARTESIAN_POINT('Ctrl Pts',(-2.50810555977564,1.,2.7959687805717));
#61803=CARTESIAN_POINT('Ctrl Pts',(-2.50547439929077,-1.,2.79323694088143));
#61804=CARTESIAN_POINT('Ctrl Pts',(-2.50547439929077,1.,2.79323694088143));
#61805=CARTESIAN_POINT('Ctrl Pts',(-2.50433799076945,-1.,2.79192122906739));
#61806=CARTESIAN_POINT('Ctrl Pts',(-2.50433799076945,1.,2.79192122906739));
#61807=CARTESIAN_POINT('Ctrl Pts',(-2.50404230339032,-1.,2.79143626022225));
#61808=CARTESIAN_POINT('Ctrl Pts',(-2.50404230339032,1.,2.79143626022225));
#61809=CARTESIAN_POINT('Ctrl Pts',(-2.50409239460011,-1.,2.79133581100044));
#61810=CARTESIAN_POINT('Ctrl Pts',(-2.50409239460011,1.,2.79133581100044));
#61811=CARTESIAN_POINT('Ctrl Pts',(-2.50417924854921,-1.,2.79134130681569));
#61812=CARTESIAN_POINT('Ctrl Pts',(-2.50417924854921,1.,2.79134130681569));
#61813=CARTESIAN_POINT('',(-2.91557726271063,1.,3.02314558451372));
#61814=CARTESIAN_POINT('Ctrl Pts',(-2.91557726271063,1.,3.02314558451372));
#61815=CARTESIAN_POINT('Ctrl Pts',(-2.91409518070707,1.,3.02261975104912));
#61816=CARTESIAN_POINT('Ctrl Pts',(-2.91113297349052,1.,3.02156522743299));
#61817=CARTESIAN_POINT('Ctrl Pts',(-2.90669553303902,1.,3.01997487194926));
#61818=CARTESIAN_POINT('Ctrl Pts',(-2.90079069102661,1.,3.01783725123646));
#61819=CARTESIAN_POINT('Ctrl Pts',(-2.8934292556764,1.,3.01513660433291));
#61820=CARTESIAN_POINT('Ctrl Pts',(-2.88608751706796,1.,3.01240727309568));
#61821=CARTESIAN_POINT('Ctrl Pts',(-2.87876560072799,1.,3.0096491810855));
#61822=CARTESIAN_POINT('Ctrl Pts',(-2.87146368430104,1.,3.00686224485374));
#61823=CARTESIAN_POINT('Ctrl Pts',(-2.86418200833065,1.,3.00404638316245));
#61824=CARTESIAN_POINT('Ctrl Pts',(-2.85692085715129,1.,3.0012015079552));
#61825=CARTESIAN_POINT('Ctrl Pts',(-2.84968053289104,1.,2.99832751144566));
#61826=CARTESIAN_POINT('Ctrl Pts',(-2.84246132984334,1.,2.995424253416));
#61827=CARTESIAN_POINT('Ctrl Pts',(-2.83526351254383,1.,2.99249155170479));
#61828=CARTESIAN_POINT('Ctrl Pts',(-2.82808728190402,1.,2.98952916401699));
#61829=CARTESIAN_POINT('Ctrl Pts',(-2.82093279065704,1.,2.98653680669434));
#61830=CARTESIAN_POINT('Ctrl Pts',(-2.81380019196454,1.,2.9835141977994));
#61831=CARTESIAN_POINT('Ctrl Pts',(-2.80668968101162,1.,2.98046109647299));
#61832=CARTESIAN_POINT('Ctrl Pts',(-2.79960153278186,1.,2.97737733718242));
#61833=CARTESIAN_POINT('Ctrl Pts',(-2.79253615718147,1.,2.97426288347475));
#61834=CARTESIAN_POINT('Ctrl Pts',(-2.78549409123657,1.,2.97111781461349));
#61835=CARTESIAN_POINT('Ctrl Pts',(-2.77847589542767,1.,2.9679422104295));
#61836=CARTESIAN_POINT('Ctrl Pts',(-2.77148206836464,1.,2.96473605585548));
#61837=CARTESIAN_POINT('Ctrl Pts',(-2.76451296269571,1.,2.96149914764832));
#61838=CARTESIAN_POINT('Ctrl Pts',(-2.75756867888393,1.,2.9582309766594));
#61839=CARTESIAN_POINT('Ctrl Pts',(-2.75064903318996,1.,2.95493069316211));
#61840=CARTESIAN_POINT('Ctrl Pts',(-2.7437537949221,1.,2.95159737214305));
#61841=CARTESIAN_POINT('Ctrl Pts',(-2.73688288329825,1.,2.94823023414381));
#61842=CARTESIAN_POINT('Ctrl Pts',(-2.73003657371613,1.,2.94482887675139));
#61843=CARTESIAN_POINT('Ctrl Pts',(-2.72321571511322,1.,2.94139351933882));
#61844=CARTESIAN_POINT('Ctrl Pts',(-2.71642190053575,1.,2.93792519474955));
#61845=CARTESIAN_POINT('Ctrl Pts',(-2.70965695523776,1.,2.93442516311168));
#61846=CARTESIAN_POINT('Ctrl Pts',(-2.70292247416881,1.,2.93089438233746));
#61847=CARTESIAN_POINT('Ctrl Pts',(-2.69621932864302,1.,2.92733294395268));
#61848=CARTESIAN_POINT('Ctrl Pts',(-2.68954721165342,1.,2.92373955325876));
#61849=CARTESIAN_POINT('Ctrl Pts',(-2.68290409279689,1.,2.92011090722152));
#61850=CARTESIAN_POINT('Ctrl Pts',(-2.67628728855309,1.,2.91644290704281));
#61851=CARTESIAN_POINT('Ctrl Pts',(-2.66969458792627,1.,2.91273193382876));
#61852=CARTESIAN_POINT('Ctrl Pts',(-2.66312542616809,1.,2.90897617968921));
#61853=CARTESIAN_POINT('Ctrl Pts',(-2.65658188464287,1.,2.90517678087467));
#61854=CARTESIAN_POINT('Ctrl Pts',(-2.65007017365576,1.,2.90133950224879));
#61855=CARTESIAN_POINT('Ctrl Pts',(-2.64359851684146,1.,2.89747231723361));
#61856=CARTESIAN_POINT('Ctrl Pts',(-2.63717442263944,1.,2.89358228854557));
#61857=CARTESIAN_POINT('Ctrl Pts',(-2.63080195420771,1.,2.88967244854243));
#61858=CARTESIAN_POINT('Ctrl Pts',(-2.62447947640253,1.,2.88573922195049));
#61859=CARTESIAN_POINT('Ctrl Pts',(-2.61819596473087,1.,2.88176821427502));
#61860=CARTESIAN_POINT('Ctrl Pts',(-2.61193507170928,1.,2.87773881947885));
#61861=CARTESIAN_POINT('Ctrl Pts',(-2.6056817788128,1.,2.87363176656475));
#61862=CARTESIAN_POINT('Ctrl Pts',(-2.59942875223202,1.,2.86943633170712));
#61863=CARTESIAN_POINT('Ctrl Pts',(-2.59318160184921,1.,2.86515629953528));
#61864=CARTESIAN_POINT('Ctrl Pts',(-2.5869677064356,1.,2.86081999003668));
#61865=CARTESIAN_POINT('Ctrl Pts',(-2.58082875254407,1.,2.85647171715147));
#61866=CARTESIAN_POINT('Ctrl Pts',(-2.57480482727128,1.,2.85215360144483));
#61867=CARTESIAN_POINT('Ctrl Pts',(-2.56891984251743,1.,2.84788893329091));
#61868=CARTESIAN_POINT('Ctrl Pts',(-2.56316920798489,1.,2.84366802680211));
#61869=CARTESIAN_POINT('Ctrl Pts',(-2.55749952145165,1.,2.83942515220699));
#61870=CARTESIAN_POINT('Ctrl Pts',(-2.55182152806964,1.,2.83505269592412));
#61871=CARTESIAN_POINT('Ctrl Pts',(-2.54604736792542,1.,2.83044254225794));
#61872=CARTESIAN_POINT('Ctrl Pts',(-2.54012272520141,1.,2.82552167649157));
#61873=CARTESIAN_POINT('Ctrl Pts',(-2.53405679667463,1.,2.82028550483744));
#61874=CARTESIAN_POINT('Ctrl Pts',(-2.52796388055457,1.,2.8148437904867));
#61875=CARTESIAN_POINT('Ctrl Pts',(-2.52205778589922,1.,2.80941521967234));
#61876=CARTESIAN_POINT('Ctrl Pts',(-2.51660190466067,1.,2.80427363984939));
#61877=CARTESIAN_POINT('Ctrl Pts',(-2.51186983687947,1.,2.79970585014308));
#61878=CARTESIAN_POINT('Ctrl Pts',(-2.50810555977564,1.,2.7959687805717));
#61879=CARTESIAN_POINT('Ctrl Pts',(-2.50567182569153,1.,2.79344192164204));
#61880=CARTESIAN_POINT('Ctrl Pts',(-2.50455968395235,1.,2.79217568804874));
#61881=CARTESIAN_POINT('Ctrl Pts',(-2.50417932839343,1.,2.79164172519039));
#61882=CARTESIAN_POINT('Ctrl Pts',(-2.50410700351427,1.,2.79145823440899));
#61883=CARTESIAN_POINT('Ctrl Pts',(-2.50410331873043,1.,2.79140942341378));
#61884=CARTESIAN_POINT('',(-2.91557726271063,0.,3.02314558451372));
#61885=CARTESIAN_POINT('Ctrl Pts',(-2.79134130681569,-1.,2.50417924854921));
#61886=CARTESIAN_POINT('Ctrl Pts',(-2.79134130681569,1.,2.50417924854921));
#61887=CARTESIAN_POINT('Ctrl Pts',(-2.7913358110015,-1.,2.50409239460108));
#61888=CARTESIAN_POINT('Ctrl Pts',(-2.7913358110015,1.,2.50409239460108));
#61889=CARTESIAN_POINT('Ctrl Pts',(-2.79143626022503,-1.,2.50404230339286));
#61890=CARTESIAN_POINT('Ctrl Pts',(-2.79143626022503,1.,2.50404230339286));
#61891=CARTESIAN_POINT('Ctrl Pts',(-2.79192122907148,-1.,2.5043379907732));
#61892=CARTESIAN_POINT('Ctrl Pts',(-2.79192122907148,1.,2.5043379907732));
#61893=CARTESIAN_POINT('Ctrl Pts',(-2.7932369408851,-1.,2.50547439929414));
#61894=CARTESIAN_POINT('Ctrl Pts',(-2.7932369408851,1.,2.50547439929414));
#61895=CARTESIAN_POINT('Ctrl Pts',(-2.79596878057287,-1.,2.50810555977671));
#61896=CARTESIAN_POINT('Ctrl Pts',(-2.79596878057287,1.,2.50810555977671));
#61897=CARTESIAN_POINT('Ctrl Pts',(-2.79970585014168,-1.,2.51186983687818));
#61898=CARTESIAN_POINT('Ctrl Pts',(-2.79970585014168,1.,2.51186983687818));
#61899=CARTESIAN_POINT('Ctrl Pts',(-2.80427363984653,-1.,2.51660190465805));
#61900=CARTESIAN_POINT('Ctrl Pts',(-2.80427363984653,1.,2.51660190465805));
#61901=CARTESIAN_POINT('Ctrl Pts',(-2.80941521966941,-1.,2.52205778589653));
#61902=CARTESIAN_POINT('Ctrl Pts',(-2.80941521966941,1.,2.52205778589653));
#61903=CARTESIAN_POINT('Ctrl Pts',(-2.81484379048475,-1.,2.52796388055278));
#61904=CARTESIAN_POINT('Ctrl Pts',(-2.81484379048475,1.,2.52796388055278));
#61905=CARTESIAN_POINT('Ctrl Pts',(-2.82028550483689,-1.,2.53405679667412));
#61906=CARTESIAN_POINT('Ctrl Pts',(-2.82028550483689,1.,2.53405679667412));
#61907=CARTESIAN_POINT('Ctrl Pts',(-2.8255216764922,-1.,2.54012272520199));
#61908=CARTESIAN_POINT('Ctrl Pts',(-2.8255216764922,1.,2.54012272520199));
#61909=CARTESIAN_POINT('Ctrl Pts',(-2.83044254225917,-1.,2.54604736792655));
#61910=CARTESIAN_POINT('Ctrl Pts',(-2.83044254225917,1.,2.54604736792655));
#61911=CARTESIAN_POINT('Ctrl Pts',(-2.83505269592536,-1.,2.55182152807077));
#61912=CARTESIAN_POINT('Ctrl Pts',(-2.83505269592536,1.,2.55182152807077));
#61913=CARTESIAN_POINT('Ctrl Pts',(-2.83942515220782,-1.,2.55749952145241));
#61914=CARTESIAN_POINT('Ctrl Pts',(-2.83942515220782,1.,2.55749952145241));
#61915=CARTESIAN_POINT('Ctrl Pts',(-2.84366802680237,-1.,2.56316920798513));
#61916=CARTESIAN_POINT('Ctrl Pts',(-2.84366802680237,1.,2.56316920798513));
#61917=CARTESIAN_POINT('Ctrl Pts',(-2.84788893329067,-1.,2.56891984251721));
#61918=CARTESIAN_POINT('Ctrl Pts',(-2.84788893329067,1.,2.56891984251721));
#61919=CARTESIAN_POINT('Ctrl Pts',(-2.85215360144431,-1.,2.57480482727081));
#61920=CARTESIAN_POINT('Ctrl Pts',(-2.85215360144431,1.,2.57480482727081));
#61921=CARTESIAN_POINT('Ctrl Pts',(-2.85647171715092,-1.,2.58082875254357));
#61922=CARTESIAN_POINT('Ctrl Pts',(-2.85647171715092,1.,2.58082875254357));
#61923=CARTESIAN_POINT('Ctrl Pts',(-2.86081999003629,-1.,2.58696770643524));
#61924=CARTESIAN_POINT('Ctrl Pts',(-2.86081999003629,1.,2.58696770643524));
#61925=CARTESIAN_POINT('Ctrl Pts',(-2.86515629953513,-1.,2.59318160184908));
#61926=CARTESIAN_POINT('Ctrl Pts',(-2.86515629953513,1.,2.59318160184908));
#61927=CARTESIAN_POINT('Ctrl Pts',(-2.86943633170722,-1.,2.5994287522321));
#61928=CARTESIAN_POINT('Ctrl Pts',(-2.86943633170722,1.,2.5994287522321));
#61929=CARTESIAN_POINT('Ctrl Pts',(-2.87363176656501,-1.,2.60568177881303));
#61930=CARTESIAN_POINT('Ctrl Pts',(-2.87363176656501,1.,2.60568177881303));
#61931=CARTESIAN_POINT('Ctrl Pts',(-2.87773881947916,-1.,2.61193507170955));
#61932=CARTESIAN_POINT('Ctrl Pts',(-2.87773881947916,1.,2.61193507170955));
#61933=CARTESIAN_POINT('Ctrl Pts',(-2.88176821427525,-1.,2.61819596473108));
#61934=CARTESIAN_POINT('Ctrl Pts',(-2.88176821427525,1.,2.61819596473108));
#61935=CARTESIAN_POINT('Ctrl Pts',(-2.88573922195059,-1.,2.62447947640262));
#61936=CARTESIAN_POINT('Ctrl Pts',(-2.88573922195059,1.,2.62447947640262));
#61937=CARTESIAN_POINT('Ctrl Pts',(-2.88967244854239,-1.,2.63080195420767));
#61938=CARTESIAN_POINT('Ctrl Pts',(-2.88967244854239,1.,2.63080195420767));
#61939=CARTESIAN_POINT('Ctrl Pts',(-2.89358228854544,-1.,2.63717442263932));
#61940=CARTESIAN_POINT('Ctrl Pts',(-2.89358228854544,1.,2.63717442263932));
#61941=CARTESIAN_POINT('Ctrl Pts',(-2.89747231723345,-1.,2.64359851684131));
#61942=CARTESIAN_POINT('Ctrl Pts',(-2.89747231723345,1.,2.64359851684131));
#61943=CARTESIAN_POINT('Ctrl Pts',(-2.90133950224867,-1.,2.65007017365564));
#61944=CARTESIAN_POINT('Ctrl Pts',(-2.90133950224867,1.,2.65007017365564));
#61945=CARTESIAN_POINT('Ctrl Pts',(-2.90517678087461,-1.,2.65658188464282));
#61946=CARTESIAN_POINT('Ctrl Pts',(-2.90517678087461,1.,2.65658188464282));
#61947=CARTESIAN_POINT('Ctrl Pts',(-2.90897617968923,-1.,2.6631254261681));
#61948=CARTESIAN_POINT('Ctrl Pts',(-2.90897617968923,1.,2.6631254261681));
#61949=CARTESIAN_POINT('Ctrl Pts',(-2.91273193382882,-1.,2.66969458792631));
#61950=CARTESIAN_POINT('Ctrl Pts',(-2.91273193382882,1.,2.66969458792631));
#61951=CARTESIAN_POINT('Ctrl Pts',(-2.91644290704285,-1.,2.67628728855312));
#61952=CARTESIAN_POINT('Ctrl Pts',(-2.91644290704285,1.,2.67628728855312));
#61953=CARTESIAN_POINT('Ctrl Pts',(-2.92011090722152,-1.,2.68290409279688));
#61954=CARTESIAN_POINT('Ctrl Pts',(-2.92011090722152,1.,2.68290409279688));
#61955=CARTESIAN_POINT('Ctrl Pts',(-2.92373955325875,-1.,2.68954721165339));
#61956=CARTESIAN_POINT('Ctrl Pts',(-2.92373955325875,1.,2.68954721165339));
#61957=CARTESIAN_POINT('Ctrl Pts',(-2.92733294395267,-1.,2.69621932864301));
#61958=CARTESIAN_POINT('Ctrl Pts',(-2.92733294395267,1.,2.69621932864301));
#61959=CARTESIAN_POINT('Ctrl Pts',(-2.9308943823375,-1.,2.70292247416885));
#61960=CARTESIAN_POINT('Ctrl Pts',(-2.9308943823375,1.,2.70292247416885));
#61961=CARTESIAN_POINT('Ctrl Pts',(-2.93442516311179,-1.,2.70965695523787));
#61962=CARTESIAN_POINT('Ctrl Pts',(-2.93442516311179,1.,2.70965695523787));
#61963=CARTESIAN_POINT('Ctrl Pts',(-2.93792519474972,-1.,2.71642190053592));
#61964=CARTESIAN_POINT('Ctrl Pts',(-2.93792519474972,1.,2.71642190053592));
#61965=CARTESIAN_POINT('Ctrl Pts',(-2.94139351933897,-1.,2.72321571511337));
#61966=CARTESIAN_POINT('Ctrl Pts',(-2.94139351933897,1.,2.72321571511337));
#61967=CARTESIAN_POINT('Ctrl Pts',(-2.94482887675143,-1.,2.73003657371617));
#61968=CARTESIAN_POINT('Ctrl Pts',(-2.94482887675143,1.,2.73003657371617));
#61969=CARTESIAN_POINT('Ctrl Pts',(-2.94823023414364,-1.,2.73688288329808));
#61970=CARTESIAN_POINT('Ctrl Pts',(-2.94823023414364,1.,2.73688288329808));
#61971=CARTESIAN_POINT('Ctrl Pts',(-2.95159737214266,-1.,2.74375379492172));
#61972=CARTESIAN_POINT('Ctrl Pts',(-2.95159737214266,1.,2.74375379492172));
#61973=CARTESIAN_POINT('Ctrl Pts',(-2.95493069316161,-1.,2.75064903318947));
#61974=CARTESIAN_POINT('Ctrl Pts',(-2.95493069316161,1.,2.75064903318947));
#61975=CARTESIAN_POINT('Ctrl Pts',(-2.95823097665896,-1.,2.7575686788835));
#61976=CARTESIAN_POINT('Ctrl Pts',(-2.95823097665896,1.,2.7575686788835));
#61977=CARTESIAN_POINT('Ctrl Pts',(-2.96149914764818,-1.,2.76451296269557));
#61978=CARTESIAN_POINT('Ctrl Pts',(-2.96149914764818,1.,2.76451296269557));
#61979=CARTESIAN_POINT('Ctrl Pts',(-2.96473605585583,-1.,2.77148206836498));
#61980=CARTESIAN_POINT('Ctrl Pts',(-2.96473605585583,1.,2.77148206836498));
#61981=CARTESIAN_POINT('Ctrl Pts',(-2.96794221043036,-1.,2.7784758954285));
#61982=CARTESIAN_POINT('Ctrl Pts',(-2.96794221043036,1.,2.7784758954285));
#61983=CARTESIAN_POINT('Ctrl Pts',(-2.97111781461465,-1.,2.78549409123769));
#61984=CARTESIAN_POINT('Ctrl Pts',(-2.97111781461465,1.,2.78549409123769));
#61985=CARTESIAN_POINT('Ctrl Pts',(-2.9742628834758,-1.,2.79253615718248));
#61986=CARTESIAN_POINT('Ctrl Pts',(-2.9742628834758,1.,2.79253615718248));
#61987=CARTESIAN_POINT('Ctrl Pts',(-2.97737733718287,-1.,2.7996015327823));
#61988=CARTESIAN_POINT('Ctrl Pts',(-2.97737733718287,1.,2.7996015327823));
#61989=CARTESIAN_POINT('Ctrl Pts',(-2.98046109647241,-1.,2.80668968101106));
#61990=CARTESIAN_POINT('Ctrl Pts',(-2.98046109647241,1.,2.80668968101106));
#61991=CARTESIAN_POINT('Ctrl Pts',(-2.98351419779767,-1.,2.81380019196286));
#61992=CARTESIAN_POINT('Ctrl Pts',(-2.98351419779767,1.,2.81380019196286));
#61993=CARTESIAN_POINT('Ctrl Pts',(-2.9865368066918,-1.,2.82093279065457));
#61994=CARTESIAN_POINT('Ctrl Pts',(-2.9865368066918,1.,2.82093279065457));
#61995=CARTESIAN_POINT('Ctrl Pts',(-2.98952916401446,-1.,2.82808728190157));
#61996=CARTESIAN_POINT('Ctrl Pts',(-2.98952916401446,1.,2.82808728190157));
#61997=CARTESIAN_POINT('Ctrl Pts',(-2.9924915517034,-1.,2.83526351254248));
#61998=CARTESIAN_POINT('Ctrl Pts',(-2.9924915517034,1.,2.83526351254248));
#61999=CARTESIAN_POINT('Ctrl Pts',(-2.99542425341685,-1.,2.84246132984415));
#62000=CARTESIAN_POINT('Ctrl Pts',(-2.99542425341685,1.,2.84246132984415));
#62001=CARTESIAN_POINT('Ctrl Pts',(-2.99832751144925,-1.,2.84968053289451));
#62002=CARTESIAN_POINT('Ctrl Pts',(-2.99832751144925,1.,2.84968053289451));
#62003=CARTESIAN_POINT('Ctrl Pts',(-3.00120150796095,-1.,2.85692085715686));
#62004=CARTESIAN_POINT('Ctrl Pts',(-3.00120150796095,1.,2.85692085715686));
#62005=CARTESIAN_POINT('Ctrl Pts',(-3.00404638316867,-1.,2.86418200833667));
#62006=CARTESIAN_POINT('Ctrl Pts',(-3.00404638316867,1.,2.86418200833667));
#62007=CARTESIAN_POINT('Ctrl Pts',(-3.00686224485784,-1.,2.87146368430502));
#62008=CARTESIAN_POINT('Ctrl Pts',(-3.00686224485784,1.,2.87146368430502));
#62009=CARTESIAN_POINT('Ctrl Pts',(-3.00964918108476,-1.,2.87876560072727));
#62010=CARTESIAN_POINT('Ctrl Pts',(-3.00964918108476,1.,2.87876560072727));
#62011=CARTESIAN_POINT('Ctrl Pts',(-3.01240727308829,-1.,2.8860875170608));
#62012=CARTESIAN_POINT('Ctrl Pts',(-3.01240727308829,1.,2.8860875170608));
#62013=CARTESIAN_POINT('Ctrl Pts',(-3.01513660431928,-1.,2.89342925566321));
#62014=CARTESIAN_POINT('Ctrl Pts',(-3.01513660431928,1.,2.89342925566321));
#62015=CARTESIAN_POINT('Ctrl Pts',(-3.01783725121981,-1.,2.9007906910105));
#62016=CARTESIAN_POINT('Ctrl Pts',(-3.01783725121981,1.,2.9007906910105));
#62017=CARTESIAN_POINT('Ctrl Pts',(-3.01997487193503,-1.,2.90669553302526));
#62018=CARTESIAN_POINT('Ctrl Pts',(-3.01997487193503,1.,2.90669553302526));
#62019=CARTESIAN_POINT('Ctrl Pts',(-3.02156522742431,-1.,2.91113297348212));
#62020=CARTESIAN_POINT('Ctrl Pts',(-3.02156522742431,1.,2.91113297348212));
#62021=CARTESIAN_POINT('Ctrl Pts',(-3.02261975104593,-1.,2.91409518070399));
#62022=CARTESIAN_POINT('Ctrl Pts',(-3.02261975104593,1.,2.91409518070399));
#62023=CARTESIAN_POINT('Ctrl Pts',(-3.02314558451372,-1.,2.91557726271063));
#62024=CARTESIAN_POINT('Ctrl Pts',(-3.02314558451372,1.,2.91557726271063));
#62025=CARTESIAN_POINT('',(-2.79140942341258,1.,2.50410331873176));
#62026=CARTESIAN_POINT('Ctrl Pts',(-2.79140942341258,-1.,2.50410331873176));
#62027=CARTESIAN_POINT('Ctrl Pts',(-2.79140942341258,-0.666666666666667,
2.50410331873176));
#62028=CARTESIAN_POINT('Ctrl Pts',(-2.79140942341258,-0.333333333333333,
2.50410331873176));
#62029=CARTESIAN_POINT('Ctrl Pts',(-2.79140942341258,0.333333333333333,
2.50410331873176));
#62030=CARTESIAN_POINT('Ctrl Pts',(-2.79140942341258,0.666666666666667,
2.50410331873176));
#62031=CARTESIAN_POINT('Ctrl Pts',(-2.79140942341258,1.,2.50410331873176));
#62032=CARTESIAN_POINT('',(-3.02314558451372,1.,2.91557726271063));
#62033=CARTESIAN_POINT('',(-3.02314558451372,0.,2.91557726271063));
#62034=CARTESIAN_POINT('Ctrl Pts',(-2.79140942341258,1.,2.50410331873176));
#62035=CARTESIAN_POINT('Ctrl Pts',(-2.79145823440781,1.,2.50410700351493));
#62036=CARTESIAN_POINT('Ctrl Pts',(-2.79164172518905,1.,2.50417932839313));
#62037=CARTESIAN_POINT('Ctrl Pts',(-2.79217568804755,1.,2.50455968395146));
#62038=CARTESIAN_POINT('Ctrl Pts',(-2.79344192164147,1.,2.50567182569081));
#62039=CARTESIAN_POINT('Ctrl Pts',(-2.79596878057287,1.,2.50810555977671));
#62040=CARTESIAN_POINT('Ctrl Pts',(-2.79970585014168,1.,2.51186983687818));
#62041=CARTESIAN_POINT('Ctrl Pts',(-2.80427363984653,1.,2.51660190465805));
#62042=CARTESIAN_POINT('Ctrl Pts',(-2.80941521966941,1.,2.52205778589653));
#62043=CARTESIAN_POINT('Ctrl Pts',(-2.81484379048475,1.,2.52796388055278));
#62044=CARTESIAN_POINT('Ctrl Pts',(-2.82028550483689,1.,2.53405679667412));
#62045=CARTESIAN_POINT('Ctrl Pts',(-2.8255216764922,1.,2.54012272520199));
#62046=CARTESIAN_POINT('Ctrl Pts',(-2.83044254225917,1.,2.54604736792655));
#62047=CARTESIAN_POINT('Ctrl Pts',(-2.83505269592536,1.,2.55182152807077));
#62048=CARTESIAN_POINT('Ctrl Pts',(-2.83942515220782,1.,2.55749952145241));
#62049=CARTESIAN_POINT('Ctrl Pts',(-2.84366802680237,1.,2.56316920798513));
#62050=CARTESIAN_POINT('Ctrl Pts',(-2.84788893329067,1.,2.56891984251721));
#62051=CARTESIAN_POINT('Ctrl Pts',(-2.85215360144431,1.,2.57480482727081));
#62052=CARTESIAN_POINT('Ctrl Pts',(-2.85647171715092,1.,2.58082875254357));
#62053=CARTESIAN_POINT('Ctrl Pts',(-2.86081999003629,1.,2.58696770643524));
#62054=CARTESIAN_POINT('Ctrl Pts',(-2.86515629953513,1.,2.59318160184908));
#62055=CARTESIAN_POINT('Ctrl Pts',(-2.86943633170722,1.,2.5994287522321));
#62056=CARTESIAN_POINT('Ctrl Pts',(-2.87363176656501,1.,2.60568177881303));
#62057=CARTESIAN_POINT('Ctrl Pts',(-2.87773881947916,1.,2.61193507170955));
#62058=CARTESIAN_POINT('Ctrl Pts',(-2.88176821427525,1.,2.61819596473108));
#62059=CARTESIAN_POINT('Ctrl Pts',(-2.88573922195059,1.,2.62447947640262));
#62060=CARTESIAN_POINT('Ctrl Pts',(-2.88967244854239,1.,2.63080195420767));
#62061=CARTESIAN_POINT('Ctrl Pts',(-2.89358228854544,1.,2.63717442263932));
#62062=CARTESIAN_POINT('Ctrl Pts',(-2.89747231723345,1.,2.64359851684131));
#62063=CARTESIAN_POINT('Ctrl Pts',(-2.90133950224867,1.,2.65007017365564));
#62064=CARTESIAN_POINT('Ctrl Pts',(-2.90517678087461,1.,2.65658188464282));
#62065=CARTESIAN_POINT('Ctrl Pts',(-2.90897617968923,1.,2.6631254261681));
#62066=CARTESIAN_POINT('Ctrl Pts',(-2.91273193382882,1.,2.66969458792631));
#62067=CARTESIAN_POINT('Ctrl Pts',(-2.91644290704285,1.,2.67628728855312));
#62068=CARTESIAN_POINT('Ctrl Pts',(-2.92011090722152,1.,2.68290409279688));
#62069=CARTESIAN_POINT('Ctrl Pts',(-2.92373955325875,1.,2.68954721165339));
#62070=CARTESIAN_POINT('Ctrl Pts',(-2.92733294395267,1.,2.69621932864301));
#62071=CARTESIAN_POINT('Ctrl Pts',(-2.9308943823375,1.,2.70292247416885));
#62072=CARTESIAN_POINT('Ctrl Pts',(-2.93442516311179,1.,2.70965695523787));
#62073=CARTESIAN_POINT('Ctrl Pts',(-2.93792519474972,1.,2.71642190053592));
#62074=CARTESIAN_POINT('Ctrl Pts',(-2.94139351933897,1.,2.72321571511337));
#62075=CARTESIAN_POINT('Ctrl Pts',(-2.94482887675143,1.,2.73003657371617));
#62076=CARTESIAN_POINT('Ctrl Pts',(-2.94823023414364,1.,2.73688288329808));
#62077=CARTESIAN_POINT('Ctrl Pts',(-2.95159737214266,1.,2.74375379492172));
#62078=CARTESIAN_POINT('Ctrl Pts',(-2.95493069316161,1.,2.75064903318947));
#62079=CARTESIAN_POINT('Ctrl Pts',(-2.95823097665896,1.,2.7575686788835));
#62080=CARTESIAN_POINT('Ctrl Pts',(-2.96149914764818,1.,2.76451296269557));
#62081=CARTESIAN_POINT('Ctrl Pts',(-2.96473605585583,1.,2.77148206836498));
#62082=CARTESIAN_POINT('Ctrl Pts',(-2.96794221043036,1.,2.7784758954285));
#62083=CARTESIAN_POINT('Ctrl Pts',(-2.97111781461465,1.,2.78549409123769));
#62084=CARTESIAN_POINT('Ctrl Pts',(-2.9742628834758,1.,2.79253615718248));
#62085=CARTESIAN_POINT('Ctrl Pts',(-2.97737733718287,1.,2.7996015327823));
#62086=CARTESIAN_POINT('Ctrl Pts',(-2.98046109647241,1.,2.80668968101106));
#62087=CARTESIAN_POINT('Ctrl Pts',(-2.98351419779767,1.,2.81380019196286));
#62088=CARTESIAN_POINT('Ctrl Pts',(-2.9865368066918,1.,2.82093279065457));
#62089=CARTESIAN_POINT('Ctrl Pts',(-2.98952916401446,1.,2.82808728190157));
#62090=CARTESIAN_POINT('Ctrl Pts',(-2.9924915517034,1.,2.83526351254248));
#62091=CARTESIAN_POINT('Ctrl Pts',(-2.99542425341685,1.,2.84246132984415));
#62092=CARTESIAN_POINT('Ctrl Pts',(-2.99832751144925,1.,2.84968053289451));
#62093=CARTESIAN_POINT('Ctrl Pts',(-3.00120150796095,1.,2.85692085715686));
#62094=CARTESIAN_POINT('Ctrl Pts',(-3.00404638316867,1.,2.86418200833667));
#62095=CARTESIAN_POINT('Ctrl Pts',(-3.00686224485784,1.,2.87146368430502));
#62096=CARTESIAN_POINT('Ctrl Pts',(-3.00964918108476,1.,2.87876560072727));
#62097=CARTESIAN_POINT('Ctrl Pts',(-3.01240727308829,1.,2.8860875170608));
#62098=CARTESIAN_POINT('Ctrl Pts',(-3.01513660431928,1.,2.89342925566321));
#62099=CARTESIAN_POINT('Ctrl Pts',(-3.01783725121981,1.,2.9007906910105));
#62100=CARTESIAN_POINT('Ctrl Pts',(-3.01997487193503,1.,2.90669553302526));
#62101=CARTESIAN_POINT('Ctrl Pts',(-3.02156522742431,1.,2.91113297348212));
#62102=CARTESIAN_POINT('Ctrl Pts',(-3.02261975104593,1.,2.91409518070399));
#62103=CARTESIAN_POINT('Ctrl Pts',(-3.02314558451372,1.,2.91557726271063));
#62104=CARTESIAN_POINT('Origin',(-3.02314558451372,0.,2.91557726271063));
#62105=CARTESIAN_POINT('',(-2.91557726271063,1.,3.02314558451372));
#62106=CARTESIAN_POINT('Origin',(0.,0.,0.));
#62107=CARTESIAN_POINT('',(-2.90994629141562,1.,2.36531447826213));
#62108=CARTESIAN_POINT('Origin',(0.,1.,0.));
#62109=CARTESIAN_POINT('Ctrl Pts',(-2.90994629141562,1.,2.36531447826213));
#62110=CARTESIAN_POINT('Ctrl Pts',(-2.90994629141562,0.666666666666667,
2.36531447826213));
#62111=CARTESIAN_POINT('Ctrl Pts',(-2.90994629141562,0.333333333333333,
2.36531447826213));
#62112=CARTESIAN_POINT('Ctrl Pts',(-2.90994629141562,-0.333333333333333,
2.36531447826213));
#62113=CARTESIAN_POINT('Ctrl Pts',(-2.90994629141562,-0.666666666666667,
2.36531447826213));
#62114=CARTESIAN_POINT('Ctrl Pts',(-2.90994629141562,-1.,2.36531447826213));
#62115=CARTESIAN_POINT('Ctrl Pts',(-3.35260583073571,-1.,2.52982887637028));
#62116=CARTESIAN_POINT('Ctrl Pts',(-3.35260583073571,1.,2.52982887637028));
#62117=CARTESIAN_POINT('Ctrl Pts',(-3.35105973714426,-1.,2.52954136549357));
#62118=CARTESIAN_POINT('Ctrl Pts',(-3.35105973714426,1.,2.52954136549357));
#62119=CARTESIAN_POINT('Ctrl Pts',(-3.34796903577628,-1.,2.5289632161143));
#62120=CARTESIAN_POINT('Ctrl Pts',(-3.34796903577628,1.,2.5289632161143));
#62121=CARTESIAN_POINT('Ctrl Pts',(-3.34333744117093,-1.,2.52808660916879));
#62122=CARTESIAN_POINT('Ctrl Pts',(-3.34333744117093,1.,2.52808660916879));
#62123=CARTESIAN_POINT('Ctrl Pts',(-3.33717090000955,-1.,2.52689902691551));
#62124=CARTESIAN_POINT('Ctrl Pts',(-3.33717090000955,1.,2.52689902691551));
#62125=CARTESIAN_POINT('Ctrl Pts',(-3.32947762189049,-1.,2.52538321165774));
#62126=CARTESIAN_POINT('Ctrl Pts',(-3.32947762189049,1.,2.52538321165774));
#62127=CARTESIAN_POINT('Ctrl Pts',(-3.32179931079521,-1.,2.52383598396878));
#62128=CARTESIAN_POINT('Ctrl Pts',(-3.32179931079521,1.,2.52383598396878));
#62129=CARTESIAN_POINT('Ctrl Pts',(-3.31413607874727,-1.,2.52225724871375));
#62130=CARTESIAN_POINT('Ctrl Pts',(-3.31413607874727,1.,2.52225724871375));
#62131=CARTESIAN_POINT('Ctrl Pts',(-3.30648808814986,-1.,2.52064689568167));
#62132=CARTESIAN_POINT('Ctrl Pts',(-3.30648808814986,1.,2.52064689568167));
#62133=CARTESIAN_POINT('Ctrl Pts',(-3.29885556387661,-1.,2.51900480700548));
#62134=CARTESIAN_POINT('Ctrl Pts',(-3.29885556387661,1.,2.51900480700548));
#62135=CARTESIAN_POINT('Ctrl Pts',(-3.2912387729863,-1.,2.51733085123316));
#62136=CARTESIAN_POINT('Ctrl Pts',(-3.2912387729863,1.,2.51733085123316));
#62137=CARTESIAN_POINT('Ctrl Pts',(-3.28363799702583,-1.,2.51562487464215));
#62138=CARTESIAN_POINT('Ctrl Pts',(-3.28363799702583,1.,2.51562487464215));
#62139=CARTESIAN_POINT('Ctrl Pts',(-3.27605350473048,-1.,2.51388669270329));
#62140=CARTESIAN_POINT('Ctrl Pts',(-3.27605350473048,1.,2.51388669270329));
#62141=CARTESIAN_POINT('Ctrl Pts',(-3.26848552888271,-1.,2.51211608411539));
#62142=CARTESIAN_POINT('Ctrl Pts',(-3.26848552888271,1.,2.51211608411539));
#62143=CARTESIAN_POINT('Ctrl Pts',(-3.26093423001716,-1.,2.51031277813697));
#62144=CARTESIAN_POINT('Ctrl Pts',(-3.26093423001716,1.,2.51031277813697));
#62145=CARTESIAN_POINT('Ctrl Pts',(-3.25339971461265,-1.,2.50847647070936));
#62146=CARTESIAN_POINT('Ctrl Pts',(-3.25339971461265,1.,2.50847647070936));
#62147=CARTESIAN_POINT('Ctrl Pts',(-3.24588208984042,-1.,2.50660685940645));
#62148=CARTESIAN_POINT('Ctrl Pts',(-3.24588208984042,1.,2.50660685940645));
#62149=CARTESIAN_POINT('Ctrl Pts',(-3.23838151080383,-1.,2.50470367580078));
#62150=CARTESIAN_POINT('Ctrl Pts',(-3.23838151080383,1.,2.50470367580078));
#62151=CARTESIAN_POINT('Ctrl Pts',(-3.23089822320596,-1.,2.50276671338074));
#62152=CARTESIAN_POINT('Ctrl Pts',(-3.23089822320596,1.,2.50276671338074));
#62153=CARTESIAN_POINT('Ctrl Pts',(-3.22343262620387,-1.,2.5007958720187));
#62154=CARTESIAN_POINT('Ctrl Pts',(-3.22343262620387,1.,2.5007958720187));
#62155=CARTESIAN_POINT('Ctrl Pts',(-3.21598526261157,-1.,2.49879114599293));
#62156=CARTESIAN_POINT('Ctrl Pts',(-3.21598526261157,1.,2.49879114599293));
#62157=CARTESIAN_POINT('Ctrl Pts',(-3.2085566984974,-1.,2.49675252647298));
#62158=CARTESIAN_POINT('Ctrl Pts',(-3.2085566984974,1.,2.49675252647298));
#62159=CARTESIAN_POINT('Ctrl Pts',(-3.20114742397549,-1.,2.49467992057726));
#62160=CARTESIAN_POINT('Ctrl Pts',(-3.20114742397549,1.,2.49467992057726));
#62161=CARTESIAN_POINT('Ctrl Pts',(-3.19375775555814,-1.,2.4925730723986));
#62162=CARTESIAN_POINT('Ctrl Pts',(-3.19375775555814,1.,2.4925730723986));
#62163=CARTESIAN_POINT('Ctrl Pts',(-3.18638771282315,-1.,2.49043146334095));
#62164=CARTESIAN_POINT('Ctrl Pts',(-3.18638771282315,1.,2.49043146334095));
#62165=CARTESIAN_POINT('Ctrl Pts',(-3.17903698136679,-1.,2.48825428288243));
#62166=CARTESIAN_POINT('Ctrl Pts',(-3.17903698136679,1.,2.48825428288243));
#62167=CARTESIAN_POINT('Ctrl Pts',(-3.17170518863357,-1.,2.48604065348619));
#62168=CARTESIAN_POINT('Ctrl Pts',(-3.17170518863357,1.,2.48604065348619));
#62169=CARTESIAN_POINT('Ctrl Pts',(-3.16439213290181,-1.,2.48378981792739));
#62170=CARTESIAN_POINT('Ctrl Pts',(-3.16439213290181,1.,2.48378981792739));
#62171=CARTESIAN_POINT('Ctrl Pts',(-3.15709802322735,-1.,2.48150133566568));
#62172=CARTESIAN_POINT('Ctrl Pts',(-3.15709802322735,1.,2.48150133566568));
#62173=CARTESIAN_POINT('Ctrl Pts',(-3.14982373241335,-1.,2.47917529057016));
#62174=CARTESIAN_POINT('Ctrl Pts',(-3.14982373241335,1.,2.47917529057016));
#62175=CARTESIAN_POINT('Ctrl Pts',(-3.14257099546531,-1.,2.47681245356095));
#62176=CARTESIAN_POINT('Ctrl Pts',(-3.14257099546531,1.,2.47681245356095));
#62177=CARTESIAN_POINT('Ctrl Pts',(-3.13534181229282,-1.,2.47441378371923));
#62178=CARTESIAN_POINT('Ctrl Pts',(-3.13534181229282,1.,2.47441378371923));
#62179=CARTESIAN_POINT('Ctrl Pts',(-3.12813790805948,-1.,2.47197997765868));
#62180=CARTESIAN_POINT('Ctrl Pts',(-3.12813790805948,1.,2.47197997765868));
#62181=CARTESIAN_POINT('Ctrl Pts',(-3.12096015766984,-1.,2.4695109894747));
#62182=CARTESIAN_POINT('Ctrl Pts',(-3.12096015766984,1.,2.4695109894747));
#62183=CARTESIAN_POINT('Ctrl Pts',(-3.11380805536124,-1.,2.46700558843507));
#62184=CARTESIAN_POINT('Ctrl Pts',(-3.11380805536124,1.,2.46700558843507));
#62185=CARTESIAN_POINT('Ctrl Pts',(-3.10667907901981,-1.,2.46446082979645));
#62186=CARTESIAN_POINT('Ctrl Pts',(-3.10667907901981,1.,2.46446082979645));
#62187=CARTESIAN_POINT('Ctrl Pts',(-3.09956993697048,-1.,2.4618730850188));
#62188=CARTESIAN_POINT('Ctrl Pts',(-3.09956993697048,1.,2.4618730850188));
#62189=CARTESIAN_POINT('Ctrl Pts',(-3.09247787931881,-1.,2.45923912563875));
#62190=CARTESIAN_POINT('Ctrl Pts',(-3.09247787931881,1.,2.45923912563875));
#62191=CARTESIAN_POINT('Ctrl Pts',(-3.08540206545313,-1.,2.45655725437037));
#62192=CARTESIAN_POINT('Ctrl Pts',(-3.08540206545313,1.,2.45655725437037));
#62193=CARTESIAN_POINT('Ctrl Pts',(-3.07834472886145,-1.,2.45382826787795));
#62194=CARTESIAN_POINT('Ctrl Pts',(-3.07834472886145,1.,2.45382826787795));
#62195=CARTESIAN_POINT('Ctrl Pts',(-3.0713129052131,-1.,2.45105688854432));
#62196=CARTESIAN_POINT('Ctrl Pts',(-3.0713129052131,1.,2.45105688854432));
#62197=CARTESIAN_POINT('Ctrl Pts',(-3.06431596421422,-1.,2.44824970516558));
#62198=CARTESIAN_POINT('Ctrl Pts',(-3.06431596421422,1.,2.44824970516558));
#62199=CARTESIAN_POINT('Ctrl Pts',(-3.05736242671521,-1.,2.44541251892568));
#62200=CARTESIAN_POINT('Ctrl Pts',(-3.05736242671521,1.,2.44541251892568));
#62201=CARTESIAN_POINT('Ctrl Pts',(-3.05045678021509,-1.,2.44254768923109));
#62202=CARTESIAN_POINT('Ctrl Pts',(-3.05045678021509,1.,2.44254768923109));
#62203=CARTESIAN_POINT('Ctrl Pts',(-3.04359685040545,-1.,2.43965194061849));
#62204=CARTESIAN_POINT('Ctrl Pts',(-3.04359685040545,1.,2.43965194061849));
#62205=CARTESIAN_POINT('Ctrl Pts',(-3.03676949672797,-1.,2.43671278042394));
#62206=CARTESIAN_POINT('Ctrl Pts',(-3.03676949672797,1.,2.43671278042394));
#62207=CARTESIAN_POINT('Ctrl Pts',(-3.02995534946946,-1.,2.43371241361462));
#62208=CARTESIAN_POINT('Ctrl Pts',(-3.02995534946946,1.,2.43371241361462));
#62209=CARTESIAN_POINT('Ctrl Pts',(-3.02313656035977,-1.,2.43063415586615));
#62210=CARTESIAN_POINT('Ctrl Pts',(-3.02313656035977,1.,2.43063415586615));
#62211=CARTESIAN_POINT('Ctrl Pts',(-3.01630420830494,-1.,2.4274685626416));
#62212=CARTESIAN_POINT('Ctrl Pts',(-3.01630420830494,1.,2.4274685626416));
#62213=CARTESIAN_POINT('Ctrl Pts',(-3.00946442616674,-1.,2.42421849439625));
#62214=CARTESIAN_POINT('Ctrl Pts',(-3.00946442616674,1.,2.42421849439625));
#62215=CARTESIAN_POINT('Ctrl Pts',(-3.00264868586038,-1.,2.42090763946812));
#62216=CARTESIAN_POINT('Ctrl Pts',(-3.00264868586038,1.,2.42090763946812));
#62217=CARTESIAN_POINT('Ctrl Pts',(-2.99590509293561,-1.,2.4175732450056));
#62218=CARTESIAN_POINT('Ctrl Pts',(-2.99590509293561,1.,2.4175732450056));
#62219=CARTESIAN_POINT('Ctrl Pts',(-2.98927983005851,-1.,2.4142506419963));
#62220=CARTESIAN_POINT('Ctrl Pts',(-2.98927983005851,1.,2.4142506419963));
#62221=CARTESIAN_POINT('Ctrl Pts',(-2.98280015815132,-1.,2.41095909342591));
#62222=CARTESIAN_POINT('Ctrl Pts',(-2.98280015815132,1.,2.41095909342591));
#62223=CARTESIAN_POINT('Ctrl Pts',(-2.97646002822395,-1.,2.40768975073691));
#62224=CARTESIAN_POINT('Ctrl Pts',(-2.97646002822395,1.,2.40768975073691));
#62225=CARTESIAN_POINT('Ctrl Pts',(-2.97019641312272,-1.,2.40438604734848));
#62226=CARTESIAN_POINT('Ctrl Pts',(-2.97019641312272,1.,2.40438604734848));
#62227=CARTESIAN_POINT('Ctrl Pts',(-2.96390432240181,-1.,2.40095565711535));
#62228=CARTESIAN_POINT('Ctrl Pts',(-2.96390432240181,1.,2.40095565711535));
#62229=CARTESIAN_POINT('Ctrl Pts',(-2.95748006482811,-1.,2.39730553974412));
#62230=CARTESIAN_POINT('Ctrl Pts',(-2.95748006482811,1.,2.39730553974412));
#62231=CARTESIAN_POINT('Ctrl Pts',(-2.95085857128372,-1.,2.39337207631613));
#62232=CARTESIAN_POINT('Ctrl Pts',(-2.95085857128372,1.,2.39337207631613));
#62233=CARTESIAN_POINT('Ctrl Pts',(-2.94404820669135,-1.,2.38914929090806));
#62234=CARTESIAN_POINT('Ctrl Pts',(-2.94404820669135,1.,2.38914929090806));
#62235=CARTESIAN_POINT('Ctrl Pts',(-2.93717903280599,-1.,2.38472771516476));
#62236=CARTESIAN_POINT('Ctrl Pts',(-2.93717903280599,1.,2.38472771516476));
#62237=CARTESIAN_POINT('Ctrl Pts',(-2.93049643640517,-1.,2.3802898958232));
#62238=CARTESIAN_POINT('Ctrl Pts',(-2.93049643640517,1.,2.3802898958232));
#62239=CARTESIAN_POINT('Ctrl Pts',(-2.92430340582912,-1.,2.37606510524271));
#62240=CARTESIAN_POINT('Ctrl Pts',(-2.92430340582912,1.,2.37606510524271));
#62241=CARTESIAN_POINT('Ctrl Pts',(-2.9189150379156,-1.,2.37229381109939));
#62242=CARTESIAN_POINT('Ctrl Pts',(-2.9189150379156,1.,2.37229381109939));
#62243=CARTESIAN_POINT('Ctrl Pts',(-2.91461249883016,-1.,2.36919161373074));
#62244=CARTESIAN_POINT('Ctrl Pts',(-2.91461249883016,1.,2.36919161373074));
#62245=CARTESIAN_POINT('Ctrl Pts',(-2.9115863784165,-1.,2.36690501170317));
#62246=CARTESIAN_POINT('Ctrl Pts',(-2.9115863784165,1.,2.36690501170317));
#62247=CARTESIAN_POINT('Ctrl Pts',(-2.91025813829606,-1.,2.36578327194396));
#62248=CARTESIAN_POINT('Ctrl Pts',(-2.91025813829606,1.,2.36578327194396));
#62249=CARTESIAN_POINT('Ctrl Pts',(-2.90989022547738,-1.,2.36535052956704));
#62250=CARTESIAN_POINT('Ctrl Pts',(-2.90989022547738,1.,2.36535052956704));
#62251=CARTESIAN_POINT('Ctrl Pts',(-2.90992398626098,-1.,2.36524348105023));
#62252=CARTESIAN_POINT('Ctrl Pts',(-2.90992398626098,1.,2.36524348105023));
#62253=CARTESIAN_POINT('Ctrl Pts',(-2.91001063062876,-1.,2.36523532225181));
#62254=CARTESIAN_POINT('Ctrl Pts',(-2.91001063062876,1.,2.36523532225181));
#62255=CARTESIAN_POINT('',(-3.35260583073571,1.,2.52982887637028));
#62256=CARTESIAN_POINT('Ctrl Pts',(-3.35260583073571,1.,2.52982887637028));
#62257=CARTESIAN_POINT('Ctrl Pts',(-3.35105973714426,1.,2.52954136549357));
#62258=CARTESIAN_POINT('Ctrl Pts',(-3.34796903577628,1.,2.5289632161143));
#62259=CARTESIAN_POINT('Ctrl Pts',(-3.34333744117093,1.,2.52808660916879));
#62260=CARTESIAN_POINT('Ctrl Pts',(-3.33717090000955,1.,2.52689902691551));
#62261=CARTESIAN_POINT('Ctrl Pts',(-3.32947762189049,1.,2.52538321165774));
#62262=CARTESIAN_POINT('Ctrl Pts',(-3.32179931079521,1.,2.52383598396878));
#62263=CARTESIAN_POINT('Ctrl Pts',(-3.31413607874727,1.,2.52225724871375));
#62264=CARTESIAN_POINT('Ctrl Pts',(-3.30648808814986,1.,2.52064689568167));
#62265=CARTESIAN_POINT('Ctrl Pts',(-3.29885556387661,1.,2.51900480700548));
#62266=CARTESIAN_POINT('Ctrl Pts',(-3.2912387729863,1.,2.51733085123316));
#62267=CARTESIAN_POINT('Ctrl Pts',(-3.28363799702583,1.,2.51562487464215));
#62268=CARTESIAN_POINT('Ctrl Pts',(-3.27605350473048,1.,2.51388669270329));
#62269=CARTESIAN_POINT('Ctrl Pts',(-3.26848552888271,1.,2.51211608411539));
#62270=CARTESIAN_POINT('Ctrl Pts',(-3.26093423001716,1.,2.51031277813697));
#62271=CARTESIAN_POINT('Ctrl Pts',(-3.25339971461265,1.,2.50847647070936));
#62272=CARTESIAN_POINT('Ctrl Pts',(-3.24588208984042,1.,2.50660685940645));
#62273=CARTESIAN_POINT('Ctrl Pts',(-3.23838151080383,1.,2.50470367580078));
#62274=CARTESIAN_POINT('Ctrl Pts',(-3.23089822320596,1.,2.50276671338074));
#62275=CARTESIAN_POINT('Ctrl Pts',(-3.22343262620387,1.,2.5007958720187));
#62276=CARTESIAN_POINT('Ctrl Pts',(-3.21598526261157,1.,2.49879114599293));
#62277=CARTESIAN_POINT('Ctrl Pts',(-3.2085566984974,1.,2.49675252647298));
#62278=CARTESIAN_POINT('Ctrl Pts',(-3.20114742397549,1.,2.49467992057726));
#62279=CARTESIAN_POINT('Ctrl Pts',(-3.19375775555814,1.,2.4925730723986));
#62280=CARTESIAN_POINT('Ctrl Pts',(-3.18638771282315,1.,2.49043146334095));
#62281=CARTESIAN_POINT('Ctrl Pts',(-3.17903698136679,1.,2.48825428288243));
#62282=CARTESIAN_POINT('Ctrl Pts',(-3.17170518863357,1.,2.48604065348619));
#62283=CARTESIAN_POINT('Ctrl Pts',(-3.16439213290181,1.,2.48378981792739));
#62284=CARTESIAN_POINT('Ctrl Pts',(-3.15709802322735,1.,2.48150133566568));
#62285=CARTESIAN_POINT('Ctrl Pts',(-3.14982373241335,1.,2.47917529057016));
#62286=CARTESIAN_POINT('Ctrl Pts',(-3.14257099546531,1.,2.47681245356095));
#62287=CARTESIAN_POINT('Ctrl Pts',(-3.13534181229282,1.,2.47441378371923));
#62288=CARTESIAN_POINT('Ctrl Pts',(-3.12813790805948,1.,2.47197997765868));
#62289=CARTESIAN_POINT('Ctrl Pts',(-3.12096015766984,1.,2.4695109894747));
#62290=CARTESIAN_POINT('Ctrl Pts',(-3.11380805536124,1.,2.46700558843507));
#62291=CARTESIAN_POINT('Ctrl Pts',(-3.10667907901981,1.,2.46446082979645));
#62292=CARTESIAN_POINT('Ctrl Pts',(-3.09956993697048,1.,2.4618730850188));
#62293=CARTESIAN_POINT('Ctrl Pts',(-3.09247787931881,1.,2.45923912563875));
#62294=CARTESIAN_POINT('Ctrl Pts',(-3.08540206545313,1.,2.45655725437037));
#62295=CARTESIAN_POINT('Ctrl Pts',(-3.07834472886145,1.,2.45382826787795));
#62296=CARTESIAN_POINT('Ctrl Pts',(-3.0713129052131,1.,2.45105688854432));
#62297=CARTESIAN_POINT('Ctrl Pts',(-3.06431596421422,1.,2.44824970516558));
#62298=CARTESIAN_POINT('Ctrl Pts',(-3.05736242671521,1.,2.44541251892568));
#62299=CARTESIAN_POINT('Ctrl Pts',(-3.05045678021509,1.,2.44254768923109));
#62300=CARTESIAN_POINT('Ctrl Pts',(-3.04359685040545,1.,2.43965194061849));
#62301=CARTESIAN_POINT('Ctrl Pts',(-3.03676949672797,1.,2.43671278042394));
#62302=CARTESIAN_POINT('Ctrl Pts',(-3.02995534946946,1.,2.43371241361462));
#62303=CARTESIAN_POINT('Ctrl Pts',(-3.02313656035977,1.,2.43063415586615));
#62304=CARTESIAN_POINT('Ctrl Pts',(-3.01630420830494,1.,2.4274685626416));
#62305=CARTESIAN_POINT('Ctrl Pts',(-3.00946442616674,1.,2.42421849439625));
#62306=CARTESIAN_POINT('Ctrl Pts',(-3.00264868586038,1.,2.42090763946812));
#62307=CARTESIAN_POINT('Ctrl Pts',(-2.99590509293561,1.,2.4175732450056));
#62308=CARTESIAN_POINT('Ctrl Pts',(-2.98927983005851,1.,2.4142506419963));
#62309=CARTESIAN_POINT('Ctrl Pts',(-2.98280015815132,1.,2.41095909342591));
#62310=CARTESIAN_POINT('Ctrl Pts',(-2.97646002822395,1.,2.40768975073691));
#62311=CARTESIAN_POINT('Ctrl Pts',(-2.97019641312272,1.,2.40438604734848));
#62312=CARTESIAN_POINT('Ctrl Pts',(-2.96390432240181,1.,2.40095565711535));
#62313=CARTESIAN_POINT('Ctrl Pts',(-2.95748006482811,1.,2.39730553974412));
#62314=CARTESIAN_POINT('Ctrl Pts',(-2.95085857128372,1.,2.39337207631613));
#62315=CARTESIAN_POINT('Ctrl Pts',(-2.94404820669135,1.,2.38914929090806));
#62316=CARTESIAN_POINT('Ctrl Pts',(-2.93717903280599,1.,2.38472771516476));
#62317=CARTESIAN_POINT('Ctrl Pts',(-2.93049643640517,1.,2.3802898958232));
#62318=CARTESIAN_POINT('Ctrl Pts',(-2.92430340582912,1.,2.37606510524271));
#62319=CARTESIAN_POINT('Ctrl Pts',(-2.9189150379156,1.,2.37229381109939));
#62320=CARTESIAN_POINT('Ctrl Pts',(-2.91461249883016,1.,2.36919161373074));
#62321=CARTESIAN_POINT('Ctrl Pts',(-2.91181344022628,1.,2.36707658451709));
#62322=CARTESIAN_POINT('Ctrl Pts',(-2.91051690822262,1.,2.36599991765853));
#62323=CARTESIAN_POINT('Ctrl Pts',(-2.9100577052777,1.,2.36553202948741));
#62324=CARTESIAN_POINT('Ctrl Pts',(-2.90995756655559,1.,2.3653621118858));
#62325=CARTESIAN_POINT('Ctrl Pts',(-2.90994629141563,1.,2.36531447826213));
#62326=CARTESIAN_POINT('',(-3.35260583073571,0.,2.52982887637028));
#62327=CARTESIAN_POINT('Ctrl Pts',(-3.1487152044751,-1.,2.03668666247593));
#62328=CARTESIAN_POINT('Ctrl Pts',(-3.1487152044751,1.,2.03668666247593));
#62329=CARTESIAN_POINT('Ctrl Pts',(-3.14869618937258,-1.,2.03660173757879));
#62330=CARTESIAN_POINT('Ctrl Pts',(-3.14869618937258,1.,2.03660173757879));
#62331=CARTESIAN_POINT('Ctrl Pts',(-3.14878756590812,-1.,2.03653654935592));
#62332=CARTESIAN_POINT('Ctrl Pts',(-3.14878756590812,1.,2.03653654935592));
#62333=CARTESIAN_POINT('Ctrl Pts',(-3.14931281968048,-1.,2.03675273049189));
#62334=CARTESIAN_POINT('Ctrl Pts',(-3.14931281968048,1.,2.03675273049189));
#62335=CARTESIAN_POINT('Ctrl Pts',(-3.15079010635742,-1.,2.03766932526445));
#62336=CARTESIAN_POINT('Ctrl Pts',(-3.15079010635742,1.,2.03766932526445));
#62337=CARTESIAN_POINT('Ctrl Pts',(-3.15389991674792,-1.,2.03984073791519));
#62338=CARTESIAN_POINT('Ctrl Pts',(-3.15389991674792,1.,2.03984073791519));
#62339=CARTESIAN_POINT('Ctrl Pts',(-3.15817983946367,-1.,2.04297406404027));
#62340=CARTESIAN_POINT('Ctrl Pts',(-3.15817983946367,1.,2.04297406404027));
#62341=CARTESIAN_POINT('Ctrl Pts',(-3.16343165058912,-1.,2.04693331247446));
#62342=CARTESIAN_POINT('Ctrl Pts',(-3.16343165058912,1.,2.04693331247446));
#62343=CARTESIAN_POINT('Ctrl Pts',(-3.16936341689527,-1.,2.05151770247233));
#62344=CARTESIAN_POINT('Ctrl Pts',(-3.16936341689527,1.,2.05151770247233));
#62345=CARTESIAN_POINT('Ctrl Pts',(-3.17564906975371,-1.,2.05650186773132));
#62346=CARTESIAN_POINT('Ctrl Pts',(-3.17564906975371,1.,2.05650186773132));
#62347=CARTESIAN_POINT('Ctrl Pts',(-3.18197692964614,-1.,2.06166849827101));
#62348=CARTESIAN_POINT('Ctrl Pts',(-3.18197692964614,1.,2.06166849827101));
#62349=CARTESIAN_POINT('Ctrl Pts',(-3.18809755562368,-1.,2.06684062744112));
#62350=CARTESIAN_POINT('Ctrl Pts',(-3.18809755562368,1.,2.06684062744112));
#62351=CARTESIAN_POINT('Ctrl Pts',(-3.19388465568252,-1.,2.07192253497857));
#62352=CARTESIAN_POINT('Ctrl Pts',(-3.19388465568252,1.,2.07192253497857));
#62353=CARTESIAN_POINT('Ctrl Pts',(-3.19934132836019,-1.,2.07690441870722));
#62354=CARTESIAN_POINT('Ctrl Pts',(-3.19934132836019,1.,2.07690441870722));
#62355=CARTESIAN_POINT('Ctrl Pts',(-3.2045481863073,-1.,2.08182850370878));
#62356=CARTESIAN_POINT('Ctrl Pts',(-3.2045481863073,1.,2.08182850370878));
#62357=CARTESIAN_POINT('Ctrl Pts',(-3.20962575845463,-1.,2.08676465517455));
#62358=CARTESIAN_POINT('Ctrl Pts',(-3.20962575845463,1.,2.08676465517455));
#62359=CARTESIAN_POINT('Ctrl Pts',(-3.21469429601654,-1.,2.09178419460443));
#62360=CARTESIAN_POINT('Ctrl Pts',(-3.21469429601654,1.,2.09178419460443));
#62361=CARTESIAN_POINT('Ctrl Pts',(-3.21982707347009,-1.,2.09692958434895));
#62362=CARTESIAN_POINT('Ctrl Pts',(-3.21982707347009,1.,2.09692958434895));
#62363=CARTESIAN_POINT('Ctrl Pts',(-3.22503437553434,-1.,2.10220384298492));
#62364=CARTESIAN_POINT('Ctrl Pts',(-3.22503437553434,1.,2.10220384298492));
#62365=CARTESIAN_POINT('Ctrl Pts',(-3.23028945793289,-1.,2.10758699642451));
#62366=CARTESIAN_POINT('Ctrl Pts',(-3.23028945793289,1.,2.10758699642451));
#62367=CARTESIAN_POINT('Ctrl Pts',(-3.23554444767099,-1.,2.11304604021773));
#62368=CARTESIAN_POINT('Ctrl Pts',(-3.23554444767099,1.,2.11304604021773));
#62369=CARTESIAN_POINT('Ctrl Pts',(-3.24074905517293,-1.,2.11854673326979));
#62370=CARTESIAN_POINT('Ctrl Pts',(-3.24074905517293,1.,2.11854673326979));
#62371=CARTESIAN_POINT('Ctrl Pts',(-3.24587102613376,-1.,2.12406646410962));
#62372=CARTESIAN_POINT('Ctrl Pts',(-3.24587102613376,1.,2.12406646410962));
#62373=CARTESIAN_POINT('Ctrl Pts',(-3.25090574494028,-1.,2.12960028396832));
#62374=CARTESIAN_POINT('Ctrl Pts',(-3.25090574494028,1.,2.12960028396832));
#62375=CARTESIAN_POINT('Ctrl Pts',(-3.25586495065054,-1.,2.13515375878803));
#62376=CARTESIAN_POINT('Ctrl Pts',(-3.25586495065054,1.,2.13515375878803));
#62377=CARTESIAN_POINT('Ctrl Pts',(-3.26077002641879,-1.,2.14073870754264));
#62378=CARTESIAN_POINT('Ctrl Pts',(-3.26077002641879,1.,2.14073870754264));
#62379=CARTESIAN_POINT('Ctrl Pts',(-3.26564388189759,-1.,2.1463680529566));
#62380=CARTESIAN_POINT('Ctrl Pts',(-3.26564388189759,1.,2.1463680529566));
#62381=CARTESIAN_POINT('Ctrl Pts',(-3.27050245897228,-1.,2.15205043199808));
#62382=CARTESIAN_POINT('Ctrl Pts',(-3.27050245897228,1.,2.15205043199808));
#62383=CARTESIAN_POINT('Ctrl Pts',(-3.27534954469187,-1.,2.15778690038347));
#62384=CARTESIAN_POINT('Ctrl Pts',(-3.27534954469187,1.,2.15778690038347));
#62385=CARTESIAN_POINT('Ctrl Pts',(-3.280181508414,-1.,2.16357391934425));
#62386=CARTESIAN_POINT('Ctrl Pts',(-3.280181508414,1.,2.16357391934425));
#62387=CARTESIAN_POINT('Ctrl Pts',(-3.28499019979724,-1.,2.16940517773455));
#62388=CARTESIAN_POINT('Ctrl Pts',(-3.28499019979724,1.,2.16940517773455));
#62389=CARTESIAN_POINT('Ctrl Pts',(-3.28976645712568,-1.,2.17527380048423));
#62390=CARTESIAN_POINT('Ctrl Pts',(-3.28976645712568,1.,2.17527380048423));
#62391=CARTESIAN_POINT('Ctrl Pts',(-3.2945036150049,-1.,2.18117455557065));
#62392=CARTESIAN_POINT('Ctrl Pts',(-3.2945036150049,1.,2.18117455557065));
#62393=CARTESIAN_POINT('Ctrl Pts',(-3.29920022557639,-1.,2.18710556500327));
#62394=CARTESIAN_POINT('Ctrl Pts',(-3.29920022557639,1.,2.18710556500327));
#62395=CARTESIAN_POINT('Ctrl Pts',(-3.30385816281831,-1.,2.19306710376111));
#62396=CARTESIAN_POINT('Ctrl Pts',(-3.30385816281831,1.,2.19306710376111));
#62397=CARTESIAN_POINT('Ctrl Pts',(-3.30848134694595,-1.,2.19906078949923));
#62398=CARTESIAN_POINT('Ctrl Pts',(-3.30848134694595,1.,2.19906078949923));
#62399=CARTESIAN_POINT('Ctrl Pts',(-3.31307424608949,-1.,2.20508863150607));
#62400=CARTESIAN_POINT('Ctrl Pts',(-3.31307424608949,1.,2.20508863150607));
#62401=CARTESIAN_POINT('Ctrl Pts',(-3.31764044024235,-1.,2.21115211847875));
#62402=CARTESIAN_POINT('Ctrl Pts',(-3.31764044024235,1.,2.21115211847875));
#62403=CARTESIAN_POINT('Ctrl Pts',(-3.32218125618968,-1.,2.21725135110898));
#62404=CARTESIAN_POINT('Ctrl Pts',(-3.32218125618968,1.,2.21725135110898));
#62405=CARTESIAN_POINT('Ctrl Pts',(-3.3266964672289,-1.,2.22338548312772));
#62406=CARTESIAN_POINT('Ctrl Pts',(-3.3266964672289,1.,2.22338548312772));
#62407=CARTESIAN_POINT('Ctrl Pts',(-3.33118487773611,-1.,2.22955308907233));
#62408=CARTESIAN_POINT('Ctrl Pts',(-3.33118487773611,1.,2.22955308907233));
#62409=CARTESIAN_POINT('Ctrl Pts',(-3.33564495756482,-1.,2.23575256328812));
#62410=CARTESIAN_POINT('Ctrl Pts',(-3.33564495756482,1.,2.23575256328812));
#62411=CARTESIAN_POINT('Ctrl Pts',(-3.34007543738025,-1.,2.24198249391422));
#62412=CARTESIAN_POINT('Ctrl Pts',(-3.34007543738025,1.,2.24198249391422));
#62413=CARTESIAN_POINT('Ctrl Pts',(-3.34447596770723,-1.,2.24824207678256));
#62414=CARTESIAN_POINT('Ctrl Pts',(-3.34447596770723,1.,2.24824207678256));
#62415=CARTESIAN_POINT('Ctrl Pts',(-3.34884690292285,-1.,2.25453097693483));
#62416=CARTESIAN_POINT('Ctrl Pts',(-3.34884690292285,1.,2.25453097693483));
#62417=CARTESIAN_POINT('Ctrl Pts',(-3.35318902552626,-1.,2.26084915222449));
#62418=CARTESIAN_POINT('Ctrl Pts',(-3.35318902552626,1.,2.26084915222449));
#62419=CARTESIAN_POINT('Ctrl Pts',(-3.35750328523061,-1.,2.2671966857991));
#62420=CARTESIAN_POINT('Ctrl Pts',(-3.35750328523061,1.,2.2671966857991));
#62421=CARTESIAN_POINT('Ctrl Pts',(-3.36179055004409,-1.,2.2735736262093));
#62422=CARTESIAN_POINT('Ctrl Pts',(-3.36179055004409,1.,2.2735736262093));
#62423=CARTESIAN_POINT('Ctrl Pts',(-3.36605130713076,-1.,2.27997979458037));
#62424=CARTESIAN_POINT('Ctrl Pts',(-3.36605130713076,1.,2.27997979458037));
#62425=CARTESIAN_POINT('Ctrl Pts',(-3.37028570206488,-1.,2.28641481081137));
#62426=CARTESIAN_POINT('Ctrl Pts',(-3.37028570206488,1.,2.28641481081137));
#62427=CARTESIAN_POINT('Ctrl Pts',(-3.37449367172826,-1.,2.29287818007393));
#62428=CARTESIAN_POINT('Ctrl Pts',(-3.37449367172826,1.,2.29287818007393));
#62429=CARTESIAN_POINT('Ctrl Pts',(-3.37867504959433,-1.,2.29936936127624));
#62430=CARTESIAN_POINT('Ctrl Pts',(-3.37867504959433,1.,2.29936936127624));
#62431=CARTESIAN_POINT('Ctrl Pts',(-3.3828296733661,-1.,2.30588783640343));
#62432=CARTESIAN_POINT('Ctrl Pts',(-3.3828296733661,1.,2.30588783640343));
#62433=CARTESIAN_POINT('Ctrl Pts',(-3.38695751492462,-1.,2.31243319489367));
#62434=CARTESIAN_POINT('Ctrl Pts',(-3.38695751492462,1.,2.31243319489367));
#62435=CARTESIAN_POINT('Ctrl Pts',(-3.39105869474822,-1.,2.31900513925424));
#62436=CARTESIAN_POINT('Ctrl Pts',(-3.39105869474822,1.,2.31900513925424));
#62437=CARTESIAN_POINT('Ctrl Pts',(-3.39513342019756,-1.,2.3256034390248));
#62438=CARTESIAN_POINT('Ctrl Pts',(-3.39513342019756,1.,2.3256034390248));
#62439=CARTESIAN_POINT('Ctrl Pts',(-3.39918194577956,-1.,2.33222789882489));
#62440=CARTESIAN_POINT('Ctrl Pts',(-3.39918194577956,1.,2.33222789882489));
#62441=CARTESIAN_POINT('Ctrl Pts',(-3.40320452776743,-1.,2.33887832342782));
#62442=CARTESIAN_POINT('Ctrl Pts',(-3.40320452776743,1.,2.33887832342782));
#62443=CARTESIAN_POINT('Ctrl Pts',(-3.40720137404297,-1.,2.34555447649188));
#62444=CARTESIAN_POINT('Ctrl Pts',(-3.40720137404297,1.,2.34555447649188));
#62445=CARTESIAN_POINT('Ctrl Pts',(-3.41117262314119,-1.,2.35225606824109));
#62446=CARTESIAN_POINT('Ctrl Pts',(-3.41117262314119,1.,2.35225606824109));
#62447=CARTESIAN_POINT('Ctrl Pts',(-3.41511836751469,-1.,2.35898278606946));
#62448=CARTESIAN_POINT('Ctrl Pts',(-3.41511836751469,1.,2.35898278606946));
#62449=CARTESIAN_POINT('Ctrl Pts',(-3.41903866635852,-1.,2.36573431470642));
#62450=CARTESIAN_POINT('Ctrl Pts',(-3.41903866635852,1.,2.36573431470642));
#62451=CARTESIAN_POINT('Ctrl Pts',(-3.42293356216511,-1.,2.37251035954292));
#62452=CARTESIAN_POINT('Ctrl Pts',(-3.42293356216511,1.,2.37251035954292));
#62453=CARTESIAN_POINT('Ctrl Pts',(-3.42680309754399,-1.,2.37931067028926));
#62454=CARTESIAN_POINT('Ctrl Pts',(-3.42680309754399,1.,2.37931067028926));
#62455=CARTESIAN_POINT('Ctrl Pts',(-3.4306473271292,-1.,2.38613505843552));
#62456=CARTESIAN_POINT('Ctrl Pts',(-3.4306473271292,1.,2.38613505843552));
#62457=CARTESIAN_POINT('Ctrl Pts',(-3.4344663067854,-1.,2.39298338804493));
#62458=CARTESIAN_POINT('Ctrl Pts',(-3.4344663067854,1.,2.39298338804493));
#62459=CARTESIAN_POINT('Ctrl Pts',(-3.43750133064416,-1.,2.39848113410292));
#62460=CARTESIAN_POINT('Ctrl Pts',(-3.43750133064416,1.,2.39848113410292));
#62461=CARTESIAN_POINT('Ctrl Pts',(-3.43976627484234,-1.,2.40261515589405));
#62462=CARTESIAN_POINT('Ctrl Pts',(-3.43976627484234,1.,2.40261515589405));
#62463=CARTESIAN_POINT('Ctrl Pts',(-3.44127120683039,-1.,2.4053759295909));
#62464=CARTESIAN_POINT('Ctrl Pts',(-3.44127120683039,1.,2.4053759295909));
#62465=CARTESIAN_POINT('Ctrl Pts',(-3.44202241512147,-1.,2.40675750623143));
#62466=CARTESIAN_POINT('Ctrl Pts',(-3.44202241512147,1.,2.40675750623143));
#62467=CARTESIAN_POINT('',(-3.14877060440327,1.,2.03660101169715));
#62468=CARTESIAN_POINT('Ctrl Pts',(-3.14877060440327,-1.,2.03660101169715));
#62469=CARTESIAN_POINT('Ctrl Pts',(-3.14877060440327,-0.666666666666667,
2.03660101169715));
#62470=CARTESIAN_POINT('Ctrl Pts',(-3.14877060440327,-0.333333333333333,
2.03660101169715));
#62471=CARTESIAN_POINT('Ctrl Pts',(-3.14877060440327,0.333333333333333,
2.03660101169715));
#62472=CARTESIAN_POINT('Ctrl Pts',(-3.14877060440327,0.666666666666667,
2.03660101169715));
#62473=CARTESIAN_POINT('Ctrl Pts',(-3.14877060440327,1.,2.03660101169715));
#62474=CARTESIAN_POINT('',(-3.44202241512147,1.,2.40675750623143));
#62475=CARTESIAN_POINT('',(-3.44202241512147,0.,2.40675750623143));
#62476=CARTESIAN_POINT('Ctrl Pts',(-3.14877060440327,1.,2.03660101169715));
#62477=CARTESIAN_POINT('Ctrl Pts',(-3.14881939088124,1.,2.03659701539259));
#62478=CARTESIAN_POINT('Ctrl Pts',(-3.1490119366901,1.,2.03663974554932));
#62479=CARTESIAN_POINT('Ctrl Pts',(-3.14959882629805,1.,2.03693188810544));
#62480=CARTESIAN_POINT('Ctrl Pts',(-3.15102344775328,1.,2.03783225495961));
#62481=CARTESIAN_POINT('Ctrl Pts',(-3.15389991674792,1.,2.03984073791519));
#62482=CARTESIAN_POINT('Ctrl Pts',(-3.15817983946367,1.,2.04297406404027));
#62483=CARTESIAN_POINT('Ctrl Pts',(-3.16343165058912,1.,2.04693331247446));
#62484=CARTESIAN_POINT('Ctrl Pts',(-3.16936341689527,1.,2.05151770247233));
#62485=CARTESIAN_POINT('Ctrl Pts',(-3.17564906975371,1.,2.05650186773132));
#62486=CARTESIAN_POINT('Ctrl Pts',(-3.18197692964614,1.,2.06166849827101));
#62487=CARTESIAN_POINT('Ctrl Pts',(-3.18809755562368,1.,2.06684062744112));
#62488=CARTESIAN_POINT('Ctrl Pts',(-3.19388465568252,1.,2.07192253497857));
#62489=CARTESIAN_POINT('Ctrl Pts',(-3.19934132836019,1.,2.07690441870722));
#62490=CARTESIAN_POINT('Ctrl Pts',(-3.2045481863073,1.,2.08182850370878));
#62491=CARTESIAN_POINT('Ctrl Pts',(-3.20962575845463,1.,2.08676465517455));
#62492=CARTESIAN_POINT('Ctrl Pts',(-3.21469429601654,1.,2.09178419460443));
#62493=CARTESIAN_POINT('Ctrl Pts',(-3.21982707347009,1.,2.09692958434895));
#62494=CARTESIAN_POINT('Ctrl Pts',(-3.22503437553434,1.,2.10220384298492));
#62495=CARTESIAN_POINT('Ctrl Pts',(-3.23028945793289,1.,2.10758699642451));
#62496=CARTESIAN_POINT('Ctrl Pts',(-3.23554444767099,1.,2.11304604021773));
#62497=CARTESIAN_POINT('Ctrl Pts',(-3.24074905517293,1.,2.11854673326979));
#62498=CARTESIAN_POINT('Ctrl Pts',(-3.24587102613376,1.,2.12406646410962));
#62499=CARTESIAN_POINT('Ctrl Pts',(-3.25090574494028,1.,2.12960028396832));
#62500=CARTESIAN_POINT('Ctrl Pts',(-3.25586495065054,1.,2.13515375878803));
#62501=CARTESIAN_POINT('Ctrl Pts',(-3.26077002641879,1.,2.14073870754264));
#62502=CARTESIAN_POINT('Ctrl Pts',(-3.26564388189759,1.,2.1463680529566));
#62503=CARTESIAN_POINT('Ctrl Pts',(-3.27050245897228,1.,2.15205043199808));
#62504=CARTESIAN_POINT('Ctrl Pts',(-3.27534954469187,1.,2.15778690038347));
#62505=CARTESIAN_POINT('Ctrl Pts',(-3.280181508414,1.,2.16357391934425));
#62506=CARTESIAN_POINT('Ctrl Pts',(-3.28499019979724,1.,2.16940517773455));
#62507=CARTESIAN_POINT('Ctrl Pts',(-3.28976645712568,1.,2.17527380048423));
#62508=CARTESIAN_POINT('Ctrl Pts',(-3.2945036150049,1.,2.18117455557065));
#62509=CARTESIAN_POINT('Ctrl Pts',(-3.29920022557639,1.,2.18710556500327));
#62510=CARTESIAN_POINT('Ctrl Pts',(-3.30385816281831,1.,2.19306710376111));
#62511=CARTESIAN_POINT('Ctrl Pts',(-3.30848134694595,1.,2.19906078949923));
#62512=CARTESIAN_POINT('Ctrl Pts',(-3.31307424608949,1.,2.20508863150607));
#62513=CARTESIAN_POINT('Ctrl Pts',(-3.31764044024235,1.,2.21115211847875));
#62514=CARTESIAN_POINT('Ctrl Pts',(-3.32218125618968,1.,2.21725135110898));
#62515=CARTESIAN_POINT('Ctrl Pts',(-3.3266964672289,1.,2.22338548312772));
#62516=CARTESIAN_POINT('Ctrl Pts',(-3.33118487773611,1.,2.22955308907233));
#62517=CARTESIAN_POINT('Ctrl Pts',(-3.33564495756482,1.,2.23575256328812));
#62518=CARTESIAN_POINT('Ctrl Pts',(-3.34007543738025,1.,2.24198249391422));
#62519=CARTESIAN_POINT('Ctrl Pts',(-3.34447596770723,1.,2.24824207678256));
#62520=CARTESIAN_POINT('Ctrl Pts',(-3.34884690292285,1.,2.25453097693483));
#62521=CARTESIAN_POINT('Ctrl Pts',(-3.35318902552626,1.,2.26084915222449));
#62522=CARTESIAN_POINT('Ctrl Pts',(-3.35750328523061,1.,2.2671966857991));
#62523=CARTESIAN_POINT('Ctrl Pts',(-3.36179055004409,1.,2.2735736262093));
#62524=CARTESIAN_POINT('Ctrl Pts',(-3.36605130713076,1.,2.27997979458037));
#62525=CARTESIAN_POINT('Ctrl Pts',(-3.37028570206488,1.,2.28641481081137));
#62526=CARTESIAN_POINT('Ctrl Pts',(-3.37449367172826,1.,2.29287818007393));
#62527=CARTESIAN_POINT('Ctrl Pts',(-3.37867504959433,1.,2.29936936127624));
#62528=CARTESIAN_POINT('Ctrl Pts',(-3.3828296733661,1.,2.30588783640343));
#62529=CARTESIAN_POINT('Ctrl Pts',(-3.38695751492462,1.,2.31243319489367));
#62530=CARTESIAN_POINT('Ctrl Pts',(-3.39105869474822,1.,2.31900513925424));
#62531=CARTESIAN_POINT('Ctrl Pts',(-3.39513342019756,1.,2.3256034390248));
#62532=CARTESIAN_POINT('Ctrl Pts',(-3.39918194577956,1.,2.33222789882489));
#62533=CARTESIAN_POINT('Ctrl Pts',(-3.40320452776743,1.,2.33887832342782));
#62534=CARTESIAN_POINT('Ctrl Pts',(-3.40720137404297,1.,2.34555447649188));
#62535=CARTESIAN_POINT('Ctrl Pts',(-3.41117262314119,1.,2.35225606824109));
#62536=CARTESIAN_POINT('Ctrl Pts',(-3.41511836751469,1.,2.35898278606946));
#62537=CARTESIAN_POINT('Ctrl Pts',(-3.41903866635852,1.,2.36573431470642));
#62538=CARTESIAN_POINT('Ctrl Pts',(-3.42293356216511,1.,2.37251035954292));
#62539=CARTESIAN_POINT('Ctrl Pts',(-3.42680309754399,1.,2.37931067028926));
#62540=CARTESIAN_POINT('Ctrl Pts',(-3.4306473271292,1.,2.38613505843552));
#62541=CARTESIAN_POINT('Ctrl Pts',(-3.4344663067854,1.,2.39298338804493));
#62542=CARTESIAN_POINT('Ctrl Pts',(-3.43750133064416,1.,2.39848113410292));
#62543=CARTESIAN_POINT('Ctrl Pts',(-3.43976627484234,1.,2.40261515589405));
#62544=CARTESIAN_POINT('Ctrl Pts',(-3.44127120683039,1.,2.4053759295909));
#62545=CARTESIAN_POINT('Ctrl Pts',(-3.44202241512147,1.,2.40675750623143));
#62546=CARTESIAN_POINT('Origin',(-3.44202241512147,0.,2.40675750623143));
#62547=CARTESIAN_POINT('',(-3.35260583073571,1.,2.52982887637028));
#62548=CARTESIAN_POINT('Origin',(0.,0.,0.));
#62549=CARTESIAN_POINT('',(-3.24413672884812,1.,1.88097764062697));
#62550=CARTESIAN_POINT('Origin',(0.,1.,0.));
#62551=CARTESIAN_POINT('Ctrl Pts',(-3.24413672884812,1.,1.88097764062697));
#62552=CARTESIAN_POINT('Ctrl Pts',(-3.24413672884812,0.666666666666667,
1.88097764062697));
#62553=CARTESIAN_POINT('Ctrl Pts',(-3.24413672884812,0.333333333333333,
1.88097764062697));
#62554=CARTESIAN_POINT('Ctrl Pts',(-3.24413672884812,-0.333333333333333,
1.88097764062697));
#62555=CARTESIAN_POINT('Ctrl Pts',(-3.24413672884812,-0.666666666666667,
1.88097764062697));
#62556=CARTESIAN_POINT('Ctrl Pts',(-3.24413672884812,-1.,1.88097764062697));
#62557=CARTESIAN_POINT('Ctrl Pts',(-3.70708211654725,-1.,1.97421938526992));
#62558=CARTESIAN_POINT('Ctrl Pts',(-3.70708211654725,1.,1.97421938526992));
#62559=CARTESIAN_POINT('Ctrl Pts',(-3.70551008132332,-1.,1.97417727645308));
#62560=CARTESIAN_POINT('Ctrl Pts',(-3.70551008132332,1.,1.97417727645308));
#62561=CARTESIAN_POINT('Ctrl Pts',(-3.70236698912904,-1.,1.97408973726715));
#62562=CARTESIAN_POINT('Ctrl Pts',(-3.70236698912904,1.,1.97408973726715));
#62563=CARTESIAN_POINT('Ctrl Pts',(-3.6976552856004,-1.,1.97394846383216));
#62564=CARTESIAN_POINT('Ctrl Pts',(-3.6976552856004,1.,1.97394846383216));
#62565=CARTESIAN_POINT('Ctrl Pts',(-3.69137888599902,-1.,1.97374016225483));
#62566=CARTESIAN_POINT('Ctrl Pts',(-3.69137888599902,1.,1.97374016225483));
#62567=CARTESIAN_POINT('Ctrl Pts',(-3.68354319915092,-1.,1.97344650304519));
#62568=CARTESIAN_POINT('Ctrl Pts',(-3.68354319915092,1.,1.97344650304519));
#62569=CARTESIAN_POINT('Ctrl Pts',(-3.67571738107084,-1.,1.97311947678516));
#62570=CARTESIAN_POINT('Ctrl Pts',(-3.67571738107084,1.,1.97311947678516));
#62571=CARTESIAN_POINT('Ctrl Pts',(-3.66790152752075,-1.,1.97275897198678));
#62572=CARTESIAN_POINT('Ctrl Pts',(-3.66790152752075,1.,1.97275897198678));
#62573=CARTESIAN_POINT('Ctrl Pts',(-3.6600957816636,-1.,1.9723648543905));
#62574=CARTESIAN_POINT('Ctrl Pts',(-3.6600957816636,1.,1.9723648543905));
#62575=CARTESIAN_POINT('Ctrl Pts',(-3.652300347166,-1.,1.9719369724024));
#62576=CARTESIAN_POINT('Ctrl Pts',(-3.652300347166,1.,1.9719369724024));
#62577=CARTESIAN_POINT('Ctrl Pts',(-3.64451546723514,-1.,1.97147515441164));
#62578=CARTESIAN_POINT('Ctrl Pts',(-3.64451546723514,1.,1.97147515441164));
#62579=CARTESIAN_POINT('Ctrl Pts',(-3.63674139590412,-1.,1.97097920454464));
#62580=CARTESIAN_POINT('Ctrl Pts',(-3.63674139590412,1.,1.97097920454464));
#62581=CARTESIAN_POINT('Ctrl Pts',(-3.62897836973293,-1.,1.97044889850463));
#62582=CARTESIAN_POINT('Ctrl Pts',(-3.62897836973293,1.,1.97044889850463));
#62583=CARTESIAN_POINT('Ctrl Pts',(-3.62122658401893,-1.,1.96988398129978));
#62584=CARTESIAN_POINT('Ctrl Pts',(-3.62122658401893,1.,1.96988398129978));
#62585=CARTESIAN_POINT('Ctrl Pts',(-3.61348615496704,-1.,1.96928416040877));
#62586=CARTESIAN_POINT('Ctrl Pts',(-3.61348615496704,1.,1.96928416040877));
#62587=CARTESIAN_POINT('Ctrl Pts',(-3.60575714017989,-1.,1.9686491188594));
#62588=CARTESIAN_POINT('Ctrl Pts',(-3.60575714017989,1.,1.9686491188594));
#62589=CARTESIAN_POINT('Ctrl Pts',(-3.59803959819938,-1.,1.96797854118369));
#62590=CARTESIAN_POINT('Ctrl Pts',(-3.59803959819938,1.,1.96797854118369));
#62591=CARTESIAN_POINT('Ctrl Pts',(-3.59033364022801,-1.,1.96727213799544));
#62592=CARTESIAN_POINT('Ctrl Pts',(-3.59033364022801,1.,1.96727213799544));
#62593=CARTESIAN_POINT('Ctrl Pts',(-3.58263947663829,-1.,1.96652966688911));
#62594=CARTESIAN_POINT('Ctrl Pts',(-3.58263947663829,1.,1.96652966688911));
#62595=CARTESIAN_POINT('Ctrl Pts',(-3.57495748600959,-1.,1.96575096652789));
#62596=CARTESIAN_POINT('Ctrl Pts',(-3.57495748600959,1.,1.96575096652789));
#62597=CARTESIAN_POINT('Ctrl Pts',(-3.56728820357791,-1.,1.96493594634567));
#62598=CARTESIAN_POINT('Ctrl Pts',(-3.56728820357791,1.,1.96493594634567));
#62599=CARTESIAN_POINT('Ctrl Pts',(-3.55963218706096,-1.,1.96408450906812));
#62600=CARTESIAN_POINT('Ctrl Pts',(-3.55963218706096,1.,1.96408450906812));
#62601=CARTESIAN_POINT('Ctrl Pts',(-3.55198990600886,-1.,1.96319648628644));
#62602=CARTESIAN_POINT('Ctrl Pts',(-3.55198990600886,1.,1.96319648628644));
#62603=CARTESIAN_POINT('Ctrl Pts',(-3.54436163300443,-1.,1.96227157573067));
#62604=CARTESIAN_POINT('Ctrl Pts',(-3.54436163300443,1.,1.96227157573067));
#62605=CARTESIAN_POINT('Ctrl Pts',(-3.53674730625813,-1.,1.96130926212689));
#62606=CARTESIAN_POINT('Ctrl Pts',(-3.53674730625813,1.,1.96130926212689));
#62607=CARTESIAN_POINT('Ctrl Pts',(-3.52914648844351,-1.,1.96030879411566));
#62608=CARTESIAN_POINT('Ctrl Pts',(-3.52914648844351,1.,1.96030879411566));
#62609=CARTESIAN_POINT('Ctrl Pts',(-3.52155867431486,-1.,1.95926936324461));
#62610=CARTESIAN_POINT('Ctrl Pts',(-3.52155867431486,1.,1.95926936324461));
#62611=CARTESIAN_POINT('Ctrl Pts',(-3.51398354617794,-1.,1.95819025316779));
#62612=CARTESIAN_POINT('Ctrl Pts',(-3.51398354617794,1.,1.95819025316779));
#62613=CARTESIAN_POINT('Ctrl Pts',(-3.50642124159909,-1.,1.95707099606511));
#62614=CARTESIAN_POINT('Ctrl Pts',(-3.50642124159909,1.,1.95707099606511));
#62615=CARTESIAN_POINT('Ctrl Pts',(-3.49887263575583,-1.,1.95591153823661));
#62616=CARTESIAN_POINT('Ctrl Pts',(-3.49887263575583,1.,1.95591153823661));
#62617=CARTESIAN_POINT('Ctrl Pts',(-3.49133956289133,-1.,1.95471236969643));
#62618=CARTESIAN_POINT('Ctrl Pts',(-3.49133956289133,1.,1.95471236969643));
#62619=CARTESIAN_POINT('Ctrl Pts',(-3.48382414832634,-1.,1.95347412486308));
#62620=CARTESIAN_POINT('Ctrl Pts',(-3.48382414832634,1.,1.95347412486308));
#62621=CARTESIAN_POINT('Ctrl Pts',(-3.47632820495921,-1.,1.95219722189876));
#62622=CARTESIAN_POINT('Ctrl Pts',(-3.47632820495921,1.,1.95219722189876));
#62623=CARTESIAN_POINT('Ctrl Pts',(-3.46885258974191,-1.,1.95088147859876));
#62624=CARTESIAN_POINT('Ctrl Pts',(-3.46885258974191,1.,1.95088147859876));
#62625=CARTESIAN_POINT('Ctrl Pts',(-3.46139661060962,-1.,1.94952575850197));
#62626=CARTESIAN_POINT('Ctrl Pts',(-3.46139661060962,1.,1.94952575850197));
#62627=CARTESIAN_POINT('Ctrl Pts',(-3.45395731584051,-1.,1.94812754766524));
#62628=CARTESIAN_POINT('Ctrl Pts',(-3.45395731584051,1.,1.94812754766524));
#62629=CARTESIAN_POINT('Ctrl Pts',(-3.44653088665681,-1.,1.94668377715329));
#62630=CARTESIAN_POINT('Ctrl Pts',(-3.44653088665681,1.,1.94668377715329));
#62631=CARTESIAN_POINT('Ctrl Pts',(-3.43911410197687,-1.,1.94519168842879));
#62632=CARTESIAN_POINT('Ctrl Pts',(-3.43911410197687,1.,1.94519168842879));
#62633=CARTESIAN_POINT('Ctrl Pts',(-3.43170586602434,-1.,1.94364973660284));
#62634=CARTESIAN_POINT('Ctrl Pts',(-3.43170586602434,1.,1.94364973660284));
#62635=CARTESIAN_POINT('Ctrl Pts',(-3.42430850941503,-1.,1.94205835913696));
#62636=CARTESIAN_POINT('Ctrl Pts',(-3.42430850941503,1.,1.94205835913696));
#62637=CARTESIAN_POINT('Ctrl Pts',(-3.41692971994096,-1.,1.94042111965246));
#62638=CARTESIAN_POINT('Ctrl Pts',(-3.41692971994096,1.,1.94042111965246));
#62639=CARTESIAN_POINT('Ctrl Pts',(-3.40957978266642,-1.,1.93874306008143));
#62640=CARTESIAN_POINT('Ctrl Pts',(-3.40957978266642,1.,1.93874306008143));
#62641=CARTESIAN_POINT('Ctrl Pts',(-3.40226802104109,-1.,1.93702857723098));
#62642=CARTESIAN_POINT('Ctrl Pts',(-3.40226802104109,1.,1.93702857723098));
#62643=CARTESIAN_POINT('Ctrl Pts',(-3.39499923640795,-1.,1.93527929945985));
#62644=CARTESIAN_POINT('Ctrl Pts',(-3.39499923640795,1.,1.93527929945985));
#62645=CARTESIAN_POINT('Ctrl Pts',(-3.38777076883256,-1.,1.93349233176788));
#62646=CARTESIAN_POINT('Ctrl Pts',(-3.38777076883256,1.,1.93349233176788));
#62647=CARTESIAN_POINT('Ctrl Pts',(-3.3805676852555,-1.,1.93165739093276));
#62648=CARTESIAN_POINT('Ctrl Pts',(-3.3805676852555,1.,1.93165739093276));
#62649=CARTESIAN_POINT('Ctrl Pts',(-3.37336807068043,-1.,1.92975993109877));
#62650=CARTESIAN_POINT('Ctrl Pts',(-3.37336807068043,1.,1.92975993109877));
#62651=CARTESIAN_POINT('Ctrl Pts',(-3.36615168657567,-1.,1.92778626543786));
#62652=CARTESIAN_POINT('Ctrl Pts',(-3.36615168657567,1.,1.92778626543786));
#62653=CARTESIAN_POINT('Ctrl Pts',(-3.35890824422965,-1.,1.92572846125756));
#62654=CARTESIAN_POINT('Ctrl Pts',(-3.35890824422965,1.,1.92572846125756));
#62655=CARTESIAN_POINT('Ctrl Pts',(-3.35164424847223,-1.,1.92358838440528));
#62656=CARTESIAN_POINT('Ctrl Pts',(-3.35164424847223,1.,1.92358838440528));
#62657=CARTESIAN_POINT('Ctrl Pts',(-3.34439448941961,-1.,1.92138450828404));
#62658=CARTESIAN_POINT('Ctrl Pts',(-3.34439448941961,1.,1.92138450828404));
#62659=CARTESIAN_POINT('Ctrl Pts',(-3.33721230710012,-1.,1.9191460961021));
#62660=CARTESIAN_POINT('Ctrl Pts',(-3.33721230710012,1.,1.9191460961021));
#62661=CARTESIAN_POINT('Ctrl Pts',(-3.33014884257873,-1.,1.91690081930331));
#62662=CARTESIAN_POINT('Ctrl Pts',(-3.33014884257873,1.,1.91690081930331));
#62663=CARTESIAN_POINT('Ctrl Pts',(-3.32323403454535,-1.,1.91466343916628));
#62664=CARTESIAN_POINT('Ctrl Pts',(-3.32323403454535,1.,1.91466343916628));
#62665=CARTESIAN_POINT('Ctrl Pts',(-3.31646052426364,-1.,1.91242616234442));
#62666=CARTESIAN_POINT('Ctrl Pts',(-3.31646052426364,1.,1.91242616234442));
#62667=CARTESIAN_POINT('Ctrl Pts',(-3.30975721158596,-1.,1.91014297830446));
#62668=CARTESIAN_POINT('Ctrl Pts',(-3.30975721158596,1.,1.91014297830446));
#62669=CARTESIAN_POINT('Ctrl Pts',(-3.30300595568195,-1.,1.90773912171341));
#62670=CARTESIAN_POINT('Ctrl Pts',(-3.30300595568195,1.,1.90773912171341));
#62671=CARTESIAN_POINT('Ctrl Pts',(-3.29608978722113,-1.,1.90513891864087));
#62672=CARTESIAN_POINT('Ctrl Pts',(-3.29608978722113,1.,1.90513891864087));
#62673=CARTESIAN_POINT('Ctrl Pts',(-3.2889344860029,-1.,1.90228971247527));
#62674=CARTESIAN_POINT('Ctrl Pts',(-3.2889344860029,1.,1.90228971247527));
#62675=CARTESIAN_POINT('Ctrl Pts',(-3.28154737912352,-1.,1.89918429230462));
#62676=CARTESIAN_POINT('Ctrl Pts',(-3.28154737912352,1.,1.89918429230462));
#62677=CARTESIAN_POINT('Ctrl Pts',(-3.27407108933139,-1.,1.89589172903793));
#62678=CARTESIAN_POINT('Ctrl Pts',(-3.27407108933139,1.,1.89589172903793));
#62679=CARTESIAN_POINT('Ctrl Pts',(-3.26677653888676,-1.,1.89255393500965));
#62680=CARTESIAN_POINT('Ctrl Pts',(-3.26677653888676,1.,1.89255393500965));
#62681=CARTESIAN_POINT('Ctrl Pts',(-3.25999885193947,-1.,1.88934996203698));
#62682=CARTESIAN_POINT('Ctrl Pts',(-3.25999885193947,1.,1.88934996203698));
#62683=CARTESIAN_POINT('Ctrl Pts',(-3.25408686339463,-1.,1.88646802523466));
#62684=CARTESIAN_POINT('Ctrl Pts',(-3.25408686339463,1.,1.88646802523466));
#62685=CARTESIAN_POINT('Ctrl Pts',(-3.24935200511918,-1.,1.88407708646357));
#62686=CARTESIAN_POINT('Ctrl Pts',(-3.24935200511918,1.,1.88407708646357));
#62687=CARTESIAN_POINT('Ctrl Pts',(-3.24600543790443,-1.,1.88229202582941));
#62688=CARTESIAN_POINT('Ctrl Pts',(-3.24600543790443,1.,1.88229202582941));
#62689=CARTESIAN_POINT('Ctrl Pts',(-3.24451807186481,-1.,1.88139187908074));
#62690=CARTESIAN_POINT('Ctrl Pts',(-3.24451807186481,1.,1.88139187908074));
#62691=CARTESIAN_POINT('Ctrl Pts',(-3.24408699284121,-1.,1.88102201872555));
#62692=CARTESIAN_POINT('Ctrl Pts',(-3.24408699284121,1.,1.88102201872555));
#62693=CARTESIAN_POINT('Ctrl Pts',(-3.24410359189609,-1.,1.88091100680349));
#62694=CARTESIAN_POINT('Ctrl Pts',(-3.24410359189609,1.,1.88091100680349));
#62695=CARTESIAN_POINT('Ctrl Pts',(-3.24418789321065,-1.,1.8808893942881));
#62696=CARTESIAN_POINT('Ctrl Pts',(-3.24418789321065,1.,1.8808893942881));
#62697=CARTESIAN_POINT('',(-3.70708211654725,1.,1.97421938526992));
#62698=CARTESIAN_POINT('Ctrl Pts',(-3.70708211654725,1.,1.97421938526992));
#62699=CARTESIAN_POINT('Ctrl Pts',(-3.70551008132332,1.,1.97417727645308));
#62700=CARTESIAN_POINT('Ctrl Pts',(-3.70236698912904,1.,1.97408973726715));
#62701=CARTESIAN_POINT('Ctrl Pts',(-3.6976552856004,1.,1.97394846383216));
#62702=CARTESIAN_POINT('Ctrl Pts',(-3.69137888599902,1.,1.97374016225483));
#62703=CARTESIAN_POINT('Ctrl Pts',(-3.68354319915092,1.,1.97344650304519));
#62704=CARTESIAN_POINT('Ctrl Pts',(-3.67571738107084,1.,1.97311947678516));
#62705=CARTESIAN_POINT('Ctrl Pts',(-3.66790152752075,1.,1.97275897198678));
#62706=CARTESIAN_POINT('Ctrl Pts',(-3.6600957816636,1.,1.9723648543905));
#62707=CARTESIAN_POINT('Ctrl Pts',(-3.652300347166,1.,1.9719369724024));
#62708=CARTESIAN_POINT('Ctrl Pts',(-3.64451546723514,1.,1.97147515441164));
#62709=CARTESIAN_POINT('Ctrl Pts',(-3.63674139590412,1.,1.97097920454464));
#62710=CARTESIAN_POINT('Ctrl Pts',(-3.62897836973293,1.,1.97044889850463));
#62711=CARTESIAN_POINT('Ctrl Pts',(-3.62122658401893,1.,1.96988398129978));
#62712=CARTESIAN_POINT('Ctrl Pts',(-3.61348615496704,1.,1.96928416040877));
#62713=CARTESIAN_POINT('Ctrl Pts',(-3.60575714017989,1.,1.9686491188594));
#62714=CARTESIAN_POINT('Ctrl Pts',(-3.59803959819938,1.,1.96797854118369));
#62715=CARTESIAN_POINT('Ctrl Pts',(-3.59033364022801,1.,1.96727213799544));
#62716=CARTESIAN_POINT('Ctrl Pts',(-3.58263947663829,1.,1.96652966688911));
#62717=CARTESIAN_POINT('Ctrl Pts',(-3.57495748600959,1.,1.96575096652789));
#62718=CARTESIAN_POINT('Ctrl Pts',(-3.56728820357791,1.,1.96493594634567));
#62719=CARTESIAN_POINT('Ctrl Pts',(-3.55963218706096,1.,1.96408450906812));
#62720=CARTESIAN_POINT('Ctrl Pts',(-3.55198990600886,1.,1.96319648628644));
#62721=CARTESIAN_POINT('Ctrl Pts',(-3.54436163300443,1.,1.96227157573067));
#62722=CARTESIAN_POINT('Ctrl Pts',(-3.53674730625813,1.,1.96130926212689));
#62723=CARTESIAN_POINT('Ctrl Pts',(-3.52914648844351,1.,1.96030879411566));
#62724=CARTESIAN_POINT('Ctrl Pts',(-3.52155867431486,1.,1.95926936324461));
#62725=CARTESIAN_POINT('Ctrl Pts',(-3.51398354617794,1.,1.95819025316779));
#62726=CARTESIAN_POINT('Ctrl Pts',(-3.50642124159909,1.,1.95707099606511));
#62727=CARTESIAN_POINT('Ctrl Pts',(-3.49887263575583,1.,1.95591153823661));
#62728=CARTESIAN_POINT('Ctrl Pts',(-3.49133956289133,1.,1.95471236969643));
#62729=CARTESIAN_POINT('Ctrl Pts',(-3.48382414832634,1.,1.95347412486308));
#62730=CARTESIAN_POINT('Ctrl Pts',(-3.47632820495921,1.,1.95219722189876));
#62731=CARTESIAN_POINT('Ctrl Pts',(-3.46885258974191,1.,1.95088147859876));
#62732=CARTESIAN_POINT('Ctrl Pts',(-3.46139661060962,1.,1.94952575850197));
#62733=CARTESIAN_POINT('Ctrl Pts',(-3.45395731584051,1.,1.94812754766524));
#62734=CARTESIAN_POINT('Ctrl Pts',(-3.44653088665681,1.,1.94668377715329));
#62735=CARTESIAN_POINT('Ctrl Pts',(-3.43911410197687,1.,1.94519168842879));
#62736=CARTESIAN_POINT('Ctrl Pts',(-3.43170586602434,1.,1.94364973660284));
#62737=CARTESIAN_POINT('Ctrl Pts',(-3.42430850941503,1.,1.94205835913696));
#62738=CARTESIAN_POINT('Ctrl Pts',(-3.41692971994096,1.,1.94042111965246));
#62739=CARTESIAN_POINT('Ctrl Pts',(-3.40957978266642,1.,1.93874306008143));
#62740=CARTESIAN_POINT('Ctrl Pts',(-3.40226802104109,1.,1.93702857723098));
#62741=CARTESIAN_POINT('Ctrl Pts',(-3.39499923640795,1.,1.93527929945985));
#62742=CARTESIAN_POINT('Ctrl Pts',(-3.38777076883256,1.,1.93349233176788));
#62743=CARTESIAN_POINT('Ctrl Pts',(-3.3805676852555,1.,1.93165739093276));
#62744=CARTESIAN_POINT('Ctrl Pts',(-3.37336807068043,1.,1.92975993109877));
#62745=CARTESIAN_POINT('Ctrl Pts',(-3.36615168657567,1.,1.92778626543786));
#62746=CARTESIAN_POINT('Ctrl Pts',(-3.35890824422965,1.,1.92572846125756));
#62747=CARTESIAN_POINT('Ctrl Pts',(-3.35164424847223,1.,1.92358838440528));
#62748=CARTESIAN_POINT('Ctrl Pts',(-3.34439448941961,1.,1.92138450828404));
#62749=CARTESIAN_POINT('Ctrl Pts',(-3.33721230710012,1.,1.9191460961021));
#62750=CARTESIAN_POINT('Ctrl Pts',(-3.33014884257873,1.,1.91690081930331));
#62751=CARTESIAN_POINT('Ctrl Pts',(-3.32323403454535,1.,1.91466343916628));
#62752=CARTESIAN_POINT('Ctrl Pts',(-3.31646052426364,1.,1.91242616234442));
#62753=CARTESIAN_POINT('Ctrl Pts',(-3.30975721158596,1.,1.91014297830446));
#62754=CARTESIAN_POINT('Ctrl Pts',(-3.30300595568195,1.,1.90773912171341));
#62755=CARTESIAN_POINT('Ctrl Pts',(-3.29608978722113,1.,1.90513891864087));
#62756=CARTESIAN_POINT('Ctrl Pts',(-3.2889344860029,1.,1.90228971247527));
#62757=CARTESIAN_POINT('Ctrl Pts',(-3.28154737912352,1.,1.89918429230462));
#62758=CARTESIAN_POINT('Ctrl Pts',(-3.27407108933139,1.,1.89589172903793));
#62759=CARTESIAN_POINT('Ctrl Pts',(-3.26677653888676,1.,1.89255393500965));
#62760=CARTESIAN_POINT('Ctrl Pts',(-3.25999885193947,1.,1.88934996203698));
#62761=CARTESIAN_POINT('Ctrl Pts',(-3.25408686339463,1.,1.88646802523466));
#62762=CARTESIAN_POINT('Ctrl Pts',(-3.24935200511918,1.,1.88407708646357));
#62763=CARTESIAN_POINT('Ctrl Pts',(-3.2462565441079,1.,1.88242596600454));
#62764=CARTESIAN_POINT('Ctrl Pts',(-3.24480754676064,1.,1.88156537699203));
#62765=CARTESIAN_POINT('Ctrl Pts',(-3.24428080353022,1.,1.88117508446775));
#62766=CARTESIAN_POINT('Ctrl Pts',(-3.24415531671284,1.,1.8810229239812));
#62767=CARTESIAN_POINT('Ctrl Pts',(-3.24413672884812,1.,1.88097764062697));
#62768=CARTESIAN_POINT('',(-3.70708211654725,0.,1.97421938526992));
#62769=CARTESIAN_POINT('Ctrl Pts',(-3.42855728381368,-1.,1.519044091397));
#62770=CARTESIAN_POINT('Ctrl Pts',(-3.42855728381368,1.,1.519044091397));
#62771=CARTESIAN_POINT('Ctrl Pts',(-3.42852521763778,-1.,1.51896318668366));
#62772=CARTESIAN_POINT('Ctrl Pts',(-3.42852521763778,1.,1.51896318668366));
#62773=CARTESIAN_POINT('Ctrl Pts',(-3.42860527149177,-1.,1.51888450659652));
#62774=CARTESIAN_POINT('Ctrl Pts',(-3.42860527149177,1.,1.51888450659652));
#62775=CARTESIAN_POINT('Ctrl Pts',(-3.42915787669893,-1.,1.51901585839109));
#62776=CARTESIAN_POINT('Ctrl Pts',(-3.42915787669893,1.,1.51901585839109));
#62777=CARTESIAN_POINT('Ctrl Pts',(-3.43076036253837,-1.,1.51969006980999));
#62778=CARTESIAN_POINT('Ctrl Pts',(-3.43076036253837,1.,1.51969006980999));
#62779=CARTESIAN_POINT('Ctrl Pts',(-3.43417156977893,-1.,1.52134826724292));
#62780=CARTESIAN_POINT('Ctrl Pts',(-3.43417156977893,1.,1.52134826724292));
#62781=CARTESIAN_POINT('Ctrl Pts',(-3.4388889597401,-1.,1.5237734895035));
#62782=CARTESIAN_POINT('Ctrl Pts',(-3.4388889597401,1.,1.5237734895035));
#62783=CARTESIAN_POINT('Ctrl Pts',(-3.44469547526647,-1.,1.52686242875556));
#62784=CARTESIAN_POINT('Ctrl Pts',(-3.44469547526647,1.,1.52686242875556));
#62785=CARTESIAN_POINT('Ctrl Pts',(-3.45127136828305,-1.,1.53046244461635));
#62786=CARTESIAN_POINT('Ctrl Pts',(-3.45127136828305,1.,1.53046244461635));
#62787=CARTESIAN_POINT('Ctrl Pts',(-3.45825932955032,-1.,1.53440195378792));
#62788=CARTESIAN_POINT('Ctrl Pts',(-3.45825932955032,1.,1.53440195378792));
#62789=CARTESIAN_POINT('Ctrl Pts',(-3.46531752207153,-1.,1.53851507915502));
#62790=CARTESIAN_POINT('Ctrl Pts',(-3.46531752207153,1.,1.53851507915502));
#62791=CARTESIAN_POINT('Ctrl Pts',(-3.47217189224653,-1.,1.54266605398187));
#62792=CARTESIAN_POINT('Ctrl Pts',(-3.47217189224653,1.,1.54266605398187));
#62793=CARTESIAN_POINT('Ctrl Pts',(-3.47868272898751,-1.,1.54678009290276));
#62794=CARTESIAN_POINT('Ctrl Pts',(-3.47868272898751,1.,1.54678009290276));
#62795=CARTESIAN_POINT('Ctrl Pts',(-3.48485155928567,-1.,1.55084702970452));
#62796=CARTESIAN_POINT('Ctrl Pts',(-3.48485155928567,1.,1.55084702970452));
#62797=CARTESIAN_POINT('Ctrl Pts',(-3.4907646087742,-1.,1.55489595901116));
#62798=CARTESIAN_POINT('Ctrl Pts',(-3.4907646087742,1.,1.55489595901116));
#62799=CARTESIAN_POINT('Ctrl Pts',(-3.49655185179655,-1.,1.55897703097874));
#62800=CARTESIAN_POINT('Ctrl Pts',(-3.49655185179655,1.,1.55897703097874));
#62801=CARTESIAN_POINT('Ctrl Pts',(-3.50234321621578,-1.,1.56314187758675));
#62802=CARTESIAN_POINT('Ctrl Pts',(-3.50234321621578,1.,1.56314187758675));
#62803=CARTESIAN_POINT('Ctrl Pts',(-3.50821771695363,-1.,1.56742097575012));
#62804=CARTESIAN_POINT('Ctrl Pts',(-3.50821771695363,1.,1.56742097575012));
#62805=CARTESIAN_POINT('Ctrl Pts',(-3.51418598431665,-1.,1.57181569799743));
#62806=CARTESIAN_POINT('Ctrl Pts',(-3.51418598431665,1.,1.57181569799743));
#62807=CARTESIAN_POINT('Ctrl Pts',(-3.52021847865912,-1.,1.57631049988158));
#62808=CARTESIAN_POINT('Ctrl Pts',(-3.52021847865912,1.,1.57631049988158));
#62809=CARTESIAN_POINT('Ctrl Pts',(-3.52626275334881,-1.,1.58088027227848));
#62810=CARTESIAN_POINT('Ctrl Pts',(-3.52626275334881,1.,1.58088027227848));
#62811=CARTESIAN_POINT('Ctrl Pts',(-3.5322637814708,-1.,1.58549906268088));
#62812=CARTESIAN_POINT('Ctrl Pts',(-3.5322637814708,1.,1.58549906268088));
#62813=CARTESIAN_POINT('Ctrl Pts',(-3.53818616861077,-1.,1.59014958368739));
#62814=CARTESIAN_POINT('Ctrl Pts',(-3.53818616861077,1.,1.59014958368739));
#62815=CARTESIAN_POINT('Ctrl Pts',(-3.54402458182337,-1.,1.59482766949766));
#62816=CARTESIAN_POINT('Ctrl Pts',(-3.54402458182337,1.,1.59482766949766));
#62817=CARTESIAN_POINT('Ctrl Pts',(-3.54979148634454,-1.,1.59953698113457));
#62818=CARTESIAN_POINT('Ctrl Pts',(-3.54979148634454,1.,1.59953698113457));
#62819=CARTESIAN_POINT('Ctrl Pts',(-3.55550985096129,-1.,1.60428584699853));
#62820=CARTESIAN_POINT('Ctrl Pts',(-3.55550985096129,1.,1.60428584699853));
#62821=CARTESIAN_POINT('Ctrl Pts',(-3.5612043248298,-1.,1.60908344685457));
#62822=CARTESIAN_POINT('Ctrl Pts',(-3.5612043248298,1.,1.60908344685457));
#62823=CARTESIAN_POINT('Ctrl Pts',(-3.56689200468387,-1.,1.61393581747514));
#62824=CARTESIAN_POINT('Ctrl Pts',(-3.56689200468387,1.,1.61393581747514));
#62825=CARTESIAN_POINT('Ctrl Pts',(-3.57257679609806,-1.,1.61884340915404));
#62826=CARTESIAN_POINT('Ctrl Pts',(-3.57257679609806,1.,1.61884340915404));
#62827=CARTESIAN_POINT('Ctrl Pts',(-3.5782545595439,-1.,1.62380329464844));
#62828=CARTESIAN_POINT('Ctrl Pts',(-3.5782545595439,1.,1.62380329464844));
#62829=CARTESIAN_POINT('Ctrl Pts',(-3.58391625774343,-1.,1.62881051550745));
#62830=CARTESIAN_POINT('Ctrl Pts',(-3.58391625774343,1.,1.62881051550745));
#62831=CARTESIAN_POINT('Ctrl Pts',(-3.58955176627879,-1.,1.6338597145126));
#62832=CARTESIAN_POINT('Ctrl Pts',(-3.58955176627879,1.,1.6338597145126));
#62833=CARTESIAN_POINT('Ctrl Pts',(-3.59515368334893,-1.,1.63894676675352));
#62834=CARTESIAN_POINT('Ctrl Pts',(-3.59515368334893,1.,1.63894676675352));
#62835=CARTESIAN_POINT('Ctrl Pts',(-3.60072028513845,-1.,1.64407004385582));
#62836=CARTESIAN_POINT('Ctrl Pts',(-3.60072028513845,1.,1.64407004385582));
#62837=CARTESIAN_POINT('Ctrl Pts',(-3.60625346556992,-1.,1.64922952425832));
#62838=CARTESIAN_POINT('Ctrl Pts',(-3.60625346556992,1.,1.64922952425832));
#62839=CARTESIAN_POINT('Ctrl Pts',(-3.61175734965127,-1.,1.65442619244325));
#62840=CARTESIAN_POINT('Ctrl Pts',(-3.61175734965127,1.,1.65442619244325));
#62841=CARTESIAN_POINT('Ctrl Pts',(-3.61723666482456,-1.,1.65966133399186));
#62842=CARTESIAN_POINT('Ctrl Pts',(-3.61723666482456,1.,1.65966133399186));
#62843=CARTESIAN_POINT('Ctrl Pts',(-3.62269517989109,-1.,1.66493585923855));
#62844=CARTESIAN_POINT('Ctrl Pts',(-3.62269517989109,1.,1.66493585923855));
#62845=CARTESIAN_POINT('Ctrl Pts',(-3.62813422105271,-1.,1.67024966008045));
#62846=CARTESIAN_POINT('Ctrl Pts',(-3.62813422105271,1.,1.67024966008045));
#62847=CARTESIAN_POINT('Ctrl Pts',(-3.63355343201232,-1.,1.67560193613156));
#62848=CARTESIAN_POINT('Ctrl Pts',(-3.63355343201232,1.,1.67560193613156));
#62849=CARTESIAN_POINT('Ctrl Pts',(-3.63895140887462,-1.,1.68099146651586));
#62850=CARTESIAN_POINT('Ctrl Pts',(-3.63895140887462,1.,1.68099146651586));
#62851=CARTESIAN_POINT('Ctrl Pts',(-3.64432638915203,-1.,1.68641690471457));
#62852=CARTESIAN_POINT('Ctrl Pts',(-3.64432638915203,1.,1.68641690471457));
#62853=CARTESIAN_POINT('Ctrl Pts',(-3.64967689827371,-1.,1.69187705481689));
#62854=CARTESIAN_POINT('Ctrl Pts',(-3.64967689827371,1.,1.69187705481689));
#62855=CARTESIAN_POINT('Ctrl Pts',(-3.65500246526749,-1.,1.69737117722534));
#62856=CARTESIAN_POINT('Ctrl Pts',(-3.65500246526749,1.,1.69737117722534));
#62857=CARTESIAN_POINT('Ctrl Pts',(-3.66030338774847,-1.,1.70289888566873));
#62858=CARTESIAN_POINT('Ctrl Pts',(-3.66030338774847,1.,1.70289888566873));
#62859=CARTESIAN_POINT('Ctrl Pts',(-3.66558043198876,-1.,1.70846001610956));
#62860=CARTESIAN_POINT('Ctrl Pts',(-3.66558043198876,1.,1.70846001610956));
#62861=CARTESIAN_POINT('Ctrl Pts',(-3.67083454901611,-1.,1.71405450210383));
#62862=CARTESIAN_POINT('Ctrl Pts',(-3.67083454901611,1.,1.71405450210383));
#62863=CARTESIAN_POINT('Ctrl Pts',(-3.67606660374709,-1.,1.71968225581808));
#62864=CARTESIAN_POINT('Ctrl Pts',(-3.67606660374709,1.,1.71968225581808));
#62865=CARTESIAN_POINT('Ctrl Pts',(-3.68127704936579,-1.,1.72534302437056));
#62866=CARTESIAN_POINT('Ctrl Pts',(-3.68127704936579,1.,1.72534302437056));
#62867=CARTESIAN_POINT('Ctrl Pts',(-3.68646597019332,-1.,1.73103640956717));
#62868=CARTESIAN_POINT('Ctrl Pts',(-3.68646597019332,1.,1.73103640956717));
#62869=CARTESIAN_POINT('Ctrl Pts',(-3.69163322648036,-1.,1.73676193254557));
#62870=CARTESIAN_POINT('Ctrl Pts',(-3.69163322648036,1.,1.73676193254557));
#62871=CARTESIAN_POINT('Ctrl Pts',(-3.69677856910517,-1.,1.74251908492617));
#62872=CARTESIAN_POINT('Ctrl Pts',(-3.69677856910517,1.,1.74251908492617));
#62873=CARTESIAN_POINT('Ctrl Pts',(-3.7019017567335,-1.,1.74830738046057));
#62874=CARTESIAN_POINT('Ctrl Pts',(-3.7019017567335,1.,1.74830738046057));
#62875=CARTESIAN_POINT('Ctrl Pts',(-3.70700269736659,-1.,1.75412641804042));
#62876=CARTESIAN_POINT('Ctrl Pts',(-3.70700269736659,1.,1.75412641804042));
#62877=CARTESIAN_POINT('Ctrl Pts',(-3.71208146346136,-1.,1.75997588498865));
#62878=CARTESIAN_POINT('Ctrl Pts',(-3.71208146346136,1.,1.75997588498865));
#62879=CARTESIAN_POINT('Ctrl Pts',(-3.71713822377359,-1.,1.76585552124394));
#62880=CARTESIAN_POINT('Ctrl Pts',(-3.71713822377359,1.,1.76585552124394));
#62881=CARTESIAN_POINT('Ctrl Pts',(-3.72217319911254,-1.,1.77176509401761));
#62882=CARTESIAN_POINT('Ctrl Pts',(-3.72217319911254,1.,1.77176509401761));
#62883=CARTESIAN_POINT('Ctrl Pts',(-3.72718661205609,-1.,1.77770437039658));
#62884=CARTESIAN_POINT('Ctrl Pts',(-3.72718661205609,1.,1.77770437039658));
#62885=CARTESIAN_POINT('Ctrl Pts',(-3.7321786309547,-1.,1.78367308442901));
#62886=CARTESIAN_POINT('Ctrl Pts',(-3.7321786309547,1.,1.78367308442901));
#62887=CARTESIAN_POINT('Ctrl Pts',(-3.73714934730681,-1.,1.78967092823491));
#62888=CARTESIAN_POINT('Ctrl Pts',(-3.73714934730681,1.,1.78967092823491));
#62889=CARTESIAN_POINT('Ctrl Pts',(-3.74209880352445,-1.,1.79569757859422));
#62890=CARTESIAN_POINT('Ctrl Pts',(-3.74209880352445,1.,1.79569757859422));
#62891=CARTESIAN_POINT('Ctrl Pts',(-3.74702700875467,-1.,1.8017527148577));
#62892=CARTESIAN_POINT('Ctrl Pts',(-3.74702700875467,1.,1.8017527148577));
#62893=CARTESIAN_POINT('Ctrl Pts',(-3.75193395887977,-1.,1.80783603939617));
#62894=CARTESIAN_POINT('Ctrl Pts',(-3.75193395887977,1.,1.80783603939617));
#62895=CARTESIAN_POINT('Ctrl Pts',(-3.75681965683071,-1.,1.8139472983358));
#62896=CARTESIAN_POINT('Ctrl Pts',(-3.75681965683071,1.,1.8139472983358));
#62897=CARTESIAN_POINT('Ctrl Pts',(-3.76168412707948,-1.,1.82008629694091));
#62898=CARTESIAN_POINT('Ctrl Pts',(-3.76168412707948,1.,1.82008629694091));
#62899=CARTESIAN_POINT('Ctrl Pts',(-3.76652740353775,-1.,1.82625289220915));
#62900=CARTESIAN_POINT('Ctrl Pts',(-3.76652740353775,1.,1.82625289220915));
#62901=CARTESIAN_POINT('Ctrl Pts',(-3.77038509817999,-1.,1.83120816955645));
#62902=CARTESIAN_POINT('Ctrl Pts',(-3.77038509817999,1.,1.83120816955645));
#62903=CARTESIAN_POINT('Ctrl Pts',(-3.77326886064398,-1.,1.83493697934534));
#62904=CARTESIAN_POINT('Ctrl Pts',(-3.77326886064398,1.,1.83493697934534));
#62905=CARTESIAN_POINT('Ctrl Pts',(-3.77518714457833,-1.,1.83742834010626));
#62906=CARTESIAN_POINT('Ctrl Pts',(-3.77518714457833,1.,1.83742834010626));
#62907=CARTESIAN_POINT('Ctrl Pts',(-3.77614523045147,-1.,1.8386753923786));
#62908=CARTESIAN_POINT('Ctrl Pts',(-3.77614523045147,1.,1.8386753923786));
#62909=CARTESIAN_POINT('',(-3.42859860294306,1.,1.5189508286633));
#62910=CARTESIAN_POINT('Ctrl Pts',(-3.42859860294306,-1.,1.5189508286633));
#62911=CARTESIAN_POINT('Ctrl Pts',(-3.42859860294306,-0.666666666666667,
1.5189508286633));
#62912=CARTESIAN_POINT('Ctrl Pts',(-3.42859860294306,-0.333333333333333,
1.5189508286633));
#62913=CARTESIAN_POINT('Ctrl Pts',(-3.42859860294306,0.333333333333333,
1.5189508286633));
#62914=CARTESIAN_POINT('Ctrl Pts',(-3.42859860294306,0.666666666666667,
1.5189508286633));
#62915=CARTESIAN_POINT('Ctrl Pts',(-3.42859860294306,1.,1.5189508286633));
#62916=CARTESIAN_POINT('',(-3.77614523045147,1.,1.8386753923786));
#62917=CARTESIAN_POINT('',(-3.77614523045147,0.,1.8386753923786));
#62918=CARTESIAN_POINT('Ctrl Pts',(-3.42859860294306,1.,1.5189508286633));
#62919=CARTESIAN_POINT('Ctrl Pts',(-3.42864616361875,1.,1.51893924967331));
#62920=CARTESIAN_POINT('Ctrl Pts',(-3.42884302333841,1.,1.5189513329503));
#62921=CARTESIAN_POINT('Ctrl Pts',(-3.42946838852587,1.,1.51914806898491));
#62922=CARTESIAN_POINT('Ctrl Pts',(-3.43101631893414,1.,1.5198144909338));
#62923=CARTESIAN_POINT('Ctrl Pts',(-3.43417156977893,1.,1.52134826724292));
#62924=CARTESIAN_POINT('Ctrl Pts',(-3.4388889597401,1.,1.5237734895035));
#62925=CARTESIAN_POINT('Ctrl Pts',(-3.44469547526647,1.,1.52686242875556));
#62926=CARTESIAN_POINT('Ctrl Pts',(-3.45127136828305,1.,1.53046244461635));
#62927=CARTESIAN_POINT('Ctrl Pts',(-3.45825932955032,1.,1.53440195378792));
#62928=CARTESIAN_POINT('Ctrl Pts',(-3.46531752207153,1.,1.53851507915502));
#62929=CARTESIAN_POINT('Ctrl Pts',(-3.47217189224653,1.,1.54266605398187));
#62930=CARTESIAN_POINT('Ctrl Pts',(-3.47868272898751,1.,1.54678009290276));
#62931=CARTESIAN_POINT('Ctrl Pts',(-3.48485155928567,1.,1.55084702970452));
#62932=CARTESIAN_POINT('Ctrl Pts',(-3.4907646087742,1.,1.55489595901116));
#62933=CARTESIAN_POINT('Ctrl Pts',(-3.49655185179655,1.,1.55897703097874));
#62934=CARTESIAN_POINT('Ctrl Pts',(-3.50234321621578,1.,1.56314187758675));
#62935=CARTESIAN_POINT('Ctrl Pts',(-3.50821771695363,1.,1.56742097575012));
#62936=CARTESIAN_POINT('Ctrl Pts',(-3.51418598431665,1.,1.57181569799743));
#62937=CARTESIAN_POINT('Ctrl Pts',(-3.52021847865912,1.,1.57631049988158));
#62938=CARTESIAN_POINT('Ctrl Pts',(-3.52626275334881,1.,1.58088027227848));
#62939=CARTESIAN_POINT('Ctrl Pts',(-3.5322637814708,1.,1.58549906268088));
#62940=CARTESIAN_POINT('Ctrl Pts',(-3.53818616861077,1.,1.59014958368739));
#62941=CARTESIAN_POINT('Ctrl Pts',(-3.54402458182337,1.,1.59482766949766));
#62942=CARTESIAN_POINT('Ctrl Pts',(-3.54979148634454,1.,1.59953698113457));
#62943=CARTESIAN_POINT('Ctrl Pts',(-3.55550985096129,1.,1.60428584699853));
#62944=CARTESIAN_POINT('Ctrl Pts',(-3.5612043248298,1.,1.60908344685457));
#62945=CARTESIAN_POINT('Ctrl Pts',(-3.56689200468387,1.,1.61393581747514));
#62946=CARTESIAN_POINT('Ctrl Pts',(-3.57257679609806,1.,1.61884340915404));
#62947=CARTESIAN_POINT('Ctrl Pts',(-3.5782545595439,1.,1.62380329464844));
#62948=CARTESIAN_POINT('Ctrl Pts',(-3.58391625774343,1.,1.62881051550745));
#62949=CARTESIAN_POINT('Ctrl Pts',(-3.58955176627879,1.,1.6338597145126));
#62950=CARTESIAN_POINT('Ctrl Pts',(-3.59515368334893,1.,1.63894676675352));
#62951=CARTESIAN_POINT('Ctrl Pts',(-3.60072028513845,1.,1.64407004385582));
#62952=CARTESIAN_POINT('Ctrl Pts',(-3.60625346556992,1.,1.64922952425832));
#62953=CARTESIAN_POINT('Ctrl Pts',(-3.61175734965127,1.,1.65442619244325));
#62954=CARTESIAN_POINT('Ctrl Pts',(-3.61723666482456,1.,1.65966133399186));
#62955=CARTESIAN_POINT('Ctrl Pts',(-3.62269517989109,1.,1.66493585923855));
#62956=CARTESIAN_POINT('Ctrl Pts',(-3.62813422105271,1.,1.67024966008045));
#62957=CARTESIAN_POINT('Ctrl Pts',(-3.63355343201232,1.,1.67560193613156));
#62958=CARTESIAN_POINT('Ctrl Pts',(-3.63895140887462,1.,1.68099146651586));
#62959=CARTESIAN_POINT('Ctrl Pts',(-3.64432638915203,1.,1.68641690471457));
#62960=CARTESIAN_POINT('Ctrl Pts',(-3.64967689827371,1.,1.69187705481689));
#62961=CARTESIAN_POINT('Ctrl Pts',(-3.65500246526749,1.,1.69737117722534));
#62962=CARTESIAN_POINT('Ctrl Pts',(-3.66030338774847,1.,1.70289888566873));
#62963=CARTESIAN_POINT('Ctrl Pts',(-3.66558043198876,1.,1.70846001610956));
#62964=CARTESIAN_POINT('Ctrl Pts',(-3.67083454901611,1.,1.71405450210383));
#62965=CARTESIAN_POINT('Ctrl Pts',(-3.67606660374709,1.,1.71968225581808));
#62966=CARTESIAN_POINT('Ctrl Pts',(-3.68127704936579,1.,1.72534302437056));
#62967=CARTESIAN_POINT('Ctrl Pts',(-3.68646597019332,1.,1.73103640956717));
#62968=CARTESIAN_POINT('Ctrl Pts',(-3.69163322648036,1.,1.73676193254557));
#62969=CARTESIAN_POINT('Ctrl Pts',(-3.69677856910517,1.,1.74251908492617));
#62970=CARTESIAN_POINT('Ctrl Pts',(-3.7019017567335,1.,1.74830738046057));
#62971=CARTESIAN_POINT('Ctrl Pts',(-3.70700269736659,1.,1.75412641804042));
#62972=CARTESIAN_POINT('Ctrl Pts',(-3.71208146346136,1.,1.75997588498865));
#62973=CARTESIAN_POINT('Ctrl Pts',(-3.71713822377359,1.,1.76585552124394));
#62974=CARTESIAN_POINT('Ctrl Pts',(-3.72217319911254,1.,1.77176509401761));
#62975=CARTESIAN_POINT('Ctrl Pts',(-3.72718661205609,1.,1.77770437039658));
#62976=CARTESIAN_POINT('Ctrl Pts',(-3.7321786309547,1.,1.78367308442901));
#62977=CARTESIAN_POINT('Ctrl Pts',(-3.73714934730681,1.,1.78967092823491));
#62978=CARTESIAN_POINT('Ctrl Pts',(-3.74209880352445,1.,1.79569757859422));
#62979=CARTESIAN_POINT('Ctrl Pts',(-3.74702700875467,1.,1.8017527148577));
#62980=CARTESIAN_POINT('Ctrl Pts',(-3.75193395887977,1.,1.80783603939617));
#62981=CARTESIAN_POINT('Ctrl Pts',(-3.75681965683071,1.,1.8139472983358));
#62982=CARTESIAN_POINT('Ctrl Pts',(-3.76168412707948,1.,1.82008629694091));
#62983=CARTESIAN_POINT('Ctrl Pts',(-3.76652740353775,1.,1.82625289220915));
#62984=CARTESIAN_POINT('Ctrl Pts',(-3.77038509817999,1.,1.83120816955645));
#62985=CARTESIAN_POINT('Ctrl Pts',(-3.77326886064398,1.,1.83493697934534));
#62986=CARTESIAN_POINT('Ctrl Pts',(-3.77518714457833,1.,1.83742834010626));
#62987=CARTESIAN_POINT('Ctrl Pts',(-3.77614523045147,1.,1.8386753923786));
#62988=CARTESIAN_POINT('Origin',(-3.77614523045147,0.,1.8386753923786));
#62989=CARTESIAN_POINT('',(-3.70708211654725,1.,1.97421938526992));
#62990=CARTESIAN_POINT('Origin',(0.,0.,0.));
#62991=CARTESIAN_POINT('',(-3.49844575334386,1.,1.35032489087269));
#62992=CARTESIAN_POINT('Origin',(0.,1.,0.));
#62993=CARTESIAN_POINT('Ctrl Pts',(-3.49844575334386,1.,1.35032489087269));
#62994=CARTESIAN_POINT('Ctrl Pts',(-3.49844575334386,0.666666666666667,
1.35032489087269));
#62995=CARTESIAN_POINT('Ctrl Pts',(-3.49844575334386,0.333333333333333,
1.35032489087269));
#62996=CARTESIAN_POINT('Ctrl Pts',(-3.49844575334386,-0.333333333333333,
1.35032489087269));
#62997=CARTESIAN_POINT('Ctrl Pts',(-3.49844575334386,-0.666666666666667,
1.35032489087269));
#62998=CARTESIAN_POINT('Ctrl Pts',(-3.49844575334386,-1.,1.35032489087269));
#62999=CARTESIAN_POINT('Ctrl Pts',(-3.97027773754922,-1.,1.36999806084572));
#63000=CARTESIAN_POINT('Ctrl Pts',(-3.97027773754922,1.,1.36999806084572));
#63001=CARTESIAN_POINT('Ctrl Pts',(-3.9687184694173,-1.,1.37020239094758));
#63002=CARTESIAN_POINT('Ctrl Pts',(-3.9687184694173,1.,1.37020239094758));
#63003=CARTESIAN_POINT('Ctrl Pts',(-3.96560037975788,-1.,1.37060761746027));
#63004=CARTESIAN_POINT('Ctrl Pts',(-3.96560037975788,1.,1.37060761746027));
#63005=CARTESIAN_POINT('Ctrl Pts',(-3.96092458508407,-1.,1.37120515615663));
#63006=CARTESIAN_POINT('Ctrl Pts',(-3.96092458508407,1.,1.37120515615663));
#63007=CARTESIAN_POINT('Ctrl Pts',(-3.95469287283105,-1.,1.37198126433139));
#63008=CARTESIAN_POINT('Ctrl Pts',(-3.95469287283105,1.,1.37198126433139));
#63009=CARTESIAN_POINT('Ctrl Pts',(-3.94690771786926,-1.,1.37291699203423));
#63010=CARTESIAN_POINT('Ctrl Pts',(-3.94690771786926,1.,1.37291699203423));
#63011=CARTESIAN_POINT('Ctrl Pts',(-3.93912709041791,-1.,1.37381821967499));
#63012=CARTESIAN_POINT('Ctrl Pts',(-3.93912709041791,1.,1.37381821967499));
#63013=CARTESIAN_POINT('Ctrl Pts',(-3.93135106761941,-1.,1.37468482215784));
#63014=CARTESIAN_POINT('Ctrl Pts',(-3.93135106761941,1.,1.37468482215784));
#63015=CARTESIAN_POINT('Ctrl Pts',(-3.92357976987132,-1.,1.37551664448057));
#63016=CARTESIAN_POINT('Ctrl Pts',(-3.92357976987132,1.,1.37551664448057));
#63017=CARTESIAN_POINT('Ctrl Pts',(-3.91581337461825,-1.,1.37631350505516));
#63018=CARTESIAN_POINT('Ctrl Pts',(-3.91581337461825,1.,1.37631350505516));
#63019=CARTESIAN_POINT('Ctrl Pts',(-3.90805209522729,-1.,1.3770751963376));
#63020=CARTESIAN_POINT('Ctrl Pts',(-3.90805209522729,1.,1.3770751963376));
#63021=CARTESIAN_POINT('Ctrl Pts',(-3.90029615196255,-1.,1.3778014851263));
#63022=CARTESIAN_POINT('Ctrl Pts',(-3.90029615196255,1.,1.3778014851263));
#63023=CARTESIAN_POINT('Ctrl Pts',(-3.89254574338385,-1.,1.37849211287981));
#63024=CARTESIAN_POINT('Ctrl Pts',(-3.89254574338385,1.,1.37849211287981));
#63025=CARTESIAN_POINT('Ctrl Pts',(-3.88480102249461,-1.,1.37914679719446));
#63026=CARTESIAN_POINT('Ctrl Pts',(-3.88480102249461,1.,1.37914679719446));
#63027=CARTESIAN_POINT('Ctrl Pts',(-3.87706205830865,-1.,1.37976523097187));
#63028=CARTESIAN_POINT('Ctrl Pts',(-3.87706205830865,1.,1.37976523097187));
#63029=CARTESIAN_POINT('Ctrl Pts',(-3.86932885813403,-1.,1.38034709213129));
#63030=CARTESIAN_POINT('Ctrl Pts',(-3.86932885813403,1.,1.38034709213129));
#63031=CARTESIAN_POINT('Ctrl Pts',(-3.86160143044187,-1.,1.38089205993067));
#63032=CARTESIAN_POINT('Ctrl Pts',(-3.86160143044187,1.,1.38089205993067));
#63033=CARTESIAN_POINT('Ctrl Pts',(-3.85387983979557,-1.,1.38139983115075));
#63034=CARTESIAN_POINT('Ctrl Pts',(-3.85387983979557,1.,1.38139983115075));
#63035=CARTESIAN_POINT('Ctrl Pts',(-3.84616425605705,-1.,1.38187013346089));
#63036=CARTESIAN_POINT('Ctrl Pts',(-3.84616425605705,1.,1.38187013346089));
#63037=CARTESIAN_POINT('Ctrl Pts',(-3.83845502790609,-1.,1.38230274828774));
#63038=CARTESIAN_POINT('Ctrl Pts',(-3.83845502790609,1.,1.38230274828774));
#63039=CARTESIAN_POINT('Ctrl Pts',(-3.83075266982138,-1.,1.38269750245086));
#63040=CARTESIAN_POINT('Ctrl Pts',(-3.83075266982138,1.,1.38269750245086));
#63041=CARTESIAN_POINT('Ctrl Pts',(-3.82305771743715,-1.,1.38305421262724));
#63042=CARTESIAN_POINT('Ctrl Pts',(-3.82305771743715,1.,1.38305421262724));
#63043=CARTESIAN_POINT('Ctrl Pts',(-3.81537060817765,-1.,1.38337263902766));
#63044=CARTESIAN_POINT('Ctrl Pts',(-3.81537060817765,1.,1.38337263902766));
#63045=CARTESIAN_POINT('Ctrl Pts',(-3.80769156398429,-1.,1.38365244046226));
#63046=CARTESIAN_POINT('Ctrl Pts',(-3.80769156398429,1.,1.38365244046226));
#63047=CARTESIAN_POINT('Ctrl Pts',(-3.80002044322169,-1.,1.38389311766701));
#63048=CARTESIAN_POINT('Ctrl Pts',(-3.80002044322169,1.,1.38389311766701));
#63049=CARTESIAN_POINT('Ctrl Pts',(-3.79235669640907,-1.,1.38409399694588));
#63050=CARTESIAN_POINT('Ctrl Pts',(-3.79235669640907,1.,1.38409399694588));
#63051=CARTESIAN_POINT('Ctrl Pts',(-3.78469969805134,-1.,1.38425435883773));
#63052=CARTESIAN_POINT('Ctrl Pts',(-3.78469969805134,1.,1.38425435883773));
#63053=CARTESIAN_POINT('Ctrl Pts',(-3.77704902230441,-1.,1.38437354551435));
#63054=CARTESIAN_POINT('Ctrl Pts',(-3.77704902230441,1.,1.38437354551435));
#63055=CARTESIAN_POINT('Ctrl Pts',(-3.76940473185775,-1.,1.38445107339517));
#63056=CARTESIAN_POINT('Ctrl Pts',(-3.76940473185775,1.,1.38445107339517));
#63057=CARTESIAN_POINT('Ctrl Pts',(-3.76176768271347,-1.,1.38448675253343));
#63058=CARTESIAN_POINT('Ctrl Pts',(-3.76176768271347,1.,1.38448675253343));
#63059=CARTESIAN_POINT('Ctrl Pts',(-3.75413976318727,-1.,1.38448077997155));
#63060=CARTESIAN_POINT('Ctrl Pts',(-3.75413976318727,1.,1.38448077997155));
#63061=CARTESIAN_POINT('Ctrl Pts',(-3.7465231716786,-1.,1.38443344984389));
#63062=CARTESIAN_POINT('Ctrl Pts',(-3.7465231716786,1.,1.38443344984389));
#63063=CARTESIAN_POINT('Ctrl Pts',(-3.73891976418099,-1.,1.38434489156456));
#63064=CARTESIAN_POINT('Ctrl Pts',(-3.73891976418099,1.,1.38434489156456));
#63065=CARTESIAN_POINT('Ctrl Pts',(-3.73133035859283,-1.,1.38421479111531));
#63066=CARTESIAN_POINT('Ctrl Pts',(-3.73133035859283,1.,1.38421479111531));
#63067=CARTESIAN_POINT('Ctrl Pts',(-3.72375409358805,-1.,1.3840421342895));
#63068=CARTESIAN_POINT('Ctrl Pts',(-3.72375409358805,1.,1.3840421342895));
#63069=CARTESIAN_POINT('Ctrl Pts',(-3.7161876605181,-1.,1.38382489984585));
#63070=CARTESIAN_POINT('Ctrl Pts',(-3.7161876605181,1.,1.38382489984585));
#63071=CARTESIAN_POINT('Ctrl Pts',(-3.70862680753343,-1.,1.38356065402122));
#63072=CARTESIAN_POINT('Ctrl Pts',(-3.70862680753343,1.,1.38356065402122));
#63073=CARTESIAN_POINT('Ctrl Pts',(-3.70106792167894,-1.,1.38324717612862));
#63074=CARTESIAN_POINT('Ctrl Pts',(-3.70106792167894,1.,1.38324717612862));
#63075=CARTESIAN_POINT('Ctrl Pts',(-3.69350967899523,-1.,1.38288311171649));
#63076=CARTESIAN_POINT('Ctrl Pts',(-3.69350967899523,1.,1.38288311171649));
#63077=CARTESIAN_POINT('Ctrl Pts',(-3.68595444983844,-1.,1.38246852827185));
#63078=CARTESIAN_POINT('Ctrl Pts',(-3.68595444983844,1.,1.38246852827185));
#63079=CARTESIAN_POINT('Ctrl Pts',(-3.6784103848243,-1.,1.38200574290626));
#63080=CARTESIAN_POINT('Ctrl Pts',(-3.6784103848243,1.,1.38200574290626));
#63081=CARTESIAN_POINT('Ctrl Pts',(-3.67088843112282,-1.,1.38149812653876));
#63082=CARTESIAN_POINT('Ctrl Pts',(-3.67088843112282,1.,1.38149812653876));
#63083=CARTESIAN_POINT('Ctrl Pts',(-3.66339848520874,-1.,1.38094856333558));
#63084=CARTESIAN_POINT('Ctrl Pts',(-3.66339848520874,1.,1.38094856333558));
#63085=CARTESIAN_POINT('Ctrl Pts',(-3.65594554404396,-1.,1.38035791051215));
#63086=CARTESIAN_POINT('Ctrl Pts',(-3.65594554404396,1.,1.38035791051215));
#63087=CARTESIAN_POINT('Ctrl Pts',(-3.64852652756444,-1.,1.37972372481598));
#63088=CARTESIAN_POINT('Ctrl Pts',(-3.64852652756444,1.,1.37972372481598));
#63089=CARTESIAN_POINT('Ctrl Pts',(-3.64112507791112,-1.,1.37903818567347));
#63090=CARTESIAN_POINT('Ctrl Pts',(-3.64112507791112,1.,1.37903818567347));
#63091=CARTESIAN_POINT('Ctrl Pts',(-3.63371727442448,-1.,1.37829035457324));
#63092=CARTESIAN_POINT('Ctrl Pts',(-3.63371727442448,1.,1.37829035457324));
#63093=CARTESIAN_POINT('Ctrl Pts',(-3.62628098665112,-1.,1.37746987919868));
#63094=CARTESIAN_POINT('Ctrl Pts',(-3.62628098665112,1.,1.37746987919868));
#63095=CARTESIAN_POINT('Ctrl Pts',(-3.61880481160408,-1.,1.37657053403102));
#63096=CARTESIAN_POINT('Ctrl Pts',(-3.61880481160408,1.,1.37657053403102));
#63097=CARTESIAN_POINT('Ctrl Pts',(-3.61129546591082,-1.,1.37559314436641));
#63098=CARTESIAN_POINT('Ctrl Pts',(-3.61129546591082,1.,1.37559314436641));
#63099=CARTESIAN_POINT('Ctrl Pts',(-3.60379020124038,-1.,1.37455051379642));
#63100=CARTESIAN_POINT('Ctrl Pts',(-3.60379020124038,1.,1.37455051379642));
#63101=CARTESIAN_POINT('Ctrl Pts',(-3.59634627869117,-1.,1.37346320103184));
#63102=CARTESIAN_POINT('Ctrl Pts',(-3.59634627869117,1.,1.37346320103184));
#63103=CARTESIAN_POINT('Ctrl Pts',(-3.5890185384643,-1.,1.37235053661));
#63104=CARTESIAN_POINT('Ctrl Pts',(-3.5890185384643,1.,1.37235053661));
#63105=CARTESIAN_POINT('Ctrl Pts',(-3.58183885982745,-1.,1.37122241663073));
#63106=CARTESIAN_POINT('Ctrl Pts',(-3.58183885982745,1.,1.37122241663073));
#63107=CARTESIAN_POINT('Ctrl Pts',(-3.57479875549453,-1.,1.37007229485646));
#63108=CARTESIAN_POINT('Ctrl Pts',(-3.57479875549453,1.,1.37007229485646));
#63109=CARTESIAN_POINT('Ctrl Pts',(-3.56782080304554,-1.,1.36886584973349));
#63110=CARTESIAN_POINT('Ctrl Pts',(-3.56782080304554,1.,1.36886584973349));
#63111=CARTESIAN_POINT('Ctrl Pts',(-3.56077662028492,-1.,1.36754771771174));
#63112=CARTESIAN_POINT('Ctrl Pts',(-3.56077662028492,1.,1.36754771771174));
#63113=CARTESIAN_POINT('Ctrl Pts',(-3.55353883995793,-1.,1.36606145456711));
#63114=CARTESIAN_POINT('Ctrl Pts',(-3.55353883995793,1.,1.36606145456711));
#63115=CARTESIAN_POINT('Ctrl Pts',(-3.54602591832893,-1.,1.36436666257567));
#63116=CARTESIAN_POINT('Ctrl Pts',(-3.54602591832893,1.,1.36436666257567));
#63117=CARTESIAN_POINT('Ctrl Pts',(-3.53824396425032,-1.,1.36245507339334));
#63118=CARTESIAN_POINT('Ctrl Pts',(-3.53824396425032,1.,1.36245507339334));
#63119=CARTESIAN_POINT('Ctrl Pts',(-3.53034464961849,-1.,1.36037259643827));
#63120=CARTESIAN_POINT('Ctrl Pts',(-3.53034464961849,1.,1.36037259643827));
#63121=CARTESIAN_POINT('Ctrl Pts',(-3.52261776117121,-1.,1.35821701528975));
#63122=CARTESIAN_POINT('Ctrl Pts',(-3.52261776117121,1.,1.35821701528975));
#63123=CARTESIAN_POINT('Ctrl Pts',(-3.51542230699919,-1.,1.35611275237288));
#63124=CARTESIAN_POINT('Ctrl Pts',(-3.51542230699919,1.,1.35611275237288));
#63125=CARTESIAN_POINT('Ctrl Pts',(-3.50913227060177,-1.,1.35419113576022));
#63126=CARTESIAN_POINT('Ctrl Pts',(-3.50913227060177,1.,1.35419113576022));
#63127=CARTESIAN_POINT('Ctrl Pts',(-3.50408168106113,-1.,1.3525703284343));
#63128=CARTESIAN_POINT('Ctrl Pts',(-3.50408168106113,1.,1.3525703284343));
#63129=CARTESIAN_POINT('Ctrl Pts',(-3.50049707063673,-1.,1.35133076331065));
#63130=CARTESIAN_POINT('Ctrl Pts',(-3.50049707063673,1.,1.35133076331065));
#63131=CARTESIAN_POINT('Ctrl Pts',(-3.49888720256612,-1.,1.35067437417289));
#63132=CARTESIAN_POINT('Ctrl Pts',(-3.49888720256612,1.,1.35067437417289));
#63133=CARTESIAN_POINT('Ctrl Pts',(-3.49840357193384,-1.,1.35037650302887));
#63134=CARTESIAN_POINT('Ctrl Pts',(-3.49840357193384,1.,1.35037650302887));
#63135=CARTESIAN_POINT('Ctrl Pts',(-3.49840260053616,-1.,1.35026426118351));
#63136=CARTESIAN_POINT('Ctrl Pts',(-3.49840260053616,1.,1.35026426118351));
#63137=CARTESIAN_POINT('Ctrl Pts',(-3.49848248301936,-1.,1.35022972712301));
#63138=CARTESIAN_POINT('Ctrl Pts',(-3.49848248301936,1.,1.35022972712301));
#63139=CARTESIAN_POINT('',(-3.97027773754922,1.,1.36999806084572));
#63140=CARTESIAN_POINT('Ctrl Pts',(-3.97027773754922,1.,1.36999806084572));
#63141=CARTESIAN_POINT('Ctrl Pts',(-3.9687184694173,1.,1.37020239094758));
#63142=CARTESIAN_POINT('Ctrl Pts',(-3.96560037975788,1.,1.37060761746027));
#63143=CARTESIAN_POINT('Ctrl Pts',(-3.96092458508407,1.,1.37120515615663));
#63144=CARTESIAN_POINT('Ctrl Pts',(-3.95469287283105,1.,1.37198126433139));
#63145=CARTESIAN_POINT('Ctrl Pts',(-3.94690771786926,1.,1.37291699203423));
#63146=CARTESIAN_POINT('Ctrl Pts',(-3.93912709041791,1.,1.37381821967499));
#63147=CARTESIAN_POINT('Ctrl Pts',(-3.93135106761941,1.,1.37468482215784));
#63148=CARTESIAN_POINT('Ctrl Pts',(-3.92357976987132,1.,1.37551664448057));
#63149=CARTESIAN_POINT('Ctrl Pts',(-3.91581337461825,1.,1.37631350505516));
#63150=CARTESIAN_POINT('Ctrl Pts',(-3.90805209522729,1.,1.3770751963376));
#63151=CARTESIAN_POINT('Ctrl Pts',(-3.90029615196255,1.,1.3778014851263));
#63152=CARTESIAN_POINT('Ctrl Pts',(-3.89254574338385,1.,1.37849211287981));
#63153=CARTESIAN_POINT('Ctrl Pts',(-3.88480102249461,1.,1.37914679719446));
#63154=CARTESIAN_POINT('Ctrl Pts',(-3.87706205830865,1.,1.37976523097187));
#63155=CARTESIAN_POINT('Ctrl Pts',(-3.86932885813403,1.,1.38034709213129));
#63156=CARTESIAN_POINT('Ctrl Pts',(-3.86160143044187,1.,1.38089205993067));
#63157=CARTESIAN_POINT('Ctrl Pts',(-3.85387983979557,1.,1.38139983115075));
#63158=CARTESIAN_POINT('Ctrl Pts',(-3.84616425605705,1.,1.38187013346089));
#63159=CARTESIAN_POINT('Ctrl Pts',(-3.83845502790609,1.,1.38230274828774));
#63160=CARTESIAN_POINT('Ctrl Pts',(-3.83075266982138,1.,1.38269750245086));
#63161=CARTESIAN_POINT('Ctrl Pts',(-3.82305771743715,1.,1.38305421262724));
#63162=CARTESIAN_POINT('Ctrl Pts',(-3.81537060817765,1.,1.38337263902766));
#63163=CARTESIAN_POINT('Ctrl Pts',(-3.80769156398429,1.,1.38365244046226));
#63164=CARTESIAN_POINT('Ctrl Pts',(-3.80002044322169,1.,1.38389311766701));
#63165=CARTESIAN_POINT('Ctrl Pts',(-3.79235669640907,1.,1.38409399694588));
#63166=CARTESIAN_POINT('Ctrl Pts',(-3.78469969805134,1.,1.38425435883773));
#63167=CARTESIAN_POINT('Ctrl Pts',(-3.77704902230441,1.,1.38437354551435));
#63168=CARTESIAN_POINT('Ctrl Pts',(-3.76940473185775,1.,1.38445107339517));
#63169=CARTESIAN_POINT('Ctrl Pts',(-3.76176768271347,1.,1.38448675253343));
#63170=CARTESIAN_POINT('Ctrl Pts',(-3.75413976318727,1.,1.38448077997155));
#63171=CARTESIAN_POINT('Ctrl Pts',(-3.7465231716786,1.,1.38443344984389));
#63172=CARTESIAN_POINT('Ctrl Pts',(-3.73891976418099,1.,1.38434489156456));
#63173=CARTESIAN_POINT('Ctrl Pts',(-3.73133035859283,1.,1.38421479111531));
#63174=CARTESIAN_POINT('Ctrl Pts',(-3.72375409358805,1.,1.3840421342895));
#63175=CARTESIAN_POINT('Ctrl Pts',(-3.7161876605181,1.,1.38382489984585));
#63176=CARTESIAN_POINT('Ctrl Pts',(-3.70862680753343,1.,1.38356065402122));
#63177=CARTESIAN_POINT('Ctrl Pts',(-3.70106792167894,1.,1.38324717612862));
#63178=CARTESIAN_POINT('Ctrl Pts',(-3.69350967899523,1.,1.38288311171649));
#63179=CARTESIAN_POINT('Ctrl Pts',(-3.68595444983844,1.,1.38246852827185));
#63180=CARTESIAN_POINT('Ctrl Pts',(-3.6784103848243,1.,1.38200574290626));
#63181=CARTESIAN_POINT('Ctrl Pts',(-3.67088843112282,1.,1.38149812653876));
#63182=CARTESIAN_POINT('Ctrl Pts',(-3.66339848520874,1.,1.38094856333558));
#63183=CARTESIAN_POINT('Ctrl Pts',(-3.65594554404396,1.,1.38035791051215));
#63184=CARTESIAN_POINT('Ctrl Pts',(-3.64852652756444,1.,1.37972372481598));
#63185=CARTESIAN_POINT('Ctrl Pts',(-3.64112507791112,1.,1.37903818567347));
#63186=CARTESIAN_POINT('Ctrl Pts',(-3.63371727442448,1.,1.37829035457324));
#63187=CARTESIAN_POINT('Ctrl Pts',(-3.62628098665112,1.,1.37746987919868));
#63188=CARTESIAN_POINT('Ctrl Pts',(-3.61880481160408,1.,1.37657053403102));
#63189=CARTESIAN_POINT('Ctrl Pts',(-3.61129546591082,1.,1.37559314436641));
#63190=CARTESIAN_POINT('Ctrl Pts',(-3.60379020124038,1.,1.37455051379642));
#63191=CARTESIAN_POINT('Ctrl Pts',(-3.59634627869117,1.,1.37346320103184));
#63192=CARTESIAN_POINT('Ctrl Pts',(-3.5890185384643,1.,1.37235053661));
#63193=CARTESIAN_POINT('Ctrl Pts',(-3.58183885982745,1.,1.37122241663073));
#63194=CARTESIAN_POINT('Ctrl Pts',(-3.57479875549453,1.,1.37007229485646));
#63195=CARTESIAN_POINT('Ctrl Pts',(-3.56782080304554,1.,1.36886584973349));
#63196=CARTESIAN_POINT('Ctrl Pts',(-3.56077662028492,1.,1.36754771771174));
#63197=CARTESIAN_POINT('Ctrl Pts',(-3.55353883995793,1.,1.36606145456711));
#63198=CARTESIAN_POINT('Ctrl Pts',(-3.54602591832893,1.,1.36436666257567));
#63199=CARTESIAN_POINT('Ctrl Pts',(-3.53824396425032,1.,1.36245507339334));
#63200=CARTESIAN_POINT('Ctrl Pts',(-3.53034464961849,1.,1.36037259643827));
#63201=CARTESIAN_POINT('Ctrl Pts',(-3.52261776117121,1.,1.35821701528975));
#63202=CARTESIAN_POINT('Ctrl Pts',(-3.51542230699919,1.,1.35611275237288));
#63203=CARTESIAN_POINT('Ctrl Pts',(-3.50913227060177,1.,1.35419113576022));
#63204=CARTESIAN_POINT('Ctrl Pts',(-3.50408168106113,1.,1.3525703284343));
#63205=CARTESIAN_POINT('Ctrl Pts',(-3.5007660381658,1.,1.35142377279535));
#63206=CARTESIAN_POINT('Ctrl Pts',(-3.49920025459856,1.,1.35080045218652));
#63207=CARTESIAN_POINT('Ctrl Pts',(-3.49861894124915,1.,1.35049736560633));
#63208=CARTESIAN_POINT('Ctrl Pts',(-3.49847119623841,1.,1.35036670893102));
#63209=CARTESIAN_POINT('Ctrl Pts',(-3.49844575334386,1.,1.35032489087269));
#63210=CARTESIAN_POINT('',(-3.97027773754922,0.,1.36999806084572));
#63211=CARTESIAN_POINT('Ctrl Pts',(-3.62397690409552,-1.,0.96399761336957));
#63212=CARTESIAN_POINT('Ctrl Pts',(-3.62397690409552,1.,0.96399761336957));
#63213=CARTESIAN_POINT('Ctrl Pts',(-3.62393257642191,-1.,0.963922720982576));
#63214=CARTESIAN_POINT('Ctrl Pts',(-3.62393257642191,1.,0.963922720982576));
#63215=CARTESIAN_POINT('Ctrl Pts',(-3.62399933640277,-1.,0.963832486396055));
#63216=CARTESIAN_POINT('Ctrl Pts',(-3.62399933640277,1.,0.963832486396055));
#63217=CARTESIAN_POINT('Ctrl Pts',(-3.62456568607055,-1.,0.963875774532102));
#63218=CARTESIAN_POINT('Ctrl Pts',(-3.62456568607055,1.,0.963875774532102));
#63219=CARTESIAN_POINT('Ctrl Pts',(-3.62625391255277,-1.,0.964291001274618));
#63220=CARTESIAN_POINT('Ctrl Pts',(-3.62625391255277,1.,0.964291001274618));
#63221=CARTESIAN_POINT('Ctrl Pts',(-3.62988252139998,-1.,0.965395153165716));
#63222=CARTESIAN_POINT('Ctrl Pts',(-3.62988252139998,1.,0.965395153165716));
#63223=CARTESIAN_POINT('Ctrl Pts',(-3.6349212208096,-1.,0.967052554540877));
#63224=CARTESIAN_POINT('Ctrl Pts',(-3.6349212208096,1.,0.967052554540877));
#63225=CARTESIAN_POINT('Ctrl Pts',(-3.64113946505393,-1.,0.969195124674829));
#63226=CARTESIAN_POINT('Ctrl Pts',(-3.64113946505393,1.,0.969195124674829));
#63227=CARTESIAN_POINT('Ctrl Pts',(-3.64819756447072,-1.,0.971722122060277));
#63228=CARTESIAN_POINT('Ctrl Pts',(-3.64819756447072,1.,0.971722122060277));
#63229=CARTESIAN_POINT('Ctrl Pts',(-3.6557157673487,-1.,0.974519971354138));
#63230=CARTESIAN_POINT('Ctrl Pts',(-3.6557157673487,1.,0.974519971354138));
#63231=CARTESIAN_POINT('Ctrl Pts',(-3.66333049637403,-1.,0.977478312751416));
#63232=CARTESIAN_POINT('Ctrl Pts',(-3.66333049637403,1.,0.977478312751416));
#63233=CARTESIAN_POINT('Ctrl Pts',(-3.67074983340444,-1.,0.980505922458494));
#63234=CARTESIAN_POINT('Ctrl Pts',(-3.67074983340444,1.,0.980505922458494));
#63235=CARTESIAN_POINT('Ctrl Pts',(-3.67782408841876,-1.,0.983550791470864));
#63236=CARTESIAN_POINT('Ctrl Pts',(-3.67782408841876,1.,0.983550791470864));
#63237=CARTESIAN_POINT('Ctrl Pts',(-3.6845531792623,-1.,0.986602639864285));
#63238=CARTESIAN_POINT('Ctrl Pts',(-3.6845531792623,1.,0.986602639864285));
#63239=CARTESIAN_POINT('Ctrl Pts',(-3.69102682138955,-1.,0.989676715398858));
#63240=CARTESIAN_POINT('Ctrl Pts',(-3.69102682138955,1.,0.989676715398858));
#63241=CARTESIAN_POINT('Ctrl Pts',(-3.69738123415696,-1.,0.992802218332103));
#63242=CARTESIAN_POINT('Ctrl Pts',(-3.69738123415696,1.,0.992802218332103));
#63243=CARTESIAN_POINT('Ctrl Pts',(-3.70375282282107,-1.,0.996009819772431));
#63244=CARTESIAN_POINT('Ctrl Pts',(-3.70375282282107,1.,0.996009819772431));
#63245=CARTESIAN_POINT('Ctrl Pts',(-3.7102243971387,-1.,0.999317260756344));
#63246=CARTESIAN_POINT('Ctrl Pts',(-3.7102243971387,1.,0.999317260756344));
#63247=CARTESIAN_POINT('Ctrl Pts',(-3.71680667125047,-1.,1.00272423396802));
#63248=CARTESIAN_POINT('Ctrl Pts',(-3.71680667125047,1.,1.00272423396802));
#63249=CARTESIAN_POINT('Ctrl Pts',(-3.72346803750544,-1.,1.00622000735696));
#63250=CARTESIAN_POINT('Ctrl Pts',(-3.72346803750544,1.,1.00622000735696));
#63251=CARTESIAN_POINT('Ctrl Pts',(-3.73015276704407,-1.,1.00978798539491));
#63252=CARTESIAN_POINT('Ctrl Pts',(-3.73015276704407,1.,1.00978798539491));
#63253=CARTESIAN_POINT('Ctrl Pts',(-3.73680245055747,-1.,1.01341114319906));
#63254=CARTESIAN_POINT('Ctrl Pts',(-3.73680245055747,1.,1.01341114319906));
#63255=CARTESIAN_POINT('Ctrl Pts',(-3.74337942504993,-1.,1.01707794311088));
#63256=CARTESIAN_POINT('Ctrl Pts',(-3.74337942504993,1.,1.01707794311088));
#63257=CARTESIAN_POINT('Ctrl Pts',(-3.74987777155873,-1.,1.02078510487439));
#63258=CARTESIAN_POINT('Ctrl Pts',(-3.74987777155873,1.,1.02078510487439));
#63259=CARTESIAN_POINT('Ctrl Pts',(-3.75631037456224,-1.,1.02453429444668));
#63260=CARTESIAN_POINT('Ctrl Pts',(-3.75631037456224,1.,1.02453429444668));
#63261=CARTESIAN_POINT('Ctrl Pts',(-3.76270122291245,-1.,1.02833014458184));
#63262=CARTESIAN_POINT('Ctrl Pts',(-3.76270122291245,1.,1.02833014458184));
#63263=CARTESIAN_POINT('Ctrl Pts',(-3.76907609832516,-1.,1.03217786604919));
#63264=CARTESIAN_POINT('Ctrl Pts',(-3.76907609832516,1.,1.03217786604919));
#63265=CARTESIAN_POINT('Ctrl Pts',(-3.77545283140427,-1.,1.03608074678008));
#63266=CARTESIAN_POINT('Ctrl Pts',(-3.77545283140427,1.,1.03608074678008));
#63267=CARTESIAN_POINT('Ctrl Pts',(-3.7818353500817,-1.,1.04003862055798));
#63268=CARTESIAN_POINT('Ctrl Pts',(-3.7818353500817,1.,1.04003862055798));
#63269=CARTESIAN_POINT('Ctrl Pts',(-3.78821910787179,-1.,1.04404924374422));
#63270=CARTESIAN_POINT('Ctrl Pts',(-3.78821910787179,1.,1.04404924374422));
#63271=CARTESIAN_POINT('Ctrl Pts',(-3.79459440308786,-1.,1.04810913267639));
#63272=CARTESIAN_POINT('Ctrl Pts',(-3.79459440308786,1.,1.04810913267639));
#63273=CARTESIAN_POINT('Ctrl Pts',(-3.80095039790681,-1.,1.05221457990016));
#63274=CARTESIAN_POINT('Ctrl Pts',(-3.80095039790681,1.,1.05221457990016));
#63275=CARTESIAN_POINT('Ctrl Pts',(-3.80727913637791,-1.,1.05636266918644));
#63276=CARTESIAN_POINT('Ctrl Pts',(-3.80727913637791,1.,1.05636266918644));
#63277=CARTESIAN_POINT('Ctrl Pts',(-3.8135786611749,-1.,1.06055206187299));
#63278=CARTESIAN_POINT('Ctrl Pts',(-3.8135786611749,1.,1.06055206187299));
#63279=CARTESIAN_POINT('Ctrl Pts',(-3.81985083953012,-1.,1.0647824403893));
#63280=CARTESIAN_POINT('Ctrl Pts',(-3.81985083953012,1.,1.0647824403893));
#63281=CARTESIAN_POINT('Ctrl Pts',(-3.82609989967276,-1.,1.06905413180359));
#63282=CARTESIAN_POINT('Ctrl Pts',(-3.82609989967276,1.,1.06905413180359));
#63283=CARTESIAN_POINT('Ctrl Pts',(-3.83233071195144,-1.,1.07336766633459));
#63284=CARTESIAN_POINT('Ctrl Pts',(-3.83233071195144,1.,1.07336766633459));
#63285=CARTESIAN_POINT('Ctrl Pts',(-3.83854714117491,-1.,1.07772335353858));
#63286=CARTESIAN_POINT('Ctrl Pts',(-3.83854714117491,1.,1.07772335353858));
#63287=CARTESIAN_POINT('Ctrl Pts',(-3.8447504803063,-1.,1.08212087917991));
#63288=CARTESIAN_POINT('Ctrl Pts',(-3.8447504803063,1.,1.08212087917991));
#63289=CARTESIAN_POINT('Ctrl Pts',(-3.85094025222713,-1.,1.08655950846384));
#63290=CARTESIAN_POINT('Ctrl Pts',(-3.85094025222713,1.,1.08655950846384));
#63291=CARTESIAN_POINT('Ctrl Pts',(-3.85711487933931,-1.,1.09103825516294));
#63292=CARTESIAN_POINT('Ctrl Pts',(-3.85711487933931,1.,1.09103825516294));
#63293=CARTESIAN_POINT('Ctrl Pts',(-3.86327241021247,-1.,1.09555606505013));
#63294=CARTESIAN_POINT('Ctrl Pts',(-3.86327241021247,1.,1.09555606505013));
#63295=CARTESIAN_POINT('Ctrl Pts',(-3.86941120134849,-1.,1.10011198761195));
#63296=CARTESIAN_POINT('Ctrl Pts',(-3.86941120134849,1.,1.10011198761195));
#63297=CARTESIAN_POINT('Ctrl Pts',(-3.87553067187514,-1.,1.10470536603287));
#63298=CARTESIAN_POINT('Ctrl Pts',(-3.87553067187514,1.,1.10470536603287));
#63299=CARTESIAN_POINT('Ctrl Pts',(-3.88163105531724,-1.,1.10933577224008));
#63300=CARTESIAN_POINT('Ctrl Pts',(-3.88163105531724,1.,1.10933577224008));
#63301=CARTESIAN_POINT('Ctrl Pts',(-3.88771308285171,-1.,1.11400292434429));
#63302=CARTESIAN_POINT('Ctrl Pts',(-3.88771308285171,1.,1.11400292434429));
#63303=CARTESIAN_POINT('Ctrl Pts',(-3.89377768340344,-1.,1.11870660794603));
#63304=CARTESIAN_POINT('Ctrl Pts',(-3.89377768340344,1.,1.11870660794603));
#63305=CARTESIAN_POINT('Ctrl Pts',(-3.89982569750025,-1.,1.12344660099043));
#63306=CARTESIAN_POINT('Ctrl Pts',(-3.89982569750025,1.,1.12344660099043));
#63307=CARTESIAN_POINT('Ctrl Pts',(-3.90585753318737,-1.,1.12822258281553));
#63308=CARTESIAN_POINT('Ctrl Pts',(-3.90585753318737,1.,1.12822258281553));
#63309=CARTESIAN_POINT('Ctrl Pts',(-3.91187321145649,-1.,1.13303414693896));
#63310=CARTESIAN_POINT('Ctrl Pts',(-3.91187321145649,1.,1.13303414693896));
#63311=CARTESIAN_POINT('Ctrl Pts',(-3.91787251936827,-1.,1.13788084225554));
#63312=CARTESIAN_POINT('Ctrl Pts',(-3.91787251936827,1.,1.13788084225554));
#63313=CARTESIAN_POINT('Ctrl Pts',(-3.92385513133997,-1.,1.14276220561593));
#63314=CARTESIAN_POINT('Ctrl Pts',(-3.92385513133997,1.,1.14276220561593));
#63315=CARTESIAN_POINT('Ctrl Pts',(-3.92982073294257,-1.,1.14767779451123));
#63316=CARTESIAN_POINT('Ctrl Pts',(-3.92982073294257,1.,1.14767779451123));
#63317=CARTESIAN_POINT('Ctrl Pts',(-3.9357691705628,-1.,1.1526272271632));
#63318=CARTESIAN_POINT('Ctrl Pts',(-3.9357691705628,1.,1.1526272271632));
#63319=CARTESIAN_POINT('Ctrl Pts',(-3.94170046685203,-1.,1.15761018340956));
#63320=CARTESIAN_POINT('Ctrl Pts',(-3.94170046685203,1.,1.15761018340956));
#63321=CARTESIAN_POINT('Ctrl Pts',(-3.94761474780583,-1.,1.16262637999157));
#63322=CARTESIAN_POINT('Ctrl Pts',(-3.94761474780583,1.,1.16262637999157));
#63323=CARTESIAN_POINT('Ctrl Pts',(-3.95351219509876,-1.,1.16767555244438));
#63324=CARTESIAN_POINT('Ctrl Pts',(-3.95351219509876,1.,1.16767555244438));
#63325=CARTESIAN_POINT('Ctrl Pts',(-3.95939299213276,-1.,1.17275743590361));
#63326=CARTESIAN_POINT('Ctrl Pts',(-3.95939299213276,1.,1.17275743590361));
#63327=CARTESIAN_POINT('Ctrl Pts',(-3.96525726358159,-1.,1.17787174135592));
#63328=CARTESIAN_POINT('Ctrl Pts',(-3.96525726358159,1.,1.17787174135592));
#63329=CARTESIAN_POINT('Ctrl Pts',(-3.97110505165415,-1.,1.18301815039831));
#63330=CARTESIAN_POINT('Ctrl Pts',(-3.97110505165415,1.,1.18301815039831));
#63331=CARTESIAN_POINT('Ctrl Pts',(-3.97693634767754,-1.,1.18819633715539));
#63332=CARTESIAN_POINT('Ctrl Pts',(-3.97693634767754,1.,1.18819633715539));
#63333=CARTESIAN_POINT('Ctrl Pts',(-3.98275111052561,-1.,1.19340598349475));
#63334=CARTESIAN_POINT('Ctrl Pts',(-3.98275111052561,1.,1.19340598349475));
#63335=CARTESIAN_POINT('Ctrl Pts',(-3.98854928957189,-1.,1.19864679609566));
#63336=CARTESIAN_POINT('Ctrl Pts',(-3.98854928957189,1.,1.19864679609566));
#63337=CARTESIAN_POINT('Ctrl Pts',(-3.99433084799666,-1.,1.20391852375139));
#63338=CARTESIAN_POINT('Ctrl Pts',(-3.99433084799666,1.,1.20391852375139));
#63339=CARTESIAN_POINT('Ctrl Pts',(-4.00009577950721,-1.,1.20922097029551));
#63340=CARTESIAN_POINT('Ctrl Pts',(-4.00009577950721,1.,1.20922097029551));
#63341=CARTESIAN_POINT('Ctrl Pts',(-4.00584409522722,-1.,1.21455398918133));
#63342=CARTESIAN_POINT('Ctrl Pts',(-4.00584409522722,1.,1.21455398918133));
#63343=CARTESIAN_POINT('Ctrl Pts',(-4.01042947140789,-1.,1.21884478244403));
#63344=CARTESIAN_POINT('Ctrl Pts',(-4.01042947140789,1.,1.21884478244403));
#63345=CARTESIAN_POINT('Ctrl Pts',(-4.01386104433519,-1.,1.22207656455845));
#63346=CARTESIAN_POINT('Ctrl Pts',(-4.01386104433519,1.,1.22207656455845));
#63347=CARTESIAN_POINT('Ctrl Pts',(-4.01614544569895,-1.,1.22423716681317));
#63348=CARTESIAN_POINT('Ctrl Pts',(-4.01614544569895,1.,1.22423716681317));
#63349=CARTESIAN_POINT('Ctrl Pts',(-4.01728681790024,-1.,1.22531898815164));
#63350=CARTESIAN_POINT('Ctrl Pts',(-4.01728681790024,1.,1.22531898815164));
#63351=CARTESIAN_POINT('',(-3.62400312501199,1.,0.963899035118986));
#63352=CARTESIAN_POINT('Ctrl Pts',(-3.62400312501199,-1.,0.963899035118986));
#63353=CARTESIAN_POINT('Ctrl Pts',(-3.62400312501199,-0.666666666666667,
0.963899035118986));
#63354=CARTESIAN_POINT('Ctrl Pts',(-3.62400312501199,-0.333333333333333,
0.963899035118986));
#63355=CARTESIAN_POINT('Ctrl Pts',(-3.62400312501199,0.333333333333333,
0.963899035118986));
#63356=CARTESIAN_POINT('Ctrl Pts',(-3.62400312501199,0.666666666666667,
0.963899035118985));
#63357=CARTESIAN_POINT('Ctrl Pts',(-3.62400312501199,1.,0.963899035118985));
#63358=CARTESIAN_POINT('',(-4.01728681790024,1.,1.22531898815164));
#63359=CARTESIAN_POINT('',(-4.01728681790024,0.,1.22531898815164));
#63360=CARTESIAN_POINT('Ctrl Pts',(-3.62400312501199,1.,0.963899035118985));
#63361=CARTESIAN_POINT('Ctrl Pts',(-3.62404828878374,1.,0.963880158556713));
#63362=CARTESIAN_POINT('Ctrl Pts',(-3.62424461507455,1.,0.963861297423579));
#63363=CARTESIAN_POINT('Ctrl Pts',(-3.62489305727516,1.,0.963957782642589));
#63364=CARTESIAN_POINT('Ctrl Pts',(-3.62652618145252,1.,0.964373850166081));
#63365=CARTESIAN_POINT('Ctrl Pts',(-3.62988252139998,1.,0.965395153165716));
#63366=CARTESIAN_POINT('Ctrl Pts',(-3.6349212208096,1.,0.967052554540877));
#63367=CARTESIAN_POINT('Ctrl Pts',(-3.64113946505393,1.,0.969195124674829));
#63368=CARTESIAN_POINT('Ctrl Pts',(-3.64819756447072,1.,0.971722122060277));
#63369=CARTESIAN_POINT('Ctrl Pts',(-3.6557157673487,1.,0.974519971354138));
#63370=CARTESIAN_POINT('Ctrl Pts',(-3.66333049637403,1.,0.977478312751416));
#63371=CARTESIAN_POINT('Ctrl Pts',(-3.67074983340444,1.,0.980505922458494));
#63372=CARTESIAN_POINT('Ctrl Pts',(-3.67782408841876,1.,0.983550791470864));
#63373=CARTESIAN_POINT('Ctrl Pts',(-3.6845531792623,1.,0.986602639864285));
#63374=CARTESIAN_POINT('Ctrl Pts',(-3.69102682138955,1.,0.989676715398858));
#63375=CARTESIAN_POINT('Ctrl Pts',(-3.69738123415696,1.,0.992802218332103));
#63376=CARTESIAN_POINT('Ctrl Pts',(-3.70375282282107,1.,0.996009819772431));
#63377=CARTESIAN_POINT('Ctrl Pts',(-3.7102243971387,1.,0.999317260756344));
#63378=CARTESIAN_POINT('Ctrl Pts',(-3.71680667125047,1.,1.00272423396802));
#63379=CARTESIAN_POINT('Ctrl Pts',(-3.72346803750544,1.,1.00622000735696));
#63380=CARTESIAN_POINT('Ctrl Pts',(-3.73015276704407,1.,1.00978798539491));
#63381=CARTESIAN_POINT('Ctrl Pts',(-3.73680245055747,1.,1.01341114319906));
#63382=CARTESIAN_POINT('Ctrl Pts',(-3.74337942504993,1.,1.01707794311088));
#63383=CARTESIAN_POINT('Ctrl Pts',(-3.74987777155873,1.,1.02078510487439));
#63384=CARTESIAN_POINT('Ctrl Pts',(-3.75631037456224,1.,1.02453429444668));
#63385=CARTESIAN_POINT('Ctrl Pts',(-3.76270122291245,1.,1.02833014458184));
#63386=CARTESIAN_POINT('Ctrl Pts',(-3.76907609832516,1.,1.03217786604919));
#63387=CARTESIAN_POINT('Ctrl Pts',(-3.77545283140427,1.,1.03608074678008));
#63388=CARTESIAN_POINT('Ctrl Pts',(-3.7818353500817,1.,1.04003862055798));
#63389=CARTESIAN_POINT('Ctrl Pts',(-3.78821910787179,1.,1.04404924374422));
#63390=CARTESIAN_POINT('Ctrl Pts',(-3.79459440308786,1.,1.04810913267639));
#63391=CARTESIAN_POINT('Ctrl Pts',(-3.80095039790681,1.,1.05221457990016));
#63392=CARTESIAN_POINT('Ctrl Pts',(-3.80727913637791,1.,1.05636266918644));
#63393=CARTESIAN_POINT('Ctrl Pts',(-3.8135786611749,1.,1.06055206187299));
#63394=CARTESIAN_POINT('Ctrl Pts',(-3.81985083953012,1.,1.0647824403893));
#63395=CARTESIAN_POINT('Ctrl Pts',(-3.82609989967276,1.,1.06905413180359));
#63396=CARTESIAN_POINT('Ctrl Pts',(-3.83233071195144,1.,1.07336766633459));
#63397=CARTESIAN_POINT('Ctrl Pts',(-3.83854714117491,1.,1.07772335353858));
#63398=CARTESIAN_POINT('Ctrl Pts',(-3.8447504803063,1.,1.08212087917991));
#63399=CARTESIAN_POINT('Ctrl Pts',(-3.85094025222713,1.,1.08655950846384));
#63400=CARTESIAN_POINT('Ctrl Pts',(-3.85711487933931,1.,1.09103825516294));
#63401=CARTESIAN_POINT('Ctrl Pts',(-3.86327241021247,1.,1.09555606505013));
#63402=CARTESIAN_POINT('Ctrl Pts',(-3.86941120134849,1.,1.10011198761195));
#63403=CARTESIAN_POINT('Ctrl Pts',(-3.87553067187514,1.,1.10470536603287));
#63404=CARTESIAN_POINT('Ctrl Pts',(-3.88163105531724,1.,1.10933577224008));
#63405=CARTESIAN_POINT('Ctrl Pts',(-3.88771308285171,1.,1.11400292434429));
#63406=CARTESIAN_POINT('Ctrl Pts',(-3.89377768340344,1.,1.11870660794603));
#63407=CARTESIAN_POINT('Ctrl Pts',(-3.89982569750025,1.,1.12344660099043));
#63408=CARTESIAN_POINT('Ctrl Pts',(-3.90585753318737,1.,1.12822258281553));
#63409=CARTESIAN_POINT('Ctrl Pts',(-3.91187321145649,1.,1.13303414693896));
#63410=CARTESIAN_POINT('Ctrl Pts',(-3.91787251936827,1.,1.13788084225554));
#63411=CARTESIAN_POINT('Ctrl Pts',(-3.92385513133997,1.,1.14276220561593));
#63412=CARTESIAN_POINT('Ctrl Pts',(-3.92982073294257,1.,1.14767779451123));
#63413=CARTESIAN_POINT('Ctrl Pts',(-3.9357691705628,1.,1.1526272271632));
#63414=CARTESIAN_POINT('Ctrl Pts',(-3.94170046685203,1.,1.15761018340956));
#63415=CARTESIAN_POINT('Ctrl Pts',(-3.94761474780583,1.,1.16262637999157));
#63416=CARTESIAN_POINT('Ctrl Pts',(-3.95351219509876,1.,1.16767555244438));
#63417=CARTESIAN_POINT('Ctrl Pts',(-3.95939299213276,1.,1.17275743590361));
#63418=CARTESIAN_POINT('Ctrl Pts',(-3.96525726358159,1.,1.17787174135592));
#63419=CARTESIAN_POINT('Ctrl Pts',(-3.97110505165415,1.,1.18301815039831));
#63420=CARTESIAN_POINT('Ctrl Pts',(-3.97693634767754,1.,1.18819633715539));
#63421=CARTESIAN_POINT('Ctrl Pts',(-3.98275111052561,1.,1.19340598349475));
#63422=CARTESIAN_POINT('Ctrl Pts',(-3.98854928957189,1.,1.19864679609566));
#63423=CARTESIAN_POINT('Ctrl Pts',(-3.99433084799666,1.,1.20391852375139));
#63424=CARTESIAN_POINT('Ctrl Pts',(-4.00009577950721,1.,1.20922097029551));
#63425=CARTESIAN_POINT('Ctrl Pts',(-4.00584409522722,1.,1.21455398918133));
#63426=CARTESIAN_POINT('Ctrl Pts',(-4.01042947140789,1.,1.21884478244403));
#63427=CARTESIAN_POINT('Ctrl Pts',(-4.01386104433519,1.,1.22207656455845));
#63428=CARTESIAN_POINT('Ctrl Pts',(-4.01614544569895,1.,1.22423716681317));
#63429=CARTESIAN_POINT('Ctrl Pts',(-4.01728681790024,1.,1.22531898815164));
#63430=CARTESIAN_POINT('Origin',(-4.01728681790024,0.,1.22531898815164));
#63431=CARTESIAN_POINT('',(-3.97027773754922,1.,1.36999806084572));
#63432=CARTESIAN_POINT('Origin',(0.,0.,0.));
#63433=CARTESIAN_POINT('',(-3.66661143271648,1.,0.786422660833743));
#63434=CARTESIAN_POINT('Origin',(0.,1.,0.));
#63435=CARTESIAN_POINT('Ctrl Pts',(-3.66661143271648,1.,0.786422660833743));
#63436=CARTESIAN_POINT('Ctrl Pts',(-3.66661143271648,0.666666666666667,
0.786422660833743));
#63437=CARTESIAN_POINT('Ctrl Pts',(-3.66661143271648,0.333333333333333,
0.786422660833743));
#63438=CARTESIAN_POINT('Ctrl Pts',(-3.66661143271648,-0.333333333333333,
0.786422660833743));
#63439=CARTESIAN_POINT('Ctrl Pts',(-3.66661143271648,-0.666666666666667,
0.786422660833743));
#63440=CARTESIAN_POINT('Ctrl Pts',(-3.66661143271648,-1.,0.786422660833743));
#63441=CARTESIAN_POINT('Ctrl Pts',(-4.13571194405636,-1.,0.732042837400619));
#63442=CARTESIAN_POINT('Ctrl Pts',(-4.13571194405636,1.,0.732042837400619));
#63443=CARTESIAN_POINT('Ctrl Pts',(-4.13420383737278,-1.,0.732488575135926));
#63444=CARTESIAN_POINT('Ctrl Pts',(-4.13420383737278,1.,0.732488575135926));
#63445=CARTESIAN_POINT('Ctrl Pts',(-4.13118752796397,-1.,0.733376589325634));
#63446=CARTESIAN_POINT('Ctrl Pts',(-4.13118752796397,1.,0.733376589325634));
#63447=CARTESIAN_POINT('Ctrl Pts',(-4.12666277572794,-1.,0.734698226767512));
#63448=CARTESIAN_POINT('Ctrl Pts',(-4.12666277572794,1.,0.734698226767512));
#63449=CARTESIAN_POINT('Ctrl Pts',(-4.12062919626082,-1.,0.736439634335347));
#63450=CARTESIAN_POINT('Ctrl Pts',(-4.12062919626082,1.,0.736439634335347));
#63451=CARTESIAN_POINT('Ctrl Pts',(-4.11308626953795,-1.,0.738581708229118));
#63452=CARTESIAN_POINT('Ctrl Pts',(-4.11308626953795,1.,0.738581708229118));
#63453=CARTESIAN_POINT('Ctrl Pts',(-4.1055424175856,-1.,0.740688998555151));
#63454=CARTESIAN_POINT('Ctrl Pts',(-4.1055424175856,1.,0.740688998555151));
#63455=CARTESIAN_POINT('Ctrl Pts',(-4.09799769702712,-1.,0.742761369690017));
#63456=CARTESIAN_POINT('Ctrl Pts',(-4.09799769702712,1.,0.742761369690017));
#63457=CARTESIAN_POINT('Ctrl Pts',(-4.09045220253011,-1.,0.744798649705514));
#63458=CARTESIAN_POINT('Ctrl Pts',(-4.09045220253011,1.,0.744798649705514));
#63459=CARTESIAN_POINT('Ctrl Pts',(-4.08290608094789,-1.,0.746800631490821));
#63460=CARTESIAN_POINT('Ctrl Pts',(-4.08290608094789,1.,0.746800631490821));
#63461=CARTESIAN_POINT('Ctrl Pts',(-4.07535951055363,-1.,0.748767076679177));
#63462=CARTESIAN_POINT('Ctrl Pts',(-4.07535951055363,1.,0.748767076679177));
#63463=CARTESIAN_POINT('Ctrl Pts',(-4.06781267241886,-1.,0.750697720483175));
#63464=CARTESIAN_POINT('Ctrl Pts',(-4.06781267241886,1.,0.750697720483175));
#63465=CARTESIAN_POINT('Ctrl Pts',(-4.06026572221399,-1.,0.752592276482869));
#63466=CARTESIAN_POINT('Ctrl Pts',(-4.06026572221399,1.,0.752592276482869));
#63467=CARTESIAN_POINT('Ctrl Pts',(-4.05271876688106,-1.,0.754450441816411));
#63468=CARTESIAN_POINT('Ctrl Pts',(-4.05271876688106,1.,0.754450441816411));
#63469=CARTESIAN_POINT('Ctrl Pts',(-4.04517182654344,-1.,0.756271902370186));
#63470=CARTESIAN_POINT('Ctrl Pts',(-4.04517182654344,1.,0.756271902370186));
#63471=CARTESIAN_POINT('Ctrl Pts',(-4.03762485803468,-1.,0.758056338885553));
#63472=CARTESIAN_POINT('Ctrl Pts',(-4.03762485803468,1.,0.758056338885553));
#63473=CARTESIAN_POINT('Ctrl Pts',(-4.0300778195465,-1.,0.759803433244166));
#63474=CARTESIAN_POINT('Ctrl Pts',(-4.0300778195465,1.,0.759803433244166));
#63475=CARTESIAN_POINT('Ctrl Pts',(-4.02253072741347,-1.,0.761512875859941));
#63476=CARTESIAN_POINT('Ctrl Pts',(-4.02253072741347,1.,0.761512875859941));
#63477=CARTESIAN_POINT('Ctrl Pts',(-4.01498370680434,-1.,0.763184371182826));
#63478=CARTESIAN_POINT('Ctrl Pts',(-4.01498370680434,1.,0.763184371182826));
#63479=CARTESIAN_POINT('Ctrl Pts',(-4.00743706791366,-1.,0.764817648784946));
#63480=CARTESIAN_POINT('Ctrl Pts',(-4.00743706791366,1.,0.764817648784946));
#63481=CARTESIAN_POINT('Ctrl Pts',(-3.99989129179464,-1.,0.766412457135785));
#63482=CARTESIAN_POINT('Ctrl Pts',(-3.99989129179464,1.,0.766412457135785));
#63483=CARTESIAN_POINT('Ctrl Pts',(-3.99234687880892,-1.,0.767968531377708));
#63484=CARTESIAN_POINT('Ctrl Pts',(-3.99234687880892,1.,0.767968531377708));
#63485=CARTESIAN_POINT('Ctrl Pts',(-3.98480422348403,-1.,0.769485566245459));
#63486=CARTESIAN_POINT('Ctrl Pts',(-3.98480422348403,1.,0.769485566245459));
#63487=CARTESIAN_POINT('Ctrl Pts',(-3.97726349165507,-1.,0.770963190030503));
#63488=CARTESIAN_POINT('Ctrl Pts',(-3.97726349165507,1.,0.770963190030503));
#63489=CARTESIAN_POINT('Ctrl Pts',(-3.96972446532832,-1.,0.772400931772238));
#63490=CARTESIAN_POINT('Ctrl Pts',(-3.96972446532832,1.,0.772400931772238));
#63491=CARTESIAN_POINT('Ctrl Pts',(-3.96218649639876,-1.,0.773798212026682));
#63492=CARTESIAN_POINT('Ctrl Pts',(-3.96218649639876,1.,0.773798212026682));
#63493=CARTESIAN_POINT('Ctrl Pts',(-3.95464885452364,-1.,0.775154418039441));
#63494=CARTESIAN_POINT('Ctrl Pts',(-3.95464885452364,1.,0.775154418039441));
#63495=CARTESIAN_POINT('Ctrl Pts',(-3.94711101619471,-1.,0.77646896669796));
#63496=CARTESIAN_POINT('Ctrl Pts',(-3.94711101619471,1.,0.77646896669796));
#63497=CARTESIAN_POINT('Ctrl Pts',(-3.93957296768098,-1.,0.777741370568549));
#63498=CARTESIAN_POINT('Ctrl Pts',(-3.93957296768098,1.,0.777741370568549));
#63499=CARTESIAN_POINT('Ctrl Pts',(-3.93203552473153,-1.,0.778971308134786));
#63500=CARTESIAN_POINT('Ctrl Pts',(-3.93203552473153,1.,0.778971308134786));
#63501=CARTESIAN_POINT('Ctrl Pts',(-3.92450058323799,-1.,0.780158678615506));
#63502=CARTESIAN_POINT('Ctrl Pts',(-3.92450058323799,1.,0.780158678615506));
#63503=CARTESIAN_POINT('Ctrl Pts',(-3.9169703605466,-1.,0.781303428618343));
#63504=CARTESIAN_POINT('Ctrl Pts',(-3.9169703605466,1.,0.781303428618343));
#63505=CARTESIAN_POINT('Ctrl Pts',(-3.90944671004536,-1.,0.782405395622758));
#63506=CARTESIAN_POINT('Ctrl Pts',(-3.90944671004536,1.,0.782405395622758));
#63507=CARTESIAN_POINT('Ctrl Pts',(-3.90193039043971,-1.,0.783464141529082));
#63508=CARTESIAN_POINT('Ctrl Pts',(-3.90193039043971,1.,0.783464141529082));
#63509=CARTESIAN_POINT('Ctrl Pts',(-3.89442039235105,-1.,0.784478799358335));
#63510=CARTESIAN_POINT('Ctrl Pts',(-3.89442039235105,1.,0.784478799358335));
#63511=CARTESIAN_POINT('Ctrl Pts',(-3.88691313167399,-1.,0.785447890340723));
#63512=CARTESIAN_POINT('Ctrl Pts',(-3.88691313167399,1.,0.785447890340723));
#63513=CARTESIAN_POINT('Ctrl Pts',(-3.87940402818186,-1.,0.786369675812592));
#63514=CARTESIAN_POINT('Ctrl Pts',(-3.87940402818186,1.,0.786369675812592));
#63515=CARTESIAN_POINT('Ctrl Pts',(-3.87188916600905,-1.,0.78724252761798));
#63516=CARTESIAN_POINT('Ctrl Pts',(-3.87188916600905,1.,0.78724252761798));
#63517=CARTESIAN_POINT('Ctrl Pts',(-3.86436702561342,-1.,0.788065315093771));
#63518=CARTESIAN_POINT('Ctrl Pts',(-3.86436702561342,1.,0.788065315093771));
#63519=CARTESIAN_POINT('Ctrl Pts',(-3.85683995872536,-1.,0.788837734090688));
#63520=CARTESIAN_POINT('Ctrl Pts',(-3.85683995872536,1.,0.788837734090688));
#63521=CARTESIAN_POINT('Ctrl Pts',(-3.8493163780891,-1.,0.789560798155618));
#63522=CARTESIAN_POINT('Ctrl Pts',(-3.8493163780891,1.,0.789560798155618));
#63523=CARTESIAN_POINT('Ctrl Pts',(-3.84180762342476,-1.,0.790236124191289));
#63524=CARTESIAN_POINT('Ctrl Pts',(-3.84180762342476,1.,0.790236124191289));
#63525=CARTESIAN_POINT('Ctrl Pts',(-3.83432392054804,-1.,0.79086501270534));
#63526=CARTESIAN_POINT('Ctrl Pts',(-3.83432392054804,1.,0.79086501270534));
#63527=CARTESIAN_POINT('Ctrl Pts',(-3.82687033899799,-1.,0.791447528662381));
#63528=CARTESIAN_POINT('Ctrl Pts',(-3.82687033899799,1.,0.791447528662381));
#63529=CARTESIAN_POINT('Ctrl Pts',(-3.81944345442237,-1.,0.791981740718606));
#63530=CARTESIAN_POINT('Ctrl Pts',(-3.81944345442237,1.,0.791981740718606));
#63531=CARTESIAN_POINT('Ctrl Pts',(-3.81202588694726,-1.,0.792462483517568));
#63532=CARTESIAN_POINT('Ctrl Pts',(-3.81202588694726,1.,0.792462483517568));
#63533=CARTESIAN_POINT('Ctrl Pts',(-3.80459229925598,-1.,0.792882695234693));
#63534=CARTESIAN_POINT('Ctrl Pts',(-3.80459229925598,1.,0.792882695234693));
#63535=CARTESIAN_POINT('Ctrl Pts',(-3.79711921389862,-1.,0.7932356129732));
#63536=CARTESIAN_POINT('Ctrl Pts',(-3.79711921389862,1.,0.7932356129732));
#63537=CARTESIAN_POINT('Ctrl Pts',(-3.78959439439222,-1.,0.793516871680966));
#63538=CARTESIAN_POINT('Ctrl Pts',(-3.78959439439222,1.,0.793516871680966));
#63539=CARTESIAN_POINT('Ctrl Pts',(-3.78202460377617,-1.,0.793726235781339));
#63540=CARTESIAN_POINT('Ctrl Pts',(-3.78202460377617,1.,0.793726235781339));
#63541=CARTESIAN_POINT('Ctrl Pts',(-3.77444863801264,-1.,0.793870523787515));
#63542=CARTESIAN_POINT('Ctrl Pts',(-3.77444863801264,1.,0.793870523787515));
#63543=CARTESIAN_POINT('Ctrl Pts',(-3.76692626931184,-1.,0.793961083689141));
#63544=CARTESIAN_POINT('Ctrl Pts',(-3.76692626931184,1.,0.793961083689141));
#63545=CARTESIAN_POINT('Ctrl Pts',(-3.75951468666325,-1.,0.794008429135047));
#63546=CARTESIAN_POINT('Ctrl Pts',(-3.75951468666325,1.,0.794008429135047));
#63547=CARTESIAN_POINT('Ctrl Pts',(-3.75224692493895,-1.,0.79401734737144));
#63548=CARTESIAN_POINT('Ctrl Pts',(-3.75224692493895,1.,0.79401734737144));
#63549=CARTESIAN_POINT('Ctrl Pts',(-3.74511357728827,-1.,0.79398270045988));
#63550=CARTESIAN_POINT('Ctrl Pts',(-3.74511357728827,1.,0.79398270045988));
#63551=CARTESIAN_POINT('Ctrl Pts',(-3.73803280541576,-1.,0.79388270093679));
#63552=CARTESIAN_POINT('Ctrl Pts',(-3.73803280541576,1.,0.79388270093679));
#63553=CARTESIAN_POINT('Ctrl Pts',(-3.7308691469564,-1.,0.793682750269347));
#63554=CARTESIAN_POINT('Ctrl Pts',(-3.7308691469564,1.,0.793682750269347));
#63555=CARTESIAN_POINT('Ctrl Pts',(-3.7234879729357,-1.,0.79334702378387));
#63556=CARTESIAN_POINT('Ctrl Pts',(-3.7234879729357,1.,0.79334702378387));
#63557=CARTESIAN_POINT('Ctrl Pts',(-3.7158024239604,-1.,0.792848377370115));
#63558=CARTESIAN_POINT('Ctrl Pts',(-3.7158024239604,1.,0.792848377370115));
#63559=CARTESIAN_POINT('Ctrl Pts',(-3.70781724021879,-1.,0.792177688845967));
#63560=CARTESIAN_POINT('Ctrl Pts',(-3.70781724021879,1.,0.792177688845967));
#63561=CARTESIAN_POINT('Ctrl Pts',(-3.69968940808982,-1.,0.791356575696509));
#63562=CARTESIAN_POINT('Ctrl Pts',(-3.69968940808982,1.,0.791356575696509));
#63563=CARTESIAN_POINT('Ctrl Pts',(-3.69172044327754,-1.,0.79043628498958));
#63564=CARTESIAN_POINT('Ctrl Pts',(-3.69172044327754,1.,0.79043628498958));
#63565=CARTESIAN_POINT('Ctrl Pts',(-3.68428439784285,-1.,0.789483546065158));
#63566=CARTESIAN_POINT('Ctrl Pts',(-3.68428439784285,1.,0.789483546065158));
#63567=CARTESIAN_POINT('Ctrl Pts',(-3.67777119516438,-1.,0.788569566220662));
#63568=CARTESIAN_POINT('Ctrl Pts',(-3.67777119516438,1.,0.788569566220662));
#63569=CARTESIAN_POINT('Ctrl Pts',(-3.672529236635,-1.,0.787758799995426));
#63570=CARTESIAN_POINT('Ctrl Pts',(-3.672529236635,1.,0.787758799995426));
#63571=CARTESIAN_POINT('Ctrl Pts',(-3.66879484800625,-1.,0.787095252589507));
#63572=CARTESIAN_POINT('Ctrl Pts',(-3.66879484800625,1.,0.787095252589507));
#63573=CARTESIAN_POINT('Ctrl Pts',(-3.66710211819938,-1.,0.786698783541657));
#63574=CARTESIAN_POINT('Ctrl Pts',(-3.66710211819938,1.,0.786698783541657));
#63575=CARTESIAN_POINT('Ctrl Pts',(-3.66657784454965,-1.,0.786480236184947));
#63576=CARTESIAN_POINT('Ctrl Pts',(-3.66657784454965,1.,0.786480236184947));
#63577=CARTESIAN_POINT('Ctrl Pts',(-3.66655932661846,-1.,0.786369528183039));
#63578=CARTESIAN_POINT('Ctrl Pts',(-3.66655932661846,1.,0.786369528183039));
#63579=CARTESIAN_POINT('Ctrl Pts',(-3.66663282329846,-1.,0.786322922920599));
#63580=CARTESIAN_POINT('Ctrl Pts',(-3.66663282329846,1.,0.786322922920599));
#63581=CARTESIAN_POINT('',(-4.13571194405636,1.,0.732042837400619));
#63582=CARTESIAN_POINT('Ctrl Pts',(-4.13571194405636,1.,0.732042837400619));
#63583=CARTESIAN_POINT('Ctrl Pts',(-4.13420383737278,1.,0.732488575135926));
#63584=CARTESIAN_POINT('Ctrl Pts',(-4.13118752796397,1.,0.733376589325634));
#63585=CARTESIAN_POINT('Ctrl Pts',(-4.12666277572794,1.,0.734698226767512));
#63586=CARTESIAN_POINT('Ctrl Pts',(-4.12062919626082,1.,0.736439634335347));
#63587=CARTESIAN_POINT('Ctrl Pts',(-4.11308626953795,1.,0.738581708229118));
#63588=CARTESIAN_POINT('Ctrl Pts',(-4.1055424175856,1.,0.740688998555151));
#63589=CARTESIAN_POINT('Ctrl Pts',(-4.09799769702712,1.,0.742761369690017));
#63590=CARTESIAN_POINT('Ctrl Pts',(-4.09045220253011,1.,0.744798649705514));
#63591=CARTESIAN_POINT('Ctrl Pts',(-4.08290608094789,1.,0.746800631490821));
#63592=CARTESIAN_POINT('Ctrl Pts',(-4.07535951055363,1.,0.748767076679177));
#63593=CARTESIAN_POINT('Ctrl Pts',(-4.06781267241886,1.,0.750697720483175));
#63594=CARTESIAN_POINT('Ctrl Pts',(-4.06026572221399,1.,0.752592276482869));
#63595=CARTESIAN_POINT('Ctrl Pts',(-4.05271876688106,1.,0.754450441816411));
#63596=CARTESIAN_POINT('Ctrl Pts',(-4.04517182654344,1.,0.756271902370186));
#63597=CARTESIAN_POINT('Ctrl Pts',(-4.03762485803468,1.,0.758056338885553));
#63598=CARTESIAN_POINT('Ctrl Pts',(-4.0300778195465,1.,0.759803433244166));
#63599=CARTESIAN_POINT('Ctrl Pts',(-4.02253072741347,1.,0.761512875859941));
#63600=CARTESIAN_POINT('Ctrl Pts',(-4.01498370680434,1.,0.763184371182826));
#63601=CARTESIAN_POINT('Ctrl Pts',(-4.00743706791366,1.,0.764817648784946));
#63602=CARTESIAN_POINT('Ctrl Pts',(-3.99989129179464,1.,0.766412457135785));
#63603=CARTESIAN_POINT('Ctrl Pts',(-3.99234687880892,1.,0.767968531377708));
#63604=CARTESIAN_POINT('Ctrl Pts',(-3.98480422348403,1.,0.769485566245459));
#63605=CARTESIAN_POINT('Ctrl Pts',(-3.97726349165507,1.,0.770963190030503));
#63606=CARTESIAN_POINT('Ctrl Pts',(-3.96972446532832,1.,0.772400931772238));
#63607=CARTESIAN_POINT('Ctrl Pts',(-3.96218649639876,1.,0.773798212026682));
#63608=CARTESIAN_POINT('Ctrl Pts',(-3.95464885452364,1.,0.775154418039441));
#63609=CARTESIAN_POINT('Ctrl Pts',(-3.94711101619471,1.,0.77646896669796));
#63610=CARTESIAN_POINT('Ctrl Pts',(-3.93957296768098,1.,0.777741370568549));
#63611=CARTESIAN_POINT('Ctrl Pts',(-3.93203552473153,1.,0.778971308134786));
#63612=CARTESIAN_POINT('Ctrl Pts',(-3.92450058323799,1.,0.780158678615506));
#63613=CARTESIAN_POINT('Ctrl Pts',(-3.9169703605466,1.,0.781303428618343));
#63614=CARTESIAN_POINT('Ctrl Pts',(-3.90944671004536,1.,0.782405395622758));
#63615=CARTESIAN_POINT('Ctrl Pts',(-3.90193039043971,1.,0.783464141529082));
#63616=CARTESIAN_POINT('Ctrl Pts',(-3.89442039235105,1.,0.784478799358335));
#63617=CARTESIAN_POINT('Ctrl Pts',(-3.88691313167399,1.,0.785447890340723));
#63618=CARTESIAN_POINT('Ctrl Pts',(-3.87940402818186,1.,0.786369675812592));
#63619=CARTESIAN_POINT('Ctrl Pts',(-3.87188916600905,1.,0.78724252761798));
#63620=CARTESIAN_POINT('Ctrl Pts',(-3.86436702561342,1.,0.788065315093771));
#63621=CARTESIAN_POINT('Ctrl Pts',(-3.85683995872536,1.,0.788837734090688));
#63622=CARTESIAN_POINT('Ctrl Pts',(-3.8493163780891,1.,0.789560798155618));
#63623=CARTESIAN_POINT('Ctrl Pts',(-3.84180762342476,1.,0.790236124191289));
#63624=CARTESIAN_POINT('Ctrl Pts',(-3.83432392054804,1.,0.79086501270534));
#63625=CARTESIAN_POINT('Ctrl Pts',(-3.82687033899799,1.,0.791447528662381));
#63626=CARTESIAN_POINT('Ctrl Pts',(-3.81944345442237,1.,0.791981740718606));
#63627=CARTESIAN_POINT('Ctrl Pts',(-3.81202588694726,1.,0.792462483517568));
#63628=CARTESIAN_POINT('Ctrl Pts',(-3.80459229925598,1.,0.792882695234693));
#63629=CARTESIAN_POINT('Ctrl Pts',(-3.79711921389862,1.,0.7932356129732));
#63630=CARTESIAN_POINT('Ctrl Pts',(-3.78959439439222,1.,0.793516871680966));
#63631=CARTESIAN_POINT('Ctrl Pts',(-3.78202460377617,1.,0.793726235781339));
#63632=CARTESIAN_POINT('Ctrl Pts',(-3.77444863801264,1.,0.793870523787515));
#63633=CARTESIAN_POINT('Ctrl Pts',(-3.76692626931184,1.,0.793961083689141));
#63634=CARTESIAN_POINT('Ctrl Pts',(-3.75951468666325,1.,0.794008429135047));
#63635=CARTESIAN_POINT('Ctrl Pts',(-3.75224692493895,1.,0.79401734737144));
#63636=CARTESIAN_POINT('Ctrl Pts',(-3.74511357728827,1.,0.79398270045988));
#63637=CARTESIAN_POINT('Ctrl Pts',(-3.73803280541576,1.,0.79388270093679));
#63638=CARTESIAN_POINT('Ctrl Pts',(-3.7308691469564,1.,0.793682750269347));
#63639=CARTESIAN_POINT('Ctrl Pts',(-3.7234879729357,1.,0.79334702378387));
#63640=CARTESIAN_POINT('Ctrl Pts',(-3.7158024239604,1.,0.792848377370115));
#63641=CARTESIAN_POINT('Ctrl Pts',(-3.70781724021879,1.,0.792177688845967));
#63642=CARTESIAN_POINT('Ctrl Pts',(-3.69968940808982,1.,0.791356575696509));
#63643=CARTESIAN_POINT('Ctrl Pts',(-3.69172044327754,1.,0.79043628498958));
#63644=CARTESIAN_POINT('Ctrl Pts',(-3.68428439784285,1.,0.789483546065158));
#63645=CARTESIAN_POINT('Ctrl Pts',(-3.67777119516438,1.,0.788569566220662));
#63646=CARTESIAN_POINT('Ctrl Pts',(-3.672529236635,1.,0.787758799995426));
#63647=CARTESIAN_POINT('Ctrl Pts',(-3.66907505398769,1.,0.787145041181588));
#63648=CARTESIAN_POINT('Ctrl Pts',(-3.66743103898844,1.,0.786774337198499));
#63649=CARTESIAN_POINT('Ctrl Pts',(-3.66680946938396,1.,0.786565919559889));
#63650=CARTESIAN_POINT('Ctrl Pts',(-3.66664310415236,1.,0.786459983896781));
#63651=CARTESIAN_POINT('Ctrl Pts',(-3.66661143271648,1.,0.786422660833743));
#63652=CARTESIAN_POINT('',(-4.13571194405636,0.,0.732042837400619));
#63653=CARTESIAN_POINT('Ctrl Pts',(-3.73016218570874,-1.,0.385214314776329));
#63654=CARTESIAN_POINT('Ctrl Pts',(-3.73016218570874,1.,0.385214314776329));
#63655=CARTESIAN_POINT('Ctrl Pts',(-3.73010668803185,-1.,0.385147278814804));
#63656=CARTESIAN_POINT('Ctrl Pts',(-3.73010668803185,1.,0.385147278814804));
#63657=CARTESIAN_POINT('Ctrl Pts',(-3.73015851028729,-1.,0.385047711603887));
#63658=CARTESIAN_POINT('Ctrl Pts',(-3.73015851028729,1.,0.385047711603887));
#63659=CARTESIAN_POINT('Ctrl Pts',(-3.73072465900727,-1.,0.385001870183841));
#63660=CARTESIAN_POINT('Ctrl Pts',(-3.73072465900727,1.,0.385001870183841));
#63661=CARTESIAN_POINT('Ctrl Pts',(-3.73245705639337,-1.,0.385147887989514));
#63662=CARTESIAN_POINT('Ctrl Pts',(-3.73245705639337,1.,0.385147887989514));
#63663=CARTESIAN_POINT('Ctrl Pts',(-3.73621371845475,-1.,0.385670806454744));
#63664=CARTESIAN_POINT('Ctrl Pts',(-3.73621371845475,1.,0.385670806454744));
#63665=CARTESIAN_POINT('Ctrl Pts',(-3.74144965781088,-1.,0.386519576222035));
#63666=CARTESIAN_POINT('Ctrl Pts',(-3.74144965781088,1.,0.386519576222035));
#63667=CARTESIAN_POINT('Ctrl Pts',(-3.74792651696269,-1.,0.387663020050396));
#63668=CARTESIAN_POINT('Ctrl Pts',(-3.74792651696269,1.,0.387663020050396));
#63669=CARTESIAN_POINT('Ctrl Pts',(-3.75529302894757,-1.,0.389054775898251));
#63670=CARTESIAN_POINT('Ctrl Pts',(-3.75529302894757,1.,0.389054775898251));
#63671=CARTESIAN_POINT('Ctrl Pts',(-3.76315635032993,-1.,0.390642072979259));
#63672=CARTESIAN_POINT('Ctrl Pts',(-3.76315635032993,1.,0.390642072979259));
#63673=CARTESIAN_POINT('Ctrl Pts',(-3.77114011595892,-1.,0.392372786223346));
#63674=CARTESIAN_POINT('Ctrl Pts',(-3.77114011595892,1.,0.392372786223346));
#63675=CARTESIAN_POINT('Ctrl Pts',(-3.77894173114368,-1.,0.394202481011595));
#63676=CARTESIAN_POINT('Ctrl Pts',(-3.77894173114368,1.,0.394202481011595));
#63677=CARTESIAN_POINT('Ctrl Pts',(-3.78640521279479,-1.,0.396103205335028));
#63678=CARTESIAN_POINT('Ctrl Pts',(-3.78640521279479,1.,0.396103205335028));
#63679=CARTESIAN_POINT('Ctrl Pts',(-3.79352887163457,-1.,0.398064818684158));
#63680=CARTESIAN_POINT('Ctrl Pts',(-3.79352887163457,1.,0.398064818684158));
#63681=CARTESIAN_POINT('Ctrl Pts',(-3.80040370384659,-1.,0.400088346504726));
#63682=CARTESIAN_POINT('Ctrl Pts',(-3.80040370384659,1.,0.400088346504726));
#63683=CARTESIAN_POINT('Ctrl Pts',(-3.80716881962763,-1.,0.402181320148474));
#63684=CARTESIAN_POINT('Ctrl Pts',(-3.80716881962763,1.,0.402181320148474));
#63685=CARTESIAN_POINT('Ctrl Pts',(-3.81396374287762,-1.,0.404352694628236));
#63686=CARTESIAN_POINT('Ctrl Pts',(-3.81396374287762,1.,0.404352694628236));
#63687=CARTESIAN_POINT('Ctrl Pts',(-3.82087303913741,-1.,0.406607038258906));
#63688=CARTESIAN_POINT('Ctrl Pts',(-3.82087303913741,1.,0.406607038258906));
#63689=CARTESIAN_POINT('Ctrl Pts',(-3.82790724256397,-1.,0.408942371447377));
#63690=CARTESIAN_POINT('Ctrl Pts',(-3.82790724256397,1.,0.408942371447377));
#63691=CARTESIAN_POINT('Ctrl Pts',(-3.83503345578645,-1.,0.411353038798459));
#63692=CARTESIAN_POINT('Ctrl Pts',(-3.83503345578645,1.,0.411353038798459));
#63693=CARTESIAN_POINT('Ctrl Pts',(-3.84219403994742,-1.,0.413831367016726));
#63694=CARTESIAN_POINT('Ctrl Pts',(-3.84219403994742,1.,0.413831367016726));
#63695=CARTESIAN_POINT('Ctrl Pts',(-3.8493286415751,-1.,0.41636967805292));
#63696=CARTESIAN_POINT('Ctrl Pts',(-3.8493286415751,1.,0.41636967805292));
#63697=CARTESIAN_POINT('Ctrl Pts',(-3.85639825648031,-1.,0.418962468086809));
#63698=CARTESIAN_POINT('Ctrl Pts',(-3.85639825648031,1.,0.418962468086809));
#63699=CARTESIAN_POINT('Ctrl Pts',(-3.86339652542749,-1.,0.421607423177575));
#63700=CARTESIAN_POINT('Ctrl Pts',(-3.86339652542749,1.,0.421607423177575));
#63701=CARTESIAN_POINT('Ctrl Pts',(-3.87033643487882,-1.,0.424304173195142));
#63702=CARTESIAN_POINT('Ctrl Pts',(-3.87033643487882,1.,0.424304173195142));
#63703=CARTESIAN_POINT('Ctrl Pts',(-3.87724240306609,-1.,0.427053541173469));
#63704=CARTESIAN_POINT('Ctrl Pts',(-3.87724240306609,1.,0.427053541173469));
#63705=CARTESIAN_POINT('Ctrl Pts',(-3.88414070943334,-1.,0.429856640579733));
#63706=CARTESIAN_POINT('Ctrl Pts',(-3.88414070943334,1.,0.429856640579733));
#63707=CARTESIAN_POINT('Ctrl Pts',(-3.89104947940592,-1.,0.432713929544439));
#63708=CARTESIAN_POINT('Ctrl Pts',(-3.89104947940592,1.,0.432713929544439));
#63709=CARTESIAN_POINT('Ctrl Pts',(-3.8979725665544,-1.,0.435624629433505));
#63710=CARTESIAN_POINT('Ctrl Pts',(-3.8979725665544,1.,0.435624629433505));
#63711=CARTESIAN_POINT('Ctrl Pts',(-3.90490512938546,-1.,0.438587235458233));
#63712=CARTESIAN_POINT('Ctrl Pts',(-3.90490512938546,1.,0.438587235458233));
#63713=CARTESIAN_POINT('Ctrl Pts',(-3.91183704069146,-1.,0.441599824524047));
#63714=CARTESIAN_POINT('Ctrl Pts',(-3.91183704069146,1.,0.441599824524047));
#63715=CARTESIAN_POINT('Ctrl Pts',(-3.91875701610721,-1.,0.444660430230592));
#63716=CARTESIAN_POINT('Ctrl Pts',(-3.91875701610721,1.,0.444660430230592));
#63717=CARTESIAN_POINT('Ctrl Pts',(-3.92565674143424,-1.,0.447767416837296));
#63718=CARTESIAN_POINT('Ctrl Pts',(-3.92565674143424,1.,0.447767416837296));
#63719=CARTESIAN_POINT('Ctrl Pts',(-3.93253407403128,-1.,0.450919768356347));
#63720=CARTESIAN_POINT('Ctrl Pts',(-3.93253407403128,1.,0.450919768356347));
#63721=CARTESIAN_POINT('Ctrl Pts',(-3.93939080846298,-1.,0.454116879027576));
#63722=CARTESIAN_POINT('Ctrl Pts',(-3.93939080846298,1.,0.454116879027576));
#63723=CARTESIAN_POINT('Ctrl Pts',(-3.94623117206675,-1.,0.457358410451674));
#63724=CARTESIAN_POINT('Ctrl Pts',(-3.94623117206675,1.,0.457358410451674));
#63725=CARTESIAN_POINT('Ctrl Pts',(-3.95306005817363,-1.,0.460644124429119));
#63726=CARTESIAN_POINT('Ctrl Pts',(-3.95306005817363,1.,0.460644124429119));
#63727=CARTESIAN_POINT('Ctrl Pts',(-3.95988133243543,-1.,0.463973722115744));
#63728=CARTESIAN_POINT('Ctrl Pts',(-3.95988133243543,1.,0.463973722115744));
#63729=CARTESIAN_POINT('Ctrl Pts',(-3.96669622273946,-1.,0.467346690880671));
#63730=CARTESIAN_POINT('Ctrl Pts',(-3.96669622273946,1.,0.467346690880671));
#63731=CARTESIAN_POINT('Ctrl Pts',(-3.97350414289415,-1.,0.470762379613477));
#63732=CARTESIAN_POINT('Ctrl Pts',(-3.97350414289415,1.,0.470762379613477));
#63733=CARTESIAN_POINT('Ctrl Pts',(-3.9803033804443,-1.,0.474220061019542));
#63734=CARTESIAN_POINT('Ctrl Pts',(-3.9803033804443,1.,0.474220061019542));
#63735=CARTESIAN_POINT('Ctrl Pts',(-3.98709184306743,-1.,0.477718999122033));
#63736=CARTESIAN_POINT('Ctrl Pts',(-3.98709184306743,1.,0.477718999122033));
#63737=CARTESIAN_POINT('Ctrl Pts',(-3.99386775880655,-1.,0.481258512209638));
#63738=CARTESIAN_POINT('Ctrl Pts',(-3.99386775880655,1.,0.481258512209638));
#63739=CARTESIAN_POINT('Ctrl Pts',(-4.00063045119234,-1.,0.484838042421754));
#63740=CARTESIAN_POINT('Ctrl Pts',(-4.00063045119234,1.,0.484838042421754));
#63741=CARTESIAN_POINT('Ctrl Pts',(-4.0073800839092,-1.,0.48845713042453));
#63742=CARTESIAN_POINT('Ctrl Pts',(-4.0073800839092,1.,0.48845713042453));
#63743=CARTESIAN_POINT('Ctrl Pts',(-4.01411733503486,-1.,0.49211538341793));
#63744=CARTESIAN_POINT('Ctrl Pts',(-4.01411733503486,1.,0.49211538341793));
#63745=CARTESIAN_POINT('Ctrl Pts',(-4.02084308851813,-1.,0.495812444326223));
#63746=CARTESIAN_POINT('Ctrl Pts',(-4.02084308851813,1.,0.495812444326223));
#63747=CARTESIAN_POINT('Ctrl Pts',(-4.0275581398015,-1.,0.499547962340889));
#63748=CARTESIAN_POINT('Ctrl Pts',(-4.0275581398015,1.,0.499547962340889));
#63749=CARTESIAN_POINT('Ctrl Pts',(-4.0342628417439,-1.,0.503321556915513));
#63750=CARTESIAN_POINT('Ctrl Pts',(-4.0342628417439,1.,0.503321556915513));
#63751=CARTESIAN_POINT('Ctrl Pts',(-4.04095715149074,-1.,0.507132823288361));
#63752=CARTESIAN_POINT('Ctrl Pts',(-4.04095715149074,1.,0.507132823288361));
#63753=CARTESIAN_POINT('Ctrl Pts',(-4.04764078815591,-1.,0.510981349219173));
#63754=CARTESIAN_POINT('Ctrl Pts',(-4.04764078815591,1.,0.510981349219173));
#63755=CARTESIAN_POINT('Ctrl Pts',(-4.05431335771261,-1.,0.514866728193104));
#63756=CARTESIAN_POINT('Ctrl Pts',(-4.05431335771261,1.,0.514866728193104));
#63757=CARTESIAN_POINT('Ctrl Pts',(-4.06097448037934,-1.,0.518788572336809));
#63758=CARTESIAN_POINT('Ctrl Pts',(-4.06097448037934,1.,0.518788572336809));
#63759=CARTESIAN_POINT('Ctrl Pts',(-4.06762394471075,-1.,0.522746528602767));
#63760=CARTESIAN_POINT('Ctrl Pts',(-4.06762394471075,1.,0.522746528602767));
#63761=CARTESIAN_POINT('Ctrl Pts',(-4.07426172299496,-1.,0.526740277226999));
#63762=CARTESIAN_POINT('Ctrl Pts',(-4.07426172299496,1.,0.526740277226999));
#63763=CARTESIAN_POINT('Ctrl Pts',(-4.08088789536488,-1.,0.530769518728075));
#63764=CARTESIAN_POINT('Ctrl Pts',(-4.08088789536488,1.,0.530769518728075));
#63765=CARTESIAN_POINT('Ctrl Pts',(-4.08750259988693,-1.,0.534833963476999));
#63766=CARTESIAN_POINT('Ctrl Pts',(-4.08750259988693,1.,0.534833963476999));
#63767=CARTESIAN_POINT('Ctrl Pts',(-4.09410597627116,-1.,0.53893332117992));
#63768=CARTESIAN_POINT('Ctrl Pts',(-4.09410597627116,1.,0.53893332117992));
#63769=CARTESIAN_POINT('Ctrl Pts',(-4.10069810244473,-1.,0.543067286878457));
#63770=CARTESIAN_POINT('Ctrl Pts',(-4.10069810244473,1.,0.543067286878457));
#63771=CARTESIAN_POINT('Ctrl Pts',(-4.1072789702877,-1.,0.547235539486759));
#63772=CARTESIAN_POINT('Ctrl Pts',(-4.1072789702877,1.,0.547235539486759));
#63773=CARTESIAN_POINT('Ctrl Pts',(-4.11384852025578,-1.,0.551437758498246));
#63774=CARTESIAN_POINT('Ctrl Pts',(-4.11384852025578,1.,0.551437758498246));
#63775=CARTESIAN_POINT('Ctrl Pts',(-4.1204066619623,-1.,0.555673636130778));
#63776=CARTESIAN_POINT('Ctrl Pts',(-4.1204066619623,1.,0.555673636130778));
#63777=CARTESIAN_POINT('Ctrl Pts',(-4.12695329951859,-1.,0.559942890594628));
#63778=CARTESIAN_POINT('Ctrl Pts',(-4.12695329951859,1.,0.559942890594628));
#63779=CARTESIAN_POINT('Ctrl Pts',(-4.13348835726086,-1.,0.564245279535705));
#63780=CARTESIAN_POINT('Ctrl Pts',(-4.13348835726086,1.,0.564245279535705));
#63781=CARTESIAN_POINT('Ctrl Pts',(-4.14001179828669,-1.,0.568580610187116));
#63782=CARTESIAN_POINT('Ctrl Pts',(-4.14001179828669,1.,0.568580610187116));
#63783=CARTESIAN_POINT('Ctrl Pts',(-4.14652361065787,-1.,0.572948736066276));
#63784=CARTESIAN_POINT('Ctrl Pts',(-4.14652361065787,1.,0.572948736066276));
#63785=CARTESIAN_POINT('Ctrl Pts',(-4.1517237611974,-1.,0.576469391673916));
#63786=CARTESIAN_POINT('Ctrl Pts',(-4.1517237611974,1.,0.576469391673916));
#63787=CARTESIAN_POINT('Ctrl Pts',(-4.15561864787379,-1.,0.579124568912543));
#63788=CARTESIAN_POINT('Ctrl Pts',(-4.15561864787379,1.,0.579124568912543));
#63789=CARTESIAN_POINT('Ctrl Pts',(-4.15821291712391,-1.,0.580901211462913));
#63790=CARTESIAN_POINT('Ctrl Pts',(-4.15821291712391,1.,0.580901211462913));
#63791=CARTESIAN_POINT('Ctrl Pts',(-4.15950947128175,-1.,0.581791163835814));
#63792=CARTESIAN_POINT('Ctrl Pts',(-4.15950947128175,1.,0.581791163835814));
#63793=CARTESIAN_POINT('',(-3.73017266276632,1.,0.385112848332549));
#63794=CARTESIAN_POINT('Ctrl Pts',(-3.73017266276632,-1.,0.385112848332549));
#63795=CARTESIAN_POINT('Ctrl Pts',(-3.73017266276632,-0.666666666666667,
0.385112848332549));
#63796=CARTESIAN_POINT('Ctrl Pts',(-3.73017266276632,-0.333333333333333,
0.385112848332549));
#63797=CARTESIAN_POINT('Ctrl Pts',(-3.73017266276632,0.333333333333333,
0.385112848332549));
#63798=CARTESIAN_POINT('Ctrl Pts',(-3.73017266276632,0.666666666666667,
0.385112848332549));
#63799=CARTESIAN_POINT('Ctrl Pts',(-3.73017266276632,1.,0.385112848332549));
#63800=CARTESIAN_POINT('',(-4.15950947128175,1.,0.581791163835814));
#63801=CARTESIAN_POINT('',(-4.15950947128175,0.,0.581791163835814));
#63802=CARTESIAN_POINT('Ctrl Pts',(-3.73017266276632,1.,0.385112848332549));
#63803=CARTESIAN_POINT('Ctrl Pts',(-3.73021431755218,1.,0.385087139001609));
#63804=CARTESIAN_POINT('Ctrl Pts',(-3.73040527620929,1.,0.385037797882046));
#63805=CARTESIAN_POINT('Ctrl Pts',(-3.73106082862399,1.,0.385031656499141));
#63806=CARTESIAN_POINT('Ctrl Pts',(-3.73273893363318,1.,0.385187124633964));
#63807=CARTESIAN_POINT('Ctrl Pts',(-3.73621371845475,1.,0.385670806454744));
#63808=CARTESIAN_POINT('Ctrl Pts',(-3.74144965781088,1.,0.386519576222035));
#63809=CARTESIAN_POINT('Ctrl Pts',(-3.74792651696269,1.,0.387663020050396));
#63810=CARTESIAN_POINT('Ctrl Pts',(-3.75529302894757,1.,0.389054775898251));
#63811=CARTESIAN_POINT('Ctrl Pts',(-3.76315635032993,1.,0.390642072979259));
#63812=CARTESIAN_POINT('Ctrl Pts',(-3.77114011595892,1.,0.392372786223346));
#63813=CARTESIAN_POINT('Ctrl Pts',(-3.77894173114368,1.,0.394202481011595));
#63814=CARTESIAN_POINT('Ctrl Pts',(-3.78640521279479,1.,0.396103205335028));
#63815=CARTESIAN_POINT('Ctrl Pts',(-3.79352887163457,1.,0.398064818684158));
#63816=CARTESIAN_POINT('Ctrl Pts',(-3.80040370384659,1.,0.400088346504726));
#63817=CARTESIAN_POINT('Ctrl Pts',(-3.80716881962763,1.,0.402181320148474));
#63818=CARTESIAN_POINT('Ctrl Pts',(-3.81396374287762,1.,0.404352694628236));
#63819=CARTESIAN_POINT('Ctrl Pts',(-3.82087303913741,1.,0.406607038258906));
#63820=CARTESIAN_POINT('Ctrl Pts',(-3.82790724256397,1.,0.408942371447377));
#63821=CARTESIAN_POINT('Ctrl Pts',(-3.83503345578645,1.,0.411353038798459));
#63822=CARTESIAN_POINT('Ctrl Pts',(-3.84219403994742,1.,0.413831367016726));
#63823=CARTESIAN_POINT('Ctrl Pts',(-3.8493286415751,1.,0.41636967805292));
#63824=CARTESIAN_POINT('Ctrl Pts',(-3.85639825648031,1.,0.418962468086809));
#63825=CARTESIAN_POINT('Ctrl Pts',(-3.86339652542749,1.,0.421607423177575));
#63826=CARTESIAN_POINT('Ctrl Pts',(-3.87033643487882,1.,0.424304173195142));
#63827=CARTESIAN_POINT('Ctrl Pts',(-3.87724240306609,1.,0.427053541173469));
#63828=CARTESIAN_POINT('Ctrl Pts',(-3.88414070943334,1.,0.429856640579733));
#63829=CARTESIAN_POINT('Ctrl Pts',(-3.89104947940592,1.,0.432713929544439));
#63830=CARTESIAN_POINT('Ctrl Pts',(-3.8979725665544,1.,0.435624629433505));
#63831=CARTESIAN_POINT('Ctrl Pts',(-3.90490512938546,1.,0.438587235458233));
#63832=CARTESIAN_POINT('Ctrl Pts',(-3.91183704069146,1.,0.441599824524047));
#63833=CARTESIAN_POINT('Ctrl Pts',(-3.91875701610721,1.,0.444660430230592));
#63834=CARTESIAN_POINT('Ctrl Pts',(-3.92565674143424,1.,0.447767416837296));
#63835=CARTESIAN_POINT('Ctrl Pts',(-3.93253407403128,1.,0.450919768356347));
#63836=CARTESIAN_POINT('Ctrl Pts',(-3.93939080846298,1.,0.454116879027576));
#63837=CARTESIAN_POINT('Ctrl Pts',(-3.94623117206675,1.,0.457358410451674));
#63838=CARTESIAN_POINT('Ctrl Pts',(-3.95306005817363,1.,0.460644124429119));
#63839=CARTESIAN_POINT('Ctrl Pts',(-3.95988133243543,1.,0.463973722115744));
#63840=CARTESIAN_POINT('Ctrl Pts',(-3.96669622273946,1.,0.467346690880671));
#63841=CARTESIAN_POINT('Ctrl Pts',(-3.97350414289415,1.,0.470762379613477));
#63842=CARTESIAN_POINT('Ctrl Pts',(-3.9803033804443,1.,0.474220061019542));
#63843=CARTESIAN_POINT('Ctrl Pts',(-3.98709184306743,1.,0.477718999122033));
#63844=CARTESIAN_POINT('Ctrl Pts',(-3.99386775880655,1.,0.481258512209638));
#63845=CARTESIAN_POINT('Ctrl Pts',(-4.00063045119234,1.,0.484838042421754));
#63846=CARTESIAN_POINT('Ctrl Pts',(-4.0073800839092,1.,0.48845713042453));
#63847=CARTESIAN_POINT('Ctrl Pts',(-4.01411733503486,1.,0.49211538341793));
#63848=CARTESIAN_POINT('Ctrl Pts',(-4.02084308851813,1.,0.495812444326223));
#63849=CARTESIAN_POINT('Ctrl Pts',(-4.0275581398015,1.,0.499547962340889));
#63850=CARTESIAN_POINT('Ctrl Pts',(-4.0342628417439,1.,0.503321556915513));
#63851=CARTESIAN_POINT('Ctrl Pts',(-4.04095715149074,1.,0.507132823288361));
#63852=CARTESIAN_POINT('Ctrl Pts',(-4.04764078815591,1.,0.510981349219173));
#63853=CARTESIAN_POINT('Ctrl Pts',(-4.05431335771261,1.,0.514866728193104));
#63854=CARTESIAN_POINT('Ctrl Pts',(-4.06097448037934,1.,0.518788572336809));
#63855=CARTESIAN_POINT('Ctrl Pts',(-4.06762394471075,1.,0.522746528602767));
#63856=CARTESIAN_POINT('Ctrl Pts',(-4.07426172299496,1.,0.526740277226999));
#63857=CARTESIAN_POINT('Ctrl Pts',(-4.08088789536488,1.,0.530769518728075));
#63858=CARTESIAN_POINT('Ctrl Pts',(-4.08750259988693,1.,0.534833963476999));
#63859=CARTESIAN_POINT('Ctrl Pts',(-4.09410597627116,1.,0.53893332117992));
#63860=CARTESIAN_POINT('Ctrl Pts',(-4.10069810244473,1.,0.543067286878457));
#63861=CARTESIAN_POINT('Ctrl Pts',(-4.1072789702877,1.,0.547235539486759));
#63862=CARTESIAN_POINT('Ctrl Pts',(-4.11384852025578,1.,0.551437758498246));
#63863=CARTESIAN_POINT('Ctrl Pts',(-4.1204066619623,1.,0.555673636130778));
#63864=CARTESIAN_POINT('Ctrl Pts',(-4.12695329951859,1.,0.559942890594628));
#63865=CARTESIAN_POINT('Ctrl Pts',(-4.13348835726086,1.,0.564245279535705));
#63866=CARTESIAN_POINT('Ctrl Pts',(-4.14001179828669,1.,0.568580610187116));
#63867=CARTESIAN_POINT('Ctrl Pts',(-4.14652361065787,1.,0.572948736066276));
#63868=CARTESIAN_POINT('Ctrl Pts',(-4.1517237611974,1.,0.576469391673916));
#63869=CARTESIAN_POINT('Ctrl Pts',(-4.15561864787379,1.,0.579124568912543));
#63870=CARTESIAN_POINT('Ctrl Pts',(-4.15821291712391,1.,0.580901211462913));
#63871=CARTESIAN_POINT('Ctrl Pts',(-4.15950947128175,1.,0.581791163835814));
#63872=CARTESIAN_POINT('Origin',(-4.15950947128175,0.,0.581791163835814));
#63873=CARTESIAN_POINT('',(-4.13571194405636,1.,0.732042837400619));
#63874=CARTESIAN_POINT('Origin',(0.,0.,0.));
#63875=CARTESIAN_POINT('',(-3.74449296982994,1.,0.203156094897896));
#63876=CARTESIAN_POINT('Origin',(0.,1.,0.));
#63877=CARTESIAN_POINT('Ctrl Pts',(-3.74449296982994,1.,0.203156094897896));
#63878=CARTESIAN_POINT('Ctrl Pts',(-3.74449296982994,0.666666666666667,
0.203156094897896));
#63879=CARTESIAN_POINT('Ctrl Pts',(-3.74449296982994,0.333333333333333,
0.203156094897896));
#63880=CARTESIAN_POINT('Ctrl Pts',(-3.74449296982994,-0.333333333333333,
0.203156094897896));
#63881=CARTESIAN_POINT('Ctrl Pts',(-3.74449296982994,-0.666666666666667,
0.203156094897896));
#63882=CARTESIAN_POINT('Ctrl Pts',(-3.74449296982994,-1.,0.203156094897896));
#63883=CARTESIAN_POINT('Ctrl Pts',(-4.19931119685982,-1.,0.0760622897878236));
#63884=CARTESIAN_POINT('Ctrl Pts',(-4.19931119685982,1.,0.0760622897878236));
#63885=CARTESIAN_POINT('Ctrl Pts',(-4.19789138621624,-1.,0.0767384596142195));
#63886=CARTESIAN_POINT('Ctrl Pts',(-4.19789138621624,1.,0.0767384596142195));
#63887=CARTESIAN_POINT('Ctrl Pts',(-4.19505112860624,-1.,0.0780873956244402));
#63888=CARTESIAN_POINT('Ctrl Pts',(-4.19505112860624,1.,0.0780873956244402));
#63889=CARTESIAN_POINT('Ctrl Pts',(-4.19078883322483,-1.,0.0801005887117603));
#63890=CARTESIAN_POINT('Ctrl Pts',(-4.19078883322483,1.,0.0801005887117603));
#63891=CARTESIAN_POINT('Ctrl Pts',(-4.1851019532944,-1.,0.082764416438951));
#63892=CARTESIAN_POINT('Ctrl Pts',(-4.1851019532944,1.,0.082764416438951));
#63893=CARTESIAN_POINT('Ctrl Pts',(-4.17798698669991,-1.,0.0860600915552515));
#63894=CARTESIAN_POINT('Ctrl Pts',(-4.17798698669991,1.,0.0860600915552515));
#63895=CARTESIAN_POINT('Ctrl Pts',(-4.17086566491823,-1.,0.0893215560850327));
#63896=CARTESIAN_POINT('Ctrl Pts',(-4.17086566491823,1.,0.0893215560850327));
#63897=CARTESIAN_POINT('Ctrl Pts',(-4.16373802265942,-1.,0.092548667216769));
#63898=CARTESIAN_POINT('Ctrl Pts',(-4.16373802265942,1.,0.092548667216769));
#63899=CARTESIAN_POINT('Ctrl Pts',(-4.15660412653006,-1.,0.0957412403297067));
#63900=CARTESIAN_POINT('Ctrl Pts',(-4.15660412653006,1.,0.0957412403297067));
#63901=CARTESIAN_POINT('Ctrl Pts',(-4.1494640891762,-1.,0.0988990478899811));
#63902=CARTESIAN_POINT('Ctrl Pts',(-4.1494640891762,1.,0.0988990478899811));
#63903=CARTESIAN_POINT('Ctrl Pts',(-4.14231804938737,-1.,0.102021826577454));
#63904=CARTESIAN_POINT('Ctrl Pts',(-4.14231804938737,1.,0.102021826577454));
#63905=CARTESIAN_POINT('Ctrl Pts',(-4.13516614458396,-1.,0.105109286538864));
#63906=CARTESIAN_POINT('Ctrl Pts',(-4.13516614458396,1.,0.105109286538864));
#63907=CARTESIAN_POINT('Ctrl Pts',(-4.12800848371386,-1.,0.10816112052835));
#63908=CARTESIAN_POINT('Ctrl Pts',(-4.12800848371386,1.,0.10816112052835));
#63909=CARTESIAN_POINT('Ctrl Pts',(-4.12084512502444,-1.,0.111177012683377));
#63910=CARTESIAN_POINT('Ctrl Pts',(-4.12084512502444,1.,0.111177012683377));
#63911=CARTESIAN_POINT('Ctrl Pts',(-4.11367603925313,-1.,0.114156649609601));
#63912=CARTESIAN_POINT('Ctrl Pts',(-4.11367603925313,1.,0.114156649609601));
#63913=CARTESIAN_POINT('Ctrl Pts',(-4.10650113382187,-1.,0.117099722731704));
#63914=CARTESIAN_POINT('Ctrl Pts',(-4.10650113382187,1.,0.117099722731704));
#63915=CARTESIAN_POINT('Ctrl Pts',(-4.09932031767243,-1.,0.120005924388162));
#63916=CARTESIAN_POINT('Ctrl Pts',(-4.09932031767243,1.,0.120005924388162));
#63917=CARTESIAN_POINT('Ctrl Pts',(-4.09213355850836,-1.,0.122874946249119));
#63918=CARTESIAN_POINT('Ctrl Pts',(-4.09213355850836,1.,0.122874946249119));
#63919=CARTESIAN_POINT('Ctrl Pts',(-4.08494093372315,-1.,0.125706476822529));
#63920=CARTESIAN_POINT('Ctrl Pts',(-4.08494093372315,1.,0.125706476822529));
#63921=CARTESIAN_POINT('Ctrl Pts',(-4.07774270738809,-1.,0.128500200484814));
#63922=CARTESIAN_POINT('Ctrl Pts',(-4.07774270738809,1.,0.128500200484814));
#63923=CARTESIAN_POINT('Ctrl Pts',(-4.07053931528579,-1.,0.131255793548914));
#63924=CARTESIAN_POINT('Ctrl Pts',(-4.07053931528579,1.,0.131255793548914));
#63925=CARTESIAN_POINT('Ctrl Pts',(-4.06333121018476,-1.,0.133972916144225));
#63926=CARTESIAN_POINT('Ctrl Pts',(-4.06333121018476,1.,0.133972916144225));
#63927=CARTESIAN_POINT('Ctrl Pts',(-4.05611873400122,-1.,0.136651205046111));
#63928=CARTESIAN_POINT('Ctrl Pts',(-4.05611873400122,1.,0.136651205046111));
#63929=CARTESIAN_POINT('Ctrl Pts',(-4.04890199238056,-1.,0.139290267180059));
#63930=CARTESIAN_POINT('Ctrl Pts',(-4.04890199238056,1.,0.139290267180059));
#63931=CARTESIAN_POINT('Ctrl Pts',(-4.04168069633842,-1.,0.141889671485508));
#63932=CARTESIAN_POINT('Ctrl Pts',(-4.04168069633842,1.,0.141889671485508));
#63933=CARTESIAN_POINT('Ctrl Pts',(-4.03445411510403,-1.,0.144448947038352));
#63934=CARTESIAN_POINT('Ctrl Pts',(-4.03445411510403,1.,0.144448947038352));
#63935=CARTESIAN_POINT('Ctrl Pts',(-4.02722143147048,-1.,0.146967602878998));
#63936=CARTESIAN_POINT('Ctrl Pts',(-4.02722143147048,1.,0.146967602878998));
#63937=CARTESIAN_POINT('Ctrl Pts',(-4.01998203715588,-1.,0.149445144968707));
#63938=CARTESIAN_POINT('Ctrl Pts',(-4.01998203715588,1.,0.149445144968707));
#63939=CARTESIAN_POINT('Ctrl Pts',(-4.01273584234684,-1.,0.151881094022909));
#63940=CARTESIAN_POINT('Ctrl Pts',(-4.01273584234684,1.,0.151881094022909));
#63941=CARTESIAN_POINT('Ctrl Pts',(-4.00548360245297,-1.,0.15427500487231));
#63942=CARTESIAN_POINT('Ctrl Pts',(-4.00548360245297,1.,0.15427500487231));
#63943=CARTESIAN_POINT('Ctrl Pts',(-3.99822717425869,-1.,0.156626481393735));
#63944=CARTESIAN_POINT('Ctrl Pts',(-3.99822717425869,1.,0.156626481393735));
#63945=CARTESIAN_POINT('Ctrl Pts',(-3.99096873945862,-1.,0.158935123982796));
#63946=CARTESIAN_POINT('Ctrl Pts',(-3.99096873945862,1.,0.158935123982796));
#63947=CARTESIAN_POINT('Ctrl Pts',(-3.98371010319866,-1.,0.161200482186087));
#63948=CARTESIAN_POINT('Ctrl Pts',(-3.98371010319866,1.,0.161200482186087));
#63949=CARTESIAN_POINT('Ctrl Pts',(-3.97645194630944,-1.,0.163422004609999));
#63950=CARTESIAN_POINT('Ctrl Pts',(-3.97645194630944,1.,0.163422004609999));
#63951=CARTESIAN_POINT('Ctrl Pts',(-3.9691931362141,-1.,0.165598992851097));
#63952=CARTESIAN_POINT('Ctrl Pts',(-3.9691931362141,1.,0.165598992851097));
#63953=CARTESIAN_POINT('Ctrl Pts',(-3.96192990160296,-1.,0.167730547023312));
#63954=CARTESIAN_POINT('Ctrl Pts',(-3.96192990160296,1.,0.167730547023312));
#63955=CARTESIAN_POINT('Ctrl Pts',(-3.95465744665263,-1.,0.16981566637413));
#63956=CARTESIAN_POINT('Ctrl Pts',(-3.95465744665263,1.,0.16981566637413));
#63957=CARTESIAN_POINT('Ctrl Pts',(-3.94737164900861,-1.,0.171853355369233));
#63958=CARTESIAN_POINT('Ctrl Pts',(-3.94737164900861,1.,0.171853355369233));
#63959=CARTESIAN_POINT('Ctrl Pts',(-3.94007083096214,-1.,0.173842734974607));
#63960=CARTESIAN_POINT('Ctrl Pts',(-3.94007083096214,1.,0.173842734974607));
#63961=CARTESIAN_POINT('Ctrl Pts',(-3.93275726771049,-1.,0.175783136893872));
#63962=CARTESIAN_POINT('Ctrl Pts',(-3.93275726771049,1.,0.175783136893872));
#63963=CARTESIAN_POINT('Ctrl Pts',(-3.92543942697672,-1.,0.177674246152328));
#63964=CARTESIAN_POINT('Ctrl Pts',(-3.92543942697672,1.,0.177674246152328));
#63965=CARTESIAN_POINT('Ctrl Pts',(-3.91812876180948,-1.,0.179515885822894));
#63966=CARTESIAN_POINT('Ctrl Pts',(-3.91812876180948,1.,0.179515885822894));
#63967=CARTESIAN_POINT('Ctrl Pts',(-3.91083557557193,-1.,0.181307740731796));
#63968=CARTESIAN_POINT('Ctrl Pts',(-3.91083557557193,1.,0.181307740731796));
#63969=CARTESIAN_POINT('Ctrl Pts',(-3.90356488555138,-1.,0.183049081993193));
#63970=CARTESIAN_POINT('Ctrl Pts',(-3.90356488555138,1.,0.183049081993193));
#63971=CARTESIAN_POINT('Ctrl Pts',(-3.89631300742633,-1.,0.184738537728035));
#63972=CARTESIAN_POINT('Ctrl Pts',(-3.89631300742633,1.,0.184738537728035));
#63973=CARTESIAN_POINT('Ctrl Pts',(-3.88906196725817,-1.,0.186373724985263));
#63974=CARTESIAN_POINT('Ctrl Pts',(-3.88906196725817,1.,0.186373724985263));
#63975=CARTESIAN_POINT('Ctrl Pts',(-3.88178563496187,-1.,0.187951632512663));
#63976=CARTESIAN_POINT('Ctrl Pts',(-3.88178563496187,1.,0.187951632512663));
#63977=CARTESIAN_POINT('Ctrl Pts',(-3.87445976418377,-1.,0.189469253358254));
#63978=CARTESIAN_POINT('Ctrl Pts',(-3.87445976418377,1.,0.189469253358254));
#63979=CARTESIAN_POINT('Ctrl Pts',(-3.8670715862477,-1.,0.190924190418613));
#63980=CARTESIAN_POINT('Ctrl Pts',(-3.8670715862477,1.,0.190924190418613));
#63981=CARTESIAN_POINT('Ctrl Pts',(-3.85962774407652,-1.,0.192315153044979));
#63982=CARTESIAN_POINT('Ctrl Pts',(-3.85962774407652,1.,0.192315153044979));
#63983=CARTESIAN_POINT('Ctrl Pts',(-3.85216762264019,-1.,0.193642806777747));
#63984=CARTESIAN_POINT('Ctrl Pts',(-3.85216762264019,1.,0.193642806777747));
#63985=CARTESIAN_POINT('Ctrl Pts',(-3.84475203347052,-1.,0.194909009460254));
#63986=CARTESIAN_POINT('Ctrl Pts',(-3.84475203347052,1.,0.194909009460254));
#63987=CARTESIAN_POINT('Ctrl Pts',(-3.83743910616265,-1.,0.196115198971889));
#63988=CARTESIAN_POINT('Ctrl Pts',(-3.83743910616265,1.,0.196115198971889));
#63989=CARTESIAN_POINT('Ctrl Pts',(-3.83026221776488,-1.,0.197260935827375));
#63990=CARTESIAN_POINT('Ctrl Pts',(-3.83026221776488,1.,0.197260935827375));
#63991=CARTESIAN_POINT('Ctrl Pts',(-3.82321127348981,-1.,0.19834261690047));
#63992=CARTESIAN_POINT('Ctrl Pts',(-3.82321127348981,1.,0.19834261690047));
#63993=CARTESIAN_POINT('Ctrl Pts',(-3.81620203429702,-1.,0.199351525297396));
#63994=CARTESIAN_POINT('Ctrl Pts',(-3.81620203429702,1.,0.199351525297396));
#63995=CARTESIAN_POINT('Ctrl Pts',(-3.80909529318501,-1.,0.20027467943329));
#63996=CARTESIAN_POINT('Ctrl Pts',(-3.80909529318501,1.,0.20027467943329));
#63997=CARTESIAN_POINT('Ctrl Pts',(-3.80175247447171,-1.,0.201097756307252));
#63998=CARTESIAN_POINT('Ctrl Pts',(-3.80175247447171,1.,0.201097756307252));
#63999=CARTESIAN_POINT('Ctrl Pts',(-3.79408354187274,-1.,0.201807533800799));
#64000=CARTESIAN_POINT('Ctrl Pts',(-3.79408354187274,1.,0.201807533800799));
#64001=CARTESIAN_POINT('Ctrl Pts',(-3.78609175019317,-1.,0.202394260512193));
#64002=CARTESIAN_POINT('Ctrl Pts',(-3.78609175019317,1.,0.202394260512193));
#64003=CARTESIAN_POINT('Ctrl Pts',(-3.77793553476879,-1.,0.202854729699196));
#64004=CARTESIAN_POINT('Ctrl Pts',(-3.77793553476879,1.,0.202854729699196));
#64005=CARTESIAN_POINT('Ctrl Pts',(-3.76992071595267,-1.,0.203192390045337));
#64006=CARTESIAN_POINT('Ctrl Pts',(-3.76992071595267,1.,0.203192390045337));
#64007=CARTESIAN_POINT('Ctrl Pts',(-3.76242717937273,-1.,0.203414634707646));
#64008=CARTESIAN_POINT('Ctrl Pts',(-3.76242717937273,1.,0.203414634707646));
#64009=CARTESIAN_POINT('Ctrl Pts',(-3.75585118707924,-1.,0.203530796848403));
#64010=CARTESIAN_POINT('Ctrl Pts',(-3.75585118707924,1.,0.203530796848403));
#64011=CARTESIAN_POINT('Ctrl Pts',(-3.75054693397716,-1.,0.203550035479097));
#64012=CARTESIAN_POINT('Ctrl Pts',(-3.75054693397716,1.,0.203550035479097));
#64013=CARTESIAN_POINT('Ctrl Pts',(-3.74675472018582,-1.,0.203478844530229));
#64014=CARTESIAN_POINT('Ctrl Pts',(-3.74675472018582,1.,0.203478844530229));
#64015=CARTESIAN_POINT('Ctrl Pts',(-3.7450208092684,-1.,0.203352057956055));
#64016=CARTESIAN_POINT('Ctrl Pts',(-3.7450208092684,1.,0.203352057956055));
#64017=CARTESIAN_POINT('Ctrl Pts',(-3.74446880195845,-1.,0.203218215747894));
#64018=CARTESIAN_POINT('Ctrl Pts',(-3.74446880195845,1.,0.203218215747894));
#64019=CARTESIAN_POINT('Ctrl Pts',(-3.74443319346666,-1.,0.20311176758786));
#64020=CARTESIAN_POINT('Ctrl Pts',(-3.74443319346666,1.,0.20311176758786));
#64021=CARTESIAN_POINT('Ctrl Pts',(-3.74449849461127,-1.,0.203054238699719));
#64022=CARTESIAN_POINT('Ctrl Pts',(-3.74449849461127,1.,0.203054238699719));
#64023=CARTESIAN_POINT('',(-4.19931119685982,1.,0.0760622897878236));
#64024=CARTESIAN_POINT('Ctrl Pts',(-4.19931119685982,1.,0.0760622897878236));
#64025=CARTESIAN_POINT('Ctrl Pts',(-4.19789138621624,1.,0.0767384596142195));
#64026=CARTESIAN_POINT('Ctrl Pts',(-4.19505112860624,1.,0.0780873956244402));
#64027=CARTESIAN_POINT('Ctrl Pts',(-4.19078883322483,1.,0.0801005887117603));
#64028=CARTESIAN_POINT('Ctrl Pts',(-4.1851019532944,1.,0.082764416438951));
#64029=CARTESIAN_POINT('Ctrl Pts',(-4.17798698669991,1.,0.0860600915552515));
#64030=CARTESIAN_POINT('Ctrl Pts',(-4.17086566491823,1.,0.0893215560850327));
#64031=CARTESIAN_POINT('Ctrl Pts',(-4.16373802265942,1.,0.092548667216769));
#64032=CARTESIAN_POINT('Ctrl Pts',(-4.15660412653006,1.,0.0957412403297067));
#64033=CARTESIAN_POINT('Ctrl Pts',(-4.1494640891762,1.,0.0988990478899811));
#64034=CARTESIAN_POINT('Ctrl Pts',(-4.14231804938737,1.,0.102021826577454));
#64035=CARTESIAN_POINT('Ctrl Pts',(-4.13516614458396,1.,0.105109286538864));
#64036=CARTESIAN_POINT('Ctrl Pts',(-4.12800848371386,1.,0.10816112052835));
#64037=CARTESIAN_POINT('Ctrl Pts',(-4.12084512502444,1.,0.111177012683377));
#64038=CARTESIAN_POINT('Ctrl Pts',(-4.11367603925313,1.,0.114156649609601));
#64039=CARTESIAN_POINT('Ctrl Pts',(-4.10650113382187,1.,0.117099722731704));
#64040=CARTESIAN_POINT('Ctrl Pts',(-4.09932031767243,1.,0.120005924388162));
#64041=CARTESIAN_POINT('Ctrl Pts',(-4.09213355850836,1.,0.122874946249119));
#64042=CARTESIAN_POINT('Ctrl Pts',(-4.08494093372315,1.,0.125706476822529));
#64043=CARTESIAN_POINT('Ctrl Pts',(-4.07774270738809,1.,0.128500200484814));
#64044=CARTESIAN_POINT('Ctrl Pts',(-4.07053931528579,1.,0.131255793548914));
#64045=CARTESIAN_POINT('Ctrl Pts',(-4.06333121018476,1.,0.133972916144225));
#64046=CARTESIAN_POINT('Ctrl Pts',(-4.05611873400122,1.,0.136651205046111));
#64047=CARTESIAN_POINT('Ctrl Pts',(-4.04890199238056,1.,0.139290267180059));
#64048=CARTESIAN_POINT('Ctrl Pts',(-4.04168069633842,1.,0.141889671485508));
#64049=CARTESIAN_POINT('Ctrl Pts',(-4.03445411510403,1.,0.144448947038352));
#64050=CARTESIAN_POINT('Ctrl Pts',(-4.02722143147048,1.,0.146967602878998));
#64051=CARTESIAN_POINT('Ctrl Pts',(-4.01998203715588,1.,0.149445144968707));
#64052=CARTESIAN_POINT('Ctrl Pts',(-4.01273584234684,1.,0.151881094022909));
#64053=CARTESIAN_POINT('Ctrl Pts',(-4.00548360245297,1.,0.15427500487231));
#64054=CARTESIAN_POINT('Ctrl Pts',(-3.99822717425869,1.,0.156626481393735));
#64055=CARTESIAN_POINT('Ctrl Pts',(-3.99096873945862,1.,0.158935123982796));
#64056=CARTESIAN_POINT('Ctrl Pts',(-3.98371010319866,1.,0.161200482186087));
#64057=CARTESIAN_POINT('Ctrl Pts',(-3.97645194630944,1.,0.163422004609999));
#64058=CARTESIAN_POINT('Ctrl Pts',(-3.9691931362141,1.,0.165598992851097));
#64059=CARTESIAN_POINT('Ctrl Pts',(-3.96192990160296,1.,0.167730547023312));
#64060=CARTESIAN_POINT('Ctrl Pts',(-3.95465744665263,1.,0.16981566637413));
#64061=CARTESIAN_POINT('Ctrl Pts',(-3.94737164900861,1.,0.171853355369233));
#64062=CARTESIAN_POINT('Ctrl Pts',(-3.94007083096214,1.,0.173842734974607));
#64063=CARTESIAN_POINT('Ctrl Pts',(-3.93275726771049,1.,0.175783136893872));
#64064=CARTESIAN_POINT('Ctrl Pts',(-3.92543942697672,1.,0.177674246152328));
#64065=CARTESIAN_POINT('Ctrl Pts',(-3.91812876180948,1.,0.179515885822894));
#64066=CARTESIAN_POINT('Ctrl Pts',(-3.91083557557193,1.,0.181307740731796));
#64067=CARTESIAN_POINT('Ctrl Pts',(-3.90356488555138,1.,0.183049081993193));
#64068=CARTESIAN_POINT('Ctrl Pts',(-3.89631300742633,1.,0.184738537728035));
#64069=CARTESIAN_POINT('Ctrl Pts',(-3.88906196725817,1.,0.186373724985263));
#64070=CARTESIAN_POINT('Ctrl Pts',(-3.88178563496187,1.,0.187951632512663));
#64071=CARTESIAN_POINT('Ctrl Pts',(-3.87445976418377,1.,0.189469253358254));
#64072=CARTESIAN_POINT('Ctrl Pts',(-3.8670715862477,1.,0.190924190418613));
#64073=CARTESIAN_POINT('Ctrl Pts',(-3.85962774407652,1.,0.192315153044979));
#64074=CARTESIAN_POINT('Ctrl Pts',(-3.85216762264019,1.,0.193642806777747));
#64075=CARTESIAN_POINT('Ctrl Pts',(-3.84475203347052,1.,0.194909009460254));
#64076=CARTESIAN_POINT('Ctrl Pts',(-3.83743910616265,1.,0.196115198971889));
#64077=CARTESIAN_POINT('Ctrl Pts',(-3.83026221776488,1.,0.197260935827375));
#64078=CARTESIAN_POINT('Ctrl Pts',(-3.82321127348981,1.,0.19834261690047));
#64079=CARTESIAN_POINT('Ctrl Pts',(-3.81620203429702,1.,0.199351525297396));
#64080=CARTESIAN_POINT('Ctrl Pts',(-3.80909529318501,1.,0.20027467943329));
#64081=CARTESIAN_POINT('Ctrl Pts',(-3.80175247447171,1.,0.201097756307252));
#64082=CARTESIAN_POINT('Ctrl Pts',(-3.79408354187274,1.,0.201807533800799));
#64083=CARTESIAN_POINT('Ctrl Pts',(-3.78609175019317,1.,0.202394260512193));
#64084=CARTESIAN_POINT('Ctrl Pts',(-3.77793553476879,1.,0.202854729699196));
#64085=CARTESIAN_POINT('Ctrl Pts',(-3.76992071595267,1.,0.203192390045337));
#64086=CARTESIAN_POINT('Ctrl Pts',(-3.76242717937273,1.,0.203414634707646));
#64087=CARTESIAN_POINT('Ctrl Pts',(-3.75585118707924,1.,0.203530796848403));
#64088=CARTESIAN_POINT('Ctrl Pts',(-3.75054693397716,1.,0.203550035479097));
#64089=CARTESIAN_POINT('Ctrl Pts',(-3.74703926501843,1.,0.203484186269314));
#64090=CARTESIAN_POINT('Ctrl Pts',(-3.74535749969262,1.,0.203375226874331));
#64091=CARTESIAN_POINT('Ctrl Pts',(-3.74471097893961,1.,0.203266610111264));
#64092=CARTESIAN_POINT('Ctrl Pts',(-3.74453008995129,1.,0.203188003947965));
#64093=CARTESIAN_POINT('Ctrl Pts',(-3.74449296982994,1.,0.203156094897896));
#64094=CARTESIAN_POINT('',(-4.19931119685982,0.,0.0760622897878236));
#64095=CARTESIAN_POINT('Ctrl Pts',(-3.74449849461127,-1.,-0.20305423869972));
#64096=CARTESIAN_POINT('Ctrl Pts',(-3.74449849461127,1.,-0.20305423869972));
#64097=CARTESIAN_POINT('Ctrl Pts',(-3.7444331934681,-1.,-0.203111767587923));
#64098=CARTESIAN_POINT('Ctrl Pts',(-3.7444331934681,1.,-0.203111767587923));
#64099=CARTESIAN_POINT('Ctrl Pts',(-3.7444688019622,-1.,-0.203218215748059));
#64100=CARTESIAN_POINT('Ctrl Pts',(-3.7444688019622,1.,-0.203218215748059));
#64101=CARTESIAN_POINT('Ctrl Pts',(-3.74502080927395,-1.,-0.203352057956297));
#64102=CARTESIAN_POINT('Ctrl Pts',(-3.74502080927395,1.,-0.203352057956297));
#64103=CARTESIAN_POINT('Ctrl Pts',(-3.7467547201908,-1.,-0.203478844530447));
#64104=CARTESIAN_POINT('Ctrl Pts',(-3.7467547201908,1.,-0.203478844530447));
#64105=CARTESIAN_POINT('Ctrl Pts',(-3.75054693397875,-1.,-0.203550035479166));
#64106=CARTESIAN_POINT('Ctrl Pts',(-3.75054693397875,1.,-0.203550035479166));
#64107=CARTESIAN_POINT('Ctrl Pts',(-3.75585118707734,-1.,-0.203530796848322));
#64108=CARTESIAN_POINT('Ctrl Pts',(-3.75585118707734,1.,-0.203530796848322));
#64109=CARTESIAN_POINT('Ctrl Pts',(-3.76242717936885,-1.,-0.203414634707478));
#64110=CARTESIAN_POINT('Ctrl Pts',(-3.76242717936885,1.,-0.203414634707478));
#64111=CARTESIAN_POINT('Ctrl Pts',(-3.7699207159487,-1.,-0.203192390045164));
#64112=CARTESIAN_POINT('Ctrl Pts',(-3.7699207159487,1.,-0.203192390045164));
#64113=CARTESIAN_POINT('Ctrl Pts',(-3.77793553476614,-1.,-0.202854729699081));
#64114=CARTESIAN_POINT('Ctrl Pts',(-3.77793553476614,1.,-0.202854729699081));
#64115=CARTESIAN_POINT('Ctrl Pts',(-3.78609175019242,-1.,-0.20239426051216));
#64116=CARTESIAN_POINT('Ctrl Pts',(-3.78609175019242,1.,-0.20239426051216));
#64117=CARTESIAN_POINT('Ctrl Pts',(-3.7940835418736,-1.,-0.201807533800837));
#64118=CARTESIAN_POINT('Ctrl Pts',(-3.7940835418736,1.,-0.201807533800837));
#64119=CARTESIAN_POINT('Ctrl Pts',(-3.80175247447337,-1.,-0.201097756307326));
#64120=CARTESIAN_POINT('Ctrl Pts',(-3.80175247447337,1.,-0.201097756307326));
#64121=CARTESIAN_POINT('Ctrl Pts',(-3.80909529318669,-1.,-0.200274679433364));
#64122=CARTESIAN_POINT('Ctrl Pts',(-3.80909529318669,1.,-0.200274679433364));
#64123=CARTESIAN_POINT('Ctrl Pts',(-3.81620203429815,-1.,-0.199351525297447));
#64124=CARTESIAN_POINT('Ctrl Pts',(-3.81620203429815,1.,-0.199351525297447));
#64125=CARTESIAN_POINT('Ctrl Pts',(-3.82321127349016,-1.,-0.198342616900486));
#64126=CARTESIAN_POINT('Ctrl Pts',(-3.82321127349016,1.,-0.198342616900486));
#64127=CARTESIAN_POINT('Ctrl Pts',(-3.83026221776456,-1.,-0.197260935827361));
#64128=CARTESIAN_POINT('Ctrl Pts',(-3.83026221776456,1.,-0.197260935827361));
#64129=CARTESIAN_POINT('Ctrl Pts',(-3.83743910616195,-1.,-0.196115198971859));
#64130=CARTESIAN_POINT('Ctrl Pts',(-3.83743910616195,1.,-0.196115198971859));
#64131=CARTESIAN_POINT('Ctrl Pts',(-3.84475203346977,-1.,-0.194909009460221));
#64132=CARTESIAN_POINT('Ctrl Pts',(-3.84475203346977,1.,-0.194909009460221));
#64133=CARTESIAN_POINT('Ctrl Pts',(-3.85216762263966,-1.,-0.193642806777723));
#64134=CARTESIAN_POINT('Ctrl Pts',(-3.85216762263966,1.,-0.193642806777723));
#64135=CARTESIAN_POINT('Ctrl Pts',(-3.85962774407633,-1.,-0.192315153044971));
#64136=CARTESIAN_POINT('Ctrl Pts',(-3.85962774407633,1.,-0.192315153044971));
#64137=CARTESIAN_POINT('Ctrl Pts',(-3.86707158624783,-1.,-0.19092419041862));
#64138=CARTESIAN_POINT('Ctrl Pts',(-3.86707158624783,1.,-0.19092419041862));
#64139=CARTESIAN_POINT('Ctrl Pts',(-3.87445976418412,-1.,-0.189469253358272));
#64140=CARTESIAN_POINT('Ctrl Pts',(-3.87445976418412,1.,-0.189469253358272));
#64141=CARTESIAN_POINT('Ctrl Pts',(-3.88178563496228,-1.,-0.187951632512685));
#64142=CARTESIAN_POINT('Ctrl Pts',(-3.88178563496228,1.,-0.187951632512685));
#64143=CARTESIAN_POINT('Ctrl Pts',(-3.88906196725848,-1.,-0.18637372498528));
#64144=CARTESIAN_POINT('Ctrl Pts',(-3.88906196725848,1.,-0.18637372498528));
#64145=CARTESIAN_POINT('Ctrl Pts',(-3.89631300742646,-1.,-0.184738537728043));
#64146=CARTESIAN_POINT('Ctrl Pts',(-3.89631300742646,1.,-0.184738537728043));
#64147=CARTESIAN_POINT('Ctrl Pts',(-3.90356488555132,-1.,-0.183049081993191));
#64148=CARTESIAN_POINT('Ctrl Pts',(-3.90356488555132,1.,-0.183049081993191));
#64149=CARTESIAN_POINT('Ctrl Pts',(-3.91083557557175,-1.,-0.181307740731786));
#64150=CARTESIAN_POINT('Ctrl Pts',(-3.91083557557175,1.,-0.181307740731786));
#64151=CARTESIAN_POINT('Ctrl Pts',(-3.91812876180926,-1.,-0.179515885822882));
#64152=CARTESIAN_POINT('Ctrl Pts',(-3.91812876180926,1.,-0.179515885822882));
#64153=CARTESIAN_POINT('Ctrl Pts',(-3.92543942697655,-1.,-0.177674246152317));
#64154=CARTESIAN_POINT('Ctrl Pts',(-3.92543942697655,1.,-0.177674246152317));
#64155=CARTESIAN_POINT('Ctrl Pts',(-3.93275726771042,-1.,-0.175783136893868));
#64156=CARTESIAN_POINT('Ctrl Pts',(-3.93275726771042,1.,-0.175783136893868));
#64157=CARTESIAN_POINT('Ctrl Pts',(-3.94007083096217,-1.,-0.17384273497461));
#64158=CARTESIAN_POINT('Ctrl Pts',(-3.94007083096217,1.,-0.17384273497461));
#64159=CARTESIAN_POINT('Ctrl Pts',(-3.94737164900868,-1.,-0.17185335536924));
#64160=CARTESIAN_POINT('Ctrl Pts',(-3.94737164900868,1.,-0.17185335536924));
#64161=CARTESIAN_POINT('Ctrl Pts',(-3.95465744665268,-1.,-0.169815666374139));
#64162=CARTESIAN_POINT('Ctrl Pts',(-3.95465744665268,1.,-0.169815666374139));
#64163=CARTESIAN_POINT('Ctrl Pts',(-3.96192990160296,-1.,-0.167730547023319));
#64164=CARTESIAN_POINT('Ctrl Pts',(-3.96192990160296,1.,-0.167730547023319));
#64165=CARTESIAN_POINT('Ctrl Pts',(-3.96919313621407,-1.,-0.165598992851102));
#64166=CARTESIAN_POINT('Ctrl Pts',(-3.96919313621407,1.,-0.165598992851102));
#64167=CARTESIAN_POINT('Ctrl Pts',(-3.97645194630943,-1.,-0.163422004609999));
#64168=CARTESIAN_POINT('Ctrl Pts',(-3.97645194630943,1.,-0.163422004609999));
#64169=CARTESIAN_POINT('Ctrl Pts',(-3.98371010319872,-1.,-0.161200482186085));
#64170=CARTESIAN_POINT('Ctrl Pts',(-3.98371010319872,1.,-0.161200482186085));
#64171=CARTESIAN_POINT('Ctrl Pts',(-3.99096873945878,-1.,-0.158935123982793));
#64172=CARTESIAN_POINT('Ctrl Pts',(-3.99096873945878,1.,-0.158935123982793));
#64173=CARTESIAN_POINT('Ctrl Pts',(-3.99822717425893,-1.,-0.156626481393734));
#64174=CARTESIAN_POINT('Ctrl Pts',(-3.99822717425893,1.,-0.156626481393734));
#64175=CARTESIAN_POINT('Ctrl Pts',(-4.00548360245319,-1.,-0.154275004872311));
#64176=CARTESIAN_POINT('Ctrl Pts',(-4.00548360245319,1.,-0.154275004872311));
#64177=CARTESIAN_POINT('Ctrl Pts',(-4.01273584234689,-1.,-0.151881094022911));
#64178=CARTESIAN_POINT('Ctrl Pts',(-4.01273584234689,1.,-0.151881094022911));
#64179=CARTESIAN_POINT('Ctrl Pts',(-4.01998203715564,-1.,-0.149445144968707));
#64180=CARTESIAN_POINT('Ctrl Pts',(-4.01998203715564,1.,-0.149445144968707));
#64181=CARTESIAN_POINT('Ctrl Pts',(-4.02722143146994,-1.,-0.146967602878994));
#64182=CARTESIAN_POINT('Ctrl Pts',(-4.02722143146994,1.,-0.146967602878994));
#64183=CARTESIAN_POINT('Ctrl Pts',(-4.03445411510333,-1.,-0.144448947038345));
#64184=CARTESIAN_POINT('Ctrl Pts',(-4.03445411510333,1.,-0.144448947038345));
#64185=CARTESIAN_POINT('Ctrl Pts',(-4.04168069633781,-1.,-0.1418896714855));
#64186=CARTESIAN_POINT('Ctrl Pts',(-4.04168069633781,1.,-0.1418896714855));
#64187=CARTESIAN_POINT('Ctrl Pts',(-4.04890199238036,-1.,-0.139290267180057));
#64188=CARTESIAN_POINT('Ctrl Pts',(-4.04890199238036,1.,-0.139290267180057));
#64189=CARTESIAN_POINT('Ctrl Pts',(-4.05611873400172,-1.,-0.136651205046119));
#64190=CARTESIAN_POINT('Ctrl Pts',(-4.05611873400172,1.,-0.136651205046119));
#64191=CARTESIAN_POINT('Ctrl Pts',(-4.06333121018596,-1.,-0.133972916144245));
#64192=CARTESIAN_POINT('Ctrl Pts',(-4.06333121018596,1.,-0.133972916144245));
#64193=CARTESIAN_POINT('Ctrl Pts',(-4.0705393152874,-1.,-0.13125579354894));
#64194=CARTESIAN_POINT('Ctrl Pts',(-4.0705393152874,1.,-0.13125579354894));
#64195=CARTESIAN_POINT('Ctrl Pts',(-4.07774270738954,-1.,-0.128500200484838));
#64196=CARTESIAN_POINT('Ctrl Pts',(-4.07774270738954,1.,-0.128500200484838));
#64197=CARTESIAN_POINT('Ctrl Pts',(-4.08494093372377,-1.,-0.12570647682254));
#64198=CARTESIAN_POINT('Ctrl Pts',(-4.08494093372377,1.,-0.12570647682254));
#64199=CARTESIAN_POINT('Ctrl Pts',(-4.09213355850756,-1.,-0.122874946249107));
#64200=CARTESIAN_POINT('Ctrl Pts',(-4.09213355850756,1.,-0.122874946249107));
#64201=CARTESIAN_POINT('Ctrl Pts',(-4.09932031767002,-1.,-0.120005924388124));
#64202=CARTESIAN_POINT('Ctrl Pts',(-4.09932031767002,1.,-0.120005924388124));
#64203=CARTESIAN_POINT('Ctrl Pts',(-4.10650113381833,-1.,-0.117099722731648));
#64204=CARTESIAN_POINT('Ctrl Pts',(-4.10650113381833,1.,-0.117099722731648));
#64205=CARTESIAN_POINT('Ctrl Pts',(-4.11367603924961,-1.,-0.114156649609546));
#64206=CARTESIAN_POINT('Ctrl Pts',(-4.11367603924961,1.,-0.114156649609546));
#64207=CARTESIAN_POINT('Ctrl Pts',(-4.1208451250225,-1.,-0.111177012683347));
#64208=CARTESIAN_POINT('Ctrl Pts',(-4.1208451250225,1.,-0.111177012683347));
#64209=CARTESIAN_POINT('Ctrl Pts',(-4.12800848371504,-1.,-0.108161120528369));
#64210=CARTESIAN_POINT('Ctrl Pts',(-4.12800848371504,1.,-0.108161120528369));
#64211=CARTESIAN_POINT('Ctrl Pts',(-4.13516614458895,-1.,-0.105109286538945));
#64212=CARTESIAN_POINT('Ctrl Pts',(-4.13516614458895,1.,-0.105109286538945));
#64213=CARTESIAN_POINT('Ctrl Pts',(-4.14231804939538,-1.,-0.102021826577584));
#64214=CARTESIAN_POINT('Ctrl Pts',(-4.14231804939538,1.,-0.102021826577584));
#64215=CARTESIAN_POINT('Ctrl Pts',(-4.14946408918485,-1.,-0.0988990478901226));
#64216=CARTESIAN_POINT('Ctrl Pts',(-4.14946408918485,1.,-0.0988990478901226));
#64217=CARTESIAN_POINT('Ctrl Pts',(-4.15660412653577,-1.,-0.0957412403298007));
#64218=CARTESIAN_POINT('Ctrl Pts',(-4.15660412653577,1.,-0.0957412403298007));
#64219=CARTESIAN_POINT('Ctrl Pts',(-4.16373802265839,-1.,-0.0925486672167531));
#64220=CARTESIAN_POINT('Ctrl Pts',(-4.16373802265839,1.,-0.0925486672167531));
#64221=CARTESIAN_POINT('Ctrl Pts',(-4.17086566490794,-1.,-0.0893215560848649));
#64222=CARTESIAN_POINT('Ctrl Pts',(-4.17086566490794,1.,-0.0893215560848649));
#64223=CARTESIAN_POINT('Ctrl Pts',(-4.17798698668094,-1.,-0.0860600915549397));
#64224=CARTESIAN_POINT('Ctrl Pts',(-4.17798698668094,1.,-0.0860600915549397));
#64225=CARTESIAN_POINT('Ctrl Pts',(-4.18510195327123,-1.,-0.0827644164385679));
#64226=CARTESIAN_POINT('Ctrl Pts',(-4.18510195327123,1.,-0.0827644164385679));
#64227=CARTESIAN_POINT('Ctrl Pts',(-4.19078883320504,-1.,-0.080100588711432));
#64228=CARTESIAN_POINT('Ctrl Pts',(-4.19078883320504,1.,-0.080100588711432));
#64229=CARTESIAN_POINT('Ctrl Pts',(-4.19505112859416,-1.,-0.0780873956242397));
#64230=CARTESIAN_POINT('Ctrl Pts',(-4.19505112859416,1.,-0.0780873956242397));
#64231=CARTESIAN_POINT('Ctrl Pts',(-4.1978913862118,-1.,-0.0767384596141464));
#64232=CARTESIAN_POINT('Ctrl Pts',(-4.1978913862118,1.,-0.0767384596141464));
#64233=CARTESIAN_POINT('Ctrl Pts',(-4.19931119685982,-1.,-0.0760622897878246));
#64234=CARTESIAN_POINT('Ctrl Pts',(-4.19931119685982,1.,-0.0760622897878246));
#64235=CARTESIAN_POINT('',(-3.74449296983004,1.,-0.2031560948961));
#64236=CARTESIAN_POINT('Ctrl Pts',(-3.74449296983004,-1.,-0.203156094896101));
#64237=CARTESIAN_POINT('Ctrl Pts',(-3.74449296983004,-0.666666666666667,
-0.203156094896101));
#64238=CARTESIAN_POINT('Ctrl Pts',(-3.74449296983004,-0.333333333333333,
-0.203156094896101));
#64239=CARTESIAN_POINT('Ctrl Pts',(-3.74449296983004,0.333333333333333,
-0.203156094896101));
#64240=CARTESIAN_POINT('Ctrl Pts',(-3.74449296983004,0.666666666666667,
-0.203156094896101));
#64241=CARTESIAN_POINT('Ctrl Pts',(-3.74449296983004,1.,-0.203156094896101));
#64242=CARTESIAN_POINT('',(-4.19931119685982,1.,-0.0760622897878246));
#64243=CARTESIAN_POINT('',(-4.19931119685982,0.,-0.0760622897878246));
#64244=CARTESIAN_POINT('Ctrl Pts',(-3.74449296983004,1.,-0.203156094896101));
#64245=CARTESIAN_POINT('Ctrl Pts',(-3.74453008995092,1.,-0.203188003946657));
#64246=CARTESIAN_POINT('Ctrl Pts',(-3.74471097893844,1.,-0.203266610110531));
#64247=CARTESIAN_POINT('Ctrl Pts',(-3.74535749969115,1.,-0.203375226874121));
#64248=CARTESIAN_POINT('Ctrl Pts',(-3.74703926501752,1.,-0.203484186269415));
#64249=CARTESIAN_POINT('Ctrl Pts',(-3.75054693397875,1.,-0.203550035479166));
#64250=CARTESIAN_POINT('Ctrl Pts',(-3.75585118707734,1.,-0.203530796848322));
#64251=CARTESIAN_POINT('Ctrl Pts',(-3.76242717936885,1.,-0.203414634707478));
#64252=CARTESIAN_POINT('Ctrl Pts',(-3.7699207159487,1.,-0.203192390045164));
#64253=CARTESIAN_POINT('Ctrl Pts',(-3.77793553476614,1.,-0.202854729699081));
#64254=CARTESIAN_POINT('Ctrl Pts',(-3.78609175019242,1.,-0.20239426051216));
#64255=CARTESIAN_POINT('Ctrl Pts',(-3.7940835418736,1.,-0.201807533800837));
#64256=CARTESIAN_POINT('Ctrl Pts',(-3.80175247447337,1.,-0.201097756307326));
#64257=CARTESIAN_POINT('Ctrl Pts',(-3.80909529318669,1.,-0.200274679433364));
#64258=CARTESIAN_POINT('Ctrl Pts',(-3.81620203429815,1.,-0.199351525297447));
#64259=CARTESIAN_POINT('Ctrl Pts',(-3.82321127349016,1.,-0.198342616900486));
#64260=CARTESIAN_POINT('Ctrl Pts',(-3.83026221776456,1.,-0.197260935827361));
#64261=CARTESIAN_POINT('Ctrl Pts',(-3.83743910616195,1.,-0.196115198971859));
#64262=CARTESIAN_POINT('Ctrl Pts',(-3.84475203346977,1.,-0.194909009460221));
#64263=CARTESIAN_POINT('Ctrl Pts',(-3.85216762263966,1.,-0.193642806777723));
#64264=CARTESIAN_POINT('Ctrl Pts',(-3.85962774407633,1.,-0.192315153044971));
#64265=CARTESIAN_POINT('Ctrl Pts',(-3.86707158624783,1.,-0.19092419041862));
#64266=CARTESIAN_POINT('Ctrl Pts',(-3.87445976418412,1.,-0.189469253358272));
#64267=CARTESIAN_POINT('Ctrl Pts',(-3.88178563496228,1.,-0.187951632512685));
#64268=CARTESIAN_POINT('Ctrl Pts',(-3.88906196725848,1.,-0.18637372498528));
#64269=CARTESIAN_POINT('Ctrl Pts',(-3.89631300742646,1.,-0.184738537728043));
#64270=CARTESIAN_POINT('Ctrl Pts',(-3.90356488555132,1.,-0.183049081993191));
#64271=CARTESIAN_POINT('Ctrl Pts',(-3.91083557557175,1.,-0.181307740731786));
#64272=CARTESIAN_POINT('Ctrl Pts',(-3.91812876180926,1.,-0.179515885822882));
#64273=CARTESIAN_POINT('Ctrl Pts',(-3.92543942697655,1.,-0.177674246152317));
#64274=CARTESIAN_POINT('Ctrl Pts',(-3.93275726771042,1.,-0.175783136893868));
#64275=CARTESIAN_POINT('Ctrl Pts',(-3.94007083096217,1.,-0.17384273497461));
#64276=CARTESIAN_POINT('Ctrl Pts',(-3.94737164900868,1.,-0.17185335536924));
#64277=CARTESIAN_POINT('Ctrl Pts',(-3.95465744665268,1.,-0.169815666374139));
#64278=CARTESIAN_POINT('Ctrl Pts',(-3.96192990160296,1.,-0.167730547023319));
#64279=CARTESIAN_POINT('Ctrl Pts',(-3.96919313621407,1.,-0.165598992851102));
#64280=CARTESIAN_POINT('Ctrl Pts',(-3.97645194630943,1.,-0.163422004609999));
#64281=CARTESIAN_POINT('Ctrl Pts',(-3.98371010319872,1.,-0.161200482186085));
#64282=CARTESIAN_POINT('Ctrl Pts',(-3.99096873945878,1.,-0.158935123982793));
#64283=CARTESIAN_POINT('Ctrl Pts',(-3.99822717425893,1.,-0.156626481393734));
#64284=CARTESIAN_POINT('Ctrl Pts',(-4.00548360245319,1.,-0.154275004872311));
#64285=CARTESIAN_POINT('Ctrl Pts',(-4.01273584234689,1.,-0.151881094022911));
#64286=CARTESIAN_POINT('Ctrl Pts',(-4.01998203715564,1.,-0.149445144968707));
#64287=CARTESIAN_POINT('Ctrl Pts',(-4.02722143146994,1.,-0.146967602878994));
#64288=CARTESIAN_POINT('Ctrl Pts',(-4.03445411510333,1.,-0.144448947038345));
#64289=CARTESIAN_POINT('Ctrl Pts',(-4.04168069633781,1.,-0.1418896714855));
#64290=CARTESIAN_POINT('Ctrl Pts',(-4.04890199238036,1.,-0.139290267180057));
#64291=CARTESIAN_POINT('Ctrl Pts',(-4.05611873400172,1.,-0.136651205046119));
#64292=CARTESIAN_POINT('Ctrl Pts',(-4.06333121018596,1.,-0.133972916144245));
#64293=CARTESIAN_POINT('Ctrl Pts',(-4.0705393152874,1.,-0.13125579354894));
#64294=CARTESIAN_POINT('Ctrl Pts',(-4.07774270738954,1.,-0.128500200484838));
#64295=CARTESIAN_POINT('Ctrl Pts',(-4.08494093372377,1.,-0.12570647682254));
#64296=CARTESIAN_POINT('Ctrl Pts',(-4.09213355850756,1.,-0.122874946249107));
#64297=CARTESIAN_POINT('Ctrl Pts',(-4.09932031767002,1.,-0.120005924388124));
#64298=CARTESIAN_POINT('Ctrl Pts',(-4.10650113381833,1.,-0.117099722731648));
#64299=CARTESIAN_POINT('Ctrl Pts',(-4.11367603924961,1.,-0.114156649609546));
#64300=CARTESIAN_POINT('Ctrl Pts',(-4.1208451250225,1.,-0.111177012683347));
#64301=CARTESIAN_POINT('Ctrl Pts',(-4.12800848371504,1.,-0.108161120528369));
#64302=CARTESIAN_POINT('Ctrl Pts',(-4.13516614458895,1.,-0.105109286538945));
#64303=CARTESIAN_POINT('Ctrl Pts',(-4.14231804939538,1.,-0.102021826577584));
#64304=CARTESIAN_POINT('Ctrl Pts',(-4.14946408918485,1.,-0.0988990478901226));
#64305=CARTESIAN_POINT('Ctrl Pts',(-4.15660412653577,1.,-0.0957412403298007));
#64306=CARTESIAN_POINT('Ctrl Pts',(-4.16373802265839,1.,-0.0925486672167531));
#64307=CARTESIAN_POINT('Ctrl Pts',(-4.17086566490794,1.,-0.0893215560848649));
#64308=CARTESIAN_POINT('Ctrl Pts',(-4.17798698668094,1.,-0.0860600915549397));
#64309=CARTESIAN_POINT('Ctrl Pts',(-4.18510195327123,1.,-0.0827644164385679));
#64310=CARTESIAN_POINT('Ctrl Pts',(-4.19078883320504,1.,-0.080100588711432));
#64311=CARTESIAN_POINT('Ctrl Pts',(-4.19505112859416,1.,-0.0780873956242397));
#64312=CARTESIAN_POINT('Ctrl Pts',(-4.1978913862118,1.,-0.0767384596141464));
#64313=CARTESIAN_POINT('Ctrl Pts',(-4.19931119685982,1.,-0.0760622897878246));
#64314=CARTESIAN_POINT('Origin',(-4.19931119685982,0.,-0.0760622897878246));
#64315=CARTESIAN_POINT('',(-4.19931119685982,1.,0.0760622897878236));
#64316=CARTESIAN_POINT('Origin',(0.,0.,0.));
#64317=CARTESIAN_POINT('',(-3.73017266276651,1.,-0.385112848330761));
#64318=CARTESIAN_POINT('Origin',(0.,1.,0.));
#64319=CARTESIAN_POINT('Ctrl Pts',(-3.73017266276651,1.,-0.385112848330762));
#64320=CARTESIAN_POINT('Ctrl Pts',(-3.73017266276651,0.666666666666667,
-0.385112848330762));
#64321=CARTESIAN_POINT('Ctrl Pts',(-3.73017266276651,0.333333333333333,
-0.385112848330762));
#64322=CARTESIAN_POINT('Ctrl Pts',(-3.73017266276651,-0.333333333333333,
-0.385112848330762));
#64323=CARTESIAN_POINT('Ctrl Pts',(-3.73017266276651,-0.666666666666667,
-0.385112848330762));
#64324=CARTESIAN_POINT('Ctrl Pts',(-3.73017266276651,-1.,-0.385112848330762));
#64325=CARTESIAN_POINT('Ctrl Pts',(-4.15950947128175,-1.,-0.581791163835815));
#64326=CARTESIAN_POINT('Ctrl Pts',(-4.15950947128175,1.,-0.581791163835815));
#64327=CARTESIAN_POINT('Ctrl Pts',(-4.1582129171283,-1.,-0.580901211463535));
#64328=CARTESIAN_POINT('Ctrl Pts',(-4.1582129171283,1.,-0.580901211463535));
#64329=CARTESIAN_POINT('Ctrl Pts',(-4.15561864788576,-1.,-0.579124568914235));
#64330=CARTESIAN_POINT('Ctrl Pts',(-4.15561864788576,1.,-0.579124568914235));
#64331=CARTESIAN_POINT('Ctrl Pts',(-4.151723761217,-1.,-0.576469391676688));
#64332=CARTESIAN_POINT('Ctrl Pts',(-4.151723761217,1.,-0.576469391676688));
#64333=CARTESIAN_POINT('Ctrl Pts',(-4.14652361068081,-1.,-0.572948736069522));
#64334=CARTESIAN_POINT('Ctrl Pts',(-4.14652361068081,1.,-0.572948736069522));
#64335=CARTESIAN_POINT('Ctrl Pts',(-4.14001179830547,-1.,-0.568580610189774));
#64336=CARTESIAN_POINT('Ctrl Pts',(-4.14001179830547,1.,-0.568580610189774));
#64337=CARTESIAN_POINT('Ctrl Pts',(-4.13348835727104,-1.,-0.564245279537148));
#64338=CARTESIAN_POINT('Ctrl Pts',(-4.13348835727104,1.,-0.564245279537148));
#64339=CARTESIAN_POINT('Ctrl Pts',(-4.12695329951961,-1.,-0.559942890594773));
#64340=CARTESIAN_POINT('Ctrl Pts',(-4.12695329951961,1.,-0.559942890594773));
#64341=CARTESIAN_POINT('Ctrl Pts',(-4.12040666195664,-1.,-0.555673636129977));
#64342=CARTESIAN_POINT('Ctrl Pts',(-4.12040666195664,1.,-0.555673636129977));
#64343=CARTESIAN_POINT('Ctrl Pts',(-4.11384852024721,-1.,-0.551437758497032));
#64344=CARTESIAN_POINT('Ctrl Pts',(-4.11384852024721,1.,-0.551437758497032));
#64345=CARTESIAN_POINT('Ctrl Pts',(-4.10727897027977,-1.,-0.547235539485637));
#64346=CARTESIAN_POINT('Ctrl Pts',(-4.10727897027977,1.,-0.547235539485637));
#64347=CARTESIAN_POINT('Ctrl Pts',(-4.10069810243979,-1.,-0.543067286877757));
#64348=CARTESIAN_POINT('Ctrl Pts',(-4.10069810243979,1.,-0.543067286877757));
#64349=CARTESIAN_POINT('Ctrl Pts',(-4.09410597627,-1.,-0.538933321179756));
#64350=CARTESIAN_POINT('Ctrl Pts',(-4.09410597627,1.,-0.538933321179756));
#64351=CARTESIAN_POINT('Ctrl Pts',(-4.08750259988885,-1.,-0.534833963477273));
#64352=CARTESIAN_POINT('Ctrl Pts',(-4.08750259988885,1.,-0.534833963477273));
#64353=CARTESIAN_POINT('Ctrl Pts',(-4.08088789536836,-1.,-0.530769518728571));
#64354=CARTESIAN_POINT('Ctrl Pts',(-4.08088789536836,1.,-0.530769518728571));
#64355=CARTESIAN_POINT('Ctrl Pts',(-4.07426172299847,-1.,-0.526740277227498));
#64356=CARTESIAN_POINT('Ctrl Pts',(-4.07426172299847,1.,-0.526740277227498));
#64357=CARTESIAN_POINT('Ctrl Pts',(-4.06762394471314,-1.,-0.522746528603107));
#64358=CARTESIAN_POINT('Ctrl Pts',(-4.06762394471314,1.,-0.522746528603107));
#64359=CARTESIAN_POINT('Ctrl Pts',(-4.06097448038013,-1.,-0.518788572336923));
#64360=CARTESIAN_POINT('Ctrl Pts',(-4.06097448038013,1.,-0.518788572336923));
#64361=CARTESIAN_POINT('Ctrl Pts',(-4.05431335771199,-1.,-0.514866728193017));
#64362=CARTESIAN_POINT('Ctrl Pts',(-4.05431335771199,1.,-0.514866728193017));
#64363=CARTESIAN_POINT('Ctrl Pts',(-4.04764078815447,-1.,-0.51098134921897));
#64364=CARTESIAN_POINT('Ctrl Pts',(-4.04764078815447,1.,-0.51098134921897));
#64365=CARTESIAN_POINT('Ctrl Pts',(-4.04095715148915,-1.,-0.507132823288136));
#64366=CARTESIAN_POINT('Ctrl Pts',(-4.04095715148915,1.,-0.507132823288136));
#64367=CARTESIAN_POINT('Ctrl Pts',(-4.03426284174272,-1.,-0.503321556915346));
#64368=CARTESIAN_POINT('Ctrl Pts',(-4.03426284174272,1.,-0.503321556915346));
#64369=CARTESIAN_POINT('Ctrl Pts',(-4.02755813980101,-1.,-0.499547962340821));
#64370=CARTESIAN_POINT('Ctrl Pts',(-4.02755813980101,1.,-0.499547962340821));
#64371=CARTESIAN_POINT('Ctrl Pts',(-4.02084308851832,-1.,-0.495812444326251));
#64372=CARTESIAN_POINT('Ctrl Pts',(-4.02084308851832,1.,-0.495812444326251));
#64373=CARTESIAN_POINT('Ctrl Pts',(-4.01411733503546,-1.,-0.492115383418018));
#64374=CARTESIAN_POINT('Ctrl Pts',(-4.01411733503546,1.,-0.492115383418018));
#64375=CARTESIAN_POINT('Ctrl Pts',(-4.0073800839099,-1.,-0.488457130424633));
#64376=CARTESIAN_POINT('Ctrl Pts',(-4.0073800839099,1.,-0.488457130424633));
#64377=CARTESIAN_POINT('Ctrl Pts',(-4.00063045119288,-1.,-0.484838042421835));
#64378=CARTESIAN_POINT('Ctrl Pts',(-4.00063045119288,1.,-0.484838042421835));
#64379=CARTESIAN_POINT('Ctrl Pts',(-3.99386775880679,-1.,-0.481258512209675));
#64380=CARTESIAN_POINT('Ctrl Pts',(-3.99386775880679,1.,-0.481258512209675));
#64381=CARTESIAN_POINT('Ctrl Pts',(-3.98709184306738,-1.,-0.477718999122027));
#64382=CARTESIAN_POINT('Ctrl Pts',(-3.98709184306738,1.,-0.477718999122027));
#64383=CARTESIAN_POINT('Ctrl Pts',(-3.98030338044409,-1.,-0.47422006101951));
#64384=CARTESIAN_POINT('Ctrl Pts',(-3.98030338044409,1.,-0.47422006101951));
#64385=CARTESIAN_POINT('Ctrl Pts',(-3.97350414289392,-1.,-0.470762379613439));
#64386=CARTESIAN_POINT('Ctrl Pts',(-3.97350414289392,1.,-0.470762379613439));
#64387=CARTESIAN_POINT('Ctrl Pts',(-3.9666962227393,-1.,-0.467346690880643));
#64388=CARTESIAN_POINT('Ctrl Pts',(-3.9666962227393,1.,-0.467346690880643));
#64389=CARTESIAN_POINT('Ctrl Pts',(-3.95988133243538,-1.,-0.463973722115733));
#64390=CARTESIAN_POINT('Ctrl Pts',(-3.95988133243538,1.,-0.463973722115733));
#64391=CARTESIAN_POINT('Ctrl Pts',(-3.95306005817364,-1.,-0.460644124429121));
#64392=CARTESIAN_POINT('Ctrl Pts',(-3.95306005817364,1.,-0.460644124429121));
#64393=CARTESIAN_POINT('Ctrl Pts',(-3.94623117206678,-1.,-0.457358410451683));
#64394=CARTESIAN_POINT('Ctrl Pts',(-3.94623117206678,1.,-0.457358410451683));
#64395=CARTESIAN_POINT('Ctrl Pts',(-3.93939080846298,-1.,-0.454116879027584));
#64396=CARTESIAN_POINT('Ctrl Pts',(-3.93939080846298,1.,-0.454116879027584));
#64397=CARTESIAN_POINT('Ctrl Pts',(-3.93253407403123,-1.,-0.450919768356348));
#64398=CARTESIAN_POINT('Ctrl Pts',(-3.93253407403123,1.,-0.450919768356348));
#64399=CARTESIAN_POINT('Ctrl Pts',(-3.92565674143416,-1.,-0.447767416837292));
#64400=CARTESIAN_POINT('Ctrl Pts',(-3.92565674143416,1.,-0.447767416837292));
#64401=CARTESIAN_POINT('Ctrl Pts',(-3.91875701610719,-1.,-0.444660430230591));
#64402=CARTESIAN_POINT('Ctrl Pts',(-3.91875701610719,1.,-0.444660430230591));
#64403=CARTESIAN_POINT('Ctrl Pts',(-3.91183704069153,-1.,-0.441599824524054));
#64404=CARTESIAN_POINT('Ctrl Pts',(-3.91183704069153,1.,-0.441599824524054));
#64405=CARTESIAN_POINT('Ctrl Pts',(-3.90490512938563,-1.,-0.438587235458249));
#64406=CARTESIAN_POINT('Ctrl Pts',(-3.90490512938563,1.,-0.438587235458249));
#64407=CARTESIAN_POINT('Ctrl Pts',(-3.89797256655462,-1.,-0.435624629433527));
#64408=CARTESIAN_POINT('Ctrl Pts',(-3.89797256655462,1.,-0.435624629433527));
#64409=CARTESIAN_POINT('Ctrl Pts',(-3.89104947940611,-1.,-0.432713929544458));
#64410=CARTESIAN_POINT('Ctrl Pts',(-3.89104947940611,1.,-0.432713929544458));
#64411=CARTESIAN_POINT('Ctrl Pts',(-3.88414070943341,-1.,-0.429856640579741));
#64412=CARTESIAN_POINT('Ctrl Pts',(-3.88414070943341,1.,-0.429856640579741));
#64413=CARTESIAN_POINT('Ctrl Pts',(-3.87724240306597,-1.,-0.427053541173457));
#64414=CARTESIAN_POINT('Ctrl Pts',(-3.87724240306597,1.,-0.427053541173457));
#64415=CARTESIAN_POINT('Ctrl Pts',(-3.87033643487851,-1.,-0.424304173195111));
#64416=CARTESIAN_POINT('Ctrl Pts',(-3.87033643487851,1.,-0.424304173195111));
#64417=CARTESIAN_POINT('Ctrl Pts',(-3.86339652542709,-1.,-0.421607423177534));
#64418=CARTESIAN_POINT('Ctrl Pts',(-3.86339652542709,1.,-0.421607423177534));
#64419=CARTESIAN_POINT('Ctrl Pts',(-3.85639825647996,-1.,-0.418962468086773));
#64420=CARTESIAN_POINT('Ctrl Pts',(-3.85639825647996,1.,-0.418962468086773));
#64421=CARTESIAN_POINT('Ctrl Pts',(-3.84932864157497,-1.,-0.416369678052907));
#64422=CARTESIAN_POINT('Ctrl Pts',(-3.84932864157497,1.,-0.416369678052907));
#64423=CARTESIAN_POINT('Ctrl Pts',(-3.84219403994762,-1.,-0.413831367016748));
#64424=CARTESIAN_POINT('Ctrl Pts',(-3.84219403994762,1.,-0.413831367016748));
#64425=CARTESIAN_POINT('Ctrl Pts',(-3.83503345578698,-1.,-0.411353038798518));
#64426=CARTESIAN_POINT('Ctrl Pts',(-3.83503345578698,1.,-0.411353038798518));
#64427=CARTESIAN_POINT('Ctrl Pts',(-3.82790724256471,-1.,-0.40894237144746));
#64428=CARTESIAN_POINT('Ctrl Pts',(-3.82790724256471,1.,-0.40894237144746));
#64429=CARTESIAN_POINT('Ctrl Pts',(-3.8208730391381,-1.,-0.406607038258985));
#64430=CARTESIAN_POINT('Ctrl Pts',(-3.8208730391381,1.,-0.406607038258985));
#64431=CARTESIAN_POINT('Ctrl Pts',(-3.81396374287793,-1.,-0.404352694628273));
#64432=CARTESIAN_POINT('Ctrl Pts',(-3.81396374287793,1.,-0.404352694628273));
#64433=CARTESIAN_POINT('Ctrl Pts',(-3.80716881962728,-1.,-0.402181320148436));
#64434=CARTESIAN_POINT('Ctrl Pts',(-3.80716881962728,1.,-0.402181320148436));
#64435=CARTESIAN_POINT('Ctrl Pts',(-3.80040370384546,-1.,-0.4000883465046));
#64436=CARTESIAN_POINT('Ctrl Pts',(-3.80040370384546,1.,-0.4000883465046));
#64437=CARTESIAN_POINT('Ctrl Pts',(-3.7935288716329,-1.,-0.398064818683969));
#64438=CARTESIAN_POINT('Ctrl Pts',(-3.7935288716329,1.,-0.398064818683969));
#64439=CARTESIAN_POINT('Ctrl Pts',(-3.78640521279313,-1.,-0.396103205334841));
#64440=CARTESIAN_POINT('Ctrl Pts',(-3.78640521279313,1.,-0.396103205334841));
#64441=CARTESIAN_POINT('Ctrl Pts',(-3.77894173114283,-1.,-0.394202481011499));
#64442=CARTESIAN_POINT('Ctrl Pts',(-3.77894173114283,1.,-0.394202481011499));
#64443=CARTESIAN_POINT('Ctrl Pts',(-3.77114011595967,-1.,-0.392372786223432));
#64444=CARTESIAN_POINT('Ctrl Pts',(-3.77114011595967,1.,-0.392372786223432));
#64445=CARTESIAN_POINT('Ctrl Pts',(-3.76315635033257,-1.,-0.39064207297956));
#64446=CARTESIAN_POINT('Ctrl Pts',(-3.76315635033257,1.,-0.39064207297956));
#64447=CARTESIAN_POINT('Ctrl Pts',(-3.75529302895152,-1.,-0.389054775898702));
#64448=CARTESIAN_POINT('Ctrl Pts',(-3.75529302895152,1.,-0.389054775898702));
#64449=CARTESIAN_POINT('Ctrl Pts',(-3.74792651696654,-1.,-0.387663020050836));
#64450=CARTESIAN_POINT('Ctrl Pts',(-3.74792651696654,1.,-0.387663020050836));
#64451=CARTESIAN_POINT('Ctrl Pts',(-3.74144965781276,-1.,-0.386519576222251));
#64452=CARTESIAN_POINT('Ctrl Pts',(-3.74144965781276,1.,-0.386519576222251));
#64453=CARTESIAN_POINT('Ctrl Pts',(-3.73621371845318,-1.,-0.385670806454566));
#64454=CARTESIAN_POINT('Ctrl Pts',(-3.73621371845318,1.,-0.385670806454566));
#64455=CARTESIAN_POINT('Ctrl Pts',(-3.73245705638843,-1.,-0.385147887988951));
#64456=CARTESIAN_POINT('Ctrl Pts',(-3.73245705638843,1.,-0.385147887988951));
#64457=CARTESIAN_POINT('Ctrl Pts',(-3.73072465900175,-1.,-0.385001870183213));
#64458=CARTESIAN_POINT('Ctrl Pts',(-3.73072465900175,1.,-0.385001870183213));
#64459=CARTESIAN_POINT('Ctrl Pts',(-3.73015851028356,-1.,-0.385047711603462));
#64460=CARTESIAN_POINT('Ctrl Pts',(-3.73015851028356,1.,-0.385047711603462));
#64461=CARTESIAN_POINT('Ctrl Pts',(-3.73010668803042,-1.,-0.385147278814642));
#64462=CARTESIAN_POINT('Ctrl Pts',(-3.73010668803042,1.,-0.385147278814642));
#64463=CARTESIAN_POINT('Ctrl Pts',(-3.73016218570874,-1.,-0.38521431477633));
#64464=CARTESIAN_POINT('Ctrl Pts',(-3.73016218570874,1.,-0.38521431477633));
#64465=CARTESIAN_POINT('',(-4.15950947128175,1.,-0.581791163835815));
#64466=CARTESIAN_POINT('Ctrl Pts',(-4.15950947128175,1.,-0.581791163835815));
#64467=CARTESIAN_POINT('Ctrl Pts',(-4.1582129171283,1.,-0.580901211463535));
#64468=CARTESIAN_POINT('Ctrl Pts',(-4.15561864788576,1.,-0.579124568914235));
#64469=CARTESIAN_POINT('Ctrl Pts',(-4.151723761217,1.,-0.576469391676688));
#64470=CARTESIAN_POINT('Ctrl Pts',(-4.14652361068081,1.,-0.572948736069522));
#64471=CARTESIAN_POINT('Ctrl Pts',(-4.14001179830547,1.,-0.568580610189774));
#64472=CARTESIAN_POINT('Ctrl Pts',(-4.13348835727104,1.,-0.564245279537148));
#64473=CARTESIAN_POINT('Ctrl Pts',(-4.12695329951961,1.,-0.559942890594773));
#64474=CARTESIAN_POINT('Ctrl Pts',(-4.12040666195664,1.,-0.555673636129977));
#64475=CARTESIAN_POINT('Ctrl Pts',(-4.11384852024721,1.,-0.551437758497032));
#64476=CARTESIAN_POINT('Ctrl Pts',(-4.10727897027977,1.,-0.547235539485637));
#64477=CARTESIAN_POINT('Ctrl Pts',(-4.10069810243979,1.,-0.543067286877757));
#64478=CARTESIAN_POINT('Ctrl Pts',(-4.09410597627,1.,-0.538933321179756));
#64479=CARTESIAN_POINT('Ctrl Pts',(-4.08750259988885,1.,-0.534833963477273));
#64480=CARTESIAN_POINT('Ctrl Pts',(-4.08088789536836,1.,-0.530769518728571));
#64481=CARTESIAN_POINT('Ctrl Pts',(-4.07426172299847,1.,-0.526740277227498));
#64482=CARTESIAN_POINT('Ctrl Pts',(-4.06762394471314,1.,-0.522746528603107));
#64483=CARTESIAN_POINT('Ctrl Pts',(-4.06097448038013,1.,-0.518788572336923));
#64484=CARTESIAN_POINT('Ctrl Pts',(-4.05431335771199,1.,-0.514866728193017));
#64485=CARTESIAN_POINT('Ctrl Pts',(-4.04764078815447,1.,-0.51098134921897));
#64486=CARTESIAN_POINT('Ctrl Pts',(-4.04095715148915,1.,-0.507132823288136));
#64487=CARTESIAN_POINT('Ctrl Pts',(-4.03426284174272,1.,-0.503321556915346));
#64488=CARTESIAN_POINT('Ctrl Pts',(-4.02755813980101,1.,-0.499547962340821));
#64489=CARTESIAN_POINT('Ctrl Pts',(-4.02084308851832,1.,-0.495812444326251));
#64490=CARTESIAN_POINT('Ctrl Pts',(-4.01411733503546,1.,-0.492115383418018));
#64491=CARTESIAN_POINT('Ctrl Pts',(-4.0073800839099,1.,-0.488457130424633));
#64492=CARTESIAN_POINT('Ctrl Pts',(-4.00063045119288,1.,-0.484838042421835));
#64493=CARTESIAN_POINT('Ctrl Pts',(-3.99386775880679,1.,-0.481258512209675));
#64494=CARTESIAN_POINT('Ctrl Pts',(-3.98709184306738,1.,-0.477718999122027));
#64495=CARTESIAN_POINT('Ctrl Pts',(-3.98030338044409,1.,-0.47422006101951));
#64496=CARTESIAN_POINT('Ctrl Pts',(-3.97350414289392,1.,-0.470762379613439));
#64497=CARTESIAN_POINT('Ctrl Pts',(-3.9666962227393,1.,-0.467346690880643));
#64498=CARTESIAN_POINT('Ctrl Pts',(-3.95988133243538,1.,-0.463973722115733));
#64499=CARTESIAN_POINT('Ctrl Pts',(-3.95306005817364,1.,-0.460644124429121));
#64500=CARTESIAN_POINT('Ctrl Pts',(-3.94623117206678,1.,-0.457358410451683));
#64501=CARTESIAN_POINT('Ctrl Pts',(-3.93939080846298,1.,-0.454116879027584));
#64502=CARTESIAN_POINT('Ctrl Pts',(-3.93253407403123,1.,-0.450919768356348));
#64503=CARTESIAN_POINT('Ctrl Pts',(-3.92565674143416,1.,-0.447767416837292));
#64504=CARTESIAN_POINT('Ctrl Pts',(-3.91875701610719,1.,-0.444660430230591));
#64505=CARTESIAN_POINT('Ctrl Pts',(-3.91183704069153,1.,-0.441599824524054));
#64506=CARTESIAN_POINT('Ctrl Pts',(-3.90490512938563,1.,-0.438587235458249));
#64507=CARTESIAN_POINT('Ctrl Pts',(-3.89797256655462,1.,-0.435624629433527));
#64508=CARTESIAN_POINT('Ctrl Pts',(-3.89104947940611,1.,-0.432713929544458));
#64509=CARTESIAN_POINT('Ctrl Pts',(-3.88414070943341,1.,-0.429856640579741));
#64510=CARTESIAN_POINT('Ctrl Pts',(-3.87724240306597,1.,-0.427053541173457));
#64511=CARTESIAN_POINT('Ctrl Pts',(-3.87033643487851,1.,-0.424304173195111));
#64512=CARTESIAN_POINT('Ctrl Pts',(-3.86339652542709,1.,-0.421607423177534));
#64513=CARTESIAN_POINT('Ctrl Pts',(-3.85639825647996,1.,-0.418962468086773));
#64514=CARTESIAN_POINT('Ctrl Pts',(-3.84932864157497,1.,-0.416369678052907));
#64515=CARTESIAN_POINT('Ctrl Pts',(-3.84219403994762,1.,-0.413831367016748));
#64516=CARTESIAN_POINT('Ctrl Pts',(-3.83503345578698,1.,-0.411353038798518));
#64517=CARTESIAN_POINT('Ctrl Pts',(-3.82790724256471,1.,-0.40894237144746));
#64518=CARTESIAN_POINT('Ctrl Pts',(-3.8208730391381,1.,-0.406607038258985));
#64519=CARTESIAN_POINT('Ctrl Pts',(-3.81396374287793,1.,-0.404352694628273));
#64520=CARTESIAN_POINT('Ctrl Pts',(-3.80716881962728,1.,-0.402181320148436));
#64521=CARTESIAN_POINT('Ctrl Pts',(-3.80040370384546,1.,-0.4000883465046));
#64522=CARTESIAN_POINT('Ctrl Pts',(-3.7935288716329,1.,-0.398064818683969));
#64523=CARTESIAN_POINT('Ctrl Pts',(-3.78640521279313,1.,-0.396103205334841));
#64524=CARTESIAN_POINT('Ctrl Pts',(-3.77894173114283,1.,-0.394202481011499));
#64525=CARTESIAN_POINT('Ctrl Pts',(-3.77114011595967,1.,-0.392372786223432));
#64526=CARTESIAN_POINT('Ctrl Pts',(-3.76315635033257,1.,-0.39064207297956));
#64527=CARTESIAN_POINT('Ctrl Pts',(-3.75529302895152,1.,-0.389054775898702));
#64528=CARTESIAN_POINT('Ctrl Pts',(-3.74792651696654,1.,-0.387663020050836));
#64529=CARTESIAN_POINT('Ctrl Pts',(-3.74144965781276,1.,-0.386519576222251));
#64530=CARTESIAN_POINT('Ctrl Pts',(-3.73621371845318,1.,-0.385670806454566));
#64531=CARTESIAN_POINT('Ctrl Pts',(-3.73273893363406,1.,-0.385187124634206));
#64532=CARTESIAN_POINT('Ctrl Pts',(-3.73106082862548,1.,-0.385031656499164));
#64533=CARTESIAN_POINT('Ctrl Pts',(-3.73040527621055,1.,-0.385037797881504));
#64534=CARTESIAN_POINT('Ctrl Pts',(-3.73021431755274,1.,-0.385087139000374));
#64535=CARTESIAN_POINT('Ctrl Pts',(-3.73017266276651,1.,-0.385112848330762));
#64536=CARTESIAN_POINT('',(-4.15950947128175,0.,-0.581791163835815));
#64537=CARTESIAN_POINT('Ctrl Pts',(-3.66663282329846,-1.,-0.7863229229206));
#64538=CARTESIAN_POINT('Ctrl Pts',(-3.66663282329846,1.,-0.7863229229206));
#64539=CARTESIAN_POINT('Ctrl Pts',(-3.66655932661986,-1.,-0.786369528183326));
#64540=CARTESIAN_POINT('Ctrl Pts',(-3.66655932661986,1.,-0.786369528183326));
#64541=CARTESIAN_POINT('Ctrl Pts',(-3.66657784455334,-1.,-0.786480236185696));
#64542=CARTESIAN_POINT('Ctrl Pts',(-3.66657784455334,1.,-0.786480236185696));
#64543=CARTESIAN_POINT('Ctrl Pts',(-3.66710211820482,-1.,-0.786698783542764));
#64544=CARTESIAN_POINT('Ctrl Pts',(-3.66710211820482,1.,-0.786698783542764));
#64545=CARTESIAN_POINT('Ctrl Pts',(-3.66879484801113,-1.,-0.787095252590501));
#64546=CARTESIAN_POINT('Ctrl Pts',(-3.66879484801113,1.,-0.787095252590501));
#64547=CARTESIAN_POINT('Ctrl Pts',(-3.67252923663655,-1.,-0.787758799995742));
#64548=CARTESIAN_POINT('Ctrl Pts',(-3.67252923663655,1.,-0.787758799995742));
#64549=CARTESIAN_POINT('Ctrl Pts',(-3.67777119516252,-1.,-0.788569566220285));
#64550=CARTESIAN_POINT('Ctrl Pts',(-3.67777119516252,1.,-0.788569566220285));
#64551=CARTESIAN_POINT('Ctrl Pts',(-3.68428439783905,-1.,-0.789483546064387));
#64552=CARTESIAN_POINT('Ctrl Pts',(-3.68428439783905,1.,-0.789483546064387));
#64553=CARTESIAN_POINT('Ctrl Pts',(-3.69172044327364,-1.,-0.790436284988787));
#64554=CARTESIAN_POINT('Ctrl Pts',(-3.69172044327364,1.,-0.790436284988787));
#64555=CARTESIAN_POINT('Ctrl Pts',(-3.69968940808721,-1.,-0.79135657569598));
#64556=CARTESIAN_POINT('Ctrl Pts',(-3.69968940808721,1.,-0.79135657569598));
#64557=CARTESIAN_POINT('Ctrl Pts',(-3.70781724021806,-1.,-0.792177688845818));
#64558=CARTESIAN_POINT('Ctrl Pts',(-3.70781724021806,1.,-0.792177688845818));
#64559=CARTESIAN_POINT('Ctrl Pts',(-3.71580242396124,-1.,-0.792848377370287));
#64560=CARTESIAN_POINT('Ctrl Pts',(-3.71580242396124,1.,-0.792848377370287));
#64561=CARTESIAN_POINT('Ctrl Pts',(-3.72348797293734,-1.,-0.793347023784205));
#64562=CARTESIAN_POINT('Ctrl Pts',(-3.72348797293734,1.,-0.793347023784205));
#64563=CARTESIAN_POINT('Ctrl Pts',(-3.73086914695805,-1.,-0.793682750269684));
#64564=CARTESIAN_POINT('Ctrl Pts',(-3.73086914695805,1.,-0.793682750269684));
#64565=CARTESIAN_POINT('Ctrl Pts',(-3.73803280541687,-1.,-0.793882700937017));
#64566=CARTESIAN_POINT('Ctrl Pts',(-3.73803280541687,1.,-0.793882700937017));
#64567=CARTESIAN_POINT('Ctrl Pts',(-3.74511357728861,-1.,-0.793982700459952));
#64568=CARTESIAN_POINT('Ctrl Pts',(-3.74511357728861,1.,-0.793982700459952));
#64569=CARTESIAN_POINT('Ctrl Pts',(-3.75224692493864,-1.,-0.794017347371377));
#64570=CARTESIAN_POINT('Ctrl Pts',(-3.75224692493864,1.,-0.794017347371377));
#64571=CARTESIAN_POINT('Ctrl Pts',(-3.75951468666257,-1.,-0.794008429134907));
#64572=CARTESIAN_POINT('Ctrl Pts',(-3.75951468666257,1.,-0.794008429134907));
#64573=CARTESIAN_POINT('Ctrl Pts',(-3.76692626931111,-1.,-0.793961083688991));
#64574=CARTESIAN_POINT('Ctrl Pts',(-3.76692626931111,1.,-0.793961083688991));
#64575=CARTESIAN_POINT('Ctrl Pts',(-3.77444863801212,-1.,-0.793870523787408));
#64576=CARTESIAN_POINT('Ctrl Pts',(-3.77444863801212,1.,-0.793870523787408));
#64577=CARTESIAN_POINT('Ctrl Pts',(-3.78202460377598,-1.,-0.7937262357813));
#64578=CARTESIAN_POINT('Ctrl Pts',(-3.78202460377598,1.,-0.7937262357813));
#64579=CARTESIAN_POINT('Ctrl Pts',(-3.78959439439235,-1.,-0.793516871680993));
#64580=CARTESIAN_POINT('Ctrl Pts',(-3.78959439439235,1.,-0.793516871680993));
#64581=CARTESIAN_POINT('Ctrl Pts',(-3.79711921389897,-1.,-0.793235612973273));
#64582=CARTESIAN_POINT('Ctrl Pts',(-3.79711921389897,1.,-0.793235612973273));
#64583=CARTESIAN_POINT('Ctrl Pts',(-3.80459229925637,-1.,-0.792882695234778));
#64584=CARTESIAN_POINT('Ctrl Pts',(-3.80459229925637,1.,-0.792882695234778));
#64585=CARTESIAN_POINT('Ctrl Pts',(-3.81202588694756,-1.,-0.792462483517634));
#64586=CARTESIAN_POINT('Ctrl Pts',(-3.81202588694756,1.,-0.792462483517634));
#64587=CARTESIAN_POINT('Ctrl Pts',(-3.81944345442249,-1.,-0.791981740718635));
#64588=CARTESIAN_POINT('Ctrl Pts',(-3.81944345442249,1.,-0.791981740718635));
#64589=CARTESIAN_POINT('Ctrl Pts',(-3.82687033899792,-1.,-0.791447528662369));
#64590=CARTESIAN_POINT('Ctrl Pts',(-3.82687033899792,1.,-0.791447528662369));
#64591=CARTESIAN_POINT('Ctrl Pts',(-3.83432392054786,-1.,-0.790865012705301));
#64592=CARTESIAN_POINT('Ctrl Pts',(-3.83432392054786,1.,-0.790865012705301));
#64593=CARTESIAN_POINT('Ctrl Pts',(-3.84180762342454,-1.,-0.790236124191242));
#64594=CARTESIAN_POINT('Ctrl Pts',(-3.84180762342454,1.,-0.790236124191242));
#64595=CARTESIAN_POINT('Ctrl Pts',(-3.84931637808894,-1.,-0.789560798155582));
#64596=CARTESIAN_POINT('Ctrl Pts',(-3.84931637808894,1.,-0.789560798155582));
#64597=CARTESIAN_POINT('Ctrl Pts',(-3.85683995872529,-1.,-0.788837734090672));
#64598=CARTESIAN_POINT('Ctrl Pts',(-3.85683995872529,1.,-0.788837734090672));
#64599=CARTESIAN_POINT('Ctrl Pts',(-3.86436702561345,-1.,-0.788065315093777));
#64600=CARTESIAN_POINT('Ctrl Pts',(-3.86436702561345,1.,-0.788065315093777));
#64601=CARTESIAN_POINT('Ctrl Pts',(-3.87188916600912,-1.,-0.787242527617999));
#64602=CARTESIAN_POINT('Ctrl Pts',(-3.87188916600912,1.,-0.787242527617999));
#64603=CARTESIAN_POINT('Ctrl Pts',(-3.8794040281819,-1.,-0.786369675812608));
#64604=CARTESIAN_POINT('Ctrl Pts',(-3.8794040281819,1.,-0.786369675812608));
#64605=CARTESIAN_POINT('Ctrl Pts',(-3.88691313167398,-1.,-0.78544789034073));
#64606=CARTESIAN_POINT('Ctrl Pts',(-3.88691313167398,1.,-0.78544789034073));
#64607=CARTESIAN_POINT('Ctrl Pts',(-3.89442039235103,-1.,-0.784478799358336));
#64608=CARTESIAN_POINT('Ctrl Pts',(-3.89442039235103,1.,-0.784478799358336));
#64609=CARTESIAN_POINT('Ctrl Pts',(-3.9019303904397,-1.,-0.783464141529081));
#64610=CARTESIAN_POINT('Ctrl Pts',(-3.9019303904397,1.,-0.783464141529081));
#64611=CARTESIAN_POINT('Ctrl Pts',(-3.90944671004542,-1.,-0.782405395622764));
#64612=CARTESIAN_POINT('Ctrl Pts',(-3.90944671004542,1.,-0.782405395622764));
#64613=CARTESIAN_POINT('Ctrl Pts',(-3.91697036054676,-1.,-0.781303428618366));
#64614=CARTESIAN_POINT('Ctrl Pts',(-3.91697036054676,1.,-0.781303428618366));
#64615=CARTESIAN_POINT('Ctrl Pts',(-3.92450058323823,-1.,-0.780158678615542));
#64616=CARTESIAN_POINT('Ctrl Pts',(-3.92450058323823,1.,-0.780158678615542));
#64617=CARTESIAN_POINT('Ctrl Pts',(-3.93203552473174,-1.,-0.778971308134821));
#64618=CARTESIAN_POINT('Ctrl Pts',(-3.93203552473174,1.,-0.778971308134821));
#64619=CARTESIAN_POINT('Ctrl Pts',(-3.93957296768103,-1.,-0.777741370568558));
#64620=CARTESIAN_POINT('Ctrl Pts',(-3.93957296768103,1.,-0.777741370568558));
#64621=CARTESIAN_POINT('Ctrl Pts',(-3.94711101619447,-1.,-0.776468966697921));
#64622=CARTESIAN_POINT('Ctrl Pts',(-3.94711101619447,1.,-0.776468966697921));
#64623=CARTESIAN_POINT('Ctrl Pts',(-3.9546488545231,-1.,-0.775154418039351));
#64624=CARTESIAN_POINT('Ctrl Pts',(-3.9546488545231,1.,-0.775154418039351));
#64625=CARTESIAN_POINT('Ctrl Pts',(-3.96218649639807,-1.,-0.773798212026565));
#64626=CARTESIAN_POINT('Ctrl Pts',(-3.96218649639807,1.,-0.773798212026565));
#64627=CARTESIAN_POINT('Ctrl Pts',(-3.96972446532772,-1.,-0.772400931772136));
#64628=CARTESIAN_POINT('Ctrl Pts',(-3.96972446532772,1.,-0.772400931772136));
#64629=CARTESIAN_POINT('Ctrl Pts',(-3.97726349165488,-1.,-0.770963190030471));
#64630=CARTESIAN_POINT('Ctrl Pts',(-3.97726349165488,1.,-0.770963190030471));
#64631=CARTESIAN_POINT('Ctrl Pts',(-3.98480422348451,-1.,-0.769485566245544));
#64632=CARTESIAN_POINT('Ctrl Pts',(-3.98480422348451,1.,-0.769485566245544));
#64633=CARTESIAN_POINT('Ctrl Pts',(-3.9923468788101,-1.,-0.767968531377915));
#64634=CARTESIAN_POINT('Ctrl Pts',(-3.9923468788101,1.,-0.767968531377915));
#64635=CARTESIAN_POINT('Ctrl Pts',(-3.99989129179622,-1.,-0.766412457136064));
#64636=CARTESIAN_POINT('Ctrl Pts',(-3.99989129179622,1.,-0.766412457136064));
#64637=CARTESIAN_POINT('Ctrl Pts',(-4.00743706791509,-1.,-0.764817648785197));
#64638=CARTESIAN_POINT('Ctrl Pts',(-4.00743706791509,1.,-0.764817648785197));
#64639=CARTESIAN_POINT('Ctrl Pts',(-4.01498370680496,-1.,-0.763184371182935));
#64640=CARTESIAN_POINT('Ctrl Pts',(-4.01498370680496,1.,-0.763184371182935));
#64641=CARTESIAN_POINT('Ctrl Pts',(-4.02253072741268,-1.,-0.761512875859804));
#64642=CARTESIAN_POINT('Ctrl Pts',(-4.02253072741268,1.,-0.761512875859804));
#64643=CARTESIAN_POINT('Ctrl Pts',(-4.03007781954412,-1.,-0.759803433243752));
#64644=CARTESIAN_POINT('Ctrl Pts',(-4.03007781954412,1.,-0.759803433243752));
#64645=CARTESIAN_POINT('Ctrl Pts',(-4.03762485803119,-1.,-0.758056338884944));
#64646=CARTESIAN_POINT('Ctrl Pts',(-4.03762485803119,1.,-0.758056338884944));
#64647=CARTESIAN_POINT('Ctrl Pts',(-4.04517182653997,-1.,-0.756271902369581));
#64648=CARTESIAN_POINT('Ctrl Pts',(-4.04517182653997,1.,-0.756271902369581));
#64649=CARTESIAN_POINT('Ctrl Pts',(-4.05271876687915,-1.,-0.754450441816078));
#64650=CARTESIAN_POINT('Ctrl Pts',(-4.05271876687915,1.,-0.754450441816078));
#64651=CARTESIAN_POINT('Ctrl Pts',(-4.06026572221515,-1.,-0.752592276483072));
#64652=CARTESIAN_POINT('Ctrl Pts',(-4.06026572221515,1.,-0.752592276483072));
#64653=CARTESIAN_POINT('Ctrl Pts',(-4.06781267242378,-1.,-0.750697720484036));
#64654=CARTESIAN_POINT('Ctrl Pts',(-4.06781267242378,1.,-0.750697720484036));
#64655=CARTESIAN_POINT('Ctrl Pts',(-4.07535951056152,-1.,-0.748767076680557));
#64656=CARTESIAN_POINT('Ctrl Pts',(-4.07535951056152,1.,-0.748767076680557));
#64657=CARTESIAN_POINT('Ctrl Pts',(-4.08290608095642,-1.,-0.746800631492315));
#64658=CARTESIAN_POINT('Ctrl Pts',(-4.08290608095642,1.,-0.746800631492315));
#64659=CARTESIAN_POINT('Ctrl Pts',(-4.09045220253573,-1.,-0.7447986497065));
#64660=CARTESIAN_POINT('Ctrl Pts',(-4.09045220253573,1.,-0.7447986497065));
#64661=CARTESIAN_POINT('Ctrl Pts',(-4.09799769702611,-1.,-0.742761369689841));
#64662=CARTESIAN_POINT('Ctrl Pts',(-4.09799769702611,1.,-0.742761369689841));
#64663=CARTESIAN_POINT('Ctrl Pts',(-4.10554241757547,-1.,-0.740688998553377));
#64664=CARTESIAN_POINT('Ctrl Pts',(-4.10554241757547,1.,-0.740688998553377));
#64665=CARTESIAN_POINT('Ctrl Pts',(-4.11308626951927,-1.,-0.738581708225844));
#64666=CARTESIAN_POINT('Ctrl Pts',(-4.11308626951927,1.,-0.738581708225844));
#64667=CARTESIAN_POINT('Ctrl Pts',(-4.120629196238,-1.,-0.736439634331345));
#64668=CARTESIAN_POINT('Ctrl Pts',(-4.120629196238,1.,-0.736439634331345));
#64669=CARTESIAN_POINT('Ctrl Pts',(-4.12666277570844,-1.,-0.734698226764092));
#64670=CARTESIAN_POINT('Ctrl Pts',(-4.12666277570844,1.,-0.734698226764092));
#64671=CARTESIAN_POINT('Ctrl Pts',(-4.13118752795207,-1.,-0.733376589323546));
#64672=CARTESIAN_POINT('Ctrl Pts',(-4.13118752795207,1.,-0.733376589323546));
#64673=CARTESIAN_POINT('Ctrl Pts',(-4.1342038373684,-1.,-0.732488575135159));
#64674=CARTESIAN_POINT('Ctrl Pts',(-4.1342038373684,1.,-0.732488575135159));
#64675=CARTESIAN_POINT('Ctrl Pts',(-4.13571194405636,-1.,-0.73204283740062));
#64676=CARTESIAN_POINT('Ctrl Pts',(-4.13571194405636,1.,-0.73204283740062));
#64677=CARTESIAN_POINT('',(-3.66661143271685,1.,-0.786422660831985));
#64678=CARTESIAN_POINT('Ctrl Pts',(-3.66661143271685,-1.,-0.786422660831985));
#64679=CARTESIAN_POINT('Ctrl Pts',(-3.66661143271685,-0.666666666666667,
-0.786422660831985));
#64680=CARTESIAN_POINT('Ctrl Pts',(-3.66661143271685,-0.333333333333333,
-0.786422660831985));
#64681=CARTESIAN_POINT('Ctrl Pts',(-3.66661143271685,0.333333333333333,
-0.786422660831985));
#64682=CARTESIAN_POINT('Ctrl Pts',(-3.66661143271685,0.666666666666667,
-0.786422660831985));
#64683=CARTESIAN_POINT('Ctrl Pts',(-3.66661143271685,1.,-0.786422660831985));
#64684=CARTESIAN_POINT('',(-4.13571194405636,1.,-0.73204283740062));
#64685=CARTESIAN_POINT('',(-4.13571194405636,0.,-0.73204283740062));
#64686=CARTESIAN_POINT('Ctrl Pts',(-3.66661143271685,1.,-0.786422660831985));
#64687=CARTESIAN_POINT('Ctrl Pts',(-3.6666431041522,1.,-0.786459983895432));
#64688=CARTESIAN_POINT('Ctrl Pts',(-3.66680946938292,1.,-0.786565919558984));
#64689=CARTESIAN_POINT('Ctrl Pts',(-3.66743103898702,1.,-0.786774337198062));
#64690=CARTESIAN_POINT('Ctrl Pts',(-3.66907505398677,1.,-0.787145041181545));
#64691=CARTESIAN_POINT('Ctrl Pts',(-3.67252923663655,1.,-0.787758799995742));
#64692=CARTESIAN_POINT('Ctrl Pts',(-3.67777119516252,1.,-0.788569566220285));
#64693=CARTESIAN_POINT('Ctrl Pts',(-3.68428439783905,1.,-0.789483546064387));
#64694=CARTESIAN_POINT('Ctrl Pts',(-3.69172044327364,1.,-0.790436284988787));
#64695=CARTESIAN_POINT('Ctrl Pts',(-3.69968940808721,1.,-0.79135657569598));
#64696=CARTESIAN_POINT('Ctrl Pts',(-3.70781724021806,1.,-0.792177688845818));
#64697=CARTESIAN_POINT('Ctrl Pts',(-3.71580242396124,1.,-0.792848377370287));
#64698=CARTESIAN_POINT('Ctrl Pts',(-3.72348797293734,1.,-0.793347023784205));
#64699=CARTESIAN_POINT('Ctrl Pts',(-3.73086914695805,1.,-0.793682750269684));
#64700=CARTESIAN_POINT('Ctrl Pts',(-3.73803280541687,1.,-0.793882700937017));
#64701=CARTESIAN_POINT('Ctrl Pts',(-3.74511357728861,1.,-0.793982700459952));
#64702=CARTESIAN_POINT('Ctrl Pts',(-3.75224692493864,1.,-0.794017347371377));
#64703=CARTESIAN_POINT('Ctrl Pts',(-3.75951468666257,1.,-0.794008429134907));
#64704=CARTESIAN_POINT('Ctrl Pts',(-3.76692626931111,1.,-0.793961083688991));
#64705=CARTESIAN_POINT('Ctrl Pts',(-3.77444863801212,1.,-0.793870523787408));
#64706=CARTESIAN_POINT('Ctrl Pts',(-3.78202460377598,1.,-0.7937262357813));
#64707=CARTESIAN_POINT('Ctrl Pts',(-3.78959439439235,1.,-0.793516871680993));
#64708=CARTESIAN_POINT('Ctrl Pts',(-3.79711921389897,1.,-0.793235612973273));
#64709=CARTESIAN_POINT('Ctrl Pts',(-3.80459229925637,1.,-0.792882695234778));
#64710=CARTESIAN_POINT('Ctrl Pts',(-3.81202588694756,1.,-0.792462483517634));
#64711=CARTESIAN_POINT('Ctrl Pts',(-3.81944345442249,1.,-0.791981740718635));
#64712=CARTESIAN_POINT('Ctrl Pts',(-3.82687033899792,1.,-0.791447528662369));
#64713=CARTESIAN_POINT('Ctrl Pts',(-3.83432392054786,1.,-0.790865012705301));
#64714=CARTESIAN_POINT('Ctrl Pts',(-3.84180762342454,1.,-0.790236124191242));
#64715=CARTESIAN_POINT('Ctrl Pts',(-3.84931637808894,1.,-0.789560798155582));
#64716=CARTESIAN_POINT('Ctrl Pts',(-3.85683995872529,1.,-0.788837734090672));
#64717=CARTESIAN_POINT('Ctrl Pts',(-3.86436702561345,1.,-0.788065315093777));
#64718=CARTESIAN_POINT('Ctrl Pts',(-3.87188916600912,1.,-0.787242527617999));
#64719=CARTESIAN_POINT('Ctrl Pts',(-3.8794040281819,1.,-0.786369675812608));
#64720=CARTESIAN_POINT('Ctrl Pts',(-3.88691313167398,1.,-0.78544789034073));
#64721=CARTESIAN_POINT('Ctrl Pts',(-3.89442039235103,1.,-0.784478799358336));
#64722=CARTESIAN_POINT('Ctrl Pts',(-3.9019303904397,1.,-0.783464141529081));
#64723=CARTESIAN_POINT('Ctrl Pts',(-3.90944671004542,1.,-0.782405395622764));
#64724=CARTESIAN_POINT('Ctrl Pts',(-3.91697036054676,1.,-0.781303428618366));
#64725=CARTESIAN_POINT('Ctrl Pts',(-3.92450058323823,1.,-0.780158678615542));
#64726=CARTESIAN_POINT('Ctrl Pts',(-3.93203552473174,1.,-0.778971308134821));
#64727=CARTESIAN_POINT('Ctrl Pts',(-3.93957296768103,1.,-0.777741370568558));
#64728=CARTESIAN_POINT('Ctrl Pts',(-3.94711101619447,1.,-0.776468966697921));
#64729=CARTESIAN_POINT('Ctrl Pts',(-3.9546488545231,1.,-0.775154418039351));
#64730=CARTESIAN_POINT('Ctrl Pts',(-3.96218649639807,1.,-0.773798212026565));
#64731=CARTESIAN_POINT('Ctrl Pts',(-3.96972446532772,1.,-0.772400931772136));
#64732=CARTESIAN_POINT('Ctrl Pts',(-3.97726349165488,1.,-0.770963190030471));
#64733=CARTESIAN_POINT('Ctrl Pts',(-3.98480422348451,1.,-0.769485566245544));
#64734=CARTESIAN_POINT('Ctrl Pts',(-3.9923468788101,1.,-0.767968531377915));
#64735=CARTESIAN_POINT('Ctrl Pts',(-3.99989129179622,1.,-0.766412457136064));
#64736=CARTESIAN_POINT('Ctrl Pts',(-4.00743706791509,1.,-0.764817648785197));
#64737=CARTESIAN_POINT('Ctrl Pts',(-4.01498370680496,1.,-0.763184371182935));
#64738=CARTESIAN_POINT('Ctrl Pts',(-4.02253072741268,1.,-0.761512875859804));
#64739=CARTESIAN_POINT('Ctrl Pts',(-4.03007781954412,1.,-0.759803433243752));
#64740=CARTESIAN_POINT('Ctrl Pts',(-4.03762485803119,1.,-0.758056338884944));
#64741=CARTESIAN_POINT('Ctrl Pts',(-4.04517182653997,1.,-0.756271902369581));
#64742=CARTESIAN_POINT('Ctrl Pts',(-4.05271876687915,1.,-0.754450441816078));
#64743=CARTESIAN_POINT('Ctrl Pts',(-4.06026572221515,1.,-0.752592276483072));
#64744=CARTESIAN_POINT('Ctrl Pts',(-4.06781267242378,1.,-0.750697720484036));
#64745=CARTESIAN_POINT('Ctrl Pts',(-4.07535951056152,1.,-0.748767076680557));
#64746=CARTESIAN_POINT('Ctrl Pts',(-4.08290608095642,1.,-0.746800631492315));
#64747=CARTESIAN_POINT('Ctrl Pts',(-4.09045220253573,1.,-0.7447986497065));
#64748=CARTESIAN_POINT('Ctrl Pts',(-4.09799769702611,1.,-0.742761369689841));
#64749=CARTESIAN_POINT('Ctrl Pts',(-4.10554241757547,1.,-0.740688998553377));
#64750=CARTESIAN_POINT('Ctrl Pts',(-4.11308626951927,1.,-0.738581708225844));
#64751=CARTESIAN_POINT('Ctrl Pts',(-4.120629196238,1.,-0.736439634331345));
#64752=CARTESIAN_POINT('Ctrl Pts',(-4.12666277570844,1.,-0.734698226764092));
#64753=CARTESIAN_POINT('Ctrl Pts',(-4.13118752795207,1.,-0.733376589323546));
#64754=CARTESIAN_POINT('Ctrl Pts',(-4.1342038373684,1.,-0.732488575135159));
#64755=CARTESIAN_POINT('Ctrl Pts',(-4.13571194405636,1.,-0.73204283740062));
#64756=CARTESIAN_POINT('Origin',(-4.13571194405636,0.,-0.73204283740062));
#64757=CARTESIAN_POINT('',(-4.15950947128175,1.,-0.581791163835815));
#64758=CARTESIAN_POINT('Origin',(0.,0.,0.));
#64759=CARTESIAN_POINT('',(-3.62400312501245,1.,-0.963899035117248));
#64760=CARTESIAN_POINT('Origin',(0.,1.,0.));
#64761=CARTESIAN_POINT('Ctrl Pts',(-3.62400312501245,1.,-0.963899035117249));
#64762=CARTESIAN_POINT('Ctrl Pts',(-3.62400312501245,0.666666666666667,
-0.963899035117249));
#64763=CARTESIAN_POINT('Ctrl Pts',(-3.62400312501245,0.333333333333333,
-0.963899035117249));
#64764=CARTESIAN_POINT('Ctrl Pts',(-3.62400312501245,-0.333333333333333,
-0.963899035117249));
#64765=CARTESIAN_POINT('Ctrl Pts',(-3.62400312501246,-0.666666666666667,
-0.963899035117249));
#64766=CARTESIAN_POINT('Ctrl Pts',(-3.62400312501246,-1.,-0.963899035117249));
#64767=CARTESIAN_POINT('Ctrl Pts',(-4.01728681790024,-1.,-1.22531898815164));
#64768=CARTESIAN_POINT('Ctrl Pts',(-4.01728681790024,1.,-1.22531898815164));
#64769=CARTESIAN_POINT('Ctrl Pts',(-4.0161454457032,-1.,-1.22423716681447));
#64770=CARTESIAN_POINT('Ctrl Pts',(-4.0161454457032,1.,-1.22423716681447));
#64771=CARTESIAN_POINT('Ctrl Pts',(-4.01386104434674,-1.,-1.22207656456199));
#64772=CARTESIAN_POINT('Ctrl Pts',(-4.01386104434674,1.,-1.22207656456199));
#64773=CARTESIAN_POINT('Ctrl Pts',(-4.01042947142681,-1.,-1.21884478244983));
#64774=CARTESIAN_POINT('Ctrl Pts',(-4.01042947142681,1.,-1.21884478244983));
#64775=CARTESIAN_POINT('Ctrl Pts',(-4.00584409524937,-1.,-1.21455398918813));
#64776=CARTESIAN_POINT('Ctrl Pts',(-4.00584409524937,1.,-1.21455398918813));
#64777=CARTESIAN_POINT('Ctrl Pts',(-4.00009577952534,-1.,-1.20922097030107));
#64778=CARTESIAN_POINT('Ctrl Pts',(-4.00009577952534,1.,-1.20922097030107));
#64779=CARTESIAN_POINT('Ctrl Pts',(-3.99433084800649,-1.,-1.2039185237544));
#64780=CARTESIAN_POINT('Ctrl Pts',(-3.99433084800649,1.,-1.2039185237544));
#64781=CARTESIAN_POINT('Ctrl Pts',(-3.98854928957287,-1.,-1.19864679609596));
#64782=CARTESIAN_POINT('Ctrl Pts',(-3.98854928957287,1.,-1.19864679609596));
#64783=CARTESIAN_POINT('Ctrl Pts',(-3.98275111052015,-1.,-1.19340598349307));
#64784=CARTESIAN_POINT('Ctrl Pts',(-3.98275111052015,1.,-1.19340598349307));
#64785=CARTESIAN_POINT('Ctrl Pts',(-3.97693634766926,-1.,-1.18819633715285));
#64786=CARTESIAN_POINT('Ctrl Pts',(-3.97693634766926,1.,-1.18819633715285));
#64787=CARTESIAN_POINT('Ctrl Pts',(-3.9711050516465,-1.,-1.18301815039596));
#64788=CARTESIAN_POINT('Ctrl Pts',(-3.9711050516465,1.,-1.18301815039596));
#64789=CARTESIAN_POINT('Ctrl Pts',(-3.96525726357682,-1.,-1.17787174135445));
#64790=CARTESIAN_POINT('Ctrl Pts',(-3.96525726357682,1.,-1.17787174135445));
#64791=CARTESIAN_POINT('Ctrl Pts',(-3.95939299213164,-1.,-1.17275743590327));
#64792=CARTESIAN_POINT('Ctrl Pts',(-3.95939299213164,1.,-1.17275743590327));
#64793=CARTESIAN_POINT('Ctrl Pts',(-3.95351219510062,-1.,-1.16767555244495));
#64794=CARTESIAN_POINT('Ctrl Pts',(-3.95351219510062,1.,-1.16767555244495));
#64795=CARTESIAN_POINT('Ctrl Pts',(-3.9476147478092,-1.,-1.16262637999261));
#64796=CARTESIAN_POINT('Ctrl Pts',(-3.9476147478092,1.,-1.16262637999261));
#64797=CARTESIAN_POINT('Ctrl Pts',(-3.94170046685542,-1.,-1.1576101834106));
#64798=CARTESIAN_POINT('Ctrl Pts',(-3.94170046685542,1.,-1.1576101834106));
#64799=CARTESIAN_POINT('Ctrl Pts',(-3.9357691705651,-1.,-1.1526272271639));
#64800=CARTESIAN_POINT('Ctrl Pts',(-3.9357691705651,1.,-1.1526272271639));
#64801=CARTESIAN_POINT('Ctrl Pts',(-3.92982073294334,-1.,-1.14767779451147));
#64802=CARTESIAN_POINT('Ctrl Pts',(-3.92982073294334,1.,-1.14767779451147));
#64803=CARTESIAN_POINT('Ctrl Pts',(-3.92385513133937,-1.,-1.14276220561575));
#64804=CARTESIAN_POINT('Ctrl Pts',(-3.92385513133937,1.,-1.14276220561575));
#64805=CARTESIAN_POINT('Ctrl Pts',(-3.91787251936688,-1.,-1.13788084225511));
#64806=CARTESIAN_POINT('Ctrl Pts',(-3.91787251936688,1.,-1.13788084225511));
#64807=CARTESIAN_POINT('Ctrl Pts',(-3.91187321145495,-1.,-1.13303414693849));
#64808=CARTESIAN_POINT('Ctrl Pts',(-3.91187321145495,1.,-1.13303414693849));
#64809=CARTESIAN_POINT('Ctrl Pts',(-3.90585753318622,-1.,-1.12822258281518));
#64810=CARTESIAN_POINT('Ctrl Pts',(-3.90585753318622,1.,-1.12822258281518));
#64811=CARTESIAN_POINT('Ctrl Pts',(-3.89982569749978,-1.,-1.12344660099029));
#64812=CARTESIAN_POINT('Ctrl Pts',(-3.89982569749978,1.,-1.12344660099029));
#64813=CARTESIAN_POINT('Ctrl Pts',(-3.89377768340362,-1.,-1.11870660794609));
#64814=CARTESIAN_POINT('Ctrl Pts',(-3.89377768340362,1.,-1.11870660794609));
#64815=CARTESIAN_POINT('Ctrl Pts',(-3.88771308285229,-1.,-1.11400292434447));
#64816=CARTESIAN_POINT('Ctrl Pts',(-3.88771308285229,1.,-1.11400292434447));
#64817=CARTESIAN_POINT('Ctrl Pts',(-3.88163105531791,-1.,-1.10933577224029));
#64818=CARTESIAN_POINT('Ctrl Pts',(-3.88163105531791,1.,-1.10933577224029));
#64819=CARTESIAN_POINT('Ctrl Pts',(-3.87553067187566,-1.,-1.10470536603303));
#64820=CARTESIAN_POINT('Ctrl Pts',(-3.87553067187566,1.,-1.10470536603303));
#64821=CARTESIAN_POINT('Ctrl Pts',(-3.86941120134872,-1.,-1.10011198761202));
#64822=CARTESIAN_POINT('Ctrl Pts',(-3.86941120134872,1.,-1.10011198761202));
#64823=CARTESIAN_POINT('Ctrl Pts',(-3.86327241021242,-1.,-1.09555606505012));
#64824=CARTESIAN_POINT('Ctrl Pts',(-3.86327241021242,1.,-1.09555606505012));
#64825=CARTESIAN_POINT('Ctrl Pts',(-3.85711487933911,-1.,-1.09103825516288));
#64826=CARTESIAN_POINT('Ctrl Pts',(-3.85711487933911,1.,-1.09103825516288));
#64827=CARTESIAN_POINT('Ctrl Pts',(-3.8509402522269,-1.,-1.08655950846377));
#64828=CARTESIAN_POINT('Ctrl Pts',(-3.8509402522269,1.,-1.08655950846377));
#64829=CARTESIAN_POINT('Ctrl Pts',(-3.84475048030615,-1.,-1.08212087917986));
#64830=CARTESIAN_POINT('Ctrl Pts',(-3.84475048030615,1.,-1.08212087917986));
#64831=CARTESIAN_POINT('Ctrl Pts',(-3.83854714117486,-1.,-1.07772335353856));
#64832=CARTESIAN_POINT('Ctrl Pts',(-3.83854714117486,1.,-1.07772335353856));
#64833=CARTESIAN_POINT('Ctrl Pts',(-3.83233071195145,-1.,-1.0733676663346));
#64834=CARTESIAN_POINT('Ctrl Pts',(-3.83233071195145,1.,-1.0733676663346));
#64835=CARTESIAN_POINT('Ctrl Pts',(-3.82609989967278,-1.,-1.0690541318036));
#64836=CARTESIAN_POINT('Ctrl Pts',(-3.82609989967278,1.,-1.0690541318036));
#64837=CARTESIAN_POINT('Ctrl Pts',(-3.81985083953012,-1.,-1.06478244038931));
#64838=CARTESIAN_POINT('Ctrl Pts',(-3.81985083953012,1.,-1.06478244038931));
#64839=CARTESIAN_POINT('Ctrl Pts',(-3.81357866117485,-1.,-1.06055206187298));
#64840=CARTESIAN_POINT('Ctrl Pts',(-3.81357866117485,1.,-1.06055206187298));
#64841=CARTESIAN_POINT('Ctrl Pts',(-3.80727913637784,-1.,-1.05636266918643));
#64842=CARTESIAN_POINT('Ctrl Pts',(-3.80727913637784,1.,-1.05636266918643));
#64843=CARTESIAN_POINT('Ctrl Pts',(-3.80095039790678,-1.,-1.05221457990015));
#64844=CARTESIAN_POINT('Ctrl Pts',(-3.80095039790678,1.,-1.05221457990015));
#64845=CARTESIAN_POINT('Ctrl Pts',(-3.79459440308793,-1.,-1.04810913267641));
#64846=CARTESIAN_POINT('Ctrl Pts',(-3.79459440308793,1.,-1.04810913267641));
#64847=CARTESIAN_POINT('Ctrl Pts',(-3.78821910787195,-1.,-1.04404924374426));
#64848=CARTESIAN_POINT('Ctrl Pts',(-3.78821910787195,1.,-1.04404924374426));
#64849=CARTESIAN_POINT('Ctrl Pts',(-3.78183535008192,-1.,-1.04003862055804));
#64850=CARTESIAN_POINT('Ctrl Pts',(-3.78183535008192,1.,-1.04003862055804));
#64851=CARTESIAN_POINT('Ctrl Pts',(-3.77545283140445,-1.,-1.03608074678013));
#64852=CARTESIAN_POINT('Ctrl Pts',(-3.77545283140445,1.,-1.03608074678013));
#64853=CARTESIAN_POINT('Ctrl Pts',(-3.76907609832522,-1.,-1.0321778660492));
#64854=CARTESIAN_POINT('Ctrl Pts',(-3.76907609832522,1.,-1.0321778660492));
#64855=CARTESIAN_POINT('Ctrl Pts',(-3.76270122291232,-1.,-1.02833014458181));
#64856=CARTESIAN_POINT('Ctrl Pts',(-3.76270122291232,1.,-1.02833014458181));
#64857=CARTESIAN_POINT('Ctrl Pts',(-3.75631037456194,-1.,-1.0245342944466));
#64858=CARTESIAN_POINT('Ctrl Pts',(-3.75631037456194,1.,-1.0245342944466));
#64859=CARTESIAN_POINT('Ctrl Pts',(-3.74987777155834,-1.,-1.02078510487428));
#64860=CARTESIAN_POINT('Ctrl Pts',(-3.74987777155834,1.,-1.02078510487428));
#64861=CARTESIAN_POINT('Ctrl Pts',(-3.74337942504959,-1.,-1.01707794311079));
#64862=CARTESIAN_POINT('Ctrl Pts',(-3.74337942504959,1.,-1.01707794311079));
#64863=CARTESIAN_POINT('Ctrl Pts',(-3.73680245055734,-1.,-1.01341114319903));
#64864=CARTESIAN_POINT('Ctrl Pts',(-3.73680245055734,1.,-1.01341114319903));
#64865=CARTESIAN_POINT('Ctrl Pts',(-3.73015276704426,-1.,-1.00978798539496));
#64866=CARTESIAN_POINT('Ctrl Pts',(-3.73015276704426,1.,-1.00978798539496));
#64867=CARTESIAN_POINT('Ctrl Pts',(-3.72346803750595,-1.,-1.0062200073571));
#64868=CARTESIAN_POINT('Ctrl Pts',(-3.72346803750595,1.,-1.0062200073571));
#64869=CARTESIAN_POINT('Ctrl Pts',(-3.71680667125118,-1.,-1.00272423396822));
#64870=CARTESIAN_POINT('Ctrl Pts',(-3.71680667125118,1.,-1.00272423396822));
#64871=CARTESIAN_POINT('Ctrl Pts',(-3.71022439713938,-1.,-0.99931726075653));
#64872=CARTESIAN_POINT('Ctrl Pts',(-3.71022439713938,1.,-0.99931726075653));
#64873=CARTESIAN_POINT('Ctrl Pts',(-3.70375282282138,-1.,-0.996009819772518));
#64874=CARTESIAN_POINT('Ctrl Pts',(-3.70375282282138,1.,-0.996009819772518));
#64875=CARTESIAN_POINT('Ctrl Pts',(-3.69738123415662,-1.,-0.99280221833201));
#64876=CARTESIAN_POINT('Ctrl Pts',(-3.69738123415662,1.,-0.99280221833201));
#64877=CARTESIAN_POINT('Ctrl Pts',(-3.69102682138846,-1.,-0.989676715398558));
#64878=CARTESIAN_POINT('Ctrl Pts',(-3.69102682138846,1.,-0.989676715398558));
#64879=CARTESIAN_POINT('Ctrl Pts',(-3.68455317926068,-1.,-0.986602639863837));
#64880=CARTESIAN_POINT('Ctrl Pts',(-3.68455317926068,1.,-0.986602639863837));
#64881=CARTESIAN_POINT('Ctrl Pts',(-3.67782408841715,-1.,-0.983550791470419));
#64882=CARTESIAN_POINT('Ctrl Pts',(-3.67782408841715,1.,-0.983550791470419));
#64883=CARTESIAN_POINT('Ctrl Pts',(-3.67074983340361,-1.,-0.980505922458267));
#64884=CARTESIAN_POINT('Ctrl Pts',(-3.67074983340361,1.,-0.980505922458267));
#64885=CARTESIAN_POINT('Ctrl Pts',(-3.66333049637475,-1.,-0.977478312751618));
#64886=CARTESIAN_POINT('Ctrl Pts',(-3.66333049637475,1.,-0.977478312751618));
#64887=CARTESIAN_POINT('Ctrl Pts',(-3.65571576735126,-1.,-0.974519971354848));
#64888=CARTESIAN_POINT('Ctrl Pts',(-3.65571576735126,1.,-0.974519971354848));
#64889=CARTESIAN_POINT('Ctrl Pts',(-3.64819756447455,-1.,-0.971722122061341));
#64890=CARTESIAN_POINT('Ctrl Pts',(-3.64819756447455,1.,-0.971722122061341));
#64891=CARTESIAN_POINT('Ctrl Pts',(-3.64113946505766,-1.,-0.969195124675865));
#64892=CARTESIAN_POINT('Ctrl Pts',(-3.64113946505766,1.,-0.969195124675865));
#64893=CARTESIAN_POINT('Ctrl Pts',(-3.63492122081143,-1.,-0.967052554541385));
#64894=CARTESIAN_POINT('Ctrl Pts',(-3.63492122081143,1.,-0.967052554541385));
#64895=CARTESIAN_POINT('Ctrl Pts',(-3.62988252139846,-1.,-0.965395153165293));
#64896=CARTESIAN_POINT('Ctrl Pts',(-3.62988252139846,1.,-0.965395153165293));
#64897=CARTESIAN_POINT('Ctrl Pts',(-3.62625391254797,-1.,-0.964291001273287));
#64898=CARTESIAN_POINT('Ctrl Pts',(-3.62625391254797,1.,-0.964291001273287));
#64899=CARTESIAN_POINT('Ctrl Pts',(-3.6245656860652,-1.,-0.963875774530619));
#64900=CARTESIAN_POINT('Ctrl Pts',(-3.6245656860652,1.,-0.963875774530619));
#64901=CARTESIAN_POINT('Ctrl Pts',(-3.62399933639914,-1.,-0.963832486395051));
#64902=CARTESIAN_POINT('Ctrl Pts',(-3.62399933639914,1.,-0.963832486395051));
#64903=CARTESIAN_POINT('Ctrl Pts',(-3.62393257642052,-1.,-0.963922720982193));
#64904=CARTESIAN_POINT('Ctrl Pts',(-3.62393257642052,1.,-0.963922720982193));
#64905=CARTESIAN_POINT('Ctrl Pts',(-3.62397690409552,-1.,-0.963997613369571));
#64906=CARTESIAN_POINT('Ctrl Pts',(-3.62397690409552,1.,-0.963997613369571));
#64907=CARTESIAN_POINT('',(-4.01728681790024,1.,-1.22531898815164));
#64908=CARTESIAN_POINT('Ctrl Pts',(-4.01728681790024,1.,-1.22531898815164));
#64909=CARTESIAN_POINT('Ctrl Pts',(-4.0161454457032,1.,-1.22423716681447));
#64910=CARTESIAN_POINT('Ctrl Pts',(-4.01386104434674,1.,-1.22207656456199));
#64911=CARTESIAN_POINT('Ctrl Pts',(-4.01042947142681,1.,-1.21884478244983));
#64912=CARTESIAN_POINT('Ctrl Pts',(-4.00584409524937,1.,-1.21455398918813));
#64913=CARTESIAN_POINT('Ctrl Pts',(-4.00009577952534,1.,-1.20922097030107));
#64914=CARTESIAN_POINT('Ctrl Pts',(-3.99433084800649,1.,-1.2039185237544));
#64915=CARTESIAN_POINT('Ctrl Pts',(-3.98854928957287,1.,-1.19864679609596));
#64916=CARTESIAN_POINT('Ctrl Pts',(-3.98275111052015,1.,-1.19340598349307));
#64917=CARTESIAN_POINT('Ctrl Pts',(-3.97693634766926,1.,-1.18819633715285));
#64918=CARTESIAN_POINT('Ctrl Pts',(-3.9711050516465,1.,-1.18301815039596));
#64919=CARTESIAN_POINT('Ctrl Pts',(-3.96525726357682,1.,-1.17787174135445));
#64920=CARTESIAN_POINT('Ctrl Pts',(-3.95939299213164,1.,-1.17275743590327));
#64921=CARTESIAN_POINT('Ctrl Pts',(-3.95351219510062,1.,-1.16767555244495));
#64922=CARTESIAN_POINT('Ctrl Pts',(-3.9476147478092,1.,-1.16262637999261));
#64923=CARTESIAN_POINT('Ctrl Pts',(-3.94170046685542,1.,-1.1576101834106));
#64924=CARTESIAN_POINT('Ctrl Pts',(-3.9357691705651,1.,-1.1526272271639));
#64925=CARTESIAN_POINT('Ctrl Pts',(-3.92982073294334,1.,-1.14767779451147));
#64926=CARTESIAN_POINT('Ctrl Pts',(-3.92385513133937,1.,-1.14276220561575));
#64927=CARTESIAN_POINT('Ctrl Pts',(-3.91787251936688,1.,-1.13788084225511));
#64928=CARTESIAN_POINT('Ctrl Pts',(-3.91187321145495,1.,-1.13303414693849));
#64929=CARTESIAN_POINT('Ctrl Pts',(-3.90585753318622,1.,-1.12822258281518));
#64930=CARTESIAN_POINT('Ctrl Pts',(-3.89982569749978,1.,-1.12344660099029));
#64931=CARTESIAN_POINT('Ctrl Pts',(-3.89377768340362,1.,-1.11870660794609));
#64932=CARTESIAN_POINT('Ctrl Pts',(-3.88771308285229,1.,-1.11400292434447));
#64933=CARTESIAN_POINT('Ctrl Pts',(-3.88163105531791,1.,-1.10933577224029));
#64934=CARTESIAN_POINT('Ctrl Pts',(-3.87553067187566,1.,-1.10470536603303));
#64935=CARTESIAN_POINT('Ctrl Pts',(-3.86941120134872,1.,-1.10011198761202));
#64936=CARTESIAN_POINT('Ctrl Pts',(-3.86327241021242,1.,-1.09555606505012));
#64937=CARTESIAN_POINT('Ctrl Pts',(-3.85711487933911,1.,-1.09103825516288));
#64938=CARTESIAN_POINT('Ctrl Pts',(-3.8509402522269,1.,-1.08655950846377));
#64939=CARTESIAN_POINT('Ctrl Pts',(-3.84475048030615,1.,-1.08212087917986));
#64940=CARTESIAN_POINT('Ctrl Pts',(-3.83854714117486,1.,-1.07772335353856));
#64941=CARTESIAN_POINT('Ctrl Pts',(-3.83233071195145,1.,-1.0733676663346));
#64942=CARTESIAN_POINT('Ctrl Pts',(-3.82609989967278,1.,-1.0690541318036));
#64943=CARTESIAN_POINT('Ctrl Pts',(-3.81985083953012,1.,-1.06478244038931));
#64944=CARTESIAN_POINT('Ctrl Pts',(-3.81357866117485,1.,-1.06055206187298));
#64945=CARTESIAN_POINT('Ctrl Pts',(-3.80727913637784,1.,-1.05636266918643));
#64946=CARTESIAN_POINT('Ctrl Pts',(-3.80095039790678,1.,-1.05221457990015));
#64947=CARTESIAN_POINT('Ctrl Pts',(-3.79459440308793,1.,-1.04810913267641));
#64948=CARTESIAN_POINT('Ctrl Pts',(-3.78821910787195,1.,-1.04404924374426));
#64949=CARTESIAN_POINT('Ctrl Pts',(-3.78183535008192,1.,-1.04003862055804));
#64950=CARTESIAN_POINT('Ctrl Pts',(-3.77545283140445,1.,-1.03608074678013));
#64951=CARTESIAN_POINT('Ctrl Pts',(-3.76907609832522,1.,-1.0321778660492));
#64952=CARTESIAN_POINT('Ctrl Pts',(-3.76270122291232,1.,-1.02833014458181));
#64953=CARTESIAN_POINT('Ctrl Pts',(-3.75631037456194,1.,-1.0245342944466));
#64954=CARTESIAN_POINT('Ctrl Pts',(-3.74987777155834,1.,-1.02078510487428));
#64955=CARTESIAN_POINT('Ctrl Pts',(-3.74337942504959,1.,-1.01707794311079));
#64956=CARTESIAN_POINT('Ctrl Pts',(-3.73680245055734,1.,-1.01341114319903));
#64957=CARTESIAN_POINT('Ctrl Pts',(-3.73015276704426,1.,-1.00978798539496));
#64958=CARTESIAN_POINT('Ctrl Pts',(-3.72346803750595,1.,-1.0062200073571));
#64959=CARTESIAN_POINT('Ctrl Pts',(-3.71680667125118,1.,-1.00272423396822));
#64960=CARTESIAN_POINT('Ctrl Pts',(-3.71022439713938,1.,-0.99931726075653));
#64961=CARTESIAN_POINT('Ctrl Pts',(-3.70375282282138,1.,-0.996009819772518));
#64962=CARTESIAN_POINT('Ctrl Pts',(-3.69738123415662,1.,-0.99280221833201));
#64963=CARTESIAN_POINT('Ctrl Pts',(-3.69102682138846,1.,-0.989676715398558));
#64964=CARTESIAN_POINT('Ctrl Pts',(-3.68455317926068,1.,-0.986602639863837));
#64965=CARTESIAN_POINT('Ctrl Pts',(-3.67782408841715,1.,-0.983550791470419));
#64966=CARTESIAN_POINT('Ctrl Pts',(-3.67074983340361,1.,-0.980505922458267));
#64967=CARTESIAN_POINT('Ctrl Pts',(-3.66333049637475,1.,-0.977478312751618));
#64968=CARTESIAN_POINT('Ctrl Pts',(-3.65571576735126,1.,-0.974519971354848));
#64969=CARTESIAN_POINT('Ctrl Pts',(-3.64819756447455,1.,-0.971722122061341));
#64970=CARTESIAN_POINT('Ctrl Pts',(-3.64113946505766,1.,-0.969195124675865));
#64971=CARTESIAN_POINT('Ctrl Pts',(-3.63492122081143,1.,-0.967052554541385));
#64972=CARTESIAN_POINT('Ctrl Pts',(-3.62988252139846,1.,-0.965395153165293));
#64973=CARTESIAN_POINT('Ctrl Pts',(-3.62652618145335,1.,-0.964373850166458));
#64974=CARTESIAN_POINT('Ctrl Pts',(-3.62489305727662,1.,-0.963957782642843));
#64975=CARTESIAN_POINT('Ctrl Pts',(-3.62424461507588,1.,-0.963861297423241));
#64976=CARTESIAN_POINT('Ctrl Pts',(-3.6240482887845,1.,-0.963880158555582));
#64977=CARTESIAN_POINT('Ctrl Pts',(-3.62400312501245,1.,-0.963899035117249));
#64978=CARTESIAN_POINT('',(-4.01728681790024,0.,-1.22531898815164));
#64979=CARTESIAN_POINT('Ctrl Pts',(-3.49848248301936,-1.,-1.35022972712301));
#64980=CARTESIAN_POINT('Ctrl Pts',(-3.49848248301936,1.,-1.35022972712301));
#64981=CARTESIAN_POINT('Ctrl Pts',(-3.4984026005375,-1.,-1.35026426118402));
#64982=CARTESIAN_POINT('Ctrl Pts',(-3.4984026005375,1.,-1.35026426118402));
#64983=CARTESIAN_POINT('Ctrl Pts',(-3.49840357193736,-1.,-1.35037650303019));
#64984=CARTESIAN_POINT('Ctrl Pts',(-3.49840357193736,1.,-1.35037650303019));
#64985=CARTESIAN_POINT('Ctrl Pts',(-3.49888720257132,-1.,-1.35067437417483));
#64986=CARTESIAN_POINT('Ctrl Pts',(-3.49888720257132,1.,-1.35067437417483));
#64987=CARTESIAN_POINT('Ctrl Pts',(-3.5004970706414,-1.,-1.3513307633124));
#64988=CARTESIAN_POINT('Ctrl Pts',(-3.5004970706414,1.,-1.3513307633124));
#64989=CARTESIAN_POINT('Ctrl Pts',(-3.50408168106261,-1.,-1.35257032843486));
#64990=CARTESIAN_POINT('Ctrl Pts',(-3.50408168106261,1.,-1.35257032843486));
#64991=CARTESIAN_POINT('Ctrl Pts',(-3.50913227059999,-1.,-1.35419113575956));
#64992=CARTESIAN_POINT('Ctrl Pts',(-3.50913227059999,1.,-1.35419113575956));
#64993=CARTESIAN_POINT('Ctrl Pts',(-3.51542230699556,-1.,-1.35611275237152));
#64994=CARTESIAN_POINT('Ctrl Pts',(-3.51542230699556,1.,-1.35611275237152));
#64995=CARTESIAN_POINT('Ctrl Pts',(-3.52261776116748,-1.,-1.35821701528836));
#64996=CARTESIAN_POINT('Ctrl Pts',(-3.52261776116748,1.,-1.35821701528836));
#64997=CARTESIAN_POINT('Ctrl Pts',(-3.530344649616,-1.,-1.36037259643734));
#64998=CARTESIAN_POINT('Ctrl Pts',(-3.530344649616,1.,-1.36037259643734));
#64999=CARTESIAN_POINT('Ctrl Pts',(-3.53824396424961,-1.,-1.36245507339307));
#65000=CARTESIAN_POINT('Ctrl Pts',(-3.53824396424961,1.,-1.36245507339307));
#65001=CARTESIAN_POINT('Ctrl Pts',(-3.54602591832973,-1.,-1.36436666257597));
#65002=CARTESIAN_POINT('Ctrl Pts',(-3.54602591832973,1.,-1.36436666257597));
#65003=CARTESIAN_POINT('Ctrl Pts',(-3.55353883995949,-1.,-1.3660614545677));
#65004=CARTESIAN_POINT('Ctrl Pts',(-3.55353883995949,1.,-1.3660614545677));
#65005=CARTESIAN_POINT('Ctrl Pts',(-3.56077662028649,-1.,-1.36754771771233));
#65006=CARTESIAN_POINT('Ctrl Pts',(-3.56077662028649,1.,-1.36754771771233));
#65007=CARTESIAN_POINT('Ctrl Pts',(-3.5678208030466,-1.,-1.36886584973389));
#65008=CARTESIAN_POINT('Ctrl Pts',(-3.5678208030466,1.,-1.36886584973389));
#65009=CARTESIAN_POINT('Ctrl Pts',(-3.57479875549486,-1.,-1.37007229485659));
#65010=CARTESIAN_POINT('Ctrl Pts',(-3.57479875549486,1.,-1.37007229485659));
#65011=CARTESIAN_POINT('Ctrl Pts',(-3.58183885982715,-1.,-1.37122241663062));
#65012=CARTESIAN_POINT('Ctrl Pts',(-3.58183885982715,1.,-1.37122241663062));
#65013=CARTESIAN_POINT('Ctrl Pts',(-3.58901853846365,-1.,-1.37235053660976));
#65014=CARTESIAN_POINT('Ctrl Pts',(-3.58901853846365,1.,-1.37235053660976));
#65015=CARTESIAN_POINT('Ctrl Pts',(-3.59634627869048,-1.,-1.37346320103157));
#65016=CARTESIAN_POINT('Ctrl Pts',(-3.59634627869048,1.,-1.37346320103157));
#65017=CARTESIAN_POINT('Ctrl Pts',(-3.60379020123988,-1.,-1.37455051379623));
#65018=CARTESIAN_POINT('Ctrl Pts',(-3.60379020123988,1.,-1.37455051379623));
#65019=CARTESIAN_POINT('Ctrl Pts',(-3.61129546591064,-1.,-1.37559314436634));
#65020=CARTESIAN_POINT('Ctrl Pts',(-3.61129546591064,1.,-1.37559314436634));
#65021=CARTESIAN_POINT('Ctrl Pts',(-3.6188048116042,-1.,-1.37657053403107));
#65022=CARTESIAN_POINT('Ctrl Pts',(-3.6188048116042,1.,-1.37657053403107));
#65023=CARTESIAN_POINT('Ctrl Pts',(-3.62628098665145,-1.,-1.37746987919881));
#65024=CARTESIAN_POINT('Ctrl Pts',(-3.62628098665145,1.,-1.37746987919881));
#65025=CARTESIAN_POINT('Ctrl Pts',(-3.63371727442486,-1.,-1.37829035457339));
#65026=CARTESIAN_POINT('Ctrl Pts',(-3.63371727442486,1.,-1.37829035457339));
#65027=CARTESIAN_POINT('Ctrl Pts',(-3.64112507791141,-1.,-1.37903818567359));
#65028=CARTESIAN_POINT('Ctrl Pts',(-3.64112507791141,1.,-1.37903818567359));
#65029=CARTESIAN_POINT('Ctrl Pts',(-3.64852652756456,-1.,-1.37972372481603));
#65030=CARTESIAN_POINT('Ctrl Pts',(-3.64852652756456,1.,-1.37972372481603));
#65031=CARTESIAN_POINT('Ctrl Pts',(-3.6559455440439,-1.,-1.38035791051212));
#65032=CARTESIAN_POINT('Ctrl Pts',(-3.6559455440439,1.,-1.38035791051212));
#65033=CARTESIAN_POINT('Ctrl Pts',(-3.66339848520857,-1.,-1.38094856333552));
#65034=CARTESIAN_POINT('Ctrl Pts',(-3.66339848520857,1.,-1.38094856333552));
#65035=CARTESIAN_POINT('Ctrl Pts',(-3.67088843112262,-1.,-1.38149812653868));
#65036=CARTESIAN_POINT('Ctrl Pts',(-3.67088843112262,1.,-1.38149812653868));
#65037=CARTESIAN_POINT('Ctrl Pts',(-3.67841038482414,-1.,-1.3820057429062));
#65038=CARTESIAN_POINT('Ctrl Pts',(-3.67841038482414,1.,-1.3820057429062));
#65039=CARTESIAN_POINT('Ctrl Pts',(-3.68595444983837,-1.,-1.38246852827182));
#65040=CARTESIAN_POINT('Ctrl Pts',(-3.68595444983837,1.,-1.38246852827182));
#65041=CARTESIAN_POINT('Ctrl Pts',(-3.69350967899526,-1.,-1.3828831117165));
#65042=CARTESIAN_POINT('Ctrl Pts',(-3.69350967899526,1.,-1.3828831117165));
#65043=CARTESIAN_POINT('Ctrl Pts',(-3.701067921679,-1.,-1.38324717612865));
#65044=CARTESIAN_POINT('Ctrl Pts',(-3.701067921679,1.,-1.38324717612865));
#65045=CARTESIAN_POINT('Ctrl Pts',(-3.70862680753347,-1.,-1.38356065402124));
#65046=CARTESIAN_POINT('Ctrl Pts',(-3.70862680753347,1.,-1.38356065402124));
#65047=CARTESIAN_POINT('Ctrl Pts',(-3.7161876605181,-1.,-1.38382489984586));
#65048=CARTESIAN_POINT('Ctrl Pts',(-3.7161876605181,1.,-1.38382489984586));
#65049=CARTESIAN_POINT('Ctrl Pts',(-3.72375409358803,-1.,-1.3840421342895));
#65050=CARTESIAN_POINT('Ctrl Pts',(-3.72375409358803,1.,-1.3840421342895));
#65051=CARTESIAN_POINT('Ctrl Pts',(-3.73133035859282,-1.,-1.38421479111531));
#65052=CARTESIAN_POINT('Ctrl Pts',(-3.73133035859282,1.,-1.38421479111531));
#65053=CARTESIAN_POINT('Ctrl Pts',(-3.73891976418104,-1.,-1.38434489156458));
#65054=CARTESIAN_POINT('Ctrl Pts',(-3.73891976418104,1.,-1.38434489156458));
#65055=CARTESIAN_POINT('Ctrl Pts',(-3.74652317167876,-1.,-1.38443344984394));
#65056=CARTESIAN_POINT('Ctrl Pts',(-3.74652317167876,1.,-1.38443344984394));
#65057=CARTESIAN_POINT('Ctrl Pts',(-3.7541397631875,-1.,-1.38448077997163));
#65058=CARTESIAN_POINT('Ctrl Pts',(-3.7541397631875,1.,-1.38448077997163));
#65059=CARTESIAN_POINT('Ctrl Pts',(-3.76176768271367,-1.,-1.3844867525335));
#65060=CARTESIAN_POINT('Ctrl Pts',(-3.76176768271367,1.,-1.3844867525335));
#65061=CARTESIAN_POINT('Ctrl Pts',(-3.76940473185779,-1.,-1.38445107339518));
#65062=CARTESIAN_POINT('Ctrl Pts',(-3.76940473185779,1.,-1.38445107339518));
#65063=CARTESIAN_POINT('Ctrl Pts',(-3.77704902230418,-1.,-1.38437354551428));
#65064=CARTESIAN_POINT('Ctrl Pts',(-3.77704902230418,1.,-1.38437354551428));
#65065=CARTESIAN_POINT('Ctrl Pts',(-3.78469969805082,-1.,-1.38425435883756));
#65066=CARTESIAN_POINT('Ctrl Pts',(-3.78469969805082,1.,-1.38425435883756));
#65067=CARTESIAN_POINT('Ctrl Pts',(-3.79235669640841,-1.,-1.38409399694566));
#65068=CARTESIAN_POINT('Ctrl Pts',(-3.79235669640841,1.,-1.38409399694566));
#65069=CARTESIAN_POINT('Ctrl Pts',(-3.80002044322111,-1.,-1.38389311766682));
#65070=CARTESIAN_POINT('Ctrl Pts',(-3.80002044322111,1.,-1.38389311766682));
#65071=CARTESIAN_POINT('Ctrl Pts',(-3.80769156398411,-1.,-1.3836524404622));
#65072=CARTESIAN_POINT('Ctrl Pts',(-3.80769156398411,1.,-1.3836524404622));
#65073=CARTESIAN_POINT('Ctrl Pts',(-3.81537060817811,-1.,-1.38337263902782));
#65074=CARTESIAN_POINT('Ctrl Pts',(-3.81537060817811,1.,-1.38337263902782));
#65075=CARTESIAN_POINT('Ctrl Pts',(-3.82305771743829,-1.,-1.38305421262763));
#65076=CARTESIAN_POINT('Ctrl Pts',(-3.82305771743829,1.,-1.38305421262763));
#65077=CARTESIAN_POINT('Ctrl Pts',(-3.8307526698229,-1.,-1.38269750245138));
#65078=CARTESIAN_POINT('Ctrl Pts',(-3.8307526698229,1.,-1.38269750245138));
#65079=CARTESIAN_POINT('Ctrl Pts',(-3.83845502790746,-1.,-1.38230274828821));
#65080=CARTESIAN_POINT('Ctrl Pts',(-3.83845502790746,1.,-1.38230274828821));
#65081=CARTESIAN_POINT('Ctrl Pts',(-3.84616425605764,-1.,-1.38187013346109));
#65082=CARTESIAN_POINT('Ctrl Pts',(-3.84616425605764,1.,-1.38187013346109));
#65083=CARTESIAN_POINT('Ctrl Pts',(-3.85387983979481,-1.,-1.38139983115049));
#65084=CARTESIAN_POINT('Ctrl Pts',(-3.85387983979481,1.,-1.38139983115049));
#65085=CARTESIAN_POINT('Ctrl Pts',(-3.86160143043959,-1.,-1.38089205992989));
#65086=CARTESIAN_POINT('Ctrl Pts',(-3.86160143043959,1.,-1.38089205992989));
#65087=CARTESIAN_POINT('Ctrl Pts',(-3.86932885813068,-1.,-1.38034709213014));
#65088=CARTESIAN_POINT('Ctrl Pts',(-3.86932885813068,1.,-1.38034709213014));
#65089=CARTESIAN_POINT('Ctrl Pts',(-3.87706205830532,-1.,-1.37976523097073));
#65090=CARTESIAN_POINT('Ctrl Pts',(-3.87706205830532,1.,-1.37976523097073));
#65091=CARTESIAN_POINT('Ctrl Pts',(-3.88480102249277,-1.,-1.37914679719383));
#65092=CARTESIAN_POINT('Ctrl Pts',(-3.88480102249277,1.,-1.37914679719383));
#65093=CARTESIAN_POINT('Ctrl Pts',(-3.89254574338496,-1.,-1.3784921128802));
#65094=CARTESIAN_POINT('Ctrl Pts',(-3.89254574338496,1.,-1.3784921128802));
#65095=CARTESIAN_POINT('Ctrl Pts',(-3.90029615196727,-1.,-1.37780148512792));
#65096=CARTESIAN_POINT('Ctrl Pts',(-3.90029615196727,1.,-1.37780148512792));
#65097=CARTESIAN_POINT('Ctrl Pts',(-3.90805209523486,-1.,-1.3770751963402));
#65098=CARTESIAN_POINT('Ctrl Pts',(-3.90805209523486,1.,-1.3770751963402));
#65099=CARTESIAN_POINT('Ctrl Pts',(-3.91581337462644,-1.,-1.37631350505797));
#65100=CARTESIAN_POINT('Ctrl Pts',(-3.91581337462644,1.,-1.37631350505797));
#65101=CARTESIAN_POINT('Ctrl Pts',(-3.92357976987672,-1.,-1.37551664448242));
#65102=CARTESIAN_POINT('Ctrl Pts',(-3.92357976987672,1.,-1.37551664448242));
#65103=CARTESIAN_POINT('Ctrl Pts',(-3.93135106761844,-1.,-1.37468482215751));
#65104=CARTESIAN_POINT('Ctrl Pts',(-3.93135106761844,1.,-1.37468482215751));
#65105=CARTESIAN_POINT('Ctrl Pts',(-3.93912709040818,-1.,-1.37381821967165));
#65106=CARTESIAN_POINT('Ctrl Pts',(-3.93912709040818,1.,-1.37381821967165));
#65107=CARTESIAN_POINT('Ctrl Pts',(-3.94690771785133,-1.,-1.37291699202807));
#65108=CARTESIAN_POINT('Ctrl Pts',(-3.94690771785133,1.,-1.37291699202807));
#65109=CARTESIAN_POINT('Ctrl Pts',(-3.95469287280914,-1.,-1.37198126432386));
#65110=CARTESIAN_POINT('Ctrl Pts',(-3.95469287280914,1.,-1.37198126432386));
#65111=CARTESIAN_POINT('Ctrl Pts',(-3.96092458506535,-1.,-1.3712051561502));
#65112=CARTESIAN_POINT('Ctrl Pts',(-3.96092458506535,1.,-1.3712051561502));
#65113=CARTESIAN_POINT('Ctrl Pts',(-3.96560037974645,-1.,-1.37060761745635));
#65114=CARTESIAN_POINT('Ctrl Pts',(-3.96560037974645,1.,-1.37060761745635));
#65115=CARTESIAN_POINT('Ctrl Pts',(-3.9687184694131,-1.,-1.37020239094614));
#65116=CARTESIAN_POINT('Ctrl Pts',(-3.9687184694131,1.,-1.37020239094614));
#65117=CARTESIAN_POINT('Ctrl Pts',(-3.97027773754922,-1.,-1.36999806084572));
#65118=CARTESIAN_POINT('Ctrl Pts',(-3.97027773754922,1.,-1.36999806084572));
#65119=CARTESIAN_POINT('',(-3.4984457533445,1.,-1.35032489087101));
#65120=CARTESIAN_POINT('Ctrl Pts',(-3.4984457533445,-1.,-1.35032489087101));
#65121=CARTESIAN_POINT('Ctrl Pts',(-3.4984457533445,-0.666666666666667,
-1.35032489087101));
#65122=CARTESIAN_POINT('Ctrl Pts',(-3.4984457533445,-0.333333333333333,
-1.35032489087101));
#65123=CARTESIAN_POINT('Ctrl Pts',(-3.4984457533445,0.333333333333333,-1.35032489087101));
#65124=CARTESIAN_POINT('Ctrl Pts',(-3.4984457533445,0.666666666666667,-1.35032489087101));
#65125=CARTESIAN_POINT('Ctrl Pts',(-3.4984457533445,1.,-1.35032489087101));
#65126=CARTESIAN_POINT('',(-3.97027773754922,1.,-1.36999806084572));
#65127=CARTESIAN_POINT('',(-3.97027773754922,0.,-1.36999806084572));
#65128=CARTESIAN_POINT('Ctrl Pts',(-3.4984457533445,1.,-1.35032489087101));
#65129=CARTESIAN_POINT('Ctrl Pts',(-3.49847119623846,1.,-1.35036670892966));
#65130=CARTESIAN_POINT('Ctrl Pts',(-3.49861894124827,1.,-1.35049736560527));
#65131=CARTESIAN_POINT('Ctrl Pts',(-3.49920025459723,1.,-1.35080045218587));
#65132=CARTESIAN_POINT('Ctrl Pts',(-3.5007660381649,1.,-1.35142377279517));
#65133=CARTESIAN_POINT('Ctrl Pts',(-3.50408168106261,1.,-1.35257032843486));
#65134=CARTESIAN_POINT('Ctrl Pts',(-3.50913227059999,1.,-1.35419113575956));
#65135=CARTESIAN_POINT('Ctrl Pts',(-3.51542230699556,1.,-1.35611275237152));
#65136=CARTESIAN_POINT('Ctrl Pts',(-3.52261776116748,1.,-1.35821701528836));
#65137=CARTESIAN_POINT('Ctrl Pts',(-3.530344649616,1.,-1.36037259643734));
#65138=CARTESIAN_POINT('Ctrl Pts',(-3.53824396424961,1.,-1.36245507339307));
#65139=CARTESIAN_POINT('Ctrl Pts',(-3.54602591832973,1.,-1.36436666257597));
#65140=CARTESIAN_POINT('Ctrl Pts',(-3.55353883995949,1.,-1.3660614545677));
#65141=CARTESIAN_POINT('Ctrl Pts',(-3.56077662028649,1.,-1.36754771771233));
#65142=CARTESIAN_POINT('Ctrl Pts',(-3.5678208030466,1.,-1.36886584973389));
#65143=CARTESIAN_POINT('Ctrl Pts',(-3.57479875549486,1.,-1.37007229485659));
#65144=CARTESIAN_POINT('Ctrl Pts',(-3.58183885982715,1.,-1.37122241663062));
#65145=CARTESIAN_POINT('Ctrl Pts',(-3.58901853846365,1.,-1.37235053660976));
#65146=CARTESIAN_POINT('Ctrl Pts',(-3.59634627869048,1.,-1.37346320103157));
#65147=CARTESIAN_POINT('Ctrl Pts',(-3.60379020123988,1.,-1.37455051379623));
#65148=CARTESIAN_POINT('Ctrl Pts',(-3.61129546591064,1.,-1.37559314436634));
#65149=CARTESIAN_POINT('Ctrl Pts',(-3.6188048116042,1.,-1.37657053403107));
#65150=CARTESIAN_POINT('Ctrl Pts',(-3.62628098665145,1.,-1.37746987919881));
#65151=CARTESIAN_POINT('Ctrl Pts',(-3.63371727442486,1.,-1.37829035457339));
#65152=CARTESIAN_POINT('Ctrl Pts',(-3.64112507791141,1.,-1.37903818567359));
#65153=CARTESIAN_POINT('Ctrl Pts',(-3.64852652756456,1.,-1.37972372481603));
#65154=CARTESIAN_POINT('Ctrl Pts',(-3.6559455440439,1.,-1.38035791051212));
#65155=CARTESIAN_POINT('Ctrl Pts',(-3.66339848520857,1.,-1.38094856333552));
#65156=CARTESIAN_POINT('Ctrl Pts',(-3.67088843112262,1.,-1.38149812653868));
#65157=CARTESIAN_POINT('Ctrl Pts',(-3.67841038482414,1.,-1.3820057429062));
#65158=CARTESIAN_POINT('Ctrl Pts',(-3.68595444983837,1.,-1.38246852827182));
#65159=CARTESIAN_POINT('Ctrl Pts',(-3.69350967899526,1.,-1.3828831117165));
#65160=CARTESIAN_POINT('Ctrl Pts',(-3.701067921679,1.,-1.38324717612865));
#65161=CARTESIAN_POINT('Ctrl Pts',(-3.70862680753347,1.,-1.38356065402124));
#65162=CARTESIAN_POINT('Ctrl Pts',(-3.7161876605181,1.,-1.38382489984586));
#65163=CARTESIAN_POINT('Ctrl Pts',(-3.72375409358803,1.,-1.3840421342895));
#65164=CARTESIAN_POINT('Ctrl Pts',(-3.73133035859282,1.,-1.38421479111531));
#65165=CARTESIAN_POINT('Ctrl Pts',(-3.73891976418104,1.,-1.38434489156458));
#65166=CARTESIAN_POINT('Ctrl Pts',(-3.74652317167876,1.,-1.38443344984394));
#65167=CARTESIAN_POINT('Ctrl Pts',(-3.7541397631875,1.,-1.38448077997163));
#65168=CARTESIAN_POINT('Ctrl Pts',(-3.76176768271367,1.,-1.3844867525335));
#65169=CARTESIAN_POINT('Ctrl Pts',(-3.76940473185779,1.,-1.38445107339518));
#65170=CARTESIAN_POINT('Ctrl Pts',(-3.77704902230418,1.,-1.38437354551428));
#65171=CARTESIAN_POINT('Ctrl Pts',(-3.78469969805082,1.,-1.38425435883756));
#65172=CARTESIAN_POINT('Ctrl Pts',(-3.79235669640841,1.,-1.38409399694566));
#65173=CARTESIAN_POINT('Ctrl Pts',(-3.80002044322111,1.,-1.38389311766682));
#65174=CARTESIAN_POINT('Ctrl Pts',(-3.80769156398411,1.,-1.3836524404622));
#65175=CARTESIAN_POINT('Ctrl Pts',(-3.81537060817811,1.,-1.38337263902782));
#65176=CARTESIAN_POINT('Ctrl Pts',(-3.82305771743829,1.,-1.38305421262763));
#65177=CARTESIAN_POINT('Ctrl Pts',(-3.8307526698229,1.,-1.38269750245138));
#65178=CARTESIAN_POINT('Ctrl Pts',(-3.83845502790746,1.,-1.38230274828821));
#65179=CARTESIAN_POINT('Ctrl Pts',(-3.84616425605764,1.,-1.38187013346109));
#65180=CARTESIAN_POINT('Ctrl Pts',(-3.85387983979481,1.,-1.38139983115049));
#65181=CARTESIAN_POINT('Ctrl Pts',(-3.86160143043959,1.,-1.38089205992989));
#65182=CARTESIAN_POINT('Ctrl Pts',(-3.86932885813068,1.,-1.38034709213014));
#65183=CARTESIAN_POINT('Ctrl Pts',(-3.87706205830532,1.,-1.37976523097073));
#65184=CARTESIAN_POINT('Ctrl Pts',(-3.88480102249277,1.,-1.37914679719383));
#65185=CARTESIAN_POINT('Ctrl Pts',(-3.89254574338496,1.,-1.3784921128802));
#65186=CARTESIAN_POINT('Ctrl Pts',(-3.90029615196727,1.,-1.37780148512792));
#65187=CARTESIAN_POINT('Ctrl Pts',(-3.90805209523486,1.,-1.3770751963402));
#65188=CARTESIAN_POINT('Ctrl Pts',(-3.91581337462644,1.,-1.37631350505797));
#65189=CARTESIAN_POINT('Ctrl Pts',(-3.92357976987672,1.,-1.37551664448242));
#65190=CARTESIAN_POINT('Ctrl Pts',(-3.93135106761844,1.,-1.37468482215751));
#65191=CARTESIAN_POINT('Ctrl Pts',(-3.93912709040818,1.,-1.37381821967165));
#65192=CARTESIAN_POINT('Ctrl Pts',(-3.94690771785133,1.,-1.37291699202807));
#65193=CARTESIAN_POINT('Ctrl Pts',(-3.95469287280914,1.,-1.37198126432386));
#65194=CARTESIAN_POINT('Ctrl Pts',(-3.96092458506535,1.,-1.3712051561502));
#65195=CARTESIAN_POINT('Ctrl Pts',(-3.96560037974645,1.,-1.37060761745635));
#65196=CARTESIAN_POINT('Ctrl Pts',(-3.9687184694131,1.,-1.37020239094614));
#65197=CARTESIAN_POINT('Ctrl Pts',(-3.97027773754922,1.,-1.36999806084572));
#65198=CARTESIAN_POINT('Origin',(-3.97027773754922,0.,-1.36999806084572));
#65199=CARTESIAN_POINT('',(-4.01728681790024,1.,-1.22531898815164));
#65200=CARTESIAN_POINT('Origin',(0.,0.,0.));
#65201=CARTESIAN_POINT('',(-3.42859860294378,1.,-1.51895082866166));
#65202=CARTESIAN_POINT('Origin',(0.,1.,0.));
#65203=CARTESIAN_POINT('Ctrl Pts',(-3.42859860294378,1.,-1.51895082866166));
#65204=CARTESIAN_POINT('Ctrl Pts',(-3.42859860294378,0.666666666666667,
-1.51895082866166));
#65205=CARTESIAN_POINT('Ctrl Pts',(-3.42859860294378,0.333333333333333,
-1.51895082866166));
#65206=CARTESIAN_POINT('Ctrl Pts',(-3.42859860294378,-0.333333333333333,
-1.51895082866166));
#65207=CARTESIAN_POINT('Ctrl Pts',(-3.42859860294378,-0.666666666666667,
-1.51895082866166));
#65208=CARTESIAN_POINT('Ctrl Pts',(-3.42859860294378,-1.,-1.51895082866166));
#65209=CARTESIAN_POINT('Ctrl Pts',(-3.77614523045147,-1.,-1.83867539237861));
#65210=CARTESIAN_POINT('Ctrl Pts',(-3.77614523045147,1.,-1.83867539237861));
#65211=CARTESIAN_POINT('Ctrl Pts',(-3.77518714458232,-1.,-1.83742834010821));
#65212=CARTESIAN_POINT('Ctrl Pts',(-3.77518714458232,1.,-1.83742834010821));
#65213=CARTESIAN_POINT('Ctrl Pts',(-3.77326886065484,-1.,-1.83493697935064));
#65214=CARTESIAN_POINT('Ctrl Pts',(-3.77326886065484,1.,-1.83493697935064));
#65215=CARTESIAN_POINT('Ctrl Pts',(-3.77038509819777,-1.,-1.83120816956515));
#65216=CARTESIAN_POINT('Ctrl Pts',(-3.77038509819777,1.,-1.83120816956515));
#65217=CARTESIAN_POINT('Ctrl Pts',(-3.76652740355856,-1.,-1.82625289221933));
#65218=CARTESIAN_POINT('Ctrl Pts',(-3.76652740355856,1.,-1.82625289221933));
#65219=CARTESIAN_POINT('Ctrl Pts',(-3.76168412709652,-1.,-1.82008629694924));
#65220=CARTESIAN_POINT('Ctrl Pts',(-3.76168412709652,1.,-1.82008629694924));
#65221=CARTESIAN_POINT('Ctrl Pts',(-3.75681965683995,-1.,-1.81394729834032));
#65222=CARTESIAN_POINT('Ctrl Pts',(-3.75681965683995,1.,-1.81394729834032));
#65223=CARTESIAN_POINT('Ctrl Pts',(-3.75193395888069,-1.,-1.80783603939662));
#65224=CARTESIAN_POINT('Ctrl Pts',(-3.75193395888069,1.,-1.80783603939662));
#65225=CARTESIAN_POINT('Ctrl Pts',(-3.74702700874954,-1.,-1.80175271485519));
#65226=CARTESIAN_POINT('Ctrl Pts',(-3.74702700874954,1.,-1.80175271485519));
#65227=CARTESIAN_POINT('Ctrl Pts',(-3.74209880351667,-1.,-1.79569757859041));
#65228=CARTESIAN_POINT('Ctrl Pts',(-3.74209880351667,1.,-1.79569757859041));
#65229=CARTESIAN_POINT('Ctrl Pts',(-3.73714934729962,-1.,-1.78967092823139));
#65230=CARTESIAN_POINT('Ctrl Pts',(-3.73714934729962,1.,-1.78967092823139));
#65231=CARTESIAN_POINT('Ctrl Pts',(-3.73217863095022,-1.,-1.78367308442682));
#65232=CARTESIAN_POINT('Ctrl Pts',(-3.73217863095022,1.,-1.78367308442682));
#65233=CARTESIAN_POINT('Ctrl Pts',(-3.72718661205504,-1.,-1.77770437039606));
#65234=CARTESIAN_POINT('Ctrl Pts',(-3.72718661205504,1.,-1.77770437039606));
#65235=CARTESIAN_POINT('Ctrl Pts',(-3.72217319911429,-1.,-1.77176509401846));
#65236=CARTESIAN_POINT('Ctrl Pts',(-3.72217319911429,1.,-1.77176509401846));
#65237=CARTESIAN_POINT('Ctrl Pts',(-3.71713822377675,-1.,-1.76585552124549));
#65238=CARTESIAN_POINT('Ctrl Pts',(-3.71713822377675,1.,-1.76585552124549));
#65239=CARTESIAN_POINT('Ctrl Pts',(-3.71208146346454,-1.,-1.75997588499021));
#65240=CARTESIAN_POINT('Ctrl Pts',(-3.71208146346454,1.,-1.75997588499021));
#65241=CARTESIAN_POINT('Ctrl Pts',(-3.70700269736876,-1.,-1.75412641804148));
#65242=CARTESIAN_POINT('Ctrl Pts',(-3.70700269736876,1.,-1.75412641804148));
#65243=CARTESIAN_POINT('Ctrl Pts',(-3.70190175673422,-1.,-1.74830738046092));
#65244=CARTESIAN_POINT('Ctrl Pts',(-3.70190175673422,1.,-1.74830738046092));
#65245=CARTESIAN_POINT('Ctrl Pts',(-3.6967785691046,-1.,-1.74251908492589));
#65246=CARTESIAN_POINT('Ctrl Pts',(-3.6967785691046,1.,-1.74251908492589));
#65247=CARTESIAN_POINT('Ctrl Pts',(-3.69163322647906,-1.,-1.73676193254493));
#65248=CARTESIAN_POINT('Ctrl Pts',(-3.69163322647906,1.,-1.73676193254493));
#65249=CARTESIAN_POINT('Ctrl Pts',(-3.68646597019188,-1.,-1.73103640956647));
#65250=CARTESIAN_POINT('Ctrl Pts',(-3.68646597019188,1.,-1.73103640956647));
#65251=CARTESIAN_POINT('Ctrl Pts',(-3.68127704936472,-1.,-1.72534302437003));
#65252=CARTESIAN_POINT('Ctrl Pts',(-3.68127704936472,1.,-1.72534302437003));
#65253=CARTESIAN_POINT('Ctrl Pts',(-3.67606660374665,-1.,-1.71968225581787));
#65254=CARTESIAN_POINT('Ctrl Pts',(-3.67606660374665,1.,-1.71968225581787));
#65255=CARTESIAN_POINT('Ctrl Pts',(-3.67083454901629,-1.,-1.71405450210392));
#65256=CARTESIAN_POINT('Ctrl Pts',(-3.67083454901629,1.,-1.71405450210392));
#65257=CARTESIAN_POINT('Ctrl Pts',(-3.6655804319893,-1.,-1.70846001610983));
#65258=CARTESIAN_POINT('Ctrl Pts',(-3.6655804319893,1.,-1.70846001610983));
#65259=CARTESIAN_POINT('Ctrl Pts',(-3.6603033877491,-1.,-1.70289888566904));
#65260=CARTESIAN_POINT('Ctrl Pts',(-3.6603033877491,1.,-1.70289888566904));
#65261=CARTESIAN_POINT('Ctrl Pts',(-3.65500246526798,-1.,-1.69737117722558));
#65262=CARTESIAN_POINT('Ctrl Pts',(-3.65500246526798,1.,-1.69737117722558));
#65263=CARTESIAN_POINT('Ctrl Pts',(-3.64967689827393,-1.,-1.691877054817));
#65264=CARTESIAN_POINT('Ctrl Pts',(-3.64967689827393,1.,-1.691877054817));
#65265=CARTESIAN_POINT('Ctrl Pts',(-3.64432638915199,-1.,-1.68641690471455));
#65266=CARTESIAN_POINT('Ctrl Pts',(-3.64432638915199,1.,-1.68641690471455));
#65267=CARTESIAN_POINT('Ctrl Pts',(-3.63895140887443,-1.,-1.68099146651577));
#65268=CARTESIAN_POINT('Ctrl Pts',(-3.63895140887443,1.,-1.68099146651577));
#65269=CARTESIAN_POINT('Ctrl Pts',(-3.63355343201211,-1.,-1.67560193613145));
#65270=CARTESIAN_POINT('Ctrl Pts',(-3.63355343201211,1.,-1.67560193613145));
#65271=CARTESIAN_POINT('Ctrl Pts',(-3.62813422105257,-1.,-1.67024966008037));
#65272=CARTESIAN_POINT('Ctrl Pts',(-3.62813422105257,1.,-1.67024966008037));
#65273=CARTESIAN_POINT('Ctrl Pts',(-3.62269517989104,-1.,-1.66493585923853));
#65274=CARTESIAN_POINT('Ctrl Pts',(-3.62269517989104,1.,-1.66493585923853));
#65275=CARTESIAN_POINT('Ctrl Pts',(-3.61723666482457,-1.,-1.65966133399186));
#65276=CARTESIAN_POINT('Ctrl Pts',(-3.61723666482457,1.,-1.65966133399186));
#65277=CARTESIAN_POINT('Ctrl Pts',(-3.61175734965129,-1.,-1.65442619244327));
#65278=CARTESIAN_POINT('Ctrl Pts',(-3.61175734965129,1.,-1.65442619244327));
#65279=CARTESIAN_POINT('Ctrl Pts',(-3.60625346556992,-1.,-1.64922952425833));
#65280=CARTESIAN_POINT('Ctrl Pts',(-3.60625346556992,1.,-1.64922952425833));
#65281=CARTESIAN_POINT('Ctrl Pts',(-3.6007202851384,-1.,-1.6440700438558));
#65282=CARTESIAN_POINT('Ctrl Pts',(-3.6007202851384,1.,-1.6440700438558));
#65283=CARTESIAN_POINT('Ctrl Pts',(-3.59515368334887,-1.,-1.63894676675349));
#65284=CARTESIAN_POINT('Ctrl Pts',(-3.59515368334887,1.,-1.63894676675349));
#65285=CARTESIAN_POINT('Ctrl Pts',(-3.58955176627876,-1.,-1.63385971451259));
#65286=CARTESIAN_POINT('Ctrl Pts',(-3.58955176627876,1.,-1.63385971451259));
#65287=CARTESIAN_POINT('Ctrl Pts',(-3.5839162577435,-1.,-1.62881051550748));
#65288=CARTESIAN_POINT('Ctrl Pts',(-3.5839162577435,1.,-1.62881051550748));
#65289=CARTESIAN_POINT('Ctrl Pts',(-3.57825455954405,-1.,-1.62380329464851));
#65290=CARTESIAN_POINT('Ctrl Pts',(-3.57825455954405,1.,-1.62380329464851));
#65291=CARTESIAN_POINT('Ctrl Pts',(-3.57257679609826,-1.,-1.61884340915412));
#65292=CARTESIAN_POINT('Ctrl Pts',(-3.57257679609826,1.,-1.61884340915412));
#65293=CARTESIAN_POINT('Ctrl Pts',(-3.56689200468404,-1.,-1.61393581747522));
#65294=CARTESIAN_POINT('Ctrl Pts',(-3.56689200468404,1.,-1.61393581747522));
#65295=CARTESIAN_POINT('Ctrl Pts',(-3.56120432482986,-1.,-1.60908344685459));
#65296=CARTESIAN_POINT('Ctrl Pts',(-3.56120432482986,1.,-1.60908344685459));
#65297=CARTESIAN_POINT('Ctrl Pts',(-3.55550985096117,-1.,-1.60428584699848));
#65298=CARTESIAN_POINT('Ctrl Pts',(-3.55550985096117,1.,-1.60428584699848));
#65299=CARTESIAN_POINT('Ctrl Pts',(-3.54979148634426,-1.,-1.59953698113444));
#65300=CARTESIAN_POINT('Ctrl Pts',(-3.54979148634426,1.,-1.59953698113444));
#65301=CARTESIAN_POINT('Ctrl Pts',(-3.544024581823,-1.,-1.5948276694975));
#65302=CARTESIAN_POINT('Ctrl Pts',(-3.544024581823,1.,-1.5948276694975));
#65303=CARTESIAN_POINT('Ctrl Pts',(-3.53818616861045,-1.,-1.59014958368725));
#65304=CARTESIAN_POINT('Ctrl Pts',(-3.53818616861045,1.,-1.59014958368725));
#65305=CARTESIAN_POINT('Ctrl Pts',(-3.53226378147068,-1.,-1.58549906268083));
#65306=CARTESIAN_POINT('Ctrl Pts',(-3.53226378147068,1.,-1.58549906268083));
#65307=CARTESIAN_POINT('Ctrl Pts',(-3.52626275334899,-1.,-1.58088027227856));
#65308=CARTESIAN_POINT('Ctrl Pts',(-3.52626275334899,1.,-1.58088027227856));
#65309=CARTESIAN_POINT('Ctrl Pts',(-3.52021847865961,-1.,-1.5763104998818));
#65310=CARTESIAN_POINT('Ctrl Pts',(-3.52021847865961,1.,-1.5763104998818));
#65311=CARTESIAN_POINT('Ctrl Pts',(-3.51418598431733,-1.,-1.57181569799774));
#65312=CARTESIAN_POINT('Ctrl Pts',(-3.51418598431733,1.,-1.57181569799774));
#65313=CARTESIAN_POINT('Ctrl Pts',(-3.50821771695427,-1.,-1.56742097575041));
#65314=CARTESIAN_POINT('Ctrl Pts',(-3.50821771695427,1.,-1.56742097575041));
#65315=CARTESIAN_POINT('Ctrl Pts',(-3.50234321621607,-1.,-1.56314187758689));
#65316=CARTESIAN_POINT('Ctrl Pts',(-3.50234321621607,1.,-1.56314187758689));
#65317=CARTESIAN_POINT('Ctrl Pts',(-3.49655185179623,-1.,-1.55897703097859));
#65318=CARTESIAN_POINT('Ctrl Pts',(-3.49655185179623,1.,-1.55897703097859));
#65319=CARTESIAN_POINT('Ctrl Pts',(-3.49076460877317,-1.,-1.5548959590107));
#65320=CARTESIAN_POINT('Ctrl Pts',(-3.49076460877317,1.,-1.5548959590107));
#65321=CARTESIAN_POINT('Ctrl Pts',(-3.48485155928414,-1.,-1.55084702970382));
#65322=CARTESIAN_POINT('Ctrl Pts',(-3.48485155928414,1.,-1.55084702970382));
#65323=CARTESIAN_POINT('Ctrl Pts',(-3.47868272898599,-1.,-1.54678009290206));
#65324=CARTESIAN_POINT('Ctrl Pts',(-3.47868272898599,1.,-1.54678009290206));
#65325=CARTESIAN_POINT('Ctrl Pts',(-3.47217189224576,-1.,-1.54266605398152));
#65326=CARTESIAN_POINT('Ctrl Pts',(-3.47217189224576,1.,-1.54266605398152));
#65327=CARTESIAN_POINT('Ctrl Pts',(-3.46531752207222,-1.,-1.53851507915533));
#65328=CARTESIAN_POINT('Ctrl Pts',(-3.46531752207222,1.,-1.53851507915533));
#65329=CARTESIAN_POINT('Ctrl Pts',(-3.45825932955273,-1.,-1.53440195378902));
#65330=CARTESIAN_POINT('Ctrl Pts',(-3.45825932955273,1.,-1.53440195378902));
#65331=CARTESIAN_POINT('Ctrl Pts',(-3.45127136828667,-1.,-1.530462444618));
#65332=CARTESIAN_POINT('Ctrl Pts',(-3.45127136828667,1.,-1.530462444618));
#65333=CARTESIAN_POINT('Ctrl Pts',(-3.44469547527,-1.,-1.52686242875717));
#65334=CARTESIAN_POINT('Ctrl Pts',(-3.44469547527,1.,-1.52686242875717));
#65335=CARTESIAN_POINT('Ctrl Pts',(-3.43888895974182,-1.,-1.52377348950429));
#65336=CARTESIAN_POINT('Ctrl Pts',(-3.43888895974182,1.,-1.52377348950429));
#65337=CARTESIAN_POINT('Ctrl Pts',(-3.43417156977749,-1.,-1.52134826724227));
#65338=CARTESIAN_POINT('Ctrl Pts',(-3.43417156977749,1.,-1.52134826724227));
#65339=CARTESIAN_POINT('Ctrl Pts',(-3.43076036253384,-1.,-1.51969006980792));
#65340=CARTESIAN_POINT('Ctrl Pts',(-3.43076036253384,1.,-1.51969006980792));
#65341=CARTESIAN_POINT('Ctrl Pts',(-3.42915787669388,-1.,-1.51901585838879));
#65342=CARTESIAN_POINT('Ctrl Pts',(-3.42915787669388,1.,-1.51901585838879));
#65343=CARTESIAN_POINT('Ctrl Pts',(-3.42860527148835,-1.,-1.51888450659497));
#65344=CARTESIAN_POINT('Ctrl Pts',(-3.42860527148835,1.,-1.51888450659497));
#65345=CARTESIAN_POINT('Ctrl Pts',(-3.42852521763648,-1.,-1.51896318668306));
#65346=CARTESIAN_POINT('Ctrl Pts',(-3.42852521763648,1.,-1.51896318668306));
#65347=CARTESIAN_POINT('Ctrl Pts',(-3.42855728381368,-1.,-1.519044091397));
#65348=CARTESIAN_POINT('Ctrl Pts',(-3.42855728381368,1.,-1.519044091397));
#65349=CARTESIAN_POINT('',(-3.77614523045147,1.,-1.83867539237861));
#65350=CARTESIAN_POINT('Ctrl Pts',(-3.77614523045147,1.,-1.83867539237861));
#65351=CARTESIAN_POINT('Ctrl Pts',(-3.77518714458232,1.,-1.83742834010821));
#65352=CARTESIAN_POINT('Ctrl Pts',(-3.77326886065484,1.,-1.83493697935064));
#65353=CARTESIAN_POINT('Ctrl Pts',(-3.77038509819777,1.,-1.83120816956515));
#65354=CARTESIAN_POINT('Ctrl Pts',(-3.76652740355856,1.,-1.82625289221933));
#65355=CARTESIAN_POINT('Ctrl Pts',(-3.76168412709652,1.,-1.82008629694924));
#65356=CARTESIAN_POINT('Ctrl Pts',(-3.75681965683995,1.,-1.81394729834032));
#65357=CARTESIAN_POINT('Ctrl Pts',(-3.75193395888069,1.,-1.80783603939662));
#65358=CARTESIAN_POINT('Ctrl Pts',(-3.74702700874954,1.,-1.80175271485519));
#65359=CARTESIAN_POINT('Ctrl Pts',(-3.74209880351667,1.,-1.79569757859041));
#65360=CARTESIAN_POINT('Ctrl Pts',(-3.73714934729962,1.,-1.78967092823139));
#65361=CARTESIAN_POINT('Ctrl Pts',(-3.73217863095022,1.,-1.78367308442682));
#65362=CARTESIAN_POINT('Ctrl Pts',(-3.72718661205504,1.,-1.77770437039606));
#65363=CARTESIAN_POINT('Ctrl Pts',(-3.72217319911429,1.,-1.77176509401846));
#65364=CARTESIAN_POINT('Ctrl Pts',(-3.71713822377675,1.,-1.76585552124549));
#65365=CARTESIAN_POINT('Ctrl Pts',(-3.71208146346454,1.,-1.75997588499021));
#65366=CARTESIAN_POINT('Ctrl Pts',(-3.70700269736876,1.,-1.75412641804148));
#65367=CARTESIAN_POINT('Ctrl Pts',(-3.70190175673422,1.,-1.74830738046092));
#65368=CARTESIAN_POINT('Ctrl Pts',(-3.6967785691046,1.,-1.74251908492589));
#65369=CARTESIAN_POINT('Ctrl Pts',(-3.69163322647906,1.,-1.73676193254493));
#65370=CARTESIAN_POINT('Ctrl Pts',(-3.68646597019188,1.,-1.73103640956647));
#65371=CARTESIAN_POINT('Ctrl Pts',(-3.68127704936472,1.,-1.72534302437003));
#65372=CARTESIAN_POINT('Ctrl Pts',(-3.67606660374665,1.,-1.71968225581787));
#65373=CARTESIAN_POINT('Ctrl Pts',(-3.67083454901629,1.,-1.71405450210392));
#65374=CARTESIAN_POINT('Ctrl Pts',(-3.6655804319893,1.,-1.70846001610983));
#65375=CARTESIAN_POINT('Ctrl Pts',(-3.6603033877491,1.,-1.70289888566904));
#65376=CARTESIAN_POINT('Ctrl Pts',(-3.65500246526798,1.,-1.69737117722558));
#65377=CARTESIAN_POINT('Ctrl Pts',(-3.64967689827393,1.,-1.691877054817));
#65378=CARTESIAN_POINT('Ctrl Pts',(-3.64432638915199,1.,-1.68641690471455));
#65379=CARTESIAN_POINT('Ctrl Pts',(-3.63895140887443,1.,-1.68099146651577));
#65380=CARTESIAN_POINT('Ctrl Pts',(-3.63355343201211,1.,-1.67560193613145));
#65381=CARTESIAN_POINT('Ctrl Pts',(-3.62813422105257,1.,-1.67024966008037));
#65382=CARTESIAN_POINT('Ctrl Pts',(-3.62269517989104,1.,-1.66493585923853));
#65383=CARTESIAN_POINT('Ctrl Pts',(-3.61723666482457,1.,-1.65966133399186));
#65384=CARTESIAN_POINT('Ctrl Pts',(-3.61175734965129,1.,-1.65442619244327));
#65385=CARTESIAN_POINT('Ctrl Pts',(-3.60625346556992,1.,-1.64922952425833));
#65386=CARTESIAN_POINT('Ctrl Pts',(-3.6007202851384,1.,-1.6440700438558));
#65387=CARTESIAN_POINT('Ctrl Pts',(-3.59515368334887,1.,-1.63894676675349));
#65388=CARTESIAN_POINT('Ctrl Pts',(-3.58955176627876,1.,-1.63385971451259));
#65389=CARTESIAN_POINT('Ctrl Pts',(-3.5839162577435,1.,-1.62881051550748));
#65390=CARTESIAN_POINT('Ctrl Pts',(-3.57825455954405,1.,-1.62380329464851));
#65391=CARTESIAN_POINT('Ctrl Pts',(-3.57257679609826,1.,-1.61884340915412));
#65392=CARTESIAN_POINT('Ctrl Pts',(-3.56689200468404,1.,-1.61393581747522));
#65393=CARTESIAN_POINT('Ctrl Pts',(-3.56120432482986,1.,-1.60908344685459));
#65394=CARTESIAN_POINT('Ctrl Pts',(-3.55550985096117,1.,-1.60428584699848));
#65395=CARTESIAN_POINT('Ctrl Pts',(-3.54979148634426,1.,-1.59953698113444));
#65396=CARTESIAN_POINT('Ctrl Pts',(-3.544024581823,1.,-1.5948276694975));
#65397=CARTESIAN_POINT('Ctrl Pts',(-3.53818616861045,1.,-1.59014958368725));
#65398=CARTESIAN_POINT('Ctrl Pts',(-3.53226378147068,1.,-1.58549906268083));
#65399=CARTESIAN_POINT('Ctrl Pts',(-3.52626275334899,1.,-1.58088027227856));
#65400=CARTESIAN_POINT('Ctrl Pts',(-3.52021847865961,1.,-1.5763104998818));
#65401=CARTESIAN_POINT('Ctrl Pts',(-3.51418598431733,1.,-1.57181569799774));
#65402=CARTESIAN_POINT('Ctrl Pts',(-3.50821771695427,1.,-1.56742097575041));
#65403=CARTESIAN_POINT('Ctrl Pts',(-3.50234321621607,1.,-1.56314187758689));
#65404=CARTESIAN_POINT('Ctrl Pts',(-3.49655185179623,1.,-1.55897703097859));
#65405=CARTESIAN_POINT('Ctrl Pts',(-3.49076460877317,1.,-1.5548959590107));
#65406=CARTESIAN_POINT('Ctrl Pts',(-3.48485155928414,1.,-1.55084702970382));
#65407=CARTESIAN_POINT('Ctrl Pts',(-3.47868272898599,1.,-1.54678009290206));
#65408=CARTESIAN_POINT('Ctrl Pts',(-3.47217189224576,1.,-1.54266605398152));
#65409=CARTESIAN_POINT('Ctrl Pts',(-3.46531752207222,1.,-1.53851507915533));
#65410=CARTESIAN_POINT('Ctrl Pts',(-3.45825932955273,1.,-1.53440195378902));
#65411=CARTESIAN_POINT('Ctrl Pts',(-3.45127136828667,1.,-1.530462444618));
#65412=CARTESIAN_POINT('Ctrl Pts',(-3.44469547527,1.,-1.52686242875717));
#65413=CARTESIAN_POINT('Ctrl Pts',(-3.43888895974182,1.,-1.52377348950429));
#65414=CARTESIAN_POINT('Ctrl Pts',(-3.43417156977749,1.,-1.52134826724227));
#65415=CARTESIAN_POINT('Ctrl Pts',(-3.43101631893491,1.,-1.5198144909343));
#65416=CARTESIAN_POINT('Ctrl Pts',(-3.42946838852728,1.,-1.51914806898539));
#65417=CARTESIAN_POINT('Ctrl Pts',(-3.42884302333978,1.,-1.51895133295017));
#65418=CARTESIAN_POINT('Ctrl Pts',(-3.42864616361967,1.,-1.51893924967231));
#65419=CARTESIAN_POINT('Ctrl Pts',(-3.42859860294378,1.,-1.51895082866166));
#65420=CARTESIAN_POINT('',(-3.77614523045147,0.,-1.83867539237861));
#65421=CARTESIAN_POINT('Ctrl Pts',(-3.24418789321065,-1.,-1.8808893942881));
#65422=CARTESIAN_POINT('Ctrl Pts',(-3.24418789321065,1.,-1.8808893942881));
#65423=CARTESIAN_POINT('Ctrl Pts',(-3.24410359189733,-1.,-1.8809110068042));
#65424=CARTESIAN_POINT('Ctrl Pts',(-3.24410359189733,1.,-1.8809110068042));
#65425=CARTESIAN_POINT('Ctrl Pts',(-3.24408699284449,-1.,-1.8810220187274));
#65426=CARTESIAN_POINT('Ctrl Pts',(-3.24408699284449,1.,-1.8810220187274));
#65427=CARTESIAN_POINT('Ctrl Pts',(-3.24451807186964,-1.,-1.88139187908347));
#65428=CARTESIAN_POINT('Ctrl Pts',(-3.24451807186964,1.,-1.88139187908347));
#65429=CARTESIAN_POINT('Ctrl Pts',(-3.24600543790876,-1.,-1.88229202583187));
#65430=CARTESIAN_POINT('Ctrl Pts',(-3.24600543790876,1.,-1.88229202583187));
#65431=CARTESIAN_POINT('Ctrl Pts',(-3.24935200512055,-1.,-1.88407708646435));
#65432=CARTESIAN_POINT('Ctrl Pts',(-3.24935200512055,1.,-1.88407708646435));
#65433=CARTESIAN_POINT('Ctrl Pts',(-3.25408686339298,-1.,-1.88646802523372));
#65434=CARTESIAN_POINT('Ctrl Pts',(-3.25408686339298,1.,-1.88646802523372));
#65435=CARTESIAN_POINT('Ctrl Pts',(-3.2599988519361,-1.,-1.88934996203508));
#65436=CARTESIAN_POINT('Ctrl Pts',(-3.2599988519361,1.,-1.88934996203508));
#65437=CARTESIAN_POINT('Ctrl Pts',(-3.2667765388833,-1.,-1.89255393500769));
#65438=CARTESIAN_POINT('Ctrl Pts',(-3.2667765388833,1.,-1.89255393500769));
#65439=CARTESIAN_POINT('Ctrl Pts',(-3.27407108932908,-1.,-1.89589172903662));
#65440=CARTESIAN_POINT('Ctrl Pts',(-3.27407108932908,1.,-1.89589172903662));
#65441=CARTESIAN_POINT('Ctrl Pts',(-3.28154737912287,-1.,-1.89918429230424));
#65442=CARTESIAN_POINT('Ctrl Pts',(-3.28154737912287,1.,-1.89918429230424));
#65443=CARTESIAN_POINT('Ctrl Pts',(-3.28893448600364,-1.,-1.9022897124757));
#65444=CARTESIAN_POINT('Ctrl Pts',(-3.28893448600364,1.,-1.9022897124757));
#65445=CARTESIAN_POINT('Ctrl Pts',(-3.29608978722258,-1.,-1.9051389186417));
#65446=CARTESIAN_POINT('Ctrl Pts',(-3.29608978722258,1.,-1.9051389186417));
#65447=CARTESIAN_POINT('Ctrl Pts',(-3.30300595568341,-1.,-1.90773912171424));
#65448=CARTESIAN_POINT('Ctrl Pts',(-3.30300595568341,1.,-1.90773912171424));
#65449=CARTESIAN_POINT('Ctrl Pts',(-3.30975721158694,-1.,-1.91014297830502));
#65450=CARTESIAN_POINT('Ctrl Pts',(-3.30975721158694,1.,-1.91014297830502));
#65451=CARTESIAN_POINT('Ctrl Pts',(-3.31646052426395,-1.,-1.91242616234459));
#65452=CARTESIAN_POINT('Ctrl Pts',(-3.31646052426395,1.,-1.91242616234459));
#65453=CARTESIAN_POINT('Ctrl Pts',(-3.32323403454507,-1.,-1.91466343916612));
#65454=CARTESIAN_POINT('Ctrl Pts',(-3.32323403454507,1.,-1.91466343916612));
#65455=CARTESIAN_POINT('Ctrl Pts',(-3.33014884257812,-1.,-1.91690081930297));
#65456=CARTESIAN_POINT('Ctrl Pts',(-3.33014884257812,1.,-1.91690081930297));
#65457=CARTESIAN_POINT('Ctrl Pts',(-3.33721230709948,-1.,-1.91914609610173));
#65458=CARTESIAN_POINT('Ctrl Pts',(-3.33721230709948,1.,-1.91914609610173));
#65459=CARTESIAN_POINT('Ctrl Pts',(-3.34439448941915,-1.,-1.92138450828378));
#65460=CARTESIAN_POINT('Ctrl Pts',(-3.34439448941915,1.,-1.92138450828378));
#65461=CARTESIAN_POINT('Ctrl Pts',(-3.35164424847206,-1.,-1.92358838440518));
#65462=CARTESIAN_POINT('Ctrl Pts',(-3.35164424847206,1.,-1.92358838440518));
#65463=CARTESIAN_POINT('Ctrl Pts',(-3.35890824422976,-1.,-1.92572846125763));
#65464=CARTESIAN_POINT('Ctrl Pts',(-3.35890824422976,1.,-1.92572846125763));
#65465=CARTESIAN_POINT('Ctrl Pts',(-3.36615168657597,-1.,-1.92778626543803));
#65466=CARTESIAN_POINT('Ctrl Pts',(-3.36615168657597,1.,-1.92778626543803));
#65467=CARTESIAN_POINT('Ctrl Pts',(-3.37336807068078,-1.,-1.92975993109897));
#65468=CARTESIAN_POINT('Ctrl Pts',(-3.37336807068078,1.,-1.92975993109897));
#65469=CARTESIAN_POINT('Ctrl Pts',(-3.38056768525577,-1.,-1.93165739093292));
#65470=CARTESIAN_POINT('Ctrl Pts',(-3.38056768525577,1.,-1.93165739093292));
#65471=CARTESIAN_POINT('Ctrl Pts',(-3.38777076883267,-1.,-1.93349233176794));
#65472=CARTESIAN_POINT('Ctrl Pts',(-3.38777076883267,1.,-1.93349233176794));
#65473=CARTESIAN_POINT('Ctrl Pts',(-3.39499923640789,-1.,-1.93527929945982));
#65474=CARTESIAN_POINT('Ctrl Pts',(-3.39499923640789,1.,-1.93527929945982));
#65475=CARTESIAN_POINT('Ctrl Pts',(-3.40226802104093,-1.,-1.93702857723089));
#65476=CARTESIAN_POINT('Ctrl Pts',(-3.40226802104093,1.,-1.93702857723089));
#65477=CARTESIAN_POINT('Ctrl Pts',(-3.40957978266622,-1.,-1.93874306008132));
#65478=CARTESIAN_POINT('Ctrl Pts',(-3.40957978266622,1.,-1.93874306008132));
#65479=CARTESIAN_POINT('Ctrl Pts',(-3.41692971994082,-1.,-1.94042111965237));
#65480=CARTESIAN_POINT('Ctrl Pts',(-3.41692971994082,1.,-1.94042111965237));
#65481=CARTESIAN_POINT('Ctrl Pts',(-3.42430850941497,-1.,-1.94205835913692));
#65482=CARTESIAN_POINT('Ctrl Pts',(-3.42430850941497,1.,-1.94205835913692));
#65483=CARTESIAN_POINT('Ctrl Pts',(-3.43170586602436,-1.,-1.94364973660285));
#65484=CARTESIAN_POINT('Ctrl Pts',(-3.43170586602436,1.,-1.94364973660285));
#65485=CARTESIAN_POINT('Ctrl Pts',(-3.43911410197693,-1.,-1.94519168842883));
#65486=CARTESIAN_POINT('Ctrl Pts',(-3.43911410197693,1.,-1.94519168842883));
#65487=CARTESIAN_POINT('Ctrl Pts',(-3.44653088665685,-1.,-1.94668377715332));
#65488=CARTESIAN_POINT('Ctrl Pts',(-3.44653088665685,1.,-1.94668377715332));
#65489=CARTESIAN_POINT('Ctrl Pts',(-3.45395731584051,-1.,-1.94812754766524));
#65490=CARTESIAN_POINT('Ctrl Pts',(-3.45395731584051,1.,-1.94812754766524));
#65491=CARTESIAN_POINT('Ctrl Pts',(-3.46139661060959,-1.,-1.94952575850196));
#65492=CARTESIAN_POINT('Ctrl Pts',(-3.46139661060959,1.,-1.94952575850196));
#65493=CARTESIAN_POINT('Ctrl Pts',(-3.4688525897419,-1.,-1.95088147859876));
#65494=CARTESIAN_POINT('Ctrl Pts',(-3.4688525897419,1.,-1.95088147859876));
#65495=CARTESIAN_POINT('Ctrl Pts',(-3.47632820495926,-1.,-1.95219722189878));
#65496=CARTESIAN_POINT('Ctrl Pts',(-3.47632820495926,1.,-1.95219722189878));
#65497=CARTESIAN_POINT('Ctrl Pts',(-3.48382414832648,-1.,-1.95347412486316));
#65498=CARTESIAN_POINT('Ctrl Pts',(-3.48382414832648,1.,-1.95347412486316));
#65499=CARTESIAN_POINT('Ctrl Pts',(-3.49133956289154,-1.,-1.95471236969653));
#65500=CARTESIAN_POINT('Ctrl Pts',(-3.49133956289154,1.,-1.95471236969653));
#65501=CARTESIAN_POINT('Ctrl Pts',(-3.49887263575602,-1.,-1.9559115382367));
#65502=CARTESIAN_POINT('Ctrl Pts',(-3.49887263575602,1.,-1.9559115382367));
#65503=CARTESIAN_POINT('Ctrl Pts',(-3.50642124159913,-1.,-1.95707099606513));
#65504=CARTESIAN_POINT('Ctrl Pts',(-3.50642124159913,1.,-1.95707099606513));
#65505=CARTESIAN_POINT('Ctrl Pts',(-3.51398354617772,-1.,-1.95819025316768));
#65506=CARTESIAN_POINT('Ctrl Pts',(-3.51398354617772,1.,-1.95819025316768));
#65507=CARTESIAN_POINT('Ctrl Pts',(-3.52155867431438,-1.,-1.95926936324436));
#65508=CARTESIAN_POINT('Ctrl Pts',(-3.52155867431438,1.,-1.95926936324436));
#65509=CARTESIAN_POINT('Ctrl Pts',(-3.52914648844289,-1.,-1.96030879411534));
#65510=CARTESIAN_POINT('Ctrl Pts',(-3.52914648844289,1.,-1.96030879411534));
#65511=CARTESIAN_POINT('Ctrl Pts',(-3.53674730625759,-1.,-1.96130926212661));
#65512=CARTESIAN_POINT('Ctrl Pts',(-3.53674730625759,1.,-1.96130926212661));
#65513=CARTESIAN_POINT('Ctrl Pts',(-3.54436163300425,-1.,-1.96227157573058));
#65514=CARTESIAN_POINT('Ctrl Pts',(-3.54436163300425,1.,-1.96227157573058));
#65515=CARTESIAN_POINT('Ctrl Pts',(-3.55198990600929,-1.,-1.96319648628667));
#65516=CARTESIAN_POINT('Ctrl Pts',(-3.55198990600929,1.,-1.96319648628667));
#65517=CARTESIAN_POINT('Ctrl Pts',(-3.55963218706201,-1.,-1.96408450906868));
#65518=CARTESIAN_POINT('Ctrl Pts',(-3.55963218706201,1.,-1.96408450906868));
#65519=CARTESIAN_POINT('Ctrl Pts',(-3.56728820357933,-1.,-1.96493594634643));
#65520=CARTESIAN_POINT('Ctrl Pts',(-3.56728820357933,1.,-1.96493594634643));
#65521=CARTESIAN_POINT('Ctrl Pts',(-3.57495748601088,-1.,-1.96575096652857));
#65522=CARTESIAN_POINT('Ctrl Pts',(-3.57495748601088,1.,-1.96575096652857));
#65523=CARTESIAN_POINT('Ctrl Pts',(-3.58263947663884,-1.,-1.9665296668894));
#65524=CARTESIAN_POINT('Ctrl Pts',(-3.58263947663884,1.,-1.9665296668894));
#65525=CARTESIAN_POINT('Ctrl Pts',(-3.5903336402273,-1.,-1.96727213799507));
#65526=CARTESIAN_POINT('Ctrl Pts',(-3.5903336402273,1.,-1.96727213799507));
#65527=CARTESIAN_POINT('Ctrl Pts',(-3.59803959819725,-1.,-1.96797854118257));
#65528=CARTESIAN_POINT('Ctrl Pts',(-3.59803959819725,1.,-1.96797854118257));
#65529=CARTESIAN_POINT('Ctrl Pts',(-3.60575714017676,-1.,-1.96864911885775));
#65530=CARTESIAN_POINT('Ctrl Pts',(-3.60575714017676,1.,-1.96864911885775));
#65531=CARTESIAN_POINT('Ctrl Pts',(-3.61348615496393,-1.,-1.96928416040712));
#65532=CARTESIAN_POINT('Ctrl Pts',(-3.61348615496393,1.,-1.96928416040712));
#65533=CARTESIAN_POINT('Ctrl Pts',(-3.62122658401722,-1.,-1.96988398129888));
#65534=CARTESIAN_POINT('Ctrl Pts',(-3.62122658401722,1.,-1.96988398129888));
#65535=CARTESIAN_POINT('Ctrl Pts',(-3.62897836973397,-1.,-1.97044889850518));
#65536=CARTESIAN_POINT('Ctrl Pts',(-3.62897836973397,1.,-1.97044889850518));
#65537=CARTESIAN_POINT('Ctrl Pts',(-3.63674139590853,-1.,-1.97097920454698));
#65538=CARTESIAN_POINT('Ctrl Pts',(-3.63674139590853,1.,-1.97097920454698));
#65539=CARTESIAN_POINT('Ctrl Pts',(-3.64451546724221,-1.,-1.97147515441539));
#65540=CARTESIAN_POINT('Ctrl Pts',(-3.64451546724221,1.,-1.97147515441539));
#65541=CARTESIAN_POINT('Ctrl Pts',(-3.65230034717364,-1.,-1.97193697240645));
#65542=CARTESIAN_POINT('Ctrl Pts',(-3.65230034717364,1.,-1.97193697240645));
#65543=CARTESIAN_POINT('Ctrl Pts',(-3.66009578166865,-1.,-1.97236485439317));
#65544=CARTESIAN_POINT('Ctrl Pts',(-3.66009578166865,1.,-1.97236485439317));
#65545=CARTESIAN_POINT('Ctrl Pts',(-3.66790152751984,-1.,-1.9727589719863));
#65546=CARTESIAN_POINT('Ctrl Pts',(-3.66790152751984,1.,-1.9727589719863));
#65547=CARTESIAN_POINT('Ctrl Pts',(-3.67571738106175,-1.,-1.97311947678035));
#65548=CARTESIAN_POINT('Ctrl Pts',(-3.67571738106175,1.,-1.97311947678035));
#65549=CARTESIAN_POINT('Ctrl Pts',(-3.68354319913416,-1.,-1.9734465030363));
#65550=CARTESIAN_POINT('Ctrl Pts',(-3.68354319913416,1.,-1.9734465030363));
#65551=CARTESIAN_POINT('Ctrl Pts',(-3.69137888597855,-1.,-1.97374016224397));
#65552=CARTESIAN_POINT('Ctrl Pts',(-3.69137888597855,1.,-1.97374016224397));
#65553=CARTESIAN_POINT('Ctrl Pts',(-3.69765528558292,-1.,-1.97394846382288));
#65554=CARTESIAN_POINT('Ctrl Pts',(-3.69765528558292,1.,-1.97394846382288));
#65555=CARTESIAN_POINT('Ctrl Pts',(-3.70236698911837,-1.,-1.97408973726149));
#65556=CARTESIAN_POINT('Ctrl Pts',(-3.70236698911837,1.,-1.97408973726149));
#65557=CARTESIAN_POINT('Ctrl Pts',(-3.7055100813194,-1.,-1.974177276451));
#65558=CARTESIAN_POINT('Ctrl Pts',(-3.7055100813194,1.,-1.974177276451));
#65559=CARTESIAN_POINT('Ctrl Pts',(-3.70708211654725,-1.,-1.97421938526992));
#65560=CARTESIAN_POINT('Ctrl Pts',(-3.70708211654725,1.,-1.97421938526992));
#65561=CARTESIAN_POINT('',(-3.24413672884902,1.,-1.88097764062542));
#65562=CARTESIAN_POINT('Ctrl Pts',(-3.24413672884902,-1.,-1.88097764062542));
#65563=CARTESIAN_POINT('Ctrl Pts',(-3.24413672884902,-0.666666666666667,
-1.88097764062542));
#65564=CARTESIAN_POINT('Ctrl Pts',(-3.24413672884902,-0.333333333333333,
-1.88097764062542));
#65565=CARTESIAN_POINT('Ctrl Pts',(-3.24413672884902,0.333333333333333,
-1.88097764062542));
#65566=CARTESIAN_POINT('Ctrl Pts',(-3.24413672884902,0.666666666666667,
-1.88097764062542));
#65567=CARTESIAN_POINT('Ctrl Pts',(-3.24413672884902,1.,-1.88097764062542));
#65568=CARTESIAN_POINT('',(-3.70708211654725,1.,-1.97421938526992));
#65569=CARTESIAN_POINT('',(-3.70708211654725,0.,-1.97421938526992));
#65570=CARTESIAN_POINT('Ctrl Pts',(-3.24413672884902,1.,-1.88097764062542));
#65571=CARTESIAN_POINT('Ctrl Pts',(-3.24415531671311,1.,-1.88102292397987));
#65572=CARTESIAN_POINT('Ctrl Pts',(-3.24428080352952,1.,-1.88117508446657));
#65573=CARTESIAN_POINT('Ctrl Pts',(-3.24480754675942,1.,-1.88156537699118));
#65574=CARTESIAN_POINT('Ctrl Pts',(-3.24625654410705,1.,-1.88242596600422));
#65575=CARTESIAN_POINT('Ctrl Pts',(-3.24935200512055,1.,-1.88407708646435));
#65576=CARTESIAN_POINT('Ctrl Pts',(-3.25408686339298,1.,-1.88646802523372));
#65577=CARTESIAN_POINT('Ctrl Pts',(-3.2599988519361,1.,-1.88934996203508));
#65578=CARTESIAN_POINT('Ctrl Pts',(-3.2667765388833,1.,-1.89255393500769));
#65579=CARTESIAN_POINT('Ctrl Pts',(-3.27407108932908,1.,-1.89589172903662));
#65580=CARTESIAN_POINT('Ctrl Pts',(-3.28154737912287,1.,-1.89918429230424));
#65581=CARTESIAN_POINT('Ctrl Pts',(-3.28893448600364,1.,-1.9022897124757));
#65582=CARTESIAN_POINT('Ctrl Pts',(-3.29608978722258,1.,-1.9051389186417));
#65583=CARTESIAN_POINT('Ctrl Pts',(-3.30300595568341,1.,-1.90773912171424));
#65584=CARTESIAN_POINT('Ctrl Pts',(-3.30975721158694,1.,-1.91014297830502));
#65585=CARTESIAN_POINT('Ctrl Pts',(-3.31646052426395,1.,-1.91242616234459));
#65586=CARTESIAN_POINT('Ctrl Pts',(-3.32323403454507,1.,-1.91466343916612));
#65587=CARTESIAN_POINT('Ctrl Pts',(-3.33014884257812,1.,-1.91690081930297));
#65588=CARTESIAN_POINT('Ctrl Pts',(-3.33721230709948,1.,-1.91914609610173));
#65589=CARTESIAN_POINT('Ctrl Pts',(-3.34439448941915,1.,-1.92138450828378));
#65590=CARTESIAN_POINT('Ctrl Pts',(-3.35164424847206,1.,-1.92358838440518));
#65591=CARTESIAN_POINT('Ctrl Pts',(-3.35890824422976,1.,-1.92572846125763));
#65592=CARTESIAN_POINT('Ctrl Pts',(-3.36615168657597,1.,-1.92778626543803));
#65593=CARTESIAN_POINT('Ctrl Pts',(-3.37336807068078,1.,-1.92975993109897));
#65594=CARTESIAN_POINT('Ctrl Pts',(-3.38056768525577,1.,-1.93165739093292));
#65595=CARTESIAN_POINT('Ctrl Pts',(-3.38777076883267,1.,-1.93349233176794));
#65596=CARTESIAN_POINT('Ctrl Pts',(-3.39499923640789,1.,-1.93527929945982));
#65597=CARTESIAN_POINT('Ctrl Pts',(-3.40226802104093,1.,-1.93702857723089));
#65598=CARTESIAN_POINT('Ctrl Pts',(-3.40957978266622,1.,-1.93874306008132));
#65599=CARTESIAN_POINT('Ctrl Pts',(-3.41692971994082,1.,-1.94042111965237));
#65600=CARTESIAN_POINT('Ctrl Pts',(-3.42430850941497,1.,-1.94205835913692));
#65601=CARTESIAN_POINT('Ctrl Pts',(-3.43170586602436,1.,-1.94364973660285));
#65602=CARTESIAN_POINT('Ctrl Pts',(-3.43911410197693,1.,-1.94519168842883));
#65603=CARTESIAN_POINT('Ctrl Pts',(-3.44653088665685,1.,-1.94668377715332));
#65604=CARTESIAN_POINT('Ctrl Pts',(-3.45395731584051,1.,-1.94812754766524));
#65605=CARTESIAN_POINT('Ctrl Pts',(-3.46139661060959,1.,-1.94952575850196));
#65606=CARTESIAN_POINT('Ctrl Pts',(-3.4688525897419,1.,-1.95088147859876));
#65607=CARTESIAN_POINT('Ctrl Pts',(-3.47632820495926,1.,-1.95219722189878));
#65608=CARTESIAN_POINT('Ctrl Pts',(-3.48382414832648,1.,-1.95347412486316));
#65609=CARTESIAN_POINT('Ctrl Pts',(-3.49133956289154,1.,-1.95471236969653));
#65610=CARTESIAN_POINT('Ctrl Pts',(-3.49887263575602,1.,-1.9559115382367));
#65611=CARTESIAN_POINT('Ctrl Pts',(-3.50642124159913,1.,-1.95707099606513));
#65612=CARTESIAN_POINT('Ctrl Pts',(-3.51398354617772,1.,-1.95819025316768));
#65613=CARTESIAN_POINT('Ctrl Pts',(-3.52155867431438,1.,-1.95926936324436));
#65614=CARTESIAN_POINT('Ctrl Pts',(-3.52914648844289,1.,-1.96030879411534));
#65615=CARTESIAN_POINT('Ctrl Pts',(-3.53674730625759,1.,-1.96130926212661));
#65616=CARTESIAN_POINT('Ctrl Pts',(-3.54436163300425,1.,-1.96227157573058));
#65617=CARTESIAN_POINT('Ctrl Pts',(-3.55198990600929,1.,-1.96319648628667));
#65618=CARTESIAN_POINT('Ctrl Pts',(-3.55963218706201,1.,-1.96408450906868));
#65619=CARTESIAN_POINT('Ctrl Pts',(-3.56728820357933,1.,-1.96493594634643));
#65620=CARTESIAN_POINT('Ctrl Pts',(-3.57495748601088,1.,-1.96575096652857));
#65621=CARTESIAN_POINT('Ctrl Pts',(-3.58263947663884,1.,-1.9665296668894));
#65622=CARTESIAN_POINT('Ctrl Pts',(-3.5903336402273,1.,-1.96727213799507));
#65623=CARTESIAN_POINT('Ctrl Pts',(-3.59803959819725,1.,-1.96797854118257));
#65624=CARTESIAN_POINT('Ctrl Pts',(-3.60575714017676,1.,-1.96864911885775));
#65625=CARTESIAN_POINT('Ctrl Pts',(-3.61348615496393,1.,-1.96928416040712));
#65626=CARTESIAN_POINT('Ctrl Pts',(-3.62122658401722,1.,-1.96988398129888));
#65627=CARTESIAN_POINT('Ctrl Pts',(-3.62897836973397,1.,-1.97044889850518));
#65628=CARTESIAN_POINT('Ctrl Pts',(-3.63674139590853,1.,-1.97097920454698));
#65629=CARTESIAN_POINT('Ctrl Pts',(-3.64451546724221,1.,-1.97147515441539));
#65630=CARTESIAN_POINT('Ctrl Pts',(-3.65230034717364,1.,-1.97193697240645));
#65631=CARTESIAN_POINT('Ctrl Pts',(-3.66009578166865,1.,-1.97236485439317));
#65632=CARTESIAN_POINT('Ctrl Pts',(-3.66790152751984,1.,-1.9727589719863));
#65633=CARTESIAN_POINT('Ctrl Pts',(-3.67571738106175,1.,-1.97311947678035));
#65634=CARTESIAN_POINT('Ctrl Pts',(-3.68354319913416,1.,-1.9734465030363));
#65635=CARTESIAN_POINT('Ctrl Pts',(-3.69137888597855,1.,-1.97374016224397));
#65636=CARTESIAN_POINT('Ctrl Pts',(-3.69765528558292,1.,-1.97394846382288));
#65637=CARTESIAN_POINT('Ctrl Pts',(-3.70236698911837,1.,-1.97408973726149));
#65638=CARTESIAN_POINT('Ctrl Pts',(-3.7055100813194,1.,-1.974177276451));
#65639=CARTESIAN_POINT('Ctrl Pts',(-3.70708211654725,1.,-1.97421938526992));
#65640=CARTESIAN_POINT('Origin',(-3.70708211654725,0.,-1.97421938526992));
#65641=CARTESIAN_POINT('',(-3.77614523045147,1.,-1.83867539237861));
#65642=CARTESIAN_POINT('Origin',(0.,0.,0.));
#65643=CARTESIAN_POINT('',(-3.14877060440425,1.,-2.03660101169564));
#65644=CARTESIAN_POINT('Origin',(0.,1.,0.));
#65645=CARTESIAN_POINT('Ctrl Pts',(-3.14877060440425,1.,-2.03660101169564));
#65646=CARTESIAN_POINT('Ctrl Pts',(-3.14877060440425,0.666666666666667,
-2.03660101169564));
#65647=CARTESIAN_POINT('Ctrl Pts',(-3.14877060440425,0.333333333333333,
-2.03660101169564));
#65648=CARTESIAN_POINT('Ctrl Pts',(-3.14877060440425,-0.333333333333333,
-2.03660101169564));
#65649=CARTESIAN_POINT('Ctrl Pts',(-3.14877060440425,-0.666666666666667,
-2.03660101169564));
#65650=CARTESIAN_POINT('Ctrl Pts',(-3.14877060440425,-1.,-2.03660101169564));
#65651=CARTESIAN_POINT('Ctrl Pts',(-3.44202241512147,-1.,-2.40675750623143));
#65652=CARTESIAN_POINT('Ctrl Pts',(-3.44202241512147,1.,-2.40675750623143));
#65653=CARTESIAN_POINT('Ctrl Pts',(-3.44127120683402,-1.,-2.40537592959345));
#65654=CARTESIAN_POINT('Ctrl Pts',(-3.44127120683402,1.,-2.40537592959345));
#65655=CARTESIAN_POINT('Ctrl Pts',(-3.43976627485223,-1.,-2.40261515590099));
#65656=CARTESIAN_POINT('Ctrl Pts',(-3.43976627485223,1.,-2.40261515590099));
#65657=CARTESIAN_POINT('Ctrl Pts',(-3.43750133066036,-1.,-2.39848113411429));
#65658=CARTESIAN_POINT('Ctrl Pts',(-3.43750133066036,1.,-2.39848113411429));
#65659=CARTESIAN_POINT('Ctrl Pts',(-3.43446630680436,-1.,-2.39298338805823));
#65660=CARTESIAN_POINT('Ctrl Pts',(-3.43446630680436,1.,-2.39298338805823));
#65661=CARTESIAN_POINT('Ctrl Pts',(-3.43064732714472,-1.,-2.38613505844641));
#65662=CARTESIAN_POINT('Ctrl Pts',(-3.43064732714472,1.,-2.38613505844641));
#65663=CARTESIAN_POINT('Ctrl Pts',(-3.42680309755241,-1.,-2.37931067029517));
#65664=CARTESIAN_POINT('Ctrl Pts',(-3.42680309755241,1.,-2.37931067029517));
#65665=CARTESIAN_POINT('Ctrl Pts',(-3.42293356216595,-1.,-2.37251035954351));
#65666=CARTESIAN_POINT('Ctrl Pts',(-3.42293356216595,1.,-2.37251035954351));
#65667=CARTESIAN_POINT('Ctrl Pts',(-3.41903866635384,-1.,-2.36573431470314));
#65668=CARTESIAN_POINT('Ctrl Pts',(-3.41903866635384,1.,-2.36573431470314));
#65669=CARTESIAN_POINT('Ctrl Pts',(-3.4151183675076,-1.,-2.35898278606449));
#65670=CARTESIAN_POINT('Ctrl Pts',(-3.4151183675076,1.,-2.35898278606449));
#65671=CARTESIAN_POINT('Ctrl Pts',(-3.41117262313464,-1.,-2.35225606823649));
#65672=CARTESIAN_POINT('Ctrl Pts',(-3.41117262313464,1.,-2.35225606823649));
#65673=CARTESIAN_POINT('Ctrl Pts',(-3.40720137403888,-1.,-2.34555447648901));
#65674=CARTESIAN_POINT('Ctrl Pts',(-3.40720137403888,1.,-2.34555447648901));
#65675=CARTESIAN_POINT('Ctrl Pts',(-3.40320452776646,-1.,-2.33887832342715));
#65676=CARTESIAN_POINT('Ctrl Pts',(-3.40320452776646,1.,-2.33887832342715));
#65677=CARTESIAN_POINT('Ctrl Pts',(-3.39918194578115,-1.,-2.33222789882601));
#65678=CARTESIAN_POINT('Ctrl Pts',(-3.39918194578115,1.,-2.33222789882601));
#65679=CARTESIAN_POINT('Ctrl Pts',(-3.39513342020045,-1.,-2.32560343902683));
#65680=CARTESIAN_POINT('Ctrl Pts',(-3.39513342020045,1.,-2.32560343902683));
#65681=CARTESIAN_POINT('Ctrl Pts',(-3.39105869475112,-1.,-2.31900513925627));
#65682=CARTESIAN_POINT('Ctrl Pts',(-3.39105869475112,1.,-2.31900513925627));
#65683=CARTESIAN_POINT('Ctrl Pts',(-3.38695751492659,-1.,-2.31243319489505));
#65684=CARTESIAN_POINT('Ctrl Pts',(-3.38695751492659,1.,-2.31243319489505));
#65685=CARTESIAN_POINT('Ctrl Pts',(-3.38282967336676,-1.,-2.30588783640389));
#65686=CARTESIAN_POINT('Ctrl Pts',(-3.38282967336676,1.,-2.30588783640389));
#65687=CARTESIAN_POINT('Ctrl Pts',(-3.37867504959382,-1.,-2.29936936127588));
#65688=CARTESIAN_POINT('Ctrl Pts',(-3.37867504959382,1.,-2.29936936127588));
#65689=CARTESIAN_POINT('Ctrl Pts',(-3.37449367172707,-1.,-2.2928781800731));
#65690=CARTESIAN_POINT('Ctrl Pts',(-3.37449367172707,1.,-2.2928781800731));
#65691=CARTESIAN_POINT('Ctrl Pts',(-3.37028570206357,-1.,-2.28641481081045));
#65692=CARTESIAN_POINT('Ctrl Pts',(-3.37028570206357,1.,-2.28641481081045));
#65693=CARTESIAN_POINT('Ctrl Pts',(-3.36605130712978,-1.,-2.27997979457968));
#65694=CARTESIAN_POINT('Ctrl Pts',(-3.36605130712978,1.,-2.27997979457968));
#65695=CARTESIAN_POINT('Ctrl Pts',(-3.36179055004369,-1.,-2.27357362620902));
#65696=CARTESIAN_POINT('Ctrl Pts',(-3.36179055004369,1.,-2.27357362620902));
#65697=CARTESIAN_POINT('Ctrl Pts',(-3.35750328523077,-1.,-2.26719668579921));
#65698=CARTESIAN_POINT('Ctrl Pts',(-3.35750328523077,1.,-2.26719668579921));
#65699=CARTESIAN_POINT('Ctrl Pts',(-3.35318902552676,-1.,-2.26084915222484));
#65700=CARTESIAN_POINT('Ctrl Pts',(-3.35318902552676,1.,-2.26084915222484));
#65701=CARTESIAN_POINT('Ctrl Pts',(-3.34884690292342,-1.,-2.25453097693524));
#65702=CARTESIAN_POINT('Ctrl Pts',(-3.34884690292342,1.,-2.25453097693524));
#65703=CARTESIAN_POINT('Ctrl Pts',(-3.34447596770768,-1.,-2.24824207678288));
#65704=CARTESIAN_POINT('Ctrl Pts',(-3.34447596770768,1.,-2.24824207678288));
#65705=CARTESIAN_POINT('Ctrl Pts',(-3.34007543738044,-1.,-2.24198249391437));
#65706=CARTESIAN_POINT('Ctrl Pts',(-3.34007543738044,1.,-2.24198249391437));
#65707=CARTESIAN_POINT('Ctrl Pts',(-3.33564495756478,-1.,-2.2357525632881));
#65708=CARTESIAN_POINT('Ctrl Pts',(-3.33564495756478,1.,-2.2357525632881));
#65709=CARTESIAN_POINT('Ctrl Pts',(-3.33118487773593,-1.,-2.22955308907221));
#65710=CARTESIAN_POINT('Ctrl Pts',(-3.33118487773593,1.,-2.22955308907221));
#65711=CARTESIAN_POINT('Ctrl Pts',(-3.32669646722871,-1.,-2.22338548312758));
#65712=CARTESIAN_POINT('Ctrl Pts',(-3.32669646722871,1.,-2.22338548312758));
#65713=CARTESIAN_POINT('Ctrl Pts',(-3.32218125618955,-1.,-2.21725135110889));
#65714=CARTESIAN_POINT('Ctrl Pts',(-3.32218125618955,1.,-2.21725135110889));
#65715=CARTESIAN_POINT('Ctrl Pts',(-3.31764044024231,-1.,-2.21115211847872));
#65716=CARTESIAN_POINT('Ctrl Pts',(-3.31764044024231,1.,-2.21115211847872));
#65717=CARTESIAN_POINT('Ctrl Pts',(-3.3130742460895,-1.,-2.20508863150608));
#65718=CARTESIAN_POINT('Ctrl Pts',(-3.3130742460895,1.,-2.20508863150608));
#65719=CARTESIAN_POINT('Ctrl Pts',(-3.30848134694596,-1.,-2.19906078949924));
#65720=CARTESIAN_POINT('Ctrl Pts',(-3.30848134694596,1.,-2.19906078949924));
#65721=CARTESIAN_POINT('Ctrl Pts',(-3.30385816281831,-1.,-2.19306710376112));
#65722=CARTESIAN_POINT('Ctrl Pts',(-3.30385816281831,1.,-2.19306710376112));
#65723=CARTESIAN_POINT('Ctrl Pts',(-3.29920022557635,-1.,-2.18710556500325));
#65724=CARTESIAN_POINT('Ctrl Pts',(-3.29920022557635,1.,-2.18710556500325));
#65725=CARTESIAN_POINT('Ctrl Pts',(-3.29450361500484,-1.,-2.18117455557062));
#65726=CARTESIAN_POINT('Ctrl Pts',(-3.29450361500484,1.,-2.18117455557062));
#65727=CARTESIAN_POINT('Ctrl Pts',(-3.28976645712566,-1.,-2.17527380048422));
#65728=CARTESIAN_POINT('Ctrl Pts',(-3.28976645712566,1.,-2.17527380048422));
#65729=CARTESIAN_POINT('Ctrl Pts',(-3.2849901997973,-1.,-2.16940517773459));
#65730=CARTESIAN_POINT('Ctrl Pts',(-3.2849901997973,1.,-2.16940517773459));
#65731=CARTESIAN_POINT('Ctrl Pts',(-3.28018150841414,-1.,-2.16357391934434));
#65732=CARTESIAN_POINT('Ctrl Pts',(-3.28018150841414,1.,-2.16357391934434));
#65733=CARTESIAN_POINT('Ctrl Pts',(-3.27534954469206,-1.,-2.15778690038359));
#65734=CARTESIAN_POINT('Ctrl Pts',(-3.27534954469206,1.,-2.15778690038359));
#65735=CARTESIAN_POINT('Ctrl Pts',(-3.27050245897244,-1.,-2.15205043199818));
#65736=CARTESIAN_POINT('Ctrl Pts',(-3.27050245897244,1.,-2.15205043199818));
#65737=CARTESIAN_POINT('Ctrl Pts',(-3.26564388189764,-1.,-2.14636805295663));
#65738=CARTESIAN_POINT('Ctrl Pts',(-3.26564388189764,1.,-2.14636805295663));
#65739=CARTESIAN_POINT('Ctrl Pts',(-3.26077002641868,-1.,-2.14073870754257));
#65740=CARTESIAN_POINT('Ctrl Pts',(-3.26077002641868,1.,-2.14073870754257));
#65741=CARTESIAN_POINT('Ctrl Pts',(-3.25586495065027,-1.,-2.13515375878786));
#65742=CARTESIAN_POINT('Ctrl Pts',(-3.25586495065027,1.,-2.13515375878786));
#65743=CARTESIAN_POINT('Ctrl Pts',(-3.25090574493994,-1.,-2.1296002839681));
#65744=CARTESIAN_POINT('Ctrl Pts',(-3.25090574493994,1.,-2.1296002839681));
#65745=CARTESIAN_POINT('Ctrl Pts',(-3.24587102613347,-1.,-2.12406646410943));
#65746=CARTESIAN_POINT('Ctrl Pts',(-3.24587102613347,1.,-2.12406646410943));
#65747=CARTESIAN_POINT('Ctrl Pts',(-3.24074905517282,-1.,-2.11854673326972));
#65748=CARTESIAN_POINT('Ctrl Pts',(-3.24074905517282,1.,-2.11854673326972));
#65749=CARTESIAN_POINT('Ctrl Pts',(-3.23554444767115,-1.,-2.11304604021784));
#65750=CARTESIAN_POINT('Ctrl Pts',(-3.23554444767115,1.,-2.11304604021784));
#65751=CARTESIAN_POINT('Ctrl Pts',(-3.23028945793334,-1.,-2.1075869964248));
#65752=CARTESIAN_POINT('Ctrl Pts',(-3.23028945793334,1.,-2.1075869964248));
#65753=CARTESIAN_POINT('Ctrl Pts',(-3.22503437553496,-1.,-2.10220384298533));
#65754=CARTESIAN_POINT('Ctrl Pts',(-3.22503437553496,1.,-2.10220384298533));
#65755=CARTESIAN_POINT('Ctrl Pts',(-3.21982707347067,-1.,-2.09692958434933));
#65756=CARTESIAN_POINT('Ctrl Pts',(-3.21982707347067,1.,-2.09692958434933));
#65757=CARTESIAN_POINT('Ctrl Pts',(-3.2146942960168,-1.,-2.0917841946046));
#65758=CARTESIAN_POINT('Ctrl Pts',(-3.2146942960168,1.,-2.0917841946046));
#65759=CARTESIAN_POINT('Ctrl Pts',(-3.20962575845433,-1.,-2.08676465517435));
#65760=CARTESIAN_POINT('Ctrl Pts',(-3.20962575845433,1.,-2.08676465517435));
#65761=CARTESIAN_POINT('Ctrl Pts',(-3.20454818630635,-1.,-2.08182850370816));
#65762=CARTESIAN_POINT('Ctrl Pts',(-3.20454818630635,1.,-2.08182850370816));
#65763=CARTESIAN_POINT('Ctrl Pts',(-3.19934132835879,-1.,-2.0769044187063));
#65764=CARTESIAN_POINT('Ctrl Pts',(-3.19934132835879,1.,-2.0769044187063));
#65765=CARTESIAN_POINT('Ctrl Pts',(-3.19388465568113,-1.,-2.07192253497765));
#65766=CARTESIAN_POINT('Ctrl Pts',(-3.19388465568113,1.,-2.07192253497765));
#65767=CARTESIAN_POINT('Ctrl Pts',(-3.18809755562297,-1.,-2.06684062744065));
#65768=CARTESIAN_POINT('Ctrl Pts',(-3.18809755562297,1.,-2.06684062744065));
#65769=CARTESIAN_POINT('Ctrl Pts',(-3.18197692964677,-1.,-2.06166849827143));
#65770=CARTESIAN_POINT('Ctrl Pts',(-3.18197692964677,1.,-2.06166849827143));
#65771=CARTESIAN_POINT('Ctrl Pts',(-3.17564906975592,-1.,-2.05650186773279));
#65772=CARTESIAN_POINT('Ctrl Pts',(-3.17564906975592,1.,-2.05650186773279));
#65773=CARTESIAN_POINT('Ctrl Pts',(-3.16936341689859,-1.,-2.05151770247452));
#65774=CARTESIAN_POINT('Ctrl Pts',(-3.16936341689859,1.,-2.05151770247452));
#65775=CARTESIAN_POINT('Ctrl Pts',(-3.16343165059235,-1.,-2.0469333124766));
#65776=CARTESIAN_POINT('Ctrl Pts',(-3.16343165059235,1.,-2.0469333124766));
#65777=CARTESIAN_POINT('Ctrl Pts',(-3.15817983946525,-1.,-2.04297406404132));
#65778=CARTESIAN_POINT('Ctrl Pts',(-3.15817983946525,1.,-2.04297406404132));
#65779=CARTESIAN_POINT('Ctrl Pts',(-3.1538999167466,-1.,-2.03984073791432));
#65780=CARTESIAN_POINT('Ctrl Pts',(-3.1538999167466,1.,-2.03984073791432));
#65781=CARTESIAN_POINT('Ctrl Pts',(-3.15079010635326,-1.,-2.03766932526171));
#65782=CARTESIAN_POINT('Ctrl Pts',(-3.15079010635326,1.,-2.03766932526171));
#65783=CARTESIAN_POINT('Ctrl Pts',(-3.14931281967585,-1.,-2.03675273048882));
#65784=CARTESIAN_POINT('Ctrl Pts',(-3.14931281967585,1.,-2.03675273048882));
#65785=CARTESIAN_POINT('Ctrl Pts',(-3.14878756590499,-1.,-2.03653654935384));
#65786=CARTESIAN_POINT('Ctrl Pts',(-3.14878756590499,1.,-2.03653654935384));
#65787=CARTESIAN_POINT('Ctrl Pts',(-3.14869618937138,-1.,-2.036601737578));
#65788=CARTESIAN_POINT('Ctrl Pts',(-3.14869618937138,1.,-2.036601737578));
#65789=CARTESIAN_POINT('Ctrl Pts',(-3.1487152044751,-1.,-2.03668666247593));
#65790=CARTESIAN_POINT('Ctrl Pts',(-3.1487152044751,1.,-2.03668666247593));
#65791=CARTESIAN_POINT('',(-3.44202241512147,1.,-2.40675750623143));
#65792=CARTESIAN_POINT('Ctrl Pts',(-3.44202241512147,1.,-2.40675750623143));
#65793=CARTESIAN_POINT('Ctrl Pts',(-3.44127120683402,1.,-2.40537592959345));
#65794=CARTESIAN_POINT('Ctrl Pts',(-3.43976627485223,1.,-2.40261515590099));
#65795=CARTESIAN_POINT('Ctrl Pts',(-3.43750133066036,1.,-2.39848113411429));
#65796=CARTESIAN_POINT('Ctrl Pts',(-3.43446630680436,1.,-2.39298338805823));
#65797=CARTESIAN_POINT('Ctrl Pts',(-3.43064732714472,1.,-2.38613505844641));
#65798=CARTESIAN_POINT('Ctrl Pts',(-3.42680309755241,1.,-2.37931067029517));
#65799=CARTESIAN_POINT('Ctrl Pts',(-3.42293356216595,1.,-2.37251035954351));
#65800=CARTESIAN_POINT('Ctrl Pts',(-3.41903866635384,1.,-2.36573431470314));
#65801=CARTESIAN_POINT('Ctrl Pts',(-3.4151183675076,1.,-2.35898278606449));
#65802=CARTESIAN_POINT('Ctrl Pts',(-3.41117262313464,1.,-2.35225606823649));
#65803=CARTESIAN_POINT('Ctrl Pts',(-3.40720137403888,1.,-2.34555447648901));
#65804=CARTESIAN_POINT('Ctrl Pts',(-3.40320452776646,1.,-2.33887832342715));
#65805=CARTESIAN_POINT('Ctrl Pts',(-3.39918194578115,1.,-2.33222789882601));
#65806=CARTESIAN_POINT('Ctrl Pts',(-3.39513342020045,1.,-2.32560343902683));
#65807=CARTESIAN_POINT('Ctrl Pts',(-3.39105869475112,1.,-2.31900513925627));
#65808=CARTESIAN_POINT('Ctrl Pts',(-3.38695751492659,1.,-2.31243319489505));
#65809=CARTESIAN_POINT('Ctrl Pts',(-3.38282967336676,1.,-2.30588783640389));
#65810=CARTESIAN_POINT('Ctrl Pts',(-3.37867504959382,1.,-2.29936936127588));
#65811=CARTESIAN_POINT('Ctrl Pts',(-3.37449367172707,1.,-2.2928781800731));
#65812=CARTESIAN_POINT('Ctrl Pts',(-3.37028570206357,1.,-2.28641481081045));
#65813=CARTESIAN_POINT('Ctrl Pts',(-3.36605130712978,1.,-2.27997979457968));
#65814=CARTESIAN_POINT('Ctrl Pts',(-3.36179055004369,1.,-2.27357362620902));
#65815=CARTESIAN_POINT('Ctrl Pts',(-3.35750328523077,1.,-2.26719668579921));
#65816=CARTESIAN_POINT('Ctrl Pts',(-3.35318902552676,1.,-2.26084915222484));
#65817=CARTESIAN_POINT('Ctrl Pts',(-3.34884690292342,1.,-2.25453097693524));
#65818=CARTESIAN_POINT('Ctrl Pts',(-3.34447596770768,1.,-2.24824207678288));
#65819=CARTESIAN_POINT('Ctrl Pts',(-3.34007543738044,1.,-2.24198249391437));
#65820=CARTESIAN_POINT('Ctrl Pts',(-3.33564495756478,1.,-2.2357525632881));
#65821=CARTESIAN_POINT('Ctrl Pts',(-3.33118487773593,1.,-2.22955308907221));
#65822=CARTESIAN_POINT('Ctrl Pts',(-3.32669646722871,1.,-2.22338548312758));
#65823=CARTESIAN_POINT('Ctrl Pts',(-3.32218125618955,1.,-2.21725135110889));
#65824=CARTESIAN_POINT('Ctrl Pts',(-3.31764044024231,1.,-2.21115211847872));
#65825=CARTESIAN_POINT('Ctrl Pts',(-3.3130742460895,1.,-2.20508863150608));
#65826=CARTESIAN_POINT('Ctrl Pts',(-3.30848134694596,1.,-2.19906078949924));
#65827=CARTESIAN_POINT('Ctrl Pts',(-3.30385816281831,1.,-2.19306710376112));
#65828=CARTESIAN_POINT('Ctrl Pts',(-3.29920022557635,1.,-2.18710556500325));
#65829=CARTESIAN_POINT('Ctrl Pts',(-3.29450361500484,1.,-2.18117455557062));
#65830=CARTESIAN_POINT('Ctrl Pts',(-3.28976645712566,1.,-2.17527380048422));
#65831=CARTESIAN_POINT('Ctrl Pts',(-3.2849901997973,1.,-2.16940517773459));
#65832=CARTESIAN_POINT('Ctrl Pts',(-3.28018150841414,1.,-2.16357391934434));
#65833=CARTESIAN_POINT('Ctrl Pts',(-3.27534954469206,1.,-2.15778690038359));
#65834=CARTESIAN_POINT('Ctrl Pts',(-3.27050245897244,1.,-2.15205043199818));
#65835=CARTESIAN_POINT('Ctrl Pts',(-3.26564388189764,1.,-2.14636805295663));
#65836=CARTESIAN_POINT('Ctrl Pts',(-3.26077002641868,1.,-2.14073870754257));
#65837=CARTESIAN_POINT('Ctrl Pts',(-3.25586495065027,1.,-2.13515375878786));
#65838=CARTESIAN_POINT('Ctrl Pts',(-3.25090574493994,1.,-2.1296002839681));
#65839=CARTESIAN_POINT('Ctrl Pts',(-3.24587102613347,1.,-2.12406646410943));
#65840=CARTESIAN_POINT('Ctrl Pts',(-3.24074905517282,1.,-2.11854673326972));
#65841=CARTESIAN_POINT('Ctrl Pts',(-3.23554444767115,1.,-2.11304604021784));
#65842=CARTESIAN_POINT('Ctrl Pts',(-3.23028945793334,1.,-2.1075869964248));
#65843=CARTESIAN_POINT('Ctrl Pts',(-3.22503437553496,1.,-2.10220384298533));
#65844=CARTESIAN_POINT('Ctrl Pts',(-3.21982707347067,1.,-2.09692958434933));
#65845=CARTESIAN_POINT('Ctrl Pts',(-3.2146942960168,1.,-2.0917841946046));
#65846=CARTESIAN_POINT('Ctrl Pts',(-3.20962575845433,1.,-2.08676465517435));
#65847=CARTESIAN_POINT('Ctrl Pts',(-3.20454818630635,1.,-2.08182850370816));
#65848=CARTESIAN_POINT('Ctrl Pts',(-3.19934132835879,1.,-2.0769044187063));
#65849=CARTESIAN_POINT('Ctrl Pts',(-3.19388465568113,1.,-2.07192253497765));
#65850=CARTESIAN_POINT('Ctrl Pts',(-3.18809755562297,1.,-2.06684062744065));
#65851=CARTESIAN_POINT('Ctrl Pts',(-3.18197692964677,1.,-2.06166849827143));
#65852=CARTESIAN_POINT('Ctrl Pts',(-3.17564906975592,1.,-2.05650186773279));
#65853=CARTESIAN_POINT('Ctrl Pts',(-3.16936341689859,1.,-2.05151770247452));
#65854=CARTESIAN_POINT('Ctrl Pts',(-3.16343165059235,1.,-2.0469333124766));
#65855=CARTESIAN_POINT('Ctrl Pts',(-3.15817983946525,1.,-2.04297406404132));
#65856=CARTESIAN_POINT('Ctrl Pts',(-3.1538999167466,1.,-2.03984073791432));
#65857=CARTESIAN_POINT('Ctrl Pts',(-3.15102344775396,1.,-2.03783225496023));
#65858=CARTESIAN_POINT('Ctrl Pts',(-3.14959882629936,1.,-2.03693188810614));
#65859=CARTESIAN_POINT('Ctrl Pts',(-3.14901193669147,1.,-2.03663974554941));
#65860=CARTESIAN_POINT('Ctrl Pts',(-3.1488193908823,1.,-2.03659701539175));
#65861=CARTESIAN_POINT('Ctrl Pts',(-3.14877060440425,1.,-2.03660101169564));
#65862=CARTESIAN_POINT('',(-3.44202241512147,0.,-2.40675750623143));
#65863=CARTESIAN_POINT('Ctrl Pts',(-2.91001063062876,-1.,-2.36523532225181));
#65864=CARTESIAN_POINT('Ctrl Pts',(-2.91001063062876,1.,-2.36523532225181));
#65865=CARTESIAN_POINT('Ctrl Pts',(-2.90992398626211,-1.,-2.36524348105112));
#65866=CARTESIAN_POINT('Ctrl Pts',(-2.90992398626211,1.,-2.36524348105112));
#65867=CARTESIAN_POINT('Ctrl Pts',(-2.90989022548032,-1.,-2.36535052956938));
#65868=CARTESIAN_POINT('Ctrl Pts',(-2.90989022548032,1.,-2.36535052956938));
#65869=CARTESIAN_POINT('Ctrl Pts',(-2.91025813830041,-1.,-2.36578327194741));
#65870=CARTESIAN_POINT('Ctrl Pts',(-2.91025813830041,1.,-2.36578327194741));
#65871=CARTESIAN_POINT('Ctrl Pts',(-2.9115863784204,-1.,-2.36690501170627));
#65872=CARTESIAN_POINT('Ctrl Pts',(-2.9115863784204,1.,-2.36690501170627));
#65873=CARTESIAN_POINT('Ctrl Pts',(-2.9146124988314,-1.,-2.36919161373173));
#65874=CARTESIAN_POINT('Ctrl Pts',(-2.9146124988314,1.,-2.36919161373173));
#65875=CARTESIAN_POINT('Ctrl Pts',(-2.91891503791411,-1.,-2.37229381109821));
#65876=CARTESIAN_POINT('Ctrl Pts',(-2.91891503791411,1.,-2.37229381109821));
#65877=CARTESIAN_POINT('Ctrl Pts',(-2.92430340582608,-1.,-2.3760651052403));
#65878=CARTESIAN_POINT('Ctrl Pts',(-2.92430340582608,1.,-2.3760651052403));
#65879=CARTESIAN_POINT('Ctrl Pts',(-2.93049643640206,-1.,-2.38028989582073));
#65880=CARTESIAN_POINT('Ctrl Pts',(-2.93049643640206,1.,-2.38028989582073));
#65881=CARTESIAN_POINT('Ctrl Pts',(-2.93717903280391,-1.,-2.38472771516311));
#65882=CARTESIAN_POINT('Ctrl Pts',(-2.93717903280391,1.,-2.38472771516311));
#65883=CARTESIAN_POINT('Ctrl Pts',(-2.94404820669076,-1.,-2.38914929090759));
#65884=CARTESIAN_POINT('Ctrl Pts',(-2.94404820669076,1.,-2.38914929090759));
#65885=CARTESIAN_POINT('Ctrl Pts',(-2.95085857128439,-1.,-2.39337207631667));
#65886=CARTESIAN_POINT('Ctrl Pts',(-2.95085857128439,1.,-2.39337207631667));
#65887=CARTESIAN_POINT('Ctrl Pts',(-2.95748006482942,-1.,-2.39730553974517));
#65888=CARTESIAN_POINT('Ctrl Pts',(-2.95748006482942,1.,-2.39730553974517));
#65889=CARTESIAN_POINT('Ctrl Pts',(-2.96390432240312,-1.,-2.4009556571164));
#65890=CARTESIAN_POINT('Ctrl Pts',(-2.96390432240312,1.,-2.4009556571164));
#65891=CARTESIAN_POINT('Ctrl Pts',(-2.9701964131236,-1.,-2.40438604734919));
#65892=CARTESIAN_POINT('Ctrl Pts',(-2.9701964131236,1.,-2.40438604734919));
#65893=CARTESIAN_POINT('Ctrl Pts',(-2.97646002822422,-1.,-2.40768975073713));
#65894=CARTESIAN_POINT('Ctrl Pts',(-2.97646002822422,1.,-2.40768975073713));
#65895=CARTESIAN_POINT('Ctrl Pts',(-2.98280015815107,-1.,-2.41095909342571));
#65896=CARTESIAN_POINT('Ctrl Pts',(-2.98280015815107,1.,-2.41095909342571));
#65897=CARTESIAN_POINT('Ctrl Pts',(-2.98927983005796,-1.,-2.41425064199586));
#65898=CARTESIAN_POINT('Ctrl Pts',(-2.98927983005796,1.,-2.41425064199586));
#65899=CARTESIAN_POINT('Ctrl Pts',(-2.99590509293503,-1.,-2.41757324500514));
#65900=CARTESIAN_POINT('Ctrl Pts',(-2.99590509293503,1.,-2.41757324500514));
#65901=CARTESIAN_POINT('Ctrl Pts',(-3.00264868585996,-1.,-2.42090763946779));
#65902=CARTESIAN_POINT('Ctrl Pts',(-3.00264868585996,1.,-2.42090763946779));
#65903=CARTESIAN_POINT('Ctrl Pts',(-3.00946442616658,-1.,-2.42421849439613));
#65904=CARTESIAN_POINT('Ctrl Pts',(-3.00946442616658,1.,-2.42421849439613));
#65905=CARTESIAN_POINT('Ctrl Pts',(-3.01630420830504,-1.,-2.42746856264168));
#65906=CARTESIAN_POINT('Ctrl Pts',(-3.01630420830504,1.,-2.42746856264168));
#65907=CARTESIAN_POINT('Ctrl Pts',(-3.02313656036004,-1.,-2.43063415586637));
#65908=CARTESIAN_POINT('Ctrl Pts',(-3.02313656036004,1.,-2.43063415586637));
#65909=CARTESIAN_POINT('Ctrl Pts',(-3.02995534946978,-1.,-2.43371241361488));
#65910=CARTESIAN_POINT('Ctrl Pts',(-3.02995534946978,1.,-2.43371241361488));
#65911=CARTESIAN_POINT('Ctrl Pts',(-3.03676949672821,-1.,-2.43671278042414));
#65912=CARTESIAN_POINT('Ctrl Pts',(-3.03676949672821,1.,-2.43671278042414));
#65913=CARTESIAN_POINT('Ctrl Pts',(-3.04359685040555,-1.,-2.43965194061857));
#65914=CARTESIAN_POINT('Ctrl Pts',(-3.04359685040555,1.,-2.43965194061857));
#65915=CARTESIAN_POINT('Ctrl Pts',(-3.05045678021504,-1.,-2.44254768923105));
#65916=CARTESIAN_POINT('Ctrl Pts',(-3.05045678021504,1.,-2.44254768923105));
#65917=CARTESIAN_POINT('Ctrl Pts',(-3.05736242671506,-1.,-2.44541251892556));
#65918=CARTESIAN_POINT('Ctrl Pts',(-3.05736242671506,1.,-2.44541251892556));
#65919=CARTESIAN_POINT('Ctrl Pts',(-3.06431596421405,-1.,-2.44824970516544));
#65920=CARTESIAN_POINT('Ctrl Pts',(-3.06431596421405,1.,-2.44824970516544));
#65921=CARTESIAN_POINT('Ctrl Pts',(-3.07131290521297,-1.,-2.45105688854422));
#65922=CARTESIAN_POINT('Ctrl Pts',(-3.07131290521297,1.,-2.45105688854422));
#65923=CARTESIAN_POINT('Ctrl Pts',(-3.07834472886139,-1.,-2.4538282678779));
#65924=CARTESIAN_POINT('Ctrl Pts',(-3.07834472886139,1.,-2.4538282678779));
#65925=CARTESIAN_POINT('Ctrl Pts',(-3.08540206545315,-1.,-2.45655725437039));
#65926=CARTESIAN_POINT('Ctrl Pts',(-3.08540206545315,1.,-2.45655725437039));
#65927=CARTESIAN_POINT('Ctrl Pts',(-3.09247787931887,-1.,-2.4592391256388));
#65928=CARTESIAN_POINT('Ctrl Pts',(-3.09247787931887,1.,-2.4592391256388));
#65929=CARTESIAN_POINT('Ctrl Pts',(-3.09956993697052,-1.,-2.46187308501884));
#65930=CARTESIAN_POINT('Ctrl Pts',(-3.09956993697052,1.,-2.46187308501884));
#65931=CARTESIAN_POINT('Ctrl Pts',(-3.1066790790198,-1.,-2.46446082979646));
#65932=CARTESIAN_POINT('Ctrl Pts',(-3.1066790790198,1.,-2.46446082979646));
#65933=CARTESIAN_POINT('Ctrl Pts',(-3.11380805536122,-1.,-2.46700558843506));
#65934=CARTESIAN_POINT('Ctrl Pts',(-3.11380805536122,1.,-2.46700558843506));
#65935=CARTESIAN_POINT('Ctrl Pts',(-3.12096015766983,-1.,-2.46951098947469));
#65936=CARTESIAN_POINT('Ctrl Pts',(-3.12096015766983,1.,-2.46951098947469));
#65937=CARTESIAN_POINT('Ctrl Pts',(-3.12813790805952,-1.,-2.47197997765871));
#65938=CARTESIAN_POINT('Ctrl Pts',(-3.12813790805952,1.,-2.47197997765871));
#65939=CARTESIAN_POINT('Ctrl Pts',(-3.13534181229295,-1.,-2.47441378371932));
#65940=CARTESIAN_POINT('Ctrl Pts',(-3.13534181229295,1.,-2.47441378371932));
#65941=CARTESIAN_POINT('Ctrl Pts',(-3.1425709954655,-1.,-2.47681245356109));
#65942=CARTESIAN_POINT('Ctrl Pts',(-3.1425709954655,1.,-2.47681245356109));
#65943=CARTESIAN_POINT('Ctrl Pts',(-3.14982373241352,-1.,-2.47917529057029));
#65944=CARTESIAN_POINT('Ctrl Pts',(-3.14982373241352,1.,-2.47917529057029));
#65945=CARTESIAN_POINT('Ctrl Pts',(-3.15709802322739,-1.,-2.48150133566571));
#65946=CARTESIAN_POINT('Ctrl Pts',(-3.15709802322739,1.,-2.48150133566571));
#65947=CARTESIAN_POINT('Ctrl Pts',(-3.16439213290161,-1.,-2.48378981792725));
#65948=CARTESIAN_POINT('Ctrl Pts',(-3.16439213290161,1.,-2.48378981792725));
#65949=CARTESIAN_POINT('Ctrl Pts',(-3.17170518863313,-1.,-2.48604065348587));
#65950=CARTESIAN_POINT('Ctrl Pts',(-3.17170518863313,1.,-2.48604065348587));
#65951=CARTESIAN_POINT('Ctrl Pts',(-3.17903698136622,-1.,-2.48825428288201));
#65952=CARTESIAN_POINT('Ctrl Pts',(-3.17903698136622,1.,-2.48825428288201));
#65953=CARTESIAN_POINT('Ctrl Pts',(-3.18638771282266,-1.,-2.49043146334059));
#65954=CARTESIAN_POINT('Ctrl Pts',(-3.18638771282266,1.,-2.49043146334059));
#65955=CARTESIAN_POINT('Ctrl Pts',(-3.19375775555798,-1.,-2.49257307239848));
#65956=CARTESIAN_POINT('Ctrl Pts',(-3.19375775555798,1.,-2.49257307239848));
#65957=CARTESIAN_POINT('Ctrl Pts',(-3.20114742397588,-1.,-2.49467992057755));
#65958=CARTESIAN_POINT('Ctrl Pts',(-3.20114742397588,1.,-2.49467992057755));
#65959=CARTESIAN_POINT('Ctrl Pts',(-3.20855669849836,-1.,-2.4967525264737));
#65960=CARTESIAN_POINT('Ctrl Pts',(-3.20855669849836,1.,-2.4967525264737));
#65961=CARTESIAN_POINT('Ctrl Pts',(-3.21598526261286,-1.,-2.4987911459939));
#65962=CARTESIAN_POINT('Ctrl Pts',(-3.21598526261286,1.,-2.4987911459939));
#65963=CARTESIAN_POINT('Ctrl Pts',(-3.22343262620503,-1.,-2.50079587201957));
#65964=CARTESIAN_POINT('Ctrl Pts',(-3.22343262620503,1.,-2.50079587201957));
#65965=CARTESIAN_POINT('Ctrl Pts',(-3.23089822320646,-1.,-2.50276671338111));
#65966=CARTESIAN_POINT('Ctrl Pts',(-3.23089822320646,1.,-2.50276671338111));
#65967=CARTESIAN_POINT('Ctrl Pts',(-3.23838151080319,-1.,-2.5047036758003));
#65968=CARTESIAN_POINT('Ctrl Pts',(-3.23838151080319,1.,-2.5047036758003));
#65969=CARTESIAN_POINT('Ctrl Pts',(-3.24588208983849,-1.,-2.506606859405));
#65970=CARTESIAN_POINT('Ctrl Pts',(-3.24588208983849,1.,-2.506606859405));
#65971=CARTESIAN_POINT('Ctrl Pts',(-3.25339971460982,-1.,-2.50847647070723));
#65972=CARTESIAN_POINT('Ctrl Pts',(-3.25339971460982,1.,-2.50847647070723));
#65973=CARTESIAN_POINT('Ctrl Pts',(-3.26093423001434,-1.,-2.51031277813486));
#65974=CARTESIAN_POINT('Ctrl Pts',(-3.26093423001434,1.,-2.51031277813486));
#65975=CARTESIAN_POINT('Ctrl Pts',(-3.26848552888115,-1.,-2.51211608411423));
#65976=CARTESIAN_POINT('Ctrl Pts',(-3.26848552888115,1.,-2.51211608411423));
#65977=CARTESIAN_POINT('Ctrl Pts',(-3.27605350473142,-1.,-2.513886692704));
#65978=CARTESIAN_POINT('Ctrl Pts',(-3.27605350473142,1.,-2.513886692704));
#65979=CARTESIAN_POINT('Ctrl Pts',(-3.28363799702982,-1.,-2.51562487464514));
#65980=CARTESIAN_POINT('Ctrl Pts',(-3.28363799702982,1.,-2.51562487464514));
#65981=CARTESIAN_POINT('Ctrl Pts',(-3.2912387729927,-1.,-2.51733085123797));
#65982=CARTESIAN_POINT('Ctrl Pts',(-3.2912387729927,1.,-2.51733085123797));
#65983=CARTESIAN_POINT('Ctrl Pts',(-3.29885556388352,-1.,-2.51900480701069));
#65984=CARTESIAN_POINT('Ctrl Pts',(-3.29885556388352,1.,-2.51900480701069));
#65985=CARTESIAN_POINT('Ctrl Pts',(-3.30648808815442,-1.,-2.52064689568511));
#65986=CARTESIAN_POINT('Ctrl Pts',(-3.30648808815442,1.,-2.52064689568511));
#65987=CARTESIAN_POINT('Ctrl Pts',(-3.31413607874645,-1.,-2.52225724871313));
#65988=CARTESIAN_POINT('Ctrl Pts',(-3.31413607874645,1.,-2.52225724871313));
#65989=CARTESIAN_POINT('Ctrl Pts',(-3.32179931078699,-1.,-2.5238359839626));
#65990=CARTESIAN_POINT('Ctrl Pts',(-3.32179931078699,1.,-2.5238359839626));
#65991=CARTESIAN_POINT('Ctrl Pts',(-3.32947762187533,-1.,-2.52538321164634));
#65992=CARTESIAN_POINT('Ctrl Pts',(-3.32947762187533,1.,-2.52538321164634));
#65993=CARTESIAN_POINT('Ctrl Pts',(-3.33717089999103,-1.,-2.52689902690158));
#65994=CARTESIAN_POINT('Ctrl Pts',(-3.33717089999103,1.,-2.52689902690158));
#65995=CARTESIAN_POINT('Ctrl Pts',(-3.34333744115511,-1.,-2.52808660915689));
#65996=CARTESIAN_POINT('Ctrl Pts',(-3.34333744115511,1.,-2.52808660915689));
#65997=CARTESIAN_POINT('Ctrl Pts',(-3.34796903576663,-1.,-2.52896321610703));
#65998=CARTESIAN_POINT('Ctrl Pts',(-3.34796903576663,1.,-2.52896321610703));
#65999=CARTESIAN_POINT('Ctrl Pts',(-3.35105973714071,-1.,-2.5295413654909));
#66000=CARTESIAN_POINT('Ctrl Pts',(-3.35105973714071,1.,-2.5295413654909));
#66001=CARTESIAN_POINT('Ctrl Pts',(-3.35260583073571,-1.,-2.52982887637028));
#66002=CARTESIAN_POINT('Ctrl Pts',(-3.35260583073571,1.,-2.52982887637028));
#66003=CARTESIAN_POINT('',(-2.90994629141676,1.,-2.36531447826073));
#66004=CARTESIAN_POINT('Ctrl Pts',(-2.90994629141676,-1.,-2.36531447826074));
#66005=CARTESIAN_POINT('Ctrl Pts',(-2.90994629141676,-0.666666666666667,
-2.36531447826074));
#66006=CARTESIAN_POINT('Ctrl Pts',(-2.90994629141676,-0.333333333333333,
-2.36531447826074));
#66007=CARTESIAN_POINT('Ctrl Pts',(-2.90994629141676,0.333333333333333,
-2.36531447826074));
#66008=CARTESIAN_POINT('Ctrl Pts',(-2.90994629141676,0.666666666666667,
-2.36531447826074));
#66009=CARTESIAN_POINT('Ctrl Pts',(-2.90994629141676,1.,-2.36531447826074));
#66010=CARTESIAN_POINT('',(-3.35260583073571,1.,-2.52982887637028));
#66011=CARTESIAN_POINT('',(-3.35260583073571,0.,-2.52982887637028));
#66012=CARTESIAN_POINT('Ctrl Pts',(-2.90994629141676,1.,-2.36531447826073));
#66013=CARTESIAN_POINT('Ctrl Pts',(-2.90995756655606,1.,-2.36536211188453));
#66014=CARTESIAN_POINT('Ctrl Pts',(-2.91005770527719,1.,-2.36553202948613));
#66015=CARTESIAN_POINT('Ctrl Pts',(-2.91051690822156,1.,-2.36599991765749));
#66016=CARTESIAN_POINT('Ctrl Pts',(-2.91181344022549,1.,-2.36707658451664));
#66017=CARTESIAN_POINT('Ctrl Pts',(-2.9146124988314,1.,-2.36919161373173));
#66018=CARTESIAN_POINT('Ctrl Pts',(-2.91891503791411,1.,-2.37229381109821));
#66019=CARTESIAN_POINT('Ctrl Pts',(-2.92430340582608,1.,-2.3760651052403));
#66020=CARTESIAN_POINT('Ctrl Pts',(-2.93049643640206,1.,-2.38028989582073));
#66021=CARTESIAN_POINT('Ctrl Pts',(-2.93717903280391,1.,-2.38472771516311));
#66022=CARTESIAN_POINT('Ctrl Pts',(-2.94404820669076,1.,-2.38914929090759));
#66023=CARTESIAN_POINT('Ctrl Pts',(-2.95085857128439,1.,-2.39337207631667));
#66024=CARTESIAN_POINT('Ctrl Pts',(-2.95748006482942,1.,-2.39730553974517));
#66025=CARTESIAN_POINT('Ctrl Pts',(-2.96390432240312,1.,-2.4009556571164));
#66026=CARTESIAN_POINT('Ctrl Pts',(-2.9701964131236,1.,-2.40438604734919));
#66027=CARTESIAN_POINT('Ctrl Pts',(-2.97646002822422,1.,-2.40768975073713));
#66028=CARTESIAN_POINT('Ctrl Pts',(-2.98280015815107,1.,-2.41095909342571));
#66029=CARTESIAN_POINT('Ctrl Pts',(-2.98927983005796,1.,-2.41425064199586));
#66030=CARTESIAN_POINT('Ctrl Pts',(-2.99590509293503,1.,-2.41757324500514));
#66031=CARTESIAN_POINT('Ctrl Pts',(-3.00264868585996,1.,-2.42090763946779));
#66032=CARTESIAN_POINT('Ctrl Pts',(-3.00946442616658,1.,-2.42421849439613));
#66033=CARTESIAN_POINT('Ctrl Pts',(-3.01630420830504,1.,-2.42746856264168));
#66034=CARTESIAN_POINT('Ctrl Pts',(-3.02313656036004,1.,-2.43063415586637));
#66035=CARTESIAN_POINT('Ctrl Pts',(-3.02995534946978,1.,-2.43371241361488));
#66036=CARTESIAN_POINT('Ctrl Pts',(-3.03676949672821,1.,-2.43671278042414));
#66037=CARTESIAN_POINT('Ctrl Pts',(-3.04359685040555,1.,-2.43965194061857));
#66038=CARTESIAN_POINT('Ctrl Pts',(-3.05045678021504,1.,-2.44254768923105));
#66039=CARTESIAN_POINT('Ctrl Pts',(-3.05736242671506,1.,-2.44541251892556));
#66040=CARTESIAN_POINT('Ctrl Pts',(-3.06431596421405,1.,-2.44824970516544));
#66041=CARTESIAN_POINT('Ctrl Pts',(-3.07131290521297,1.,-2.45105688854422));
#66042=CARTESIAN_POINT('Ctrl Pts',(-3.07834472886139,1.,-2.4538282678779));
#66043=CARTESIAN_POINT('Ctrl Pts',(-3.08540206545315,1.,-2.45655725437039));
#66044=CARTESIAN_POINT('Ctrl Pts',(-3.09247787931887,1.,-2.4592391256388));
#66045=CARTESIAN_POINT('Ctrl Pts',(-3.09956993697052,1.,-2.46187308501884));
#66046=CARTESIAN_POINT('Ctrl Pts',(-3.1066790790198,1.,-2.46446082979646));
#66047=CARTESIAN_POINT('Ctrl Pts',(-3.11380805536122,1.,-2.46700558843506));
#66048=CARTESIAN_POINT('Ctrl Pts',(-3.12096015766983,1.,-2.46951098947469));
#66049=CARTESIAN_POINT('Ctrl Pts',(-3.12813790805952,1.,-2.47197997765871));
#66050=CARTESIAN_POINT('Ctrl Pts',(-3.13534181229295,1.,-2.47441378371932));
#66051=CARTESIAN_POINT('Ctrl Pts',(-3.1425709954655,1.,-2.47681245356109));
#66052=CARTESIAN_POINT('Ctrl Pts',(-3.14982373241352,1.,-2.47917529057029));
#66053=CARTESIAN_POINT('Ctrl Pts',(-3.15709802322739,1.,-2.48150133566571));
#66054=CARTESIAN_POINT('Ctrl Pts',(-3.16439213290161,1.,-2.48378981792725));
#66055=CARTESIAN_POINT('Ctrl Pts',(-3.17170518863313,1.,-2.48604065348587));
#66056=CARTESIAN_POINT('Ctrl Pts',(-3.17903698136622,1.,-2.48825428288201));
#66057=CARTESIAN_POINT('Ctrl Pts',(-3.18638771282266,1.,-2.49043146334059));
#66058=CARTESIAN_POINT('Ctrl Pts',(-3.19375775555798,1.,-2.49257307239848));
#66059=CARTESIAN_POINT('Ctrl Pts',(-3.20114742397588,1.,-2.49467992057755));
#66060=CARTESIAN_POINT('Ctrl Pts',(-3.20855669849836,1.,-2.4967525264737));
#66061=CARTESIAN_POINT('Ctrl Pts',(-3.21598526261286,1.,-2.4987911459939));
#66062=CARTESIAN_POINT('Ctrl Pts',(-3.22343262620503,1.,-2.50079587201957));
#66063=CARTESIAN_POINT('Ctrl Pts',(-3.23089822320646,1.,-2.50276671338111));
#66064=CARTESIAN_POINT('Ctrl Pts',(-3.23838151080319,1.,-2.5047036758003));
#66065=CARTESIAN_POINT('Ctrl Pts',(-3.24588208983849,1.,-2.506606859405));
#66066=CARTESIAN_POINT('Ctrl Pts',(-3.25339971460982,1.,-2.50847647070723));
#66067=CARTESIAN_POINT('Ctrl Pts',(-3.26093423001434,1.,-2.51031277813486));
#66068=CARTESIAN_POINT('Ctrl Pts',(-3.26848552888115,1.,-2.51211608411423));
#66069=CARTESIAN_POINT('Ctrl Pts',(-3.27605350473142,1.,-2.513886692704));
#66070=CARTESIAN_POINT('Ctrl Pts',(-3.28363799702982,1.,-2.51562487464514));
#66071=CARTESIAN_POINT('Ctrl Pts',(-3.2912387729927,1.,-2.51733085123797));
#66072=CARTESIAN_POINT('Ctrl Pts',(-3.29885556388352,1.,-2.51900480701069));
#66073=CARTESIAN_POINT('Ctrl Pts',(-3.30648808815442,1.,-2.52064689568511));
#66074=CARTESIAN_POINT('Ctrl Pts',(-3.31413607874645,1.,-2.52225724871313));
#66075=CARTESIAN_POINT('Ctrl Pts',(-3.32179931078699,1.,-2.5238359839626));
#66076=CARTESIAN_POINT('Ctrl Pts',(-3.32947762187533,1.,-2.52538321164634));
#66077=CARTESIAN_POINT('Ctrl Pts',(-3.33717089999103,1.,-2.52689902690158));
#66078=CARTESIAN_POINT('Ctrl Pts',(-3.34333744115511,1.,-2.52808660915689));
#66079=CARTESIAN_POINT('Ctrl Pts',(-3.34796903576663,1.,-2.52896321610703));
#66080=CARTESIAN_POINT('Ctrl Pts',(-3.35105973714071,1.,-2.5295413654909));
#66081=CARTESIAN_POINT('Ctrl Pts',(-3.35260583073571,1.,-2.52982887637028));
#66082=CARTESIAN_POINT('Origin',(-3.35260583073571,0.,-2.52982887637028));
#66083=CARTESIAN_POINT('',(-3.44202241512147,1.,-2.40675750623143));
#66084=CARTESIAN_POINT('Origin',(0.,0.,0.));
#66085=CARTESIAN_POINT('',(-2.79140942341378,1.,-2.50410331873042));
#66086=CARTESIAN_POINT('Origin',(0.,1.,0.));
#66087=CARTESIAN_POINT('Ctrl Pts',(-2.79140942341378,1.,-2.50410331873042));
#66088=CARTESIAN_POINT('Ctrl Pts',(-2.79140942341378,0.666666666666667,
-2.50410331873042));
#66089=CARTESIAN_POINT('Ctrl Pts',(-2.79140942341378,0.333333333333333,
-2.50410331873042));
#66090=CARTESIAN_POINT('Ctrl Pts',(-2.79140942341378,-0.333333333333333,
-2.50410331873042));
#66091=CARTESIAN_POINT('Ctrl Pts',(-2.79140942341378,-0.666666666666667,
-2.50410331873042));
#66092=CARTESIAN_POINT('Ctrl Pts',(-2.79140942341378,-1.,-2.50410331873042));
#66093=CARTESIAN_POINT('Ctrl Pts',(-3.02314558451372,-1.,-2.91557726271063));
#66094=CARTESIAN_POINT('Ctrl Pts',(-3.02314558451372,1.,-2.91557726271063));
#66095=CARTESIAN_POINT('Ctrl Pts',(-3.02261975104912,-1.,-2.91409518070707));
#66096=CARTESIAN_POINT('Ctrl Pts',(-3.02261975104912,1.,-2.91409518070707));
#66097=CARTESIAN_POINT('Ctrl Pts',(-3.02156522743299,-1.,-2.91113297349052));
#66098=CARTESIAN_POINT('Ctrl Pts',(-3.02156522743299,1.,-2.91113297349052));
#66099=CARTESIAN_POINT('Ctrl Pts',(-3.01997487194926,-1.,-2.90669553303902));
#66100=CARTESIAN_POINT('Ctrl Pts',(-3.01997487194926,1.,-2.90669553303902));
#66101=CARTESIAN_POINT('Ctrl Pts',(-3.01783725123646,-1.,-2.90079069102661));
#66102=CARTESIAN_POINT('Ctrl Pts',(-3.01783725123646,1.,-2.90079069102661));
#66103=CARTESIAN_POINT('Ctrl Pts',(-3.01513660433291,-1.,-2.8934292556764));
#66104=CARTESIAN_POINT('Ctrl Pts',(-3.01513660433291,1.,-2.8934292556764));
#66105=CARTESIAN_POINT('Ctrl Pts',(-3.01240727309568,-1.,-2.88608751706796));
#66106=CARTESIAN_POINT('Ctrl Pts',(-3.01240727309568,1.,-2.88608751706796));
#66107=CARTESIAN_POINT('Ctrl Pts',(-3.0096491810855,-1.,-2.87876560072799));
#66108=CARTESIAN_POINT('Ctrl Pts',(-3.0096491810855,1.,-2.87876560072799));
#66109=CARTESIAN_POINT('Ctrl Pts',(-3.00686224485374,-1.,-2.87146368430104));
#66110=CARTESIAN_POINT('Ctrl Pts',(-3.00686224485374,1.,-2.87146368430104));
#66111=CARTESIAN_POINT('Ctrl Pts',(-3.00404638316245,-1.,-2.86418200833065));
#66112=CARTESIAN_POINT('Ctrl Pts',(-3.00404638316245,1.,-2.86418200833065));
#66113=CARTESIAN_POINT('Ctrl Pts',(-3.0012015079552,-1.,-2.85692085715129));
#66114=CARTESIAN_POINT('Ctrl Pts',(-3.0012015079552,1.,-2.85692085715129));
#66115=CARTESIAN_POINT('Ctrl Pts',(-2.99832751144566,-1.,-2.84968053289104));
#66116=CARTESIAN_POINT('Ctrl Pts',(-2.99832751144566,1.,-2.84968053289104));
#66117=CARTESIAN_POINT('Ctrl Pts',(-2.995424253416,-1.,-2.84246132984334));
#66118=CARTESIAN_POINT('Ctrl Pts',(-2.995424253416,1.,-2.84246132984334));
#66119=CARTESIAN_POINT('Ctrl Pts',(-2.99249155170479,-1.,-2.83526351254383));
#66120=CARTESIAN_POINT('Ctrl Pts',(-2.99249155170479,1.,-2.83526351254383));
#66121=CARTESIAN_POINT('Ctrl Pts',(-2.98952916401699,-1.,-2.82808728190402));
#66122=CARTESIAN_POINT('Ctrl Pts',(-2.98952916401699,1.,-2.82808728190402));
#66123=CARTESIAN_POINT('Ctrl Pts',(-2.98653680669434,-1.,-2.82093279065704));
#66124=CARTESIAN_POINT('Ctrl Pts',(-2.98653680669434,1.,-2.82093279065704));
#66125=CARTESIAN_POINT('Ctrl Pts',(-2.9835141977994,-1.,-2.81380019196454));
#66126=CARTESIAN_POINT('Ctrl Pts',(-2.9835141977994,1.,-2.81380019196454));
#66127=CARTESIAN_POINT('Ctrl Pts',(-2.98046109647299,-1.,-2.80668968101162));
#66128=CARTESIAN_POINT('Ctrl Pts',(-2.98046109647299,1.,-2.80668968101162));
#66129=CARTESIAN_POINT('Ctrl Pts',(-2.97737733718242,-1.,-2.79960153278186));
#66130=CARTESIAN_POINT('Ctrl Pts',(-2.97737733718242,1.,-2.79960153278186));
#66131=CARTESIAN_POINT('Ctrl Pts',(-2.97426288347475,-1.,-2.79253615718147));
#66132=CARTESIAN_POINT('Ctrl Pts',(-2.97426288347475,1.,-2.79253615718147));
#66133=CARTESIAN_POINT('Ctrl Pts',(-2.97111781461349,-1.,-2.78549409123657));
#66134=CARTESIAN_POINT('Ctrl Pts',(-2.97111781461349,1.,-2.78549409123657));
#66135=CARTESIAN_POINT('Ctrl Pts',(-2.9679422104295,-1.,-2.77847589542767));
#66136=CARTESIAN_POINT('Ctrl Pts',(-2.9679422104295,1.,-2.77847589542767));
#66137=CARTESIAN_POINT('Ctrl Pts',(-2.96473605585548,-1.,-2.77148206836464));
#66138=CARTESIAN_POINT('Ctrl Pts',(-2.96473605585548,1.,-2.77148206836464));
#66139=CARTESIAN_POINT('Ctrl Pts',(-2.96149914764832,-1.,-2.76451296269571));
#66140=CARTESIAN_POINT('Ctrl Pts',(-2.96149914764832,1.,-2.76451296269571));
#66141=CARTESIAN_POINT('Ctrl Pts',(-2.9582309766594,-1.,-2.75756867888393));
#66142=CARTESIAN_POINT('Ctrl Pts',(-2.9582309766594,1.,-2.75756867888393));
#66143=CARTESIAN_POINT('Ctrl Pts',(-2.95493069316211,-1.,-2.75064903318996));
#66144=CARTESIAN_POINT('Ctrl Pts',(-2.95493069316211,1.,-2.75064903318996));
#66145=CARTESIAN_POINT('Ctrl Pts',(-2.95159737214305,-1.,-2.7437537949221));
#66146=CARTESIAN_POINT('Ctrl Pts',(-2.95159737214305,1.,-2.7437537949221));
#66147=CARTESIAN_POINT('Ctrl Pts',(-2.94823023414381,-1.,-2.73688288329825));
#66148=CARTESIAN_POINT('Ctrl Pts',(-2.94823023414381,1.,-2.73688288329825));
#66149=CARTESIAN_POINT('Ctrl Pts',(-2.94482887675139,-1.,-2.73003657371613));
#66150=CARTESIAN_POINT('Ctrl Pts',(-2.94482887675139,1.,-2.73003657371613));
#66151=CARTESIAN_POINT('Ctrl Pts',(-2.94139351933882,-1.,-2.72321571511322));
#66152=CARTESIAN_POINT('Ctrl Pts',(-2.94139351933882,1.,-2.72321571511322));
#66153=CARTESIAN_POINT('Ctrl Pts',(-2.93792519474955,-1.,-2.71642190053575));
#66154=CARTESIAN_POINT('Ctrl Pts',(-2.93792519474955,1.,-2.71642190053575));
#66155=CARTESIAN_POINT('Ctrl Pts',(-2.93442516311168,-1.,-2.70965695523776));
#66156=CARTESIAN_POINT('Ctrl Pts',(-2.93442516311168,1.,-2.70965695523776));
#66157=CARTESIAN_POINT('Ctrl Pts',(-2.93089438233746,-1.,-2.70292247416881));
#66158=CARTESIAN_POINT('Ctrl Pts',(-2.93089438233746,1.,-2.70292247416881));
#66159=CARTESIAN_POINT('Ctrl Pts',(-2.92733294395268,-1.,-2.69621932864302));
#66160=CARTESIAN_POINT('Ctrl Pts',(-2.92733294395268,1.,-2.69621932864302));
#66161=CARTESIAN_POINT('Ctrl Pts',(-2.92373955325876,-1.,-2.68954721165342));
#66162=CARTESIAN_POINT('Ctrl Pts',(-2.92373955325876,1.,-2.68954721165342));
#66163=CARTESIAN_POINT('Ctrl Pts',(-2.92011090722152,-1.,-2.68290409279689));
#66164=CARTESIAN_POINT('Ctrl Pts',(-2.92011090722152,1.,-2.68290409279689));
#66165=CARTESIAN_POINT('Ctrl Pts',(-2.91644290704281,-1.,-2.67628728855309));
#66166=CARTESIAN_POINT('Ctrl Pts',(-2.91644290704281,1.,-2.67628728855309));
#66167=CARTESIAN_POINT('Ctrl Pts',(-2.91273193382876,-1.,-2.66969458792627));
#66168=CARTESIAN_POINT('Ctrl Pts',(-2.91273193382876,1.,-2.66969458792627));
#66169=CARTESIAN_POINT('Ctrl Pts',(-2.90897617968921,-1.,-2.66312542616808));
#66170=CARTESIAN_POINT('Ctrl Pts',(-2.90897617968921,1.,-2.66312542616808));
#66171=CARTESIAN_POINT('Ctrl Pts',(-2.90517678087467,-1.,-2.65658188464287));
#66172=CARTESIAN_POINT('Ctrl Pts',(-2.90517678087467,1.,-2.65658188464287));
#66173=CARTESIAN_POINT('Ctrl Pts',(-2.90133950224879,-1.,-2.65007017365576));
#66174=CARTESIAN_POINT('Ctrl Pts',(-2.90133950224879,1.,-2.65007017365576));
#66175=CARTESIAN_POINT('Ctrl Pts',(-2.89747231723361,-1.,-2.64359851684146));
#66176=CARTESIAN_POINT('Ctrl Pts',(-2.89747231723361,1.,-2.64359851684146));
#66177=CARTESIAN_POINT('Ctrl Pts',(-2.89358228854557,-1.,-2.63717442263944));
#66178=CARTESIAN_POINT('Ctrl Pts',(-2.89358228854557,1.,-2.63717442263944));
#66179=CARTESIAN_POINT('Ctrl Pts',(-2.88967244854243,-1.,-2.63080195420771));
#66180=CARTESIAN_POINT('Ctrl Pts',(-2.88967244854243,1.,-2.63080195420771));
#66181=CARTESIAN_POINT('Ctrl Pts',(-2.88573922195049,-1.,-2.62447947640253));
#66182=CARTESIAN_POINT('Ctrl Pts',(-2.88573922195049,1.,-2.62447947640253));
#66183=CARTESIAN_POINT('Ctrl Pts',(-2.88176821427502,-1.,-2.61819596473087));
#66184=CARTESIAN_POINT('Ctrl Pts',(-2.88176821427502,1.,-2.61819596473087));
#66185=CARTESIAN_POINT('Ctrl Pts',(-2.87773881947885,-1.,-2.61193507170928));
#66186=CARTESIAN_POINT('Ctrl Pts',(-2.87773881947885,1.,-2.61193507170928));
#66187=CARTESIAN_POINT('Ctrl Pts',(-2.87363176656475,-1.,-2.6056817788128));
#66188=CARTESIAN_POINT('Ctrl Pts',(-2.87363176656475,1.,-2.6056817788128));
#66189=CARTESIAN_POINT('Ctrl Pts',(-2.86943633170712,-1.,-2.59942875223202));
#66190=CARTESIAN_POINT('Ctrl Pts',(-2.86943633170712,1.,-2.59942875223202));
#66191=CARTESIAN_POINT('Ctrl Pts',(-2.86515629953528,-1.,-2.59318160184921));
#66192=CARTESIAN_POINT('Ctrl Pts',(-2.86515629953528,1.,-2.59318160184921));
#66193=CARTESIAN_POINT('Ctrl Pts',(-2.86081999003668,-1.,-2.5869677064356));
#66194=CARTESIAN_POINT('Ctrl Pts',(-2.86081999003668,1.,-2.5869677064356));
#66195=CARTESIAN_POINT('Ctrl Pts',(-2.85647171715147,-1.,-2.58082875254407));
#66196=CARTESIAN_POINT('Ctrl Pts',(-2.85647171715147,1.,-2.58082875254407));
#66197=CARTESIAN_POINT('Ctrl Pts',(-2.85215360144483,-1.,-2.57480482727128));
#66198=CARTESIAN_POINT('Ctrl Pts',(-2.85215360144483,1.,-2.57480482727128));
#66199=CARTESIAN_POINT('Ctrl Pts',(-2.84788893329091,-1.,-2.56891984251743));
#66200=CARTESIAN_POINT('Ctrl Pts',(-2.84788893329091,1.,-2.56891984251743));
#66201=CARTESIAN_POINT('Ctrl Pts',(-2.84366802680211,-1.,-2.56316920798489));
#66202=CARTESIAN_POINT('Ctrl Pts',(-2.84366802680211,1.,-2.56316920798489));
#66203=CARTESIAN_POINT('Ctrl Pts',(-2.83942515220699,-1.,-2.55749952145165));
#66204=CARTESIAN_POINT('Ctrl Pts',(-2.83942515220699,1.,-2.55749952145165));
#66205=CARTESIAN_POINT('Ctrl Pts',(-2.83505269592412,-1.,-2.55182152806964));
#66206=CARTESIAN_POINT('Ctrl Pts',(-2.83505269592412,1.,-2.55182152806964));
#66207=CARTESIAN_POINT('Ctrl Pts',(-2.83044254225794,-1.,-2.54604736792542));
#66208=CARTESIAN_POINT('Ctrl Pts',(-2.83044254225794,1.,-2.54604736792542));
#66209=CARTESIAN_POINT('Ctrl Pts',(-2.82552167649157,-1.,-2.54012272520141));
#66210=CARTESIAN_POINT('Ctrl Pts',(-2.82552167649157,1.,-2.54012272520141));
#66211=CARTESIAN_POINT('Ctrl Pts',(-2.82028550483744,-1.,-2.53405679667463));
#66212=CARTESIAN_POINT('Ctrl Pts',(-2.82028550483744,1.,-2.53405679667463));
#66213=CARTESIAN_POINT('Ctrl Pts',(-2.8148437904867,-1.,-2.52796388055457));
#66214=CARTESIAN_POINT('Ctrl Pts',(-2.8148437904867,1.,-2.52796388055457));
#66215=CARTESIAN_POINT('Ctrl Pts',(-2.80941521967234,-1.,-2.52205778589922));
#66216=CARTESIAN_POINT('Ctrl Pts',(-2.80941521967234,1.,-2.52205778589922));
#66217=CARTESIAN_POINT('Ctrl Pts',(-2.80427363984939,-1.,-2.51660190466067));
#66218=CARTESIAN_POINT('Ctrl Pts',(-2.80427363984939,1.,-2.51660190466067));
#66219=CARTESIAN_POINT('Ctrl Pts',(-2.79970585014308,-1.,-2.51186983687947));
#66220=CARTESIAN_POINT('Ctrl Pts',(-2.79970585014308,1.,-2.51186983687947));
#66221=CARTESIAN_POINT('Ctrl Pts',(-2.7959687805717,-1.,-2.50810555977564));
#66222=CARTESIAN_POINT('Ctrl Pts',(-2.7959687805717,1.,-2.50810555977564));
#66223=CARTESIAN_POINT('Ctrl Pts',(-2.79323694088143,-1.,-2.50547439929077));
#66224=CARTESIAN_POINT('Ctrl Pts',(-2.79323694088143,1.,-2.50547439929077));
#66225=CARTESIAN_POINT('Ctrl Pts',(-2.79192122906739,-1.,-2.50433799076945));
#66226=CARTESIAN_POINT('Ctrl Pts',(-2.79192122906739,1.,-2.50433799076945));
#66227=CARTESIAN_POINT('Ctrl Pts',(-2.79143626022225,-1.,-2.50404230339032));
#66228=CARTESIAN_POINT('Ctrl Pts',(-2.79143626022225,1.,-2.50404230339032));
#66229=CARTESIAN_POINT('Ctrl Pts',(-2.79133581100044,-1.,-2.50409239460011));
#66230=CARTESIAN_POINT('Ctrl Pts',(-2.79133581100044,1.,-2.50409239460011));
#66231=CARTESIAN_POINT('Ctrl Pts',(-2.79134130681569,-1.,-2.50417924854921));
#66232=CARTESIAN_POINT('Ctrl Pts',(-2.79134130681569,1.,-2.50417924854921));
#66233=CARTESIAN_POINT('',(-3.02314558451372,1.,-2.91557726271063));
#66234=CARTESIAN_POINT('Ctrl Pts',(-3.02314558451372,1.,-2.91557726271063));
#66235=CARTESIAN_POINT('Ctrl Pts',(-3.02261975104912,1.,-2.91409518070707));
#66236=CARTESIAN_POINT('Ctrl Pts',(-3.02156522743299,1.,-2.91113297349052));
#66237=CARTESIAN_POINT('Ctrl Pts',(-3.01997487194926,1.,-2.90669553303902));
#66238=CARTESIAN_POINT('Ctrl Pts',(-3.01783725123646,1.,-2.90079069102661));
#66239=CARTESIAN_POINT('Ctrl Pts',(-3.01513660433291,1.,-2.8934292556764));
#66240=CARTESIAN_POINT('Ctrl Pts',(-3.01240727309568,1.,-2.88608751706796));
#66241=CARTESIAN_POINT('Ctrl Pts',(-3.0096491810855,1.,-2.87876560072799));
#66242=CARTESIAN_POINT('Ctrl Pts',(-3.00686224485374,1.,-2.87146368430104));
#66243=CARTESIAN_POINT('Ctrl Pts',(-3.00404638316245,1.,-2.86418200833065));
#66244=CARTESIAN_POINT('Ctrl Pts',(-3.0012015079552,1.,-2.85692085715129));
#66245=CARTESIAN_POINT('Ctrl Pts',(-2.99832751144566,1.,-2.84968053289104));
#66246=CARTESIAN_POINT('Ctrl Pts',(-2.995424253416,1.,-2.84246132984334));
#66247=CARTESIAN_POINT('Ctrl Pts',(-2.99249155170479,1.,-2.83526351254383));
#66248=CARTESIAN_POINT('Ctrl Pts',(-2.98952916401699,1.,-2.82808728190402));
#66249=CARTESIAN_POINT('Ctrl Pts',(-2.98653680669434,1.,-2.82093279065704));
#66250=CARTESIAN_POINT('Ctrl Pts',(-2.9835141977994,1.,-2.81380019196454));
#66251=CARTESIAN_POINT('Ctrl Pts',(-2.98046109647299,1.,-2.80668968101162));
#66252=CARTESIAN_POINT('Ctrl Pts',(-2.97737733718242,1.,-2.79960153278186));
#66253=CARTESIAN_POINT('Ctrl Pts',(-2.97426288347475,1.,-2.79253615718147));
#66254=CARTESIAN_POINT('Ctrl Pts',(-2.97111781461349,1.,-2.78549409123657));
#66255=CARTESIAN_POINT('Ctrl Pts',(-2.9679422104295,1.,-2.77847589542767));
#66256=CARTESIAN_POINT('Ctrl Pts',(-2.96473605585548,1.,-2.77148206836464));
#66257=CARTESIAN_POINT('Ctrl Pts',(-2.96149914764832,1.,-2.76451296269571));
#66258=CARTESIAN_POINT('Ctrl Pts',(-2.9582309766594,1.,-2.75756867888393));
#66259=CARTESIAN_POINT('Ctrl Pts',(-2.95493069316211,1.,-2.75064903318996));
#66260=CARTESIAN_POINT('Ctrl Pts',(-2.95159737214305,1.,-2.7437537949221));
#66261=CARTESIAN_POINT('Ctrl Pts',(-2.94823023414381,1.,-2.73688288329825));
#66262=CARTESIAN_POINT('Ctrl Pts',(-2.94482887675139,1.,-2.73003657371613));
#66263=CARTESIAN_POINT('Ctrl Pts',(-2.94139351933882,1.,-2.72321571511322));
#66264=CARTESIAN_POINT('Ctrl Pts',(-2.93792519474955,1.,-2.71642190053575));
#66265=CARTESIAN_POINT('Ctrl Pts',(-2.93442516311168,1.,-2.70965695523776));
#66266=CARTESIAN_POINT('Ctrl Pts',(-2.93089438233746,1.,-2.70292247416881));
#66267=CARTESIAN_POINT('Ctrl Pts',(-2.92733294395268,1.,-2.69621932864302));
#66268=CARTESIAN_POINT('Ctrl Pts',(-2.92373955325876,1.,-2.68954721165342));
#66269=CARTESIAN_POINT('Ctrl Pts',(-2.92011090722152,1.,-2.68290409279689));
#66270=CARTESIAN_POINT('Ctrl Pts',(-2.91644290704281,1.,-2.67628728855309));
#66271=CARTESIAN_POINT('Ctrl Pts',(-2.91273193382876,1.,-2.66969458792627));
#66272=CARTESIAN_POINT('Ctrl Pts',(-2.90897617968921,1.,-2.66312542616808));
#66273=CARTESIAN_POINT('Ctrl Pts',(-2.90517678087467,1.,-2.65658188464287));
#66274=CARTESIAN_POINT('Ctrl Pts',(-2.90133950224879,1.,-2.65007017365576));
#66275=CARTESIAN_POINT('Ctrl Pts',(-2.89747231723361,1.,-2.64359851684146));
#66276=CARTESIAN_POINT('Ctrl Pts',(-2.89358228854557,1.,-2.63717442263944));
#66277=CARTESIAN_POINT('Ctrl Pts',(-2.88967244854243,1.,-2.63080195420771));
#66278=CARTESIAN_POINT('Ctrl Pts',(-2.88573922195049,1.,-2.62447947640253));
#66279=CARTESIAN_POINT('Ctrl Pts',(-2.88176821427502,1.,-2.61819596473087));
#66280=CARTESIAN_POINT('Ctrl Pts',(-2.87773881947885,1.,-2.61193507170928));
#66281=CARTESIAN_POINT('Ctrl Pts',(-2.87363176656475,1.,-2.6056817788128));
#66282=CARTESIAN_POINT('Ctrl Pts',(-2.86943633170712,1.,-2.59942875223202));
#66283=CARTESIAN_POINT('Ctrl Pts',(-2.86515629953528,1.,-2.59318160184921));
#66284=CARTESIAN_POINT('Ctrl Pts',(-2.86081999003668,1.,-2.5869677064356));
#66285=CARTESIAN_POINT('Ctrl Pts',(-2.85647171715147,1.,-2.58082875254407));
#66286=CARTESIAN_POINT('Ctrl Pts',(-2.85215360144483,1.,-2.57480482727128));
#66287=CARTESIAN_POINT('Ctrl Pts',(-2.84788893329091,1.,-2.56891984251743));
#66288=CARTESIAN_POINT('Ctrl Pts',(-2.84366802680211,1.,-2.56316920798489));
#66289=CARTESIAN_POINT('Ctrl Pts',(-2.83942515220699,1.,-2.55749952145165));
#66290=CARTESIAN_POINT('Ctrl Pts',(-2.83505269592412,1.,-2.55182152806964));
#66291=CARTESIAN_POINT('Ctrl Pts',(-2.83044254225794,1.,-2.54604736792542));
#66292=CARTESIAN_POINT('Ctrl Pts',(-2.82552167649157,1.,-2.54012272520141));
#66293=CARTESIAN_POINT('Ctrl Pts',(-2.82028550483744,1.,-2.53405679667463));
#66294=CARTESIAN_POINT('Ctrl Pts',(-2.8148437904867,1.,-2.52796388055457));
#66295=CARTESIAN_POINT('Ctrl Pts',(-2.80941521967234,1.,-2.52205778589922));
#66296=CARTESIAN_POINT('Ctrl Pts',(-2.80427363984939,1.,-2.51660190466067));
#66297=CARTESIAN_POINT('Ctrl Pts',(-2.79970585014308,1.,-2.51186983687947));
#66298=CARTESIAN_POINT('Ctrl Pts',(-2.7959687805717,1.,-2.50810555977564));
#66299=CARTESIAN_POINT('Ctrl Pts',(-2.79344192164204,1.,-2.50567182569153));
#66300=CARTESIAN_POINT('Ctrl Pts',(-2.79217568804874,1.,-2.50455968395235));
#66301=CARTESIAN_POINT('Ctrl Pts',(-2.79164172519039,1.,-2.50417932839344));
#66302=CARTESIAN_POINT('Ctrl Pts',(-2.79145823440899,1.,-2.50410700351427));
#66303=CARTESIAN_POINT('Ctrl Pts',(-2.79140942341378,1.,-2.50410331873043));
#66304=CARTESIAN_POINT('',(-3.02314558451372,0.,-2.91557726271063));
#66305=CARTESIAN_POINT('Ctrl Pts',(-2.50417924854921,-1.,-2.79134130681569));
#66306=CARTESIAN_POINT('Ctrl Pts',(-2.50417924854921,1.,-2.79134130681569));
#66307=CARTESIAN_POINT('Ctrl Pts',(-2.50409239460108,-1.,-2.7913358110015));
#66308=CARTESIAN_POINT('Ctrl Pts',(-2.50409239460108,1.,-2.7913358110015));
#66309=CARTESIAN_POINT('Ctrl Pts',(-2.50404230339286,-1.,-2.79143626022503));
#66310=CARTESIAN_POINT('Ctrl Pts',(-2.50404230339286,1.,-2.79143626022503));
#66311=CARTESIAN_POINT('Ctrl Pts',(-2.5043379907732,-1.,-2.79192122907148));
#66312=CARTESIAN_POINT('Ctrl Pts',(-2.5043379907732,1.,-2.79192122907148));
#66313=CARTESIAN_POINT('Ctrl Pts',(-2.50547439929414,-1.,-2.7932369408851));
#66314=CARTESIAN_POINT('Ctrl Pts',(-2.50547439929414,1.,-2.7932369408851));
#66315=CARTESIAN_POINT('Ctrl Pts',(-2.50810555977671,-1.,-2.79596878057287));
#66316=CARTESIAN_POINT('Ctrl Pts',(-2.50810555977671,1.,-2.79596878057287));
#66317=CARTESIAN_POINT('Ctrl Pts',(-2.51186983687818,-1.,-2.79970585014168));
#66318=CARTESIAN_POINT('Ctrl Pts',(-2.51186983687818,1.,-2.79970585014168));
#66319=CARTESIAN_POINT('Ctrl Pts',(-2.51660190465805,-1.,-2.80427363984653));
#66320=CARTESIAN_POINT('Ctrl Pts',(-2.51660190465805,1.,-2.80427363984653));
#66321=CARTESIAN_POINT('Ctrl Pts',(-2.52205778589653,-1.,-2.80941521966941));
#66322=CARTESIAN_POINT('Ctrl Pts',(-2.52205778589653,1.,-2.80941521966941));
#66323=CARTESIAN_POINT('Ctrl Pts',(-2.52796388055278,-1.,-2.81484379048475));
#66324=CARTESIAN_POINT('Ctrl Pts',(-2.52796388055278,1.,-2.81484379048475));
#66325=CARTESIAN_POINT('Ctrl Pts',(-2.53405679667412,-1.,-2.82028550483689));
#66326=CARTESIAN_POINT('Ctrl Pts',(-2.53405679667412,1.,-2.82028550483689));
#66327=CARTESIAN_POINT('Ctrl Pts',(-2.54012272520199,-1.,-2.8255216764922));
#66328=CARTESIAN_POINT('Ctrl Pts',(-2.54012272520199,1.,-2.8255216764922));
#66329=CARTESIAN_POINT('Ctrl Pts',(-2.54604736792655,-1.,-2.83044254225917));
#66330=CARTESIAN_POINT('Ctrl Pts',(-2.54604736792655,1.,-2.83044254225917));
#66331=CARTESIAN_POINT('Ctrl Pts',(-2.55182152807077,-1.,-2.83505269592536));
#66332=CARTESIAN_POINT('Ctrl Pts',(-2.55182152807077,1.,-2.83505269592536));
#66333=CARTESIAN_POINT('Ctrl Pts',(-2.55749952145241,-1.,-2.83942515220782));
#66334=CARTESIAN_POINT('Ctrl Pts',(-2.55749952145241,1.,-2.83942515220782));
#66335=CARTESIAN_POINT('Ctrl Pts',(-2.56316920798513,-1.,-2.84366802680237));
#66336=CARTESIAN_POINT('Ctrl Pts',(-2.56316920798513,1.,-2.84366802680237));
#66337=CARTESIAN_POINT('Ctrl Pts',(-2.56891984251721,-1.,-2.84788893329067));
#66338=CARTESIAN_POINT('Ctrl Pts',(-2.56891984251721,1.,-2.84788893329067));
#66339=CARTESIAN_POINT('Ctrl Pts',(-2.57480482727081,-1.,-2.85215360144431));
#66340=CARTESIAN_POINT('Ctrl Pts',(-2.57480482727081,1.,-2.85215360144431));
#66341=CARTESIAN_POINT('Ctrl Pts',(-2.58082875254357,-1.,-2.85647171715092));
#66342=CARTESIAN_POINT('Ctrl Pts',(-2.58082875254357,1.,-2.85647171715092));
#66343=CARTESIAN_POINT('Ctrl Pts',(-2.58696770643524,-1.,-2.86081999003629));
#66344=CARTESIAN_POINT('Ctrl Pts',(-2.58696770643524,1.,-2.86081999003629));
#66345=CARTESIAN_POINT('Ctrl Pts',(-2.59318160184908,-1.,-2.86515629953513));
#66346=CARTESIAN_POINT('Ctrl Pts',(-2.59318160184908,1.,-2.86515629953513));
#66347=CARTESIAN_POINT('Ctrl Pts',(-2.5994287522321,-1.,-2.86943633170722));
#66348=CARTESIAN_POINT('Ctrl Pts',(-2.5994287522321,1.,-2.86943633170722));
#66349=CARTESIAN_POINT('Ctrl Pts',(-2.60568177881303,-1.,-2.87363176656501));
#66350=CARTESIAN_POINT('Ctrl Pts',(-2.60568177881303,1.,-2.87363176656501));
#66351=CARTESIAN_POINT('Ctrl Pts',(-2.61193507170955,-1.,-2.87773881947915));
#66352=CARTESIAN_POINT('Ctrl Pts',(-2.61193507170955,1.,-2.87773881947915));
#66353=CARTESIAN_POINT('Ctrl Pts',(-2.61819596473108,-1.,-2.88176821427525));
#66354=CARTESIAN_POINT('Ctrl Pts',(-2.61819596473108,1.,-2.88176821427525));
#66355=CARTESIAN_POINT('Ctrl Pts',(-2.62447947640262,-1.,-2.88573922195059));
#66356=CARTESIAN_POINT('Ctrl Pts',(-2.62447947640262,1.,-2.88573922195059));
#66357=CARTESIAN_POINT('Ctrl Pts',(-2.63080195420767,-1.,-2.88967244854239));
#66358=CARTESIAN_POINT('Ctrl Pts',(-2.63080195420767,1.,-2.88967244854239));
#66359=CARTESIAN_POINT('Ctrl Pts',(-2.63717442263932,-1.,-2.89358228854544));
#66360=CARTESIAN_POINT('Ctrl Pts',(-2.63717442263932,1.,-2.89358228854544));
#66361=CARTESIAN_POINT('Ctrl Pts',(-2.64359851684131,-1.,-2.89747231723345));
#66362=CARTESIAN_POINT('Ctrl Pts',(-2.64359851684131,1.,-2.89747231723345));
#66363=CARTESIAN_POINT('Ctrl Pts',(-2.65007017365564,-1.,-2.90133950224867));
#66364=CARTESIAN_POINT('Ctrl Pts',(-2.65007017365564,1.,-2.90133950224867));
#66365=CARTESIAN_POINT('Ctrl Pts',(-2.65658188464282,-1.,-2.90517678087461));
#66366=CARTESIAN_POINT('Ctrl Pts',(-2.65658188464282,1.,-2.90517678087461));
#66367=CARTESIAN_POINT('Ctrl Pts',(-2.6631254261681,-1.,-2.90897617968923));
#66368=CARTESIAN_POINT('Ctrl Pts',(-2.6631254261681,1.,-2.90897617968923));
#66369=CARTESIAN_POINT('Ctrl Pts',(-2.66969458792631,-1.,-2.91273193382882));
#66370=CARTESIAN_POINT('Ctrl Pts',(-2.66969458792631,1.,-2.91273193382882));
#66371=CARTESIAN_POINT('Ctrl Pts',(-2.67628728855312,-1.,-2.91644290704285));
#66372=CARTESIAN_POINT('Ctrl Pts',(-2.67628728855312,1.,-2.91644290704285));
#66373=CARTESIAN_POINT('Ctrl Pts',(-2.68290409279688,-1.,-2.92011090722152));
#66374=CARTESIAN_POINT('Ctrl Pts',(-2.68290409279688,1.,-2.92011090722152));
#66375=CARTESIAN_POINT('Ctrl Pts',(-2.68954721165339,-1.,-2.92373955325875));
#66376=CARTESIAN_POINT('Ctrl Pts',(-2.68954721165339,1.,-2.92373955325875));
#66377=CARTESIAN_POINT('Ctrl Pts',(-2.69621932864301,-1.,-2.92733294395267));
#66378=CARTESIAN_POINT('Ctrl Pts',(-2.69621932864301,1.,-2.92733294395267));
#66379=CARTESIAN_POINT('Ctrl Pts',(-2.70292247416885,-1.,-2.93089438233749));
#66380=CARTESIAN_POINT('Ctrl Pts',(-2.70292247416885,1.,-2.93089438233749));
#66381=CARTESIAN_POINT('Ctrl Pts',(-2.70965695523787,-1.,-2.93442516311179));
#66382=CARTESIAN_POINT('Ctrl Pts',(-2.70965695523787,1.,-2.93442516311179));
#66383=CARTESIAN_POINT('Ctrl Pts',(-2.71642190053592,-1.,-2.93792519474972));
#66384=CARTESIAN_POINT('Ctrl Pts',(-2.71642190053592,1.,-2.93792519474972));
#66385=CARTESIAN_POINT('Ctrl Pts',(-2.72321571511337,-1.,-2.94139351933897));
#66386=CARTESIAN_POINT('Ctrl Pts',(-2.72321571511337,1.,-2.94139351933897));
#66387=CARTESIAN_POINT('Ctrl Pts',(-2.73003657371617,-1.,-2.94482887675143));
#66388=CARTESIAN_POINT('Ctrl Pts',(-2.73003657371617,1.,-2.94482887675143));
#66389=CARTESIAN_POINT('Ctrl Pts',(-2.73688288329808,-1.,-2.94823023414364));
#66390=CARTESIAN_POINT('Ctrl Pts',(-2.73688288329808,1.,-2.94823023414364));
#66391=CARTESIAN_POINT('Ctrl Pts',(-2.74375379492172,-1.,-2.95159737214266));
#66392=CARTESIAN_POINT('Ctrl Pts',(-2.74375379492172,1.,-2.95159737214266));
#66393=CARTESIAN_POINT('Ctrl Pts',(-2.75064903318947,-1.,-2.95493069316161));
#66394=CARTESIAN_POINT('Ctrl Pts',(-2.75064903318947,1.,-2.95493069316161));
#66395=CARTESIAN_POINT('Ctrl Pts',(-2.7575686788835,-1.,-2.95823097665896));
#66396=CARTESIAN_POINT('Ctrl Pts',(-2.7575686788835,1.,-2.95823097665896));
#66397=CARTESIAN_POINT('Ctrl Pts',(-2.76451296269557,-1.,-2.96149914764818));
#66398=CARTESIAN_POINT('Ctrl Pts',(-2.76451296269557,1.,-2.96149914764818));
#66399=CARTESIAN_POINT('Ctrl Pts',(-2.77148206836498,-1.,-2.96473605585583));
#66400=CARTESIAN_POINT('Ctrl Pts',(-2.77148206836498,1.,-2.96473605585583));
#66401=CARTESIAN_POINT('Ctrl Pts',(-2.7784758954285,-1.,-2.96794221043036));
#66402=CARTESIAN_POINT('Ctrl Pts',(-2.7784758954285,1.,-2.96794221043036));
#66403=CARTESIAN_POINT('Ctrl Pts',(-2.78549409123769,-1.,-2.97111781461465));
#66404=CARTESIAN_POINT('Ctrl Pts',(-2.78549409123769,1.,-2.97111781461465));
#66405=CARTESIAN_POINT('Ctrl Pts',(-2.79253615718248,-1.,-2.9742628834758));
#66406=CARTESIAN_POINT('Ctrl Pts',(-2.79253615718248,1.,-2.9742628834758));
#66407=CARTESIAN_POINT('Ctrl Pts',(-2.7996015327823,-1.,-2.97737733718287));
#66408=CARTESIAN_POINT('Ctrl Pts',(-2.7996015327823,1.,-2.97737733718287));
#66409=CARTESIAN_POINT('Ctrl Pts',(-2.80668968101106,-1.,-2.98046109647241));
#66410=CARTESIAN_POINT('Ctrl Pts',(-2.80668968101106,1.,-2.98046109647241));
#66411=CARTESIAN_POINT('Ctrl Pts',(-2.81380019196286,-1.,-2.98351419779767));
#66412=CARTESIAN_POINT('Ctrl Pts',(-2.81380019196286,1.,-2.98351419779767));
#66413=CARTESIAN_POINT('Ctrl Pts',(-2.82093279065457,-1.,-2.9865368066918));
#66414=CARTESIAN_POINT('Ctrl Pts',(-2.82093279065457,1.,-2.9865368066918));
#66415=CARTESIAN_POINT('Ctrl Pts',(-2.82808728190157,-1.,-2.98952916401446));
#66416=CARTESIAN_POINT('Ctrl Pts',(-2.82808728190157,1.,-2.98952916401446));
#66417=CARTESIAN_POINT('Ctrl Pts',(-2.83526351254248,-1.,-2.99249155170339));
#66418=CARTESIAN_POINT('Ctrl Pts',(-2.83526351254248,1.,-2.99249155170339));
#66419=CARTESIAN_POINT('Ctrl Pts',(-2.84246132984415,-1.,-2.99542425341685));
#66420=CARTESIAN_POINT('Ctrl Pts',(-2.84246132984415,1.,-2.99542425341685));
#66421=CARTESIAN_POINT('Ctrl Pts',(-2.84968053289451,-1.,-2.99832751144925));
#66422=CARTESIAN_POINT('Ctrl Pts',(-2.84968053289451,1.,-2.99832751144925));
#66423=CARTESIAN_POINT('Ctrl Pts',(-2.85692085715686,-1.,-3.00120150796095));
#66424=CARTESIAN_POINT('Ctrl Pts',(-2.85692085715686,1.,-3.00120150796095));
#66425=CARTESIAN_POINT('Ctrl Pts',(-2.86418200833667,-1.,-3.00404638316867));
#66426=CARTESIAN_POINT('Ctrl Pts',(-2.86418200833667,1.,-3.00404638316867));
#66427=CARTESIAN_POINT('Ctrl Pts',(-2.87146368430502,-1.,-3.00686224485784));
#66428=CARTESIAN_POINT('Ctrl Pts',(-2.87146368430502,1.,-3.00686224485784));
#66429=CARTESIAN_POINT('Ctrl Pts',(-2.87876560072727,-1.,-3.00964918108476));
#66430=CARTESIAN_POINT('Ctrl Pts',(-2.87876560072727,1.,-3.00964918108476));
#66431=CARTESIAN_POINT('Ctrl Pts',(-2.8860875170608,-1.,-3.01240727308829));
#66432=CARTESIAN_POINT('Ctrl Pts',(-2.8860875170608,1.,-3.01240727308829));
#66433=CARTESIAN_POINT('Ctrl Pts',(-2.89342925566321,-1.,-3.01513660431928));
#66434=CARTESIAN_POINT('Ctrl Pts',(-2.89342925566321,1.,-3.01513660431928));
#66435=CARTESIAN_POINT('Ctrl Pts',(-2.9007906910105,-1.,-3.01783725121981));
#66436=CARTESIAN_POINT('Ctrl Pts',(-2.9007906910105,1.,-3.01783725121981));
#66437=CARTESIAN_POINT('Ctrl Pts',(-2.90669553302526,-1.,-3.01997487193503));
#66438=CARTESIAN_POINT('Ctrl Pts',(-2.90669553302526,1.,-3.01997487193503));
#66439=CARTESIAN_POINT('Ctrl Pts',(-2.91113297348212,-1.,-3.02156522742431));
#66440=CARTESIAN_POINT('Ctrl Pts',(-2.91113297348212,1.,-3.02156522742431));
#66441=CARTESIAN_POINT('Ctrl Pts',(-2.91409518070399,-1.,-3.02261975104593));
#66442=CARTESIAN_POINT('Ctrl Pts',(-2.91409518070399,1.,-3.02261975104593));
#66443=CARTESIAN_POINT('Ctrl Pts',(-2.91557726271063,-1.,-3.02314558451372));
#66444=CARTESIAN_POINT('Ctrl Pts',(-2.91557726271063,1.,-3.02314558451372));
#66445=CARTESIAN_POINT('',(-2.50410331873176,1.,-2.79140942341258));
#66446=CARTESIAN_POINT('Ctrl Pts',(-2.50410331873176,-1.,-2.79140942341258));
#66447=CARTESIAN_POINT('Ctrl Pts',(-2.50410331873176,-0.666666666666667,
-2.79140942341258));
#66448=CARTESIAN_POINT('Ctrl Pts',(-2.50410331873176,-0.333333333333333,
-2.79140942341258));
#66449=CARTESIAN_POINT('Ctrl Pts',(-2.50410331873176,0.333333333333333,
-2.79140942341258));
#66450=CARTESIAN_POINT('Ctrl Pts',(-2.50410331873176,0.666666666666667,
-2.79140942341258));
#66451=CARTESIAN_POINT('Ctrl Pts',(-2.50410331873176,1.,-2.79140942341258));
#66452=CARTESIAN_POINT('',(-2.91557726271063,1.,-3.02314558451372));
#66453=CARTESIAN_POINT('',(-2.91557726271063,0.,-3.02314558451372));
#66454=CARTESIAN_POINT('Ctrl Pts',(-2.50410331873176,1.,-2.79140942341258));
#66455=CARTESIAN_POINT('Ctrl Pts',(-2.50410700351493,1.,-2.79145823440781));
#66456=CARTESIAN_POINT('Ctrl Pts',(-2.50417932839313,1.,-2.79164172518905));
#66457=CARTESIAN_POINT('Ctrl Pts',(-2.50455968395146,1.,-2.79217568804755));
#66458=CARTESIAN_POINT('Ctrl Pts',(-2.50567182569081,1.,-2.79344192164147));
#66459=CARTESIAN_POINT('Ctrl Pts',(-2.50810555977671,1.,-2.79596878057287));
#66460=CARTESIAN_POINT('Ctrl Pts',(-2.51186983687818,1.,-2.79970585014168));
#66461=CARTESIAN_POINT('Ctrl Pts',(-2.51660190465805,1.,-2.80427363984653));
#66462=CARTESIAN_POINT('Ctrl Pts',(-2.52205778589653,1.,-2.80941521966941));
#66463=CARTESIAN_POINT('Ctrl Pts',(-2.52796388055278,1.,-2.81484379048475));
#66464=CARTESIAN_POINT('Ctrl Pts',(-2.53405679667412,1.,-2.82028550483689));
#66465=CARTESIAN_POINT('Ctrl Pts',(-2.54012272520199,1.,-2.8255216764922));
#66466=CARTESIAN_POINT('Ctrl Pts',(-2.54604736792655,1.,-2.83044254225917));
#66467=CARTESIAN_POINT('Ctrl Pts',(-2.55182152807077,1.,-2.83505269592536));
#66468=CARTESIAN_POINT('Ctrl Pts',(-2.55749952145241,1.,-2.83942515220782));
#66469=CARTESIAN_POINT('Ctrl Pts',(-2.56316920798513,1.,-2.84366802680237));
#66470=CARTESIAN_POINT('Ctrl Pts',(-2.56891984251721,1.,-2.84788893329067));
#66471=CARTESIAN_POINT('Ctrl Pts',(-2.57480482727081,1.,-2.85215360144431));
#66472=CARTESIAN_POINT('Ctrl Pts',(-2.58082875254357,1.,-2.85647171715092));
#66473=CARTESIAN_POINT('Ctrl Pts',(-2.58696770643524,1.,-2.86081999003629));
#66474=CARTESIAN_POINT('Ctrl Pts',(-2.59318160184908,1.,-2.86515629953513));
#66475=CARTESIAN_POINT('Ctrl Pts',(-2.5994287522321,1.,-2.86943633170722));
#66476=CARTESIAN_POINT('Ctrl Pts',(-2.60568177881303,1.,-2.87363176656501));
#66477=CARTESIAN_POINT('Ctrl Pts',(-2.61193507170955,1.,-2.87773881947915));
#66478=CARTESIAN_POINT('Ctrl Pts',(-2.61819596473108,1.,-2.88176821427525));
#66479=CARTESIAN_POINT('Ctrl Pts',(-2.62447947640262,1.,-2.88573922195059));
#66480=CARTESIAN_POINT('Ctrl Pts',(-2.63080195420767,1.,-2.88967244854239));
#66481=CARTESIAN_POINT('Ctrl Pts',(-2.63717442263932,1.,-2.89358228854544));
#66482=CARTESIAN_POINT('Ctrl Pts',(-2.64359851684131,1.,-2.89747231723345));
#66483=CARTESIAN_POINT('Ctrl Pts',(-2.65007017365564,1.,-2.90133950224867));
#66484=CARTESIAN_POINT('Ctrl Pts',(-2.65658188464282,1.,-2.90517678087461));
#66485=CARTESIAN_POINT('Ctrl Pts',(-2.6631254261681,1.,-2.90897617968923));
#66486=CARTESIAN_POINT('Ctrl Pts',(-2.66969458792631,1.,-2.91273193382882));
#66487=CARTESIAN_POINT('Ctrl Pts',(-2.67628728855312,1.,-2.91644290704285));
#66488=CARTESIAN_POINT('Ctrl Pts',(-2.68290409279688,1.,-2.92011090722152));
#66489=CARTESIAN_POINT('Ctrl Pts',(-2.68954721165339,1.,-2.92373955325875));
#66490=CARTESIAN_POINT('Ctrl Pts',(-2.69621932864301,1.,-2.92733294395267));
#66491=CARTESIAN_POINT('Ctrl Pts',(-2.70292247416885,1.,-2.93089438233749));
#66492=CARTESIAN_POINT('Ctrl Pts',(-2.70965695523787,1.,-2.93442516311179));
#66493=CARTESIAN_POINT('Ctrl Pts',(-2.71642190053592,1.,-2.93792519474972));
#66494=CARTESIAN_POINT('Ctrl Pts',(-2.72321571511337,1.,-2.94139351933897));
#66495=CARTESIAN_POINT('Ctrl Pts',(-2.73003657371617,1.,-2.94482887675143));
#66496=CARTESIAN_POINT('Ctrl Pts',(-2.73688288329808,1.,-2.94823023414364));
#66497=CARTESIAN_POINT('Ctrl Pts',(-2.74375379492172,1.,-2.95159737214266));
#66498=CARTESIAN_POINT('Ctrl Pts',(-2.75064903318947,1.,-2.95493069316161));
#66499=CARTESIAN_POINT('Ctrl Pts',(-2.7575686788835,1.,-2.95823097665896));
#66500=CARTESIAN_POINT('Ctrl Pts',(-2.76451296269557,1.,-2.96149914764818));
#66501=CARTESIAN_POINT('Ctrl Pts',(-2.77148206836498,1.,-2.96473605585583));
#66502=CARTESIAN_POINT('Ctrl Pts',(-2.7784758954285,1.,-2.96794221043036));
#66503=CARTESIAN_POINT('Ctrl Pts',(-2.78549409123769,1.,-2.97111781461465));
#66504=CARTESIAN_POINT('Ctrl Pts',(-2.79253615718248,1.,-2.9742628834758));
#66505=CARTESIAN_POINT('Ctrl Pts',(-2.7996015327823,1.,-2.97737733718287));
#66506=CARTESIAN_POINT('Ctrl Pts',(-2.80668968101106,1.,-2.98046109647241));
#66507=CARTESIAN_POINT('Ctrl Pts',(-2.81380019196286,1.,-2.98351419779767));
#66508=CARTESIAN_POINT('Ctrl Pts',(-2.82093279065457,1.,-2.9865368066918));
#66509=CARTESIAN_POINT('Ctrl Pts',(-2.82808728190157,1.,-2.98952916401446));
#66510=CARTESIAN_POINT('Ctrl Pts',(-2.83526351254248,1.,-2.99249155170339));
#66511=CARTESIAN_POINT('Ctrl Pts',(-2.84246132984415,1.,-2.99542425341685));
#66512=CARTESIAN_POINT('Ctrl Pts',(-2.84968053289451,1.,-2.99832751144925));
#66513=CARTESIAN_POINT('Ctrl Pts',(-2.85692085715686,1.,-3.00120150796095));
#66514=CARTESIAN_POINT('Ctrl Pts',(-2.86418200833667,1.,-3.00404638316867));
#66515=CARTESIAN_POINT('Ctrl Pts',(-2.87146368430502,1.,-3.00686224485784));
#66516=CARTESIAN_POINT('Ctrl Pts',(-2.87876560072727,1.,-3.00964918108476));
#66517=CARTESIAN_POINT('Ctrl Pts',(-2.8860875170608,1.,-3.01240727308829));
#66518=CARTESIAN_POINT('Ctrl Pts',(-2.89342925566321,1.,-3.01513660431928));
#66519=CARTESIAN_POINT('Ctrl Pts',(-2.9007906910105,1.,-3.01783725121981));
#66520=CARTESIAN_POINT('Ctrl Pts',(-2.90669553302526,1.,-3.01997487193503));
#66521=CARTESIAN_POINT('Ctrl Pts',(-2.91113297348212,1.,-3.02156522742431));
#66522=CARTESIAN_POINT('Ctrl Pts',(-2.91409518070399,1.,-3.02261975104593));
#66523=CARTESIAN_POINT('Ctrl Pts',(-2.91557726271063,1.,-3.02314558451372));
#66524=CARTESIAN_POINT('Origin',(-2.91557726271063,0.,-3.02314558451372));
#66525=CARTESIAN_POINT('',(-3.02314558451372,1.,-2.91557726271063));
#66526=CARTESIAN_POINT('Origin',(0.,0.,0.));
#66527=CARTESIAN_POINT('',(-2.36531447826213,1.,-2.90994629141562));
#66528=CARTESIAN_POINT('Origin',(0.,1.,0.));
#66529=CARTESIAN_POINT('Ctrl Pts',(-2.36531447826213,1.,-2.90994629141562));
#66530=CARTESIAN_POINT('Ctrl Pts',(-2.36531447826213,0.666666666666667,
-2.90994629141562));
#66531=CARTESIAN_POINT('Ctrl Pts',(-2.36531447826213,0.333333333333333,
-2.90994629141562));
#66532=CARTESIAN_POINT('Ctrl Pts',(-2.36531447826213,-0.333333333333333,
-2.90994629141562));
#66533=CARTESIAN_POINT('Ctrl Pts',(-2.36531447826213,-0.666666666666667,
-2.90994629141562));
#66534=CARTESIAN_POINT('Ctrl Pts',(-2.36531447826213,-1.,-2.90994629141562));
#66535=CARTESIAN_POINT('Ctrl Pts',(-2.52982887637028,-1.,-3.35260583073571));
#66536=CARTESIAN_POINT('Ctrl Pts',(-2.52982887637028,1.,-3.35260583073571));
#66537=CARTESIAN_POINT('Ctrl Pts',(-2.52954136549357,-1.,-3.35105973714426));
#66538=CARTESIAN_POINT('Ctrl Pts',(-2.52954136549357,1.,-3.35105973714426));
#66539=CARTESIAN_POINT('Ctrl Pts',(-2.5289632161143,-1.,-3.34796903577628));
#66540=CARTESIAN_POINT('Ctrl Pts',(-2.5289632161143,1.,-3.34796903577628));
#66541=CARTESIAN_POINT('Ctrl Pts',(-2.52808660916879,-1.,-3.34333744117093));
#66542=CARTESIAN_POINT('Ctrl Pts',(-2.52808660916879,1.,-3.34333744117093));
#66543=CARTESIAN_POINT('Ctrl Pts',(-2.52689902691551,-1.,-3.33717090000955));
#66544=CARTESIAN_POINT('Ctrl Pts',(-2.52689902691551,1.,-3.33717090000955));
#66545=CARTESIAN_POINT('Ctrl Pts',(-2.52538321165774,-1.,-3.32947762189049));
#66546=CARTESIAN_POINT('Ctrl Pts',(-2.52538321165774,1.,-3.32947762189049));
#66547=CARTESIAN_POINT('Ctrl Pts',(-2.52383598396878,-1.,-3.32179931079521));
#66548=CARTESIAN_POINT('Ctrl Pts',(-2.52383598396878,1.,-3.32179931079521));
#66549=CARTESIAN_POINT('Ctrl Pts',(-2.52225724871375,-1.,-3.31413607874727));
#66550=CARTESIAN_POINT('Ctrl Pts',(-2.52225724871375,1.,-3.31413607874727));
#66551=CARTESIAN_POINT('Ctrl Pts',(-2.52064689568167,-1.,-3.30648808814986));
#66552=CARTESIAN_POINT('Ctrl Pts',(-2.52064689568167,1.,-3.30648808814986));
#66553=CARTESIAN_POINT('Ctrl Pts',(-2.51900480700548,-1.,-3.29885556387661));
#66554=CARTESIAN_POINT('Ctrl Pts',(-2.51900480700548,1.,-3.29885556387661));
#66555=CARTESIAN_POINT('Ctrl Pts',(-2.51733085123316,-1.,-3.2912387729863));
#66556=CARTESIAN_POINT('Ctrl Pts',(-2.51733085123316,1.,-3.2912387729863));
#66557=CARTESIAN_POINT('Ctrl Pts',(-2.51562487464215,-1.,-3.28363799702583));
#66558=CARTESIAN_POINT('Ctrl Pts',(-2.51562487464215,1.,-3.28363799702583));
#66559=CARTESIAN_POINT('Ctrl Pts',(-2.51388669270329,-1.,-3.27605350473048));
#66560=CARTESIAN_POINT('Ctrl Pts',(-2.51388669270329,1.,-3.27605350473048));
#66561=CARTESIAN_POINT('Ctrl Pts',(-2.51211608411539,-1.,-3.26848552888271));
#66562=CARTESIAN_POINT('Ctrl Pts',(-2.51211608411539,1.,-3.26848552888271));
#66563=CARTESIAN_POINT('Ctrl Pts',(-2.51031277813697,-1.,-3.26093423001716));
#66564=CARTESIAN_POINT('Ctrl Pts',(-2.51031277813697,1.,-3.26093423001716));
#66565=CARTESIAN_POINT('Ctrl Pts',(-2.50847647070936,-1.,-3.25339971461265));
#66566=CARTESIAN_POINT('Ctrl Pts',(-2.50847647070936,1.,-3.25339971461265));
#66567=CARTESIAN_POINT('Ctrl Pts',(-2.50660685940645,-1.,-3.24588208984042));
#66568=CARTESIAN_POINT('Ctrl Pts',(-2.50660685940645,1.,-3.24588208984042));
#66569=CARTESIAN_POINT('Ctrl Pts',(-2.50470367580078,-1.,-3.23838151080383));
#66570=CARTESIAN_POINT('Ctrl Pts',(-2.50470367580078,1.,-3.23838151080383));
#66571=CARTESIAN_POINT('Ctrl Pts',(-2.50276671338074,-1.,-3.23089822320596));
#66572=CARTESIAN_POINT('Ctrl Pts',(-2.50276671338074,1.,-3.23089822320596));
#66573=CARTESIAN_POINT('Ctrl Pts',(-2.5007958720187,-1.,-3.22343262620387));
#66574=CARTESIAN_POINT('Ctrl Pts',(-2.5007958720187,1.,-3.22343262620387));
#66575=CARTESIAN_POINT('Ctrl Pts',(-2.49879114599293,-1.,-3.21598526261157));
#66576=CARTESIAN_POINT('Ctrl Pts',(-2.49879114599293,1.,-3.21598526261157));
#66577=CARTESIAN_POINT('Ctrl Pts',(-2.49675252647298,-1.,-3.2085566984974));
#66578=CARTESIAN_POINT('Ctrl Pts',(-2.49675252647298,1.,-3.2085566984974));
#66579=CARTESIAN_POINT('Ctrl Pts',(-2.49467992057726,-1.,-3.20114742397549));
#66580=CARTESIAN_POINT('Ctrl Pts',(-2.49467992057726,1.,-3.20114742397549));
#66581=CARTESIAN_POINT('Ctrl Pts',(-2.4925730723986,-1.,-3.19375775555814));
#66582=CARTESIAN_POINT('Ctrl Pts',(-2.4925730723986,1.,-3.19375775555814));
#66583=CARTESIAN_POINT('Ctrl Pts',(-2.49043146334095,-1.,-3.18638771282315));
#66584=CARTESIAN_POINT('Ctrl Pts',(-2.49043146334095,1.,-3.18638771282315));
#66585=CARTESIAN_POINT('Ctrl Pts',(-2.48825428288243,-1.,-3.17903698136679));
#66586=CARTESIAN_POINT('Ctrl Pts',(-2.48825428288243,1.,-3.17903698136679));
#66587=CARTESIAN_POINT('Ctrl Pts',(-2.48604065348619,-1.,-3.17170518863357));
#66588=CARTESIAN_POINT('Ctrl Pts',(-2.48604065348619,1.,-3.17170518863357));
#66589=CARTESIAN_POINT('Ctrl Pts',(-2.48378981792739,-1.,-3.16439213290181));
#66590=CARTESIAN_POINT('Ctrl Pts',(-2.48378981792739,1.,-3.16439213290181));
#66591=CARTESIAN_POINT('Ctrl Pts',(-2.48150133566568,-1.,-3.15709802322735));
#66592=CARTESIAN_POINT('Ctrl Pts',(-2.48150133566568,1.,-3.15709802322735));
#66593=CARTESIAN_POINT('Ctrl Pts',(-2.47917529057016,-1.,-3.14982373241335));
#66594=CARTESIAN_POINT('Ctrl Pts',(-2.47917529057016,1.,-3.14982373241335));
#66595=CARTESIAN_POINT('Ctrl Pts',(-2.47681245356095,-1.,-3.14257099546531));
#66596=CARTESIAN_POINT('Ctrl Pts',(-2.47681245356095,1.,-3.14257099546531));
#66597=CARTESIAN_POINT('Ctrl Pts',(-2.47441378371923,-1.,-3.13534181229282));
#66598=CARTESIAN_POINT('Ctrl Pts',(-2.47441378371923,1.,-3.13534181229282));
#66599=CARTESIAN_POINT('Ctrl Pts',(-2.47197997765868,-1.,-3.12813790805948));
#66600=CARTESIAN_POINT('Ctrl Pts',(-2.47197997765868,1.,-3.12813790805948));
#66601=CARTESIAN_POINT('Ctrl Pts',(-2.4695109894747,-1.,-3.12096015766984));
#66602=CARTESIAN_POINT('Ctrl Pts',(-2.4695109894747,1.,-3.12096015766984));
#66603=CARTESIAN_POINT('Ctrl Pts',(-2.46700558843507,-1.,-3.11380805536124));
#66604=CARTESIAN_POINT('Ctrl Pts',(-2.46700558843507,1.,-3.11380805536124));
#66605=CARTESIAN_POINT('Ctrl Pts',(-2.46446082979645,-1.,-3.10667907901981));
#66606=CARTESIAN_POINT('Ctrl Pts',(-2.46446082979645,1.,-3.10667907901981));
#66607=CARTESIAN_POINT('Ctrl Pts',(-2.4618730850188,-1.,-3.09956993697048));
#66608=CARTESIAN_POINT('Ctrl Pts',(-2.4618730850188,1.,-3.09956993697048));
#66609=CARTESIAN_POINT('Ctrl Pts',(-2.45923912563875,-1.,-3.09247787931881));
#66610=CARTESIAN_POINT('Ctrl Pts',(-2.45923912563875,1.,-3.09247787931881));
#66611=CARTESIAN_POINT('Ctrl Pts',(-2.45655725437037,-1.,-3.08540206545313));
#66612=CARTESIAN_POINT('Ctrl Pts',(-2.45655725437037,1.,-3.08540206545313));
#66613=CARTESIAN_POINT('Ctrl Pts',(-2.45382826787795,-1.,-3.07834472886145));
#66614=CARTESIAN_POINT('Ctrl Pts',(-2.45382826787795,1.,-3.07834472886145));
#66615=CARTESIAN_POINT('Ctrl Pts',(-2.45105688854432,-1.,-3.0713129052131));
#66616=CARTESIAN_POINT('Ctrl Pts',(-2.45105688854432,1.,-3.0713129052131));
#66617=CARTESIAN_POINT('Ctrl Pts',(-2.44824970516558,-1.,-3.06431596421422));
#66618=CARTESIAN_POINT('Ctrl Pts',(-2.44824970516558,1.,-3.06431596421422));
#66619=CARTESIAN_POINT('Ctrl Pts',(-2.44541251892568,-1.,-3.05736242671521));
#66620=CARTESIAN_POINT('Ctrl Pts',(-2.44541251892568,1.,-3.05736242671521));
#66621=CARTESIAN_POINT('Ctrl Pts',(-2.44254768923109,-1.,-3.05045678021509));
#66622=CARTESIAN_POINT('Ctrl Pts',(-2.44254768923109,1.,-3.05045678021509));
#66623=CARTESIAN_POINT('Ctrl Pts',(-2.43965194061849,-1.,-3.04359685040545));
#66624=CARTESIAN_POINT('Ctrl Pts',(-2.43965194061849,1.,-3.04359685040545));
#66625=CARTESIAN_POINT('Ctrl Pts',(-2.43671278042394,-1.,-3.03676949672797));
#66626=CARTESIAN_POINT('Ctrl Pts',(-2.43671278042394,1.,-3.03676949672797));
#66627=CARTESIAN_POINT('Ctrl Pts',(-2.43371241361462,-1.,-3.02995534946946));
#66628=CARTESIAN_POINT('Ctrl Pts',(-2.43371241361462,1.,-3.02995534946946));
#66629=CARTESIAN_POINT('Ctrl Pts',(-2.43063415586615,-1.,-3.02313656035977));
#66630=CARTESIAN_POINT('Ctrl Pts',(-2.43063415586615,1.,-3.02313656035977));
#66631=CARTESIAN_POINT('Ctrl Pts',(-2.4274685626416,-1.,-3.01630420830494));
#66632=CARTESIAN_POINT('Ctrl Pts',(-2.4274685626416,1.,-3.01630420830494));
#66633=CARTESIAN_POINT('Ctrl Pts',(-2.42421849439625,-1.,-3.00946442616674));
#66634=CARTESIAN_POINT('Ctrl Pts',(-2.42421849439625,1.,-3.00946442616674));
#66635=CARTESIAN_POINT('Ctrl Pts',(-2.42090763946812,-1.,-3.00264868586038));
#66636=CARTESIAN_POINT('Ctrl Pts',(-2.42090763946812,1.,-3.00264868586038));
#66637=CARTESIAN_POINT('Ctrl Pts',(-2.4175732450056,-1.,-2.99590509293561));
#66638=CARTESIAN_POINT('Ctrl Pts',(-2.4175732450056,1.,-2.99590509293561));
#66639=CARTESIAN_POINT('Ctrl Pts',(-2.4142506419963,-1.,-2.98927983005851));
#66640=CARTESIAN_POINT('Ctrl Pts',(-2.4142506419963,1.,-2.98927983005851));
#66641=CARTESIAN_POINT('Ctrl Pts',(-2.41095909342591,-1.,-2.98280015815132));
#66642=CARTESIAN_POINT('Ctrl Pts',(-2.41095909342591,1.,-2.98280015815132));
#66643=CARTESIAN_POINT('Ctrl Pts',(-2.40768975073691,-1.,-2.97646002822395));
#66644=CARTESIAN_POINT('Ctrl Pts',(-2.40768975073691,1.,-2.97646002822395));
#66645=CARTESIAN_POINT('Ctrl Pts',(-2.40438604734848,-1.,-2.97019641312272));
#66646=CARTESIAN_POINT('Ctrl Pts',(-2.40438604734848,1.,-2.97019641312272));
#66647=CARTESIAN_POINT('Ctrl Pts',(-2.40095565711535,-1.,-2.96390432240181));
#66648=CARTESIAN_POINT('Ctrl Pts',(-2.40095565711535,1.,-2.96390432240181));
#66649=CARTESIAN_POINT('Ctrl Pts',(-2.39730553974412,-1.,-2.95748006482811));
#66650=CARTESIAN_POINT('Ctrl Pts',(-2.39730553974412,1.,-2.95748006482811));
#66651=CARTESIAN_POINT('Ctrl Pts',(-2.39337207631613,-1.,-2.95085857128372));
#66652=CARTESIAN_POINT('Ctrl Pts',(-2.39337207631613,1.,-2.95085857128372));
#66653=CARTESIAN_POINT('Ctrl Pts',(-2.38914929090806,-1.,-2.94404820669135));
#66654=CARTESIAN_POINT('Ctrl Pts',(-2.38914929090806,1.,-2.94404820669135));
#66655=CARTESIAN_POINT('Ctrl Pts',(-2.38472771516476,-1.,-2.93717903280599));
#66656=CARTESIAN_POINT('Ctrl Pts',(-2.38472771516476,1.,-2.93717903280599));
#66657=CARTESIAN_POINT('Ctrl Pts',(-2.3802898958232,-1.,-2.93049643640517));
#66658=CARTESIAN_POINT('Ctrl Pts',(-2.3802898958232,1.,-2.93049643640517));
#66659=CARTESIAN_POINT('Ctrl Pts',(-2.37606510524271,-1.,-2.92430340582912));
#66660=CARTESIAN_POINT('Ctrl Pts',(-2.37606510524271,1.,-2.92430340582912));
#66661=CARTESIAN_POINT('Ctrl Pts',(-2.37229381109939,-1.,-2.9189150379156));
#66662=CARTESIAN_POINT('Ctrl Pts',(-2.37229381109939,1.,-2.9189150379156));
#66663=CARTESIAN_POINT('Ctrl Pts',(-2.36919161373074,-1.,-2.91461249883016));
#66664=CARTESIAN_POINT('Ctrl Pts',(-2.36919161373074,1.,-2.91461249883016));
#66665=CARTESIAN_POINT('Ctrl Pts',(-2.36690501170317,-1.,-2.9115863784165));
#66666=CARTESIAN_POINT('Ctrl Pts',(-2.36690501170317,1.,-2.9115863784165));
#66667=CARTESIAN_POINT('Ctrl Pts',(-2.36578327194396,-1.,-2.91025813829606));
#66668=CARTESIAN_POINT('Ctrl Pts',(-2.36578327194396,1.,-2.91025813829606));
#66669=CARTESIAN_POINT('Ctrl Pts',(-2.36535052956704,-1.,-2.90989022547738));
#66670=CARTESIAN_POINT('Ctrl Pts',(-2.36535052956704,1.,-2.90989022547738));
#66671=CARTESIAN_POINT('Ctrl Pts',(-2.36524348105023,-1.,-2.90992398626098));
#66672=CARTESIAN_POINT('Ctrl Pts',(-2.36524348105023,1.,-2.90992398626098));
#66673=CARTESIAN_POINT('Ctrl Pts',(-2.36523532225181,-1.,-2.91001063062876));
#66674=CARTESIAN_POINT('Ctrl Pts',(-2.36523532225181,1.,-2.91001063062876));
#66675=CARTESIAN_POINT('',(-2.52982887637028,1.,-3.35260583073571));
#66676=CARTESIAN_POINT('Ctrl Pts',(-2.52982887637028,1.,-3.35260583073571));
#66677=CARTESIAN_POINT('Ctrl Pts',(-2.52954136549357,1.,-3.35105973714426));
#66678=CARTESIAN_POINT('Ctrl Pts',(-2.5289632161143,1.,-3.34796903577628));
#66679=CARTESIAN_POINT('Ctrl Pts',(-2.52808660916879,1.,-3.34333744117093));
#66680=CARTESIAN_POINT('Ctrl Pts',(-2.52689902691551,1.,-3.33717090000955));
#66681=CARTESIAN_POINT('Ctrl Pts',(-2.52538321165774,1.,-3.32947762189049));
#66682=CARTESIAN_POINT('Ctrl Pts',(-2.52383598396878,1.,-3.32179931079521));
#66683=CARTESIAN_POINT('Ctrl Pts',(-2.52225724871375,1.,-3.31413607874727));
#66684=CARTESIAN_POINT('Ctrl Pts',(-2.52064689568167,1.,-3.30648808814986));
#66685=CARTESIAN_POINT('Ctrl Pts',(-2.51900480700548,1.,-3.29885556387661));
#66686=CARTESIAN_POINT('Ctrl Pts',(-2.51733085123316,1.,-3.2912387729863));
#66687=CARTESIAN_POINT('Ctrl Pts',(-2.51562487464215,1.,-3.28363799702583));
#66688=CARTESIAN_POINT('Ctrl Pts',(-2.51388669270329,1.,-3.27605350473048));
#66689=CARTESIAN_POINT('Ctrl Pts',(-2.51211608411539,1.,-3.26848552888271));
#66690=CARTESIAN_POINT('Ctrl Pts',(-2.51031277813697,1.,-3.26093423001716));
#66691=CARTESIAN_POINT('Ctrl Pts',(-2.50847647070936,1.,-3.25339971461265));
#66692=CARTESIAN_POINT('Ctrl Pts',(-2.50660685940645,1.,-3.24588208984042));
#66693=CARTESIAN_POINT('Ctrl Pts',(-2.50470367580078,1.,-3.23838151080383));
#66694=CARTESIAN_POINT('Ctrl Pts',(-2.50276671338074,1.,-3.23089822320596));
#66695=CARTESIAN_POINT('Ctrl Pts',(-2.5007958720187,1.,-3.22343262620387));
#66696=CARTESIAN_POINT('Ctrl Pts',(-2.49879114599293,1.,-3.21598526261157));
#66697=CARTESIAN_POINT('Ctrl Pts',(-2.49675252647298,1.,-3.2085566984974));
#66698=CARTESIAN_POINT('Ctrl Pts',(-2.49467992057726,1.,-3.20114742397549));
#66699=CARTESIAN_POINT('Ctrl Pts',(-2.4925730723986,1.,-3.19375775555814));
#66700=CARTESIAN_POINT('Ctrl Pts',(-2.49043146334095,1.,-3.18638771282315));
#66701=CARTESIAN_POINT('Ctrl Pts',(-2.48825428288243,1.,-3.17903698136679));
#66702=CARTESIAN_POINT('Ctrl Pts',(-2.48604065348619,1.,-3.17170518863357));
#66703=CARTESIAN_POINT('Ctrl Pts',(-2.48378981792739,1.,-3.16439213290181));
#66704=CARTESIAN_POINT('Ctrl Pts',(-2.48150133566568,1.,-3.15709802322735));
#66705=CARTESIAN_POINT('Ctrl Pts',(-2.47917529057016,1.,-3.14982373241335));
#66706=CARTESIAN_POINT('Ctrl Pts',(-2.47681245356095,1.,-3.14257099546531));
#66707=CARTESIAN_POINT('Ctrl Pts',(-2.47441378371923,1.,-3.13534181229282));
#66708=CARTESIAN_POINT('Ctrl Pts',(-2.47197997765868,1.,-3.12813790805948));
#66709=CARTESIAN_POINT('Ctrl Pts',(-2.4695109894747,1.,-3.12096015766984));
#66710=CARTESIAN_POINT('Ctrl Pts',(-2.46700558843507,1.,-3.11380805536124));
#66711=CARTESIAN_POINT('Ctrl Pts',(-2.46446082979645,1.,-3.10667907901981));
#66712=CARTESIAN_POINT('Ctrl Pts',(-2.4618730850188,1.,-3.09956993697048));
#66713=CARTESIAN_POINT('Ctrl Pts',(-2.45923912563875,1.,-3.09247787931881));
#66714=CARTESIAN_POINT('Ctrl Pts',(-2.45655725437037,1.,-3.08540206545313));
#66715=CARTESIAN_POINT('Ctrl Pts',(-2.45382826787795,1.,-3.07834472886145));
#66716=CARTESIAN_POINT('Ctrl Pts',(-2.45105688854432,1.,-3.0713129052131));
#66717=CARTESIAN_POINT('Ctrl Pts',(-2.44824970516558,1.,-3.06431596421422));
#66718=CARTESIAN_POINT('Ctrl Pts',(-2.44541251892568,1.,-3.05736242671521));
#66719=CARTESIAN_POINT('Ctrl Pts',(-2.44254768923109,1.,-3.05045678021509));
#66720=CARTESIAN_POINT('Ctrl Pts',(-2.43965194061849,1.,-3.04359685040545));
#66721=CARTESIAN_POINT('Ctrl Pts',(-2.43671278042394,1.,-3.03676949672797));
#66722=CARTESIAN_POINT('Ctrl Pts',(-2.43371241361462,1.,-3.02995534946946));
#66723=CARTESIAN_POINT('Ctrl Pts',(-2.43063415586615,1.,-3.02313656035977));
#66724=CARTESIAN_POINT('Ctrl Pts',(-2.4274685626416,1.,-3.01630420830494));
#66725=CARTESIAN_POINT('Ctrl Pts',(-2.42421849439625,1.,-3.00946442616674));
#66726=CARTESIAN_POINT('Ctrl Pts',(-2.42090763946812,1.,-3.00264868586038));
#66727=CARTESIAN_POINT('Ctrl Pts',(-2.4175732450056,1.,-2.99590509293561));
#66728=CARTESIAN_POINT('Ctrl Pts',(-2.4142506419963,1.,-2.98927983005851));
#66729=CARTESIAN_POINT('Ctrl Pts',(-2.41095909342591,1.,-2.98280015815132));
#66730=CARTESIAN_POINT('Ctrl Pts',(-2.40768975073691,1.,-2.97646002822395));
#66731=CARTESIAN_POINT('Ctrl Pts',(-2.40438604734848,1.,-2.97019641312272));
#66732=CARTESIAN_POINT('Ctrl Pts',(-2.40095565711535,1.,-2.96390432240181));
#66733=CARTESIAN_POINT('Ctrl Pts',(-2.39730553974412,1.,-2.95748006482811));
#66734=CARTESIAN_POINT('Ctrl Pts',(-2.39337207631613,1.,-2.95085857128372));
#66735=CARTESIAN_POINT('Ctrl Pts',(-2.38914929090806,1.,-2.94404820669135));
#66736=CARTESIAN_POINT('Ctrl Pts',(-2.38472771516476,1.,-2.93717903280599));
#66737=CARTESIAN_POINT('Ctrl Pts',(-2.3802898958232,1.,-2.93049643640517));
#66738=CARTESIAN_POINT('Ctrl Pts',(-2.37606510524271,1.,-2.92430340582912));
#66739=CARTESIAN_POINT('Ctrl Pts',(-2.37229381109939,1.,-2.9189150379156));
#66740=CARTESIAN_POINT('Ctrl Pts',(-2.36919161373074,1.,-2.91461249883016));
#66741=CARTESIAN_POINT('Ctrl Pts',(-2.36707658451709,1.,-2.91181344022628));
#66742=CARTESIAN_POINT('Ctrl Pts',(-2.36599991765853,1.,-2.91051690822262));
#66743=CARTESIAN_POINT('Ctrl Pts',(-2.36553202948741,1.,-2.9100577052777));
#66744=CARTESIAN_POINT('Ctrl Pts',(-2.3653621118858,1.,-2.90995756655559));
#66745=CARTESIAN_POINT('Ctrl Pts',(-2.36531447826213,1.,-2.90994629141563));
#66746=CARTESIAN_POINT('',(-2.52982887637028,0.,-3.35260583073571));
#66747=CARTESIAN_POINT('Ctrl Pts',(-2.03668666247593,-1.,-3.1487152044751));
#66748=CARTESIAN_POINT('Ctrl Pts',(-2.03668666247593,1.,-3.1487152044751));
#66749=CARTESIAN_POINT('Ctrl Pts',(-2.03660173757879,-1.,-3.14869618937258));
#66750=CARTESIAN_POINT('Ctrl Pts',(-2.03660173757879,1.,-3.14869618937258));
#66751=CARTESIAN_POINT('Ctrl Pts',(-2.03653654935592,-1.,-3.14878756590812));
#66752=CARTESIAN_POINT('Ctrl Pts',(-2.03653654935592,1.,-3.14878756590812));
#66753=CARTESIAN_POINT('Ctrl Pts',(-2.03675273049189,-1.,-3.14931281968048));
#66754=CARTESIAN_POINT('Ctrl Pts',(-2.03675273049189,1.,-3.14931281968048));
#66755=CARTESIAN_POINT('Ctrl Pts',(-2.03766932526445,-1.,-3.15079010635742));
#66756=CARTESIAN_POINT('Ctrl Pts',(-2.03766932526445,1.,-3.15079010635742));
#66757=CARTESIAN_POINT('Ctrl Pts',(-2.03984073791519,-1.,-3.15389991674792));
#66758=CARTESIAN_POINT('Ctrl Pts',(-2.03984073791519,1.,-3.15389991674792));
#66759=CARTESIAN_POINT('Ctrl Pts',(-2.04297406404027,-1.,-3.15817983946367));
#66760=CARTESIAN_POINT('Ctrl Pts',(-2.04297406404027,1.,-3.15817983946367));
#66761=CARTESIAN_POINT('Ctrl Pts',(-2.04693331247446,-1.,-3.16343165058912));
#66762=CARTESIAN_POINT('Ctrl Pts',(-2.04693331247446,1.,-3.16343165058912));
#66763=CARTESIAN_POINT('Ctrl Pts',(-2.05151770247233,-1.,-3.16936341689527));
#66764=CARTESIAN_POINT('Ctrl Pts',(-2.05151770247233,1.,-3.16936341689527));
#66765=CARTESIAN_POINT('Ctrl Pts',(-2.05650186773132,-1.,-3.17564906975371));
#66766=CARTESIAN_POINT('Ctrl Pts',(-2.05650186773132,1.,-3.17564906975371));
#66767=CARTESIAN_POINT('Ctrl Pts',(-2.06166849827101,-1.,-3.18197692964614));
#66768=CARTESIAN_POINT('Ctrl Pts',(-2.06166849827101,1.,-3.18197692964614));
#66769=CARTESIAN_POINT('Ctrl Pts',(-2.06684062744112,-1.,-3.18809755562368));
#66770=CARTESIAN_POINT('Ctrl Pts',(-2.06684062744112,1.,-3.18809755562368));
#66771=CARTESIAN_POINT('Ctrl Pts',(-2.07192253497857,-1.,-3.19388465568252));
#66772=CARTESIAN_POINT('Ctrl Pts',(-2.07192253497857,1.,-3.19388465568252));
#66773=CARTESIAN_POINT('Ctrl Pts',(-2.07690441870722,-1.,-3.19934132836019));
#66774=CARTESIAN_POINT('Ctrl Pts',(-2.07690441870722,1.,-3.19934132836019));
#66775=CARTESIAN_POINT('Ctrl Pts',(-2.08182850370878,-1.,-3.2045481863073));
#66776=CARTESIAN_POINT('Ctrl Pts',(-2.08182850370878,1.,-3.2045481863073));
#66777=CARTESIAN_POINT('Ctrl Pts',(-2.08676465517455,-1.,-3.20962575845463));
#66778=CARTESIAN_POINT('Ctrl Pts',(-2.08676465517455,1.,-3.20962575845463));
#66779=CARTESIAN_POINT('Ctrl Pts',(-2.09178419460443,-1.,-3.21469429601654));
#66780=CARTESIAN_POINT('Ctrl Pts',(-2.09178419460443,1.,-3.21469429601654));
#66781=CARTESIAN_POINT('Ctrl Pts',(-2.09692958434895,-1.,-3.21982707347009));
#66782=CARTESIAN_POINT('Ctrl Pts',(-2.09692958434895,1.,-3.21982707347009));
#66783=CARTESIAN_POINT('Ctrl Pts',(-2.10220384298492,-1.,-3.22503437553434));
#66784=CARTESIAN_POINT('Ctrl Pts',(-2.10220384298492,1.,-3.22503437553434));
#66785=CARTESIAN_POINT('Ctrl Pts',(-2.10758699642451,-1.,-3.23028945793289));
#66786=CARTESIAN_POINT('Ctrl Pts',(-2.10758699642451,1.,-3.23028945793289));
#66787=CARTESIAN_POINT('Ctrl Pts',(-2.11304604021773,-1.,-3.23554444767099));
#66788=CARTESIAN_POINT('Ctrl Pts',(-2.11304604021773,1.,-3.23554444767099));
#66789=CARTESIAN_POINT('Ctrl Pts',(-2.11854673326979,-1.,-3.24074905517293));
#66790=CARTESIAN_POINT('Ctrl Pts',(-2.11854673326979,1.,-3.24074905517293));
#66791=CARTESIAN_POINT('Ctrl Pts',(-2.12406646410962,-1.,-3.24587102613376));
#66792=CARTESIAN_POINT('Ctrl Pts',(-2.12406646410962,1.,-3.24587102613376));
#66793=CARTESIAN_POINT('Ctrl Pts',(-2.12960028396832,-1.,-3.25090574494028));
#66794=CARTESIAN_POINT('Ctrl Pts',(-2.12960028396832,1.,-3.25090574494028));
#66795=CARTESIAN_POINT('Ctrl Pts',(-2.13515375878803,-1.,-3.25586495065054));
#66796=CARTESIAN_POINT('Ctrl Pts',(-2.13515375878803,1.,-3.25586495065054));
#66797=CARTESIAN_POINT('Ctrl Pts',(-2.14073870754264,-1.,-3.26077002641879));
#66798=CARTESIAN_POINT('Ctrl Pts',(-2.14073870754264,1.,-3.26077002641879));
#66799=CARTESIAN_POINT('Ctrl Pts',(-2.1463680529566,-1.,-3.26564388189759));
#66800=CARTESIAN_POINT('Ctrl Pts',(-2.1463680529566,1.,-3.26564388189759));
#66801=CARTESIAN_POINT('Ctrl Pts',(-2.15205043199808,-1.,-3.27050245897228));
#66802=CARTESIAN_POINT('Ctrl Pts',(-2.15205043199808,1.,-3.27050245897228));
#66803=CARTESIAN_POINT('Ctrl Pts',(-2.15778690038347,-1.,-3.27534954469187));
#66804=CARTESIAN_POINT('Ctrl Pts',(-2.15778690038347,1.,-3.27534954469187));
#66805=CARTESIAN_POINT('Ctrl Pts',(-2.16357391934425,-1.,-3.280181508414));
#66806=CARTESIAN_POINT('Ctrl Pts',(-2.16357391934425,1.,-3.280181508414));
#66807=CARTESIAN_POINT('Ctrl Pts',(-2.16940517773455,-1.,-3.28499019979724));
#66808=CARTESIAN_POINT('Ctrl Pts',(-2.16940517773455,1.,-3.28499019979724));
#66809=CARTESIAN_POINT('Ctrl Pts',(-2.17527380048423,-1.,-3.28976645712568));
#66810=CARTESIAN_POINT('Ctrl Pts',(-2.17527380048423,1.,-3.28976645712568));
#66811=CARTESIAN_POINT('Ctrl Pts',(-2.18117455557065,-1.,-3.2945036150049));
#66812=CARTESIAN_POINT('Ctrl Pts',(-2.18117455557065,1.,-3.2945036150049));
#66813=CARTESIAN_POINT('Ctrl Pts',(-2.18710556500327,-1.,-3.29920022557639));
#66814=CARTESIAN_POINT('Ctrl Pts',(-2.18710556500327,1.,-3.29920022557639));
#66815=CARTESIAN_POINT('Ctrl Pts',(-2.19306710376111,-1.,-3.30385816281831));
#66816=CARTESIAN_POINT('Ctrl Pts',(-2.19306710376111,1.,-3.30385816281831));
#66817=CARTESIAN_POINT('Ctrl Pts',(-2.19906078949923,-1.,-3.30848134694595));
#66818=CARTESIAN_POINT('Ctrl Pts',(-2.19906078949923,1.,-3.30848134694595));
#66819=CARTESIAN_POINT('Ctrl Pts',(-2.20508863150607,-1.,-3.31307424608949));
#66820=CARTESIAN_POINT('Ctrl Pts',(-2.20508863150607,1.,-3.31307424608949));
#66821=CARTESIAN_POINT('Ctrl Pts',(-2.21115211847875,-1.,-3.31764044024235));
#66822=CARTESIAN_POINT('Ctrl Pts',(-2.21115211847875,1.,-3.31764044024235));
#66823=CARTESIAN_POINT('Ctrl Pts',(-2.21725135110898,-1.,-3.32218125618968));
#66824=CARTESIAN_POINT('Ctrl Pts',(-2.21725135110898,1.,-3.32218125618968));
#66825=CARTESIAN_POINT('Ctrl Pts',(-2.22338548312772,-1.,-3.3266964672289));
#66826=CARTESIAN_POINT('Ctrl Pts',(-2.22338548312772,1.,-3.3266964672289));
#66827=CARTESIAN_POINT('Ctrl Pts',(-2.22955308907233,-1.,-3.33118487773611));
#66828=CARTESIAN_POINT('Ctrl Pts',(-2.22955308907233,1.,-3.33118487773611));
#66829=CARTESIAN_POINT('Ctrl Pts',(-2.23575256328812,-1.,-3.33564495756482));
#66830=CARTESIAN_POINT('Ctrl Pts',(-2.23575256328812,1.,-3.33564495756482));
#66831=CARTESIAN_POINT('Ctrl Pts',(-2.24198249391422,-1.,-3.34007543738025));
#66832=CARTESIAN_POINT('Ctrl Pts',(-2.24198249391422,1.,-3.34007543738025));
#66833=CARTESIAN_POINT('Ctrl Pts',(-2.24824207678256,-1.,-3.34447596770723));
#66834=CARTESIAN_POINT('Ctrl Pts',(-2.24824207678256,1.,-3.34447596770723));
#66835=CARTESIAN_POINT('Ctrl Pts',(-2.25453097693483,-1.,-3.34884690292285));
#66836=CARTESIAN_POINT('Ctrl Pts',(-2.25453097693483,1.,-3.34884690292285));
#66837=CARTESIAN_POINT('Ctrl Pts',(-2.26084915222449,-1.,-3.35318902552626));
#66838=CARTESIAN_POINT('Ctrl Pts',(-2.26084915222449,1.,-3.35318902552626));
#66839=CARTESIAN_POINT('Ctrl Pts',(-2.2671966857991,-1.,-3.35750328523061));
#66840=CARTESIAN_POINT('Ctrl Pts',(-2.2671966857991,1.,-3.35750328523061));
#66841=CARTESIAN_POINT('Ctrl Pts',(-2.2735736262093,-1.,-3.36179055004409));
#66842=CARTESIAN_POINT('Ctrl Pts',(-2.2735736262093,1.,-3.36179055004409));
#66843=CARTESIAN_POINT('Ctrl Pts',(-2.27997979458037,-1.,-3.36605130713076));
#66844=CARTESIAN_POINT('Ctrl Pts',(-2.27997979458037,1.,-3.36605130713076));
#66845=CARTESIAN_POINT('Ctrl Pts',(-2.28641481081137,-1.,-3.37028570206488));
#66846=CARTESIAN_POINT('Ctrl Pts',(-2.28641481081137,1.,-3.37028570206488));
#66847=CARTESIAN_POINT('Ctrl Pts',(-2.29287818007393,-1.,-3.37449367172826));
#66848=CARTESIAN_POINT('Ctrl Pts',(-2.29287818007393,1.,-3.37449367172826));
#66849=CARTESIAN_POINT('Ctrl Pts',(-2.29936936127624,-1.,-3.37867504959433));
#66850=CARTESIAN_POINT('Ctrl Pts',(-2.29936936127624,1.,-3.37867504959433));
#66851=CARTESIAN_POINT('Ctrl Pts',(-2.30588783640343,-1.,-3.3828296733661));
#66852=CARTESIAN_POINT('Ctrl Pts',(-2.30588783640343,1.,-3.3828296733661));
#66853=CARTESIAN_POINT('Ctrl Pts',(-2.31243319489367,-1.,-3.38695751492462));
#66854=CARTESIAN_POINT('Ctrl Pts',(-2.31243319489367,1.,-3.38695751492462));
#66855=CARTESIAN_POINT('Ctrl Pts',(-2.31900513925424,-1.,-3.39105869474822));
#66856=CARTESIAN_POINT('Ctrl Pts',(-2.31900513925424,1.,-3.39105869474822));
#66857=CARTESIAN_POINT('Ctrl Pts',(-2.3256034390248,-1.,-3.39513342019756));
#66858=CARTESIAN_POINT('Ctrl Pts',(-2.3256034390248,1.,-3.39513342019756));
#66859=CARTESIAN_POINT('Ctrl Pts',(-2.33222789882489,-1.,-3.39918194577956));
#66860=CARTESIAN_POINT('Ctrl Pts',(-2.33222789882489,1.,-3.39918194577956));
#66861=CARTESIAN_POINT('Ctrl Pts',(-2.33887832342782,-1.,-3.40320452776743));
#66862=CARTESIAN_POINT('Ctrl Pts',(-2.33887832342782,1.,-3.40320452776743));
#66863=CARTESIAN_POINT('Ctrl Pts',(-2.34555447649188,-1.,-3.40720137404297));
#66864=CARTESIAN_POINT('Ctrl Pts',(-2.34555447649188,1.,-3.40720137404297));
#66865=CARTESIAN_POINT('Ctrl Pts',(-2.35225606824109,-1.,-3.41117262314119));
#66866=CARTESIAN_POINT('Ctrl Pts',(-2.35225606824109,1.,-3.41117262314119));
#66867=CARTESIAN_POINT('Ctrl Pts',(-2.35898278606946,-1.,-3.41511836751469));
#66868=CARTESIAN_POINT('Ctrl Pts',(-2.35898278606946,1.,-3.41511836751469));
#66869=CARTESIAN_POINT('Ctrl Pts',(-2.36573431470642,-1.,-3.41903866635852));
#66870=CARTESIAN_POINT('Ctrl Pts',(-2.36573431470642,1.,-3.41903866635852));
#66871=CARTESIAN_POINT('Ctrl Pts',(-2.37251035954292,-1.,-3.42293356216511));
#66872=CARTESIAN_POINT('Ctrl Pts',(-2.37251035954292,1.,-3.42293356216511));
#66873=CARTESIAN_POINT('Ctrl Pts',(-2.37931067028926,-1.,-3.42680309754399));
#66874=CARTESIAN_POINT('Ctrl Pts',(-2.37931067028926,1.,-3.42680309754399));
#66875=CARTESIAN_POINT('Ctrl Pts',(-2.38613505843552,-1.,-3.4306473271292));
#66876=CARTESIAN_POINT('Ctrl Pts',(-2.38613505843552,1.,-3.4306473271292));
#66877=CARTESIAN_POINT('Ctrl Pts',(-2.39298338804493,-1.,-3.4344663067854));
#66878=CARTESIAN_POINT('Ctrl Pts',(-2.39298338804493,1.,-3.4344663067854));
#66879=CARTESIAN_POINT('Ctrl Pts',(-2.39848113410292,-1.,-3.43750133064416));
#66880=CARTESIAN_POINT('Ctrl Pts',(-2.39848113410292,1.,-3.43750133064416));
#66881=CARTESIAN_POINT('Ctrl Pts',(-2.40261515589405,-1.,-3.43976627484234));
#66882=CARTESIAN_POINT('Ctrl Pts',(-2.40261515589405,1.,-3.43976627484234));
#66883=CARTESIAN_POINT('Ctrl Pts',(-2.4053759295909,-1.,-3.44127120683039));
#66884=CARTESIAN_POINT('Ctrl Pts',(-2.4053759295909,1.,-3.44127120683039));
#66885=CARTESIAN_POINT('Ctrl Pts',(-2.40675750623143,-1.,-3.44202241512147));
#66886=CARTESIAN_POINT('Ctrl Pts',(-2.40675750623143,1.,-3.44202241512147));
#66887=CARTESIAN_POINT('',(-2.03660101169714,1.,-3.14877060440328));
#66888=CARTESIAN_POINT('Ctrl Pts',(-2.03660101169715,-1.,-3.14877060440327));
#66889=CARTESIAN_POINT('Ctrl Pts',(-2.03660101169715,-0.666666666666667,
-3.14877060440327));
#66890=CARTESIAN_POINT('Ctrl Pts',(-2.03660101169715,-0.333333333333333,
-3.14877060440327));
#66891=CARTESIAN_POINT('Ctrl Pts',(-2.03660101169715,0.333333333333333,
-3.14877060440327));
#66892=CARTESIAN_POINT('Ctrl Pts',(-2.03660101169715,0.666666666666667,
-3.14877060440327));
#66893=CARTESIAN_POINT('Ctrl Pts',(-2.03660101169715,1.,-3.14877060440327));
#66894=CARTESIAN_POINT('',(-2.40675750623143,1.,-3.44202241512147));
#66895=CARTESIAN_POINT('',(-2.40675750623143,0.,-3.44202241512147));
#66896=CARTESIAN_POINT('Ctrl Pts',(-2.03660101169715,1.,-3.14877060440328));
#66897=CARTESIAN_POINT('Ctrl Pts',(-2.03659701539259,1.,-3.14881939088124));
#66898=CARTESIAN_POINT('Ctrl Pts',(-2.03663974554932,1.,-3.1490119366901));
#66899=CARTESIAN_POINT('Ctrl Pts',(-2.03693188810545,1.,-3.14959882629805));
#66900=CARTESIAN_POINT('Ctrl Pts',(-2.03783225495961,1.,-3.15102344775328));
#66901=CARTESIAN_POINT('Ctrl Pts',(-2.03984073791519,1.,-3.15389991674792));
#66902=CARTESIAN_POINT('Ctrl Pts',(-2.04297406404027,1.,-3.15817983946367));
#66903=CARTESIAN_POINT('Ctrl Pts',(-2.04693331247446,1.,-3.16343165058912));
#66904=CARTESIAN_POINT('Ctrl Pts',(-2.05151770247233,1.,-3.16936341689527));
#66905=CARTESIAN_POINT('Ctrl Pts',(-2.05650186773132,1.,-3.17564906975371));
#66906=CARTESIAN_POINT('Ctrl Pts',(-2.06166849827101,1.,-3.18197692964614));
#66907=CARTESIAN_POINT('Ctrl Pts',(-2.06684062744112,1.,-3.18809755562368));
#66908=CARTESIAN_POINT('Ctrl Pts',(-2.07192253497857,1.,-3.19388465568252));
#66909=CARTESIAN_POINT('Ctrl Pts',(-2.07690441870722,1.,-3.19934132836019));
#66910=CARTESIAN_POINT('Ctrl Pts',(-2.08182850370878,1.,-3.2045481863073));
#66911=CARTESIAN_POINT('Ctrl Pts',(-2.08676465517455,1.,-3.20962575845463));
#66912=CARTESIAN_POINT('Ctrl Pts',(-2.09178419460443,1.,-3.21469429601654));
#66913=CARTESIAN_POINT('Ctrl Pts',(-2.09692958434895,1.,-3.21982707347009));
#66914=CARTESIAN_POINT('Ctrl Pts',(-2.10220384298492,1.,-3.22503437553434));
#66915=CARTESIAN_POINT('Ctrl Pts',(-2.10758699642451,1.,-3.23028945793289));
#66916=CARTESIAN_POINT('Ctrl Pts',(-2.11304604021773,1.,-3.23554444767099));
#66917=CARTESIAN_POINT('Ctrl Pts',(-2.11854673326979,1.,-3.24074905517293));
#66918=CARTESIAN_POINT('Ctrl Pts',(-2.12406646410962,1.,-3.24587102613376));
#66919=CARTESIAN_POINT('Ctrl Pts',(-2.12960028396832,1.,-3.25090574494028));
#66920=CARTESIAN_POINT('Ctrl Pts',(-2.13515375878803,1.,-3.25586495065054));
#66921=CARTESIAN_POINT('Ctrl Pts',(-2.14073870754264,1.,-3.26077002641879));
#66922=CARTESIAN_POINT('Ctrl Pts',(-2.1463680529566,1.,-3.26564388189759));
#66923=CARTESIAN_POINT('Ctrl Pts',(-2.15205043199808,1.,-3.27050245897228));
#66924=CARTESIAN_POINT('Ctrl Pts',(-2.15778690038347,1.,-3.27534954469187));
#66925=CARTESIAN_POINT('Ctrl Pts',(-2.16357391934425,1.,-3.280181508414));
#66926=CARTESIAN_POINT('Ctrl Pts',(-2.16940517773455,1.,-3.28499019979724));
#66927=CARTESIAN_POINT('Ctrl Pts',(-2.17527380048423,1.,-3.28976645712568));
#66928=CARTESIAN_POINT('Ctrl Pts',(-2.18117455557065,1.,-3.2945036150049));
#66929=CARTESIAN_POINT('Ctrl Pts',(-2.18710556500327,1.,-3.29920022557639));
#66930=CARTESIAN_POINT('Ctrl Pts',(-2.19306710376111,1.,-3.30385816281831));
#66931=CARTESIAN_POINT('Ctrl Pts',(-2.19906078949923,1.,-3.30848134694595));
#66932=CARTESIAN_POINT('Ctrl Pts',(-2.20508863150607,1.,-3.31307424608949));
#66933=CARTESIAN_POINT('Ctrl Pts',(-2.21115211847875,1.,-3.31764044024235));
#66934=CARTESIAN_POINT('Ctrl Pts',(-2.21725135110898,1.,-3.32218125618968));
#66935=CARTESIAN_POINT('Ctrl Pts',(-2.22338548312772,1.,-3.3266964672289));
#66936=CARTESIAN_POINT('Ctrl Pts',(-2.22955308907233,1.,-3.33118487773611));
#66937=CARTESIAN_POINT('Ctrl Pts',(-2.23575256328812,1.,-3.33564495756482));
#66938=CARTESIAN_POINT('Ctrl Pts',(-2.24198249391422,1.,-3.34007543738025));
#66939=CARTESIAN_POINT('Ctrl Pts',(-2.24824207678256,1.,-3.34447596770723));
#66940=CARTESIAN_POINT('Ctrl Pts',(-2.25453097693483,1.,-3.34884690292285));
#66941=CARTESIAN_POINT('Ctrl Pts',(-2.26084915222449,1.,-3.35318902552626));
#66942=CARTESIAN_POINT('Ctrl Pts',(-2.2671966857991,1.,-3.35750328523061));
#66943=CARTESIAN_POINT('Ctrl Pts',(-2.2735736262093,1.,-3.36179055004409));
#66944=CARTESIAN_POINT('Ctrl Pts',(-2.27997979458037,1.,-3.36605130713076));
#66945=CARTESIAN_POINT('Ctrl Pts',(-2.28641481081137,1.,-3.37028570206488));
#66946=CARTESIAN_POINT('Ctrl Pts',(-2.29287818007393,1.,-3.37449367172826));
#66947=CARTESIAN_POINT('Ctrl Pts',(-2.29936936127624,1.,-3.37867504959433));
#66948=CARTESIAN_POINT('Ctrl Pts',(-2.30588783640343,1.,-3.3828296733661));
#66949=CARTESIAN_POINT('Ctrl Pts',(-2.31243319489367,1.,-3.38695751492462));
#66950=CARTESIAN_POINT('Ctrl Pts',(-2.31900513925424,1.,-3.39105869474822));
#66951=CARTESIAN_POINT('Ctrl Pts',(-2.3256034390248,1.,-3.39513342019756));
#66952=CARTESIAN_POINT('Ctrl Pts',(-2.33222789882489,1.,-3.39918194577956));
#66953=CARTESIAN_POINT('Ctrl Pts',(-2.33887832342782,1.,-3.40320452776743));
#66954=CARTESIAN_POINT('Ctrl Pts',(-2.34555447649188,1.,-3.40720137404297));
#66955=CARTESIAN_POINT('Ctrl Pts',(-2.35225606824109,1.,-3.41117262314119));
#66956=CARTESIAN_POINT('Ctrl Pts',(-2.35898278606946,1.,-3.41511836751469));
#66957=CARTESIAN_POINT('Ctrl Pts',(-2.36573431470642,1.,-3.41903866635852));
#66958=CARTESIAN_POINT('Ctrl Pts',(-2.37251035954292,1.,-3.42293356216511));
#66959=CARTESIAN_POINT('Ctrl Pts',(-2.37931067028926,1.,-3.42680309754399));
#66960=CARTESIAN_POINT('Ctrl Pts',(-2.38613505843552,1.,-3.4306473271292));
#66961=CARTESIAN_POINT('Ctrl Pts',(-2.39298338804493,1.,-3.4344663067854));
#66962=CARTESIAN_POINT('Ctrl Pts',(-2.39848113410292,1.,-3.43750133064416));
#66963=CARTESIAN_POINT('Ctrl Pts',(-2.40261515589405,1.,-3.43976627484234));
#66964=CARTESIAN_POINT('Ctrl Pts',(-2.4053759295909,1.,-3.44127120683039));
#66965=CARTESIAN_POINT('Ctrl Pts',(-2.40675750623143,1.,-3.44202241512147));
#66966=CARTESIAN_POINT('Origin',(-2.40675750623143,0.,-3.44202241512147));
#66967=CARTESIAN_POINT('',(-2.52982887637028,1.,-3.35260583073571));
#66968=CARTESIAN_POINT('Origin',(0.,0.,0.));
#66969=CARTESIAN_POINT('',(-1.88097764062697,1.,-3.24413672884812));
#66970=CARTESIAN_POINT('Origin',(0.,1.,0.));
#66971=CARTESIAN_POINT('Ctrl Pts',(-1.88097764062697,1.,-3.24413672884812));
#66972=CARTESIAN_POINT('Ctrl Pts',(-1.88097764062697,0.666666666666667,
-3.24413672884812));
#66973=CARTESIAN_POINT('Ctrl Pts',(-1.88097764062697,0.333333333333333,
-3.24413672884812));
#66974=CARTESIAN_POINT('Ctrl Pts',(-1.88097764062697,-0.333333333333333,
-3.24413672884812));
#66975=CARTESIAN_POINT('Ctrl Pts',(-1.88097764062697,-0.666666666666667,
-3.24413672884812));
#66976=CARTESIAN_POINT('Ctrl Pts',(-1.88097764062697,-1.,-3.24413672884812));
#66977=CARTESIAN_POINT('Ctrl Pts',(-1.97421938526992,-1.,-3.70708211654725));
#66978=CARTESIAN_POINT('Ctrl Pts',(-1.97421938526992,1.,-3.70708211654725));
#66979=CARTESIAN_POINT('Ctrl Pts',(-1.97417727645308,-1.,-3.70551008132332));
#66980=CARTESIAN_POINT('Ctrl Pts',(-1.97417727645308,1.,-3.70551008132332));
#66981=CARTESIAN_POINT('Ctrl Pts',(-1.97408973726715,-1.,-3.70236698912904));
#66982=CARTESIAN_POINT('Ctrl Pts',(-1.97408973726715,1.,-3.70236698912904));
#66983=CARTESIAN_POINT('Ctrl Pts',(-1.97394846383216,-1.,-3.6976552856004));
#66984=CARTESIAN_POINT('Ctrl Pts',(-1.97394846383216,1.,-3.6976552856004));
#66985=CARTESIAN_POINT('Ctrl Pts',(-1.97374016225483,-1.,-3.69137888599902));
#66986=CARTESIAN_POINT('Ctrl Pts',(-1.97374016225483,1.,-3.69137888599902));
#66987=CARTESIAN_POINT('Ctrl Pts',(-1.97344650304519,-1.,-3.68354319915092));
#66988=CARTESIAN_POINT('Ctrl Pts',(-1.97344650304519,1.,-3.68354319915092));
#66989=CARTESIAN_POINT('Ctrl Pts',(-1.97311947678517,-1.,-3.67571738107084));
#66990=CARTESIAN_POINT('Ctrl Pts',(-1.97311947678517,1.,-3.67571738107084));
#66991=CARTESIAN_POINT('Ctrl Pts',(-1.97275897198678,-1.,-3.66790152752075));
#66992=CARTESIAN_POINT('Ctrl Pts',(-1.97275897198678,1.,-3.66790152752075));
#66993=CARTESIAN_POINT('Ctrl Pts',(-1.9723648543905,-1.,-3.6600957816636));
#66994=CARTESIAN_POINT('Ctrl Pts',(-1.9723648543905,1.,-3.6600957816636));
#66995=CARTESIAN_POINT('Ctrl Pts',(-1.9719369724024,-1.,-3.652300347166));
#66996=CARTESIAN_POINT('Ctrl Pts',(-1.9719369724024,1.,-3.652300347166));
#66997=CARTESIAN_POINT('Ctrl Pts',(-1.97147515441164,-1.,-3.64451546723514));
#66998=CARTESIAN_POINT('Ctrl Pts',(-1.97147515441164,1.,-3.64451546723514));
#66999=CARTESIAN_POINT('Ctrl Pts',(-1.97097920454464,-1.,-3.63674139590412));
#67000=CARTESIAN_POINT('Ctrl Pts',(-1.97097920454464,1.,-3.63674139590412));
#67001=CARTESIAN_POINT('Ctrl Pts',(-1.97044889850463,-1.,-3.62897836973293));
#67002=CARTESIAN_POINT('Ctrl Pts',(-1.97044889850463,1.,-3.62897836973293));
#67003=CARTESIAN_POINT('Ctrl Pts',(-1.96988398129978,-1.,-3.62122658401893));
#67004=CARTESIAN_POINT('Ctrl Pts',(-1.96988398129978,1.,-3.62122658401893));
#67005=CARTESIAN_POINT('Ctrl Pts',(-1.96928416040877,-1.,-3.61348615496704));
#67006=CARTESIAN_POINT('Ctrl Pts',(-1.96928416040877,1.,-3.61348615496704));
#67007=CARTESIAN_POINT('Ctrl Pts',(-1.9686491188594,-1.,-3.60575714017989));
#67008=CARTESIAN_POINT('Ctrl Pts',(-1.9686491188594,1.,-3.60575714017989));
#67009=CARTESIAN_POINT('Ctrl Pts',(-1.96797854118369,-1.,-3.59803959819938));
#67010=CARTESIAN_POINT('Ctrl Pts',(-1.96797854118369,1.,-3.59803959819938));
#67011=CARTESIAN_POINT('Ctrl Pts',(-1.96727213799544,-1.,-3.59033364022801));
#67012=CARTESIAN_POINT('Ctrl Pts',(-1.96727213799544,1.,-3.59033364022801));
#67013=CARTESIAN_POINT('Ctrl Pts',(-1.96652966688911,-1.,-3.58263947663829));
#67014=CARTESIAN_POINT('Ctrl Pts',(-1.96652966688911,1.,-3.58263947663829));
#67015=CARTESIAN_POINT('Ctrl Pts',(-1.96575096652789,-1.,-3.57495748600959));
#67016=CARTESIAN_POINT('Ctrl Pts',(-1.96575096652789,1.,-3.57495748600959));
#67017=CARTESIAN_POINT('Ctrl Pts',(-1.96493594634567,-1.,-3.56728820357791));
#67018=CARTESIAN_POINT('Ctrl Pts',(-1.96493594634567,1.,-3.56728820357791));
#67019=CARTESIAN_POINT('Ctrl Pts',(-1.96408450906812,-1.,-3.55963218706096));
#67020=CARTESIAN_POINT('Ctrl Pts',(-1.96408450906812,1.,-3.55963218706096));
#67021=CARTESIAN_POINT('Ctrl Pts',(-1.96319648628644,-1.,-3.55198990600886));
#67022=CARTESIAN_POINT('Ctrl Pts',(-1.96319648628644,1.,-3.55198990600886));
#67023=CARTESIAN_POINT('Ctrl Pts',(-1.96227157573067,-1.,-3.54436163300443));
#67024=CARTESIAN_POINT('Ctrl Pts',(-1.96227157573067,1.,-3.54436163300443));
#67025=CARTESIAN_POINT('Ctrl Pts',(-1.96130926212689,-1.,-3.53674730625813));
#67026=CARTESIAN_POINT('Ctrl Pts',(-1.96130926212689,1.,-3.53674730625813));
#67027=CARTESIAN_POINT('Ctrl Pts',(-1.96030879411566,-1.,-3.52914648844351));
#67028=CARTESIAN_POINT('Ctrl Pts',(-1.96030879411566,1.,-3.52914648844351));
#67029=CARTESIAN_POINT('Ctrl Pts',(-1.95926936324461,-1.,-3.52155867431486));
#67030=CARTESIAN_POINT('Ctrl Pts',(-1.95926936324461,1.,-3.52155867431486));
#67031=CARTESIAN_POINT('Ctrl Pts',(-1.95819025316779,-1.,-3.51398354617794));
#67032=CARTESIAN_POINT('Ctrl Pts',(-1.95819025316779,1.,-3.51398354617794));
#67033=CARTESIAN_POINT('Ctrl Pts',(-1.95707099606511,-1.,-3.50642124159909));
#67034=CARTESIAN_POINT('Ctrl Pts',(-1.95707099606511,1.,-3.50642124159909));
#67035=CARTESIAN_POINT('Ctrl Pts',(-1.95591153823661,-1.,-3.49887263575583));
#67036=CARTESIAN_POINT('Ctrl Pts',(-1.95591153823661,1.,-3.49887263575583));
#67037=CARTESIAN_POINT('Ctrl Pts',(-1.95471236969643,-1.,-3.49133956289133));
#67038=CARTESIAN_POINT('Ctrl Pts',(-1.95471236969643,1.,-3.49133956289133));
#67039=CARTESIAN_POINT('Ctrl Pts',(-1.95347412486309,-1.,-3.48382414832634));
#67040=CARTESIAN_POINT('Ctrl Pts',(-1.95347412486309,1.,-3.48382414832634));
#67041=CARTESIAN_POINT('Ctrl Pts',(-1.95219722189876,-1.,-3.47632820495921));
#67042=CARTESIAN_POINT('Ctrl Pts',(-1.95219722189876,1.,-3.47632820495921));
#67043=CARTESIAN_POINT('Ctrl Pts',(-1.95088147859877,-1.,-3.46885258974191));
#67044=CARTESIAN_POINT('Ctrl Pts',(-1.95088147859877,1.,-3.46885258974191));
#67045=CARTESIAN_POINT('Ctrl Pts',(-1.94952575850197,-1.,-3.46139661060962));
#67046=CARTESIAN_POINT('Ctrl Pts',(-1.94952575850197,1.,-3.46139661060962));
#67047=CARTESIAN_POINT('Ctrl Pts',(-1.94812754766524,-1.,-3.45395731584051));
#67048=CARTESIAN_POINT('Ctrl Pts',(-1.94812754766524,1.,-3.45395731584051));
#67049=CARTESIAN_POINT('Ctrl Pts',(-1.94668377715329,-1.,-3.44653088665681));
#67050=CARTESIAN_POINT('Ctrl Pts',(-1.94668377715329,1.,-3.44653088665681));
#67051=CARTESIAN_POINT('Ctrl Pts',(-1.94519168842879,-1.,-3.43911410197687));
#67052=CARTESIAN_POINT('Ctrl Pts',(-1.94519168842879,1.,-3.43911410197687));
#67053=CARTESIAN_POINT('Ctrl Pts',(-1.94364973660284,-1.,-3.43170586602434));
#67054=CARTESIAN_POINT('Ctrl Pts',(-1.94364973660284,1.,-3.43170586602434));
#67055=CARTESIAN_POINT('Ctrl Pts',(-1.94205835913696,-1.,-3.42430850941503));
#67056=CARTESIAN_POINT('Ctrl Pts',(-1.94205835913696,1.,-3.42430850941503));
#67057=CARTESIAN_POINT('Ctrl Pts',(-1.94042111965246,-1.,-3.41692971994096));
#67058=CARTESIAN_POINT('Ctrl Pts',(-1.94042111965246,1.,-3.41692971994096));
#67059=CARTESIAN_POINT('Ctrl Pts',(-1.93874306008143,-1.,-3.40957978266642));
#67060=CARTESIAN_POINT('Ctrl Pts',(-1.93874306008143,1.,-3.40957978266642));
#67061=CARTESIAN_POINT('Ctrl Pts',(-1.93702857723098,-1.,-3.40226802104109));
#67062=CARTESIAN_POINT('Ctrl Pts',(-1.93702857723098,1.,-3.40226802104109));
#67063=CARTESIAN_POINT('Ctrl Pts',(-1.93527929945985,-1.,-3.39499923640795));
#67064=CARTESIAN_POINT('Ctrl Pts',(-1.93527929945985,1.,-3.39499923640795));
#67065=CARTESIAN_POINT('Ctrl Pts',(-1.93349233176788,-1.,-3.38777076883256));
#67066=CARTESIAN_POINT('Ctrl Pts',(-1.93349233176788,1.,-3.38777076883256));
#67067=CARTESIAN_POINT('Ctrl Pts',(-1.93165739093276,-1.,-3.3805676852555));
#67068=CARTESIAN_POINT('Ctrl Pts',(-1.93165739093276,1.,-3.3805676852555));
#67069=CARTESIAN_POINT('Ctrl Pts',(-1.92975993109877,-1.,-3.37336807068043));
#67070=CARTESIAN_POINT('Ctrl Pts',(-1.92975993109877,1.,-3.37336807068043));
#67071=CARTESIAN_POINT('Ctrl Pts',(-1.92778626543786,-1.,-3.36615168657567));
#67072=CARTESIAN_POINT('Ctrl Pts',(-1.92778626543786,1.,-3.36615168657567));
#67073=CARTESIAN_POINT('Ctrl Pts',(-1.92572846125756,-1.,-3.35890824422965));
#67074=CARTESIAN_POINT('Ctrl Pts',(-1.92572846125756,1.,-3.35890824422965));
#67075=CARTESIAN_POINT('Ctrl Pts',(-1.92358838440528,-1.,-3.35164424847223));
#67076=CARTESIAN_POINT('Ctrl Pts',(-1.92358838440528,1.,-3.35164424847223));
#67077=CARTESIAN_POINT('Ctrl Pts',(-1.92138450828404,-1.,-3.34439448941961));
#67078=CARTESIAN_POINT('Ctrl Pts',(-1.92138450828404,1.,-3.34439448941961));
#67079=CARTESIAN_POINT('Ctrl Pts',(-1.9191460961021,-1.,-3.33721230710012));
#67080=CARTESIAN_POINT('Ctrl Pts',(-1.9191460961021,1.,-3.33721230710012));
#67081=CARTESIAN_POINT('Ctrl Pts',(-1.91690081930331,-1.,-3.33014884257873));
#67082=CARTESIAN_POINT('Ctrl Pts',(-1.91690081930331,1.,-3.33014884257873));
#67083=CARTESIAN_POINT('Ctrl Pts',(-1.91466343916628,-1.,-3.32323403454535));
#67084=CARTESIAN_POINT('Ctrl Pts',(-1.91466343916628,1.,-3.32323403454535));
#67085=CARTESIAN_POINT('Ctrl Pts',(-1.91242616234442,-1.,-3.31646052426364));
#67086=CARTESIAN_POINT('Ctrl Pts',(-1.91242616234442,1.,-3.31646052426364));
#67087=CARTESIAN_POINT('Ctrl Pts',(-1.91014297830446,-1.,-3.30975721158596));
#67088=CARTESIAN_POINT('Ctrl Pts',(-1.91014297830446,1.,-3.30975721158596));
#67089=CARTESIAN_POINT('Ctrl Pts',(-1.90773912171341,-1.,-3.30300595568195));
#67090=CARTESIAN_POINT('Ctrl Pts',(-1.90773912171341,1.,-3.30300595568195));
#67091=CARTESIAN_POINT('Ctrl Pts',(-1.90513891864087,-1.,-3.29608978722113));
#67092=CARTESIAN_POINT('Ctrl Pts',(-1.90513891864087,1.,-3.29608978722113));
#67093=CARTESIAN_POINT('Ctrl Pts',(-1.90228971247527,-1.,-3.2889344860029));
#67094=CARTESIAN_POINT('Ctrl Pts',(-1.90228971247527,1.,-3.2889344860029));
#67095=CARTESIAN_POINT('Ctrl Pts',(-1.89918429230462,-1.,-3.28154737912352));
#67096=CARTESIAN_POINT('Ctrl Pts',(-1.89918429230462,1.,-3.28154737912352));
#67097=CARTESIAN_POINT('Ctrl Pts',(-1.89589172903793,-1.,-3.27407108933139));
#67098=CARTESIAN_POINT('Ctrl Pts',(-1.89589172903793,1.,-3.27407108933139));
#67099=CARTESIAN_POINT('Ctrl Pts',(-1.89255393500965,-1.,-3.26677653888676));
#67100=CARTESIAN_POINT('Ctrl Pts',(-1.89255393500965,1.,-3.26677653888676));
#67101=CARTESIAN_POINT('Ctrl Pts',(-1.88934996203698,-1.,-3.25999885193947));
#67102=CARTESIAN_POINT('Ctrl Pts',(-1.88934996203698,1.,-3.25999885193947));
#67103=CARTESIAN_POINT('Ctrl Pts',(-1.88646802523466,-1.,-3.25408686339463));
#67104=CARTESIAN_POINT('Ctrl Pts',(-1.88646802523466,1.,-3.25408686339463));
#67105=CARTESIAN_POINT('Ctrl Pts',(-1.88407708646357,-1.,-3.24935200511918));
#67106=CARTESIAN_POINT('Ctrl Pts',(-1.88407708646357,1.,-3.24935200511918));
#67107=CARTESIAN_POINT('Ctrl Pts',(-1.88229202582941,-1.,-3.24600543790443));
#67108=CARTESIAN_POINT('Ctrl Pts',(-1.88229202582941,1.,-3.24600543790443));
#67109=CARTESIAN_POINT('Ctrl Pts',(-1.88139187908074,-1.,-3.24451807186481));
#67110=CARTESIAN_POINT('Ctrl Pts',(-1.88139187908074,1.,-3.24451807186481));
#67111=CARTESIAN_POINT('Ctrl Pts',(-1.88102201872555,-1.,-3.24408699284121));
#67112=CARTESIAN_POINT('Ctrl Pts',(-1.88102201872555,1.,-3.24408699284121));
#67113=CARTESIAN_POINT('Ctrl Pts',(-1.88091100680349,-1.,-3.24410359189609));
#67114=CARTESIAN_POINT('Ctrl Pts',(-1.88091100680349,1.,-3.24410359189609));
#67115=CARTESIAN_POINT('Ctrl Pts',(-1.8808893942881,-1.,-3.24418789321065));
#67116=CARTESIAN_POINT('Ctrl Pts',(-1.8808893942881,1.,-3.24418789321065));
#67117=CARTESIAN_POINT('',(-1.97421938526992,1.,-3.70708211654725));
#67118=CARTESIAN_POINT('Ctrl Pts',(-1.97421938526992,1.,-3.70708211654725));
#67119=CARTESIAN_POINT('Ctrl Pts',(-1.97417727645308,1.,-3.70551008132332));
#67120=CARTESIAN_POINT('Ctrl Pts',(-1.97408973726715,1.,-3.70236698912904));
#67121=CARTESIAN_POINT('Ctrl Pts',(-1.97394846383216,1.,-3.6976552856004));
#67122=CARTESIAN_POINT('Ctrl Pts',(-1.97374016225483,1.,-3.69137888599902));
#67123=CARTESIAN_POINT('Ctrl Pts',(-1.97344650304519,1.,-3.68354319915092));
#67124=CARTESIAN_POINT('Ctrl Pts',(-1.97311947678517,1.,-3.67571738107084));
#67125=CARTESIAN_POINT('Ctrl Pts',(-1.97275897198678,1.,-3.66790152752075));
#67126=CARTESIAN_POINT('Ctrl Pts',(-1.9723648543905,1.,-3.6600957816636));
#67127=CARTESIAN_POINT('Ctrl Pts',(-1.9719369724024,1.,-3.652300347166));
#67128=CARTESIAN_POINT('Ctrl Pts',(-1.97147515441164,1.,-3.64451546723514));
#67129=CARTESIAN_POINT('Ctrl Pts',(-1.97097920454464,1.,-3.63674139590412));
#67130=CARTESIAN_POINT('Ctrl Pts',(-1.97044889850463,1.,-3.62897836973293));
#67131=CARTESIAN_POINT('Ctrl Pts',(-1.96988398129978,1.,-3.62122658401893));
#67132=CARTESIAN_POINT('Ctrl Pts',(-1.96928416040877,1.,-3.61348615496704));
#67133=CARTESIAN_POINT('Ctrl Pts',(-1.9686491188594,1.,-3.60575714017989));
#67134=CARTESIAN_POINT('Ctrl Pts',(-1.96797854118369,1.,-3.59803959819938));
#67135=CARTESIAN_POINT('Ctrl Pts',(-1.96727213799544,1.,-3.59033364022801));
#67136=CARTESIAN_POINT('Ctrl Pts',(-1.96652966688911,1.,-3.58263947663829));
#67137=CARTESIAN_POINT('Ctrl Pts',(-1.96575096652789,1.,-3.57495748600959));
#67138=CARTESIAN_POINT('Ctrl Pts',(-1.96493594634567,1.,-3.56728820357791));
#67139=CARTESIAN_POINT('Ctrl Pts',(-1.96408450906812,1.,-3.55963218706096));
#67140=CARTESIAN_POINT('Ctrl Pts',(-1.96319648628644,1.,-3.55198990600886));
#67141=CARTESIAN_POINT('Ctrl Pts',(-1.96227157573067,1.,-3.54436163300443));
#67142=CARTESIAN_POINT('Ctrl Pts',(-1.96130926212689,1.,-3.53674730625813));
#67143=CARTESIAN_POINT('Ctrl Pts',(-1.96030879411566,1.,-3.52914648844351));
#67144=CARTESIAN_POINT('Ctrl Pts',(-1.95926936324461,1.,-3.52155867431486));
#67145=CARTESIAN_POINT('Ctrl Pts',(-1.95819025316779,1.,-3.51398354617794));
#67146=CARTESIAN_POINT('Ctrl Pts',(-1.95707099606511,1.,-3.50642124159909));
#67147=CARTESIAN_POINT('Ctrl Pts',(-1.95591153823661,1.,-3.49887263575583));
#67148=CARTESIAN_POINT('Ctrl Pts',(-1.95471236969643,1.,-3.49133956289133));
#67149=CARTESIAN_POINT('Ctrl Pts',(-1.95347412486309,1.,-3.48382414832634));
#67150=CARTESIAN_POINT('Ctrl Pts',(-1.95219722189876,1.,-3.47632820495921));
#67151=CARTESIAN_POINT('Ctrl Pts',(-1.95088147859877,1.,-3.46885258974191));
#67152=CARTESIAN_POINT('Ctrl Pts',(-1.94952575850197,1.,-3.46139661060962));
#67153=CARTESIAN_POINT('Ctrl Pts',(-1.94812754766524,1.,-3.45395731584051));
#67154=CARTESIAN_POINT('Ctrl Pts',(-1.94668377715329,1.,-3.44653088665681));
#67155=CARTESIAN_POINT('Ctrl Pts',(-1.94519168842879,1.,-3.43911410197687));
#67156=CARTESIAN_POINT('Ctrl Pts',(-1.94364973660284,1.,-3.43170586602434));
#67157=CARTESIAN_POINT('Ctrl Pts',(-1.94205835913696,1.,-3.42430850941503));
#67158=CARTESIAN_POINT('Ctrl Pts',(-1.94042111965246,1.,-3.41692971994096));
#67159=CARTESIAN_POINT('Ctrl Pts',(-1.93874306008143,1.,-3.40957978266642));
#67160=CARTESIAN_POINT('Ctrl Pts',(-1.93702857723098,1.,-3.40226802104109));
#67161=CARTESIAN_POINT('Ctrl Pts',(-1.93527929945985,1.,-3.39499923640795));
#67162=CARTESIAN_POINT('Ctrl Pts',(-1.93349233176788,1.,-3.38777076883256));
#67163=CARTESIAN_POINT('Ctrl Pts',(-1.93165739093276,1.,-3.3805676852555));
#67164=CARTESIAN_POINT('Ctrl Pts',(-1.92975993109877,1.,-3.37336807068043));
#67165=CARTESIAN_POINT('Ctrl Pts',(-1.92778626543786,1.,-3.36615168657567));
#67166=CARTESIAN_POINT('Ctrl Pts',(-1.92572846125756,1.,-3.35890824422965));
#67167=CARTESIAN_POINT('Ctrl Pts',(-1.92358838440528,1.,-3.35164424847223));
#67168=CARTESIAN_POINT('Ctrl Pts',(-1.92138450828404,1.,-3.34439448941961));
#67169=CARTESIAN_POINT('Ctrl Pts',(-1.9191460961021,1.,-3.33721230710012));
#67170=CARTESIAN_POINT('Ctrl Pts',(-1.91690081930331,1.,-3.33014884257873));
#67171=CARTESIAN_POINT('Ctrl Pts',(-1.91466343916628,1.,-3.32323403454535));
#67172=CARTESIAN_POINT('Ctrl Pts',(-1.91242616234442,1.,-3.31646052426364));
#67173=CARTESIAN_POINT('Ctrl Pts',(-1.91014297830446,1.,-3.30975721158596));
#67174=CARTESIAN_POINT('Ctrl Pts',(-1.90773912171341,1.,-3.30300595568195));
#67175=CARTESIAN_POINT('Ctrl Pts',(-1.90513891864087,1.,-3.29608978722113));
#67176=CARTESIAN_POINT('Ctrl Pts',(-1.90228971247527,1.,-3.2889344860029));
#67177=CARTESIAN_POINT('Ctrl Pts',(-1.89918429230462,1.,-3.28154737912352));
#67178=CARTESIAN_POINT('Ctrl Pts',(-1.89589172903793,1.,-3.27407108933139));
#67179=CARTESIAN_POINT('Ctrl Pts',(-1.89255393500965,1.,-3.26677653888676));
#67180=CARTESIAN_POINT('Ctrl Pts',(-1.88934996203698,1.,-3.25999885193947));
#67181=CARTESIAN_POINT('Ctrl Pts',(-1.88646802523466,1.,-3.25408686339463));
#67182=CARTESIAN_POINT('Ctrl Pts',(-1.88407708646357,1.,-3.24935200511918));
#67183=CARTESIAN_POINT('Ctrl Pts',(-1.88242596600454,1.,-3.2462565441079));
#67184=CARTESIAN_POINT('Ctrl Pts',(-1.88156537699203,1.,-3.24480754676064));
#67185=CARTESIAN_POINT('Ctrl Pts',(-1.88117508446775,1.,-3.24428080353022));
#67186=CARTESIAN_POINT('Ctrl Pts',(-1.8810229239812,1.,-3.24415531671284));
#67187=CARTESIAN_POINT('Ctrl Pts',(-1.88097764062697,1.,-3.24413672884812));
#67188=CARTESIAN_POINT('',(-1.97421938526992,0.,-3.70708211654725));
#67189=CARTESIAN_POINT('Ctrl Pts',(-1.519044091397,-1.,-3.42855728381368));
#67190=CARTESIAN_POINT('Ctrl Pts',(-1.519044091397,1.,-3.42855728381368));
#67191=CARTESIAN_POINT('Ctrl Pts',(-1.51896318668366,-1.,-3.42852521763778));
#67192=CARTESIAN_POINT('Ctrl Pts',(-1.51896318668366,1.,-3.42852521763778));
#67193=CARTESIAN_POINT('Ctrl Pts',(-1.51888450659652,-1.,-3.42860527149177));
#67194=CARTESIAN_POINT('Ctrl Pts',(-1.51888450659652,1.,-3.42860527149177));
#67195=CARTESIAN_POINT('Ctrl Pts',(-1.51901585839109,-1.,-3.42915787669893));
#67196=CARTESIAN_POINT('Ctrl Pts',(-1.51901585839109,1.,-3.42915787669893));
#67197=CARTESIAN_POINT('Ctrl Pts',(-1.51969006980999,-1.,-3.43076036253837));
#67198=CARTESIAN_POINT('Ctrl Pts',(-1.51969006980999,1.,-3.43076036253837));
#67199=CARTESIAN_POINT('Ctrl Pts',(-1.52134826724293,-1.,-3.43417156977893));
#67200=CARTESIAN_POINT('Ctrl Pts',(-1.52134826724293,1.,-3.43417156977893));
#67201=CARTESIAN_POINT('Ctrl Pts',(-1.5237734895035,-1.,-3.4388889597401));
#67202=CARTESIAN_POINT('Ctrl Pts',(-1.5237734895035,1.,-3.4388889597401));
#67203=CARTESIAN_POINT('Ctrl Pts',(-1.52686242875556,-1.,-3.44469547526647));
#67204=CARTESIAN_POINT('Ctrl Pts',(-1.52686242875556,1.,-3.44469547526647));
#67205=CARTESIAN_POINT('Ctrl Pts',(-1.53046244461635,-1.,-3.45127136828305));
#67206=CARTESIAN_POINT('Ctrl Pts',(-1.53046244461635,1.,-3.45127136828305));
#67207=CARTESIAN_POINT('Ctrl Pts',(-1.53440195378792,-1.,-3.45825932955032));
#67208=CARTESIAN_POINT('Ctrl Pts',(-1.53440195378792,1.,-3.45825932955032));
#67209=CARTESIAN_POINT('Ctrl Pts',(-1.53851507915502,-1.,-3.46531752207153));
#67210=CARTESIAN_POINT('Ctrl Pts',(-1.53851507915502,1.,-3.46531752207153));
#67211=CARTESIAN_POINT('Ctrl Pts',(-1.54266605398187,-1.,-3.47217189224653));
#67212=CARTESIAN_POINT('Ctrl Pts',(-1.54266605398187,1.,-3.47217189224653));
#67213=CARTESIAN_POINT('Ctrl Pts',(-1.54678009290276,-1.,-3.47868272898751));
#67214=CARTESIAN_POINT('Ctrl Pts',(-1.54678009290276,1.,-3.47868272898751));
#67215=CARTESIAN_POINT('Ctrl Pts',(-1.55084702970452,-1.,-3.48485155928567));
#67216=CARTESIAN_POINT('Ctrl Pts',(-1.55084702970452,1.,-3.48485155928567));
#67217=CARTESIAN_POINT('Ctrl Pts',(-1.55489595901116,-1.,-3.4907646087742));
#67218=CARTESIAN_POINT('Ctrl Pts',(-1.55489595901116,1.,-3.4907646087742));
#67219=CARTESIAN_POINT('Ctrl Pts',(-1.55897703097874,-1.,-3.49655185179655));
#67220=CARTESIAN_POINT('Ctrl Pts',(-1.55897703097874,1.,-3.49655185179655));
#67221=CARTESIAN_POINT('Ctrl Pts',(-1.56314187758675,-1.,-3.50234321621578));
#67222=CARTESIAN_POINT('Ctrl Pts',(-1.56314187758675,1.,-3.50234321621578));
#67223=CARTESIAN_POINT('Ctrl Pts',(-1.56742097575012,-1.,-3.50821771695363));
#67224=CARTESIAN_POINT('Ctrl Pts',(-1.56742097575012,1.,-3.50821771695363));
#67225=CARTESIAN_POINT('Ctrl Pts',(-1.57181569799743,-1.,-3.51418598431665));
#67226=CARTESIAN_POINT('Ctrl Pts',(-1.57181569799743,1.,-3.51418598431665));
#67227=CARTESIAN_POINT('Ctrl Pts',(-1.57631049988158,-1.,-3.52021847865912));
#67228=CARTESIAN_POINT('Ctrl Pts',(-1.57631049988158,1.,-3.52021847865912));
#67229=CARTESIAN_POINT('Ctrl Pts',(-1.58088027227848,-1.,-3.52626275334881));
#67230=CARTESIAN_POINT('Ctrl Pts',(-1.58088027227848,1.,-3.52626275334881));
#67231=CARTESIAN_POINT('Ctrl Pts',(-1.58549906268088,-1.,-3.5322637814708));
#67232=CARTESIAN_POINT('Ctrl Pts',(-1.58549906268088,1.,-3.5322637814708));
#67233=CARTESIAN_POINT('Ctrl Pts',(-1.59014958368739,-1.,-3.53818616861077));
#67234=CARTESIAN_POINT('Ctrl Pts',(-1.59014958368739,1.,-3.53818616861077));
#67235=CARTESIAN_POINT('Ctrl Pts',(-1.59482766949766,-1.,-3.54402458182337));
#67236=CARTESIAN_POINT('Ctrl Pts',(-1.59482766949766,1.,-3.54402458182337));
#67237=CARTESIAN_POINT('Ctrl Pts',(-1.59953698113457,-1.,-3.54979148634454));
#67238=CARTESIAN_POINT('Ctrl Pts',(-1.59953698113457,1.,-3.54979148634454));
#67239=CARTESIAN_POINT('Ctrl Pts',(-1.60428584699853,-1.,-3.55550985096129));
#67240=CARTESIAN_POINT('Ctrl Pts',(-1.60428584699853,1.,-3.55550985096129));
#67241=CARTESIAN_POINT('Ctrl Pts',(-1.60908344685457,-1.,-3.5612043248298));
#67242=CARTESIAN_POINT('Ctrl Pts',(-1.60908344685457,1.,-3.5612043248298));
#67243=CARTESIAN_POINT('Ctrl Pts',(-1.61393581747514,-1.,-3.56689200468387));
#67244=CARTESIAN_POINT('Ctrl Pts',(-1.61393581747514,1.,-3.56689200468387));
#67245=CARTESIAN_POINT('Ctrl Pts',(-1.61884340915404,-1.,-3.57257679609806));
#67246=CARTESIAN_POINT('Ctrl Pts',(-1.61884340915404,1.,-3.57257679609806));
#67247=CARTESIAN_POINT('Ctrl Pts',(-1.62380329464844,-1.,-3.5782545595439));
#67248=CARTESIAN_POINT('Ctrl Pts',(-1.62380329464844,1.,-3.5782545595439));
#67249=CARTESIAN_POINT('Ctrl Pts',(-1.62881051550745,-1.,-3.58391625774343));
#67250=CARTESIAN_POINT('Ctrl Pts',(-1.62881051550745,1.,-3.58391625774343));
#67251=CARTESIAN_POINT('Ctrl Pts',(-1.6338597145126,-1.,-3.58955176627879));
#67252=CARTESIAN_POINT('Ctrl Pts',(-1.6338597145126,1.,-3.58955176627879));
#67253=CARTESIAN_POINT('Ctrl Pts',(-1.63894676675352,-1.,-3.59515368334893));
#67254=CARTESIAN_POINT('Ctrl Pts',(-1.63894676675352,1.,-3.59515368334893));
#67255=CARTESIAN_POINT('Ctrl Pts',(-1.64407004385582,-1.,-3.60072028513845));
#67256=CARTESIAN_POINT('Ctrl Pts',(-1.64407004385582,1.,-3.60072028513845));
#67257=CARTESIAN_POINT('Ctrl Pts',(-1.64922952425832,-1.,-3.60625346556992));
#67258=CARTESIAN_POINT('Ctrl Pts',(-1.64922952425832,1.,-3.60625346556992));
#67259=CARTESIAN_POINT('Ctrl Pts',(-1.65442619244325,-1.,-3.61175734965127));
#67260=CARTESIAN_POINT('Ctrl Pts',(-1.65442619244325,1.,-3.61175734965127));
#67261=CARTESIAN_POINT('Ctrl Pts',(-1.65966133399186,-1.,-3.61723666482456));
#67262=CARTESIAN_POINT('Ctrl Pts',(-1.65966133399186,1.,-3.61723666482456));
#67263=CARTESIAN_POINT('Ctrl Pts',(-1.66493585923855,-1.,-3.62269517989109));
#67264=CARTESIAN_POINT('Ctrl Pts',(-1.66493585923855,1.,-3.62269517989109));
#67265=CARTESIAN_POINT('Ctrl Pts',(-1.67024966008045,-1.,-3.62813422105271));
#67266=CARTESIAN_POINT('Ctrl Pts',(-1.67024966008045,1.,-3.62813422105271));
#67267=CARTESIAN_POINT('Ctrl Pts',(-1.67560193613156,-1.,-3.63355343201232));
#67268=CARTESIAN_POINT('Ctrl Pts',(-1.67560193613156,1.,-3.63355343201232));
#67269=CARTESIAN_POINT('Ctrl Pts',(-1.68099146651586,-1.,-3.63895140887462));
#67270=CARTESIAN_POINT('Ctrl Pts',(-1.68099146651586,1.,-3.63895140887462));
#67271=CARTESIAN_POINT('Ctrl Pts',(-1.68641690471457,-1.,-3.64432638915203));
#67272=CARTESIAN_POINT('Ctrl Pts',(-1.68641690471457,1.,-3.64432638915203));
#67273=CARTESIAN_POINT('Ctrl Pts',(-1.69187705481689,-1.,-3.64967689827371));
#67274=CARTESIAN_POINT('Ctrl Pts',(-1.69187705481689,1.,-3.64967689827371));
#67275=CARTESIAN_POINT('Ctrl Pts',(-1.69737117722534,-1.,-3.65500246526749));
#67276=CARTESIAN_POINT('Ctrl Pts',(-1.69737117722534,1.,-3.65500246526749));
#67277=CARTESIAN_POINT('Ctrl Pts',(-1.70289888566873,-1.,-3.66030338774847));
#67278=CARTESIAN_POINT('Ctrl Pts',(-1.70289888566873,1.,-3.66030338774847));
#67279=CARTESIAN_POINT('Ctrl Pts',(-1.70846001610956,-1.,-3.66558043198876));
#67280=CARTESIAN_POINT('Ctrl Pts',(-1.70846001610956,1.,-3.66558043198876));
#67281=CARTESIAN_POINT('Ctrl Pts',(-1.71405450210384,-1.,-3.67083454901611));
#67282=CARTESIAN_POINT('Ctrl Pts',(-1.71405450210384,1.,-3.67083454901611));
#67283=CARTESIAN_POINT('Ctrl Pts',(-1.71968225581808,-1.,-3.67606660374709));
#67284=CARTESIAN_POINT('Ctrl Pts',(-1.71968225581808,1.,-3.67606660374709));
#67285=CARTESIAN_POINT('Ctrl Pts',(-1.72534302437056,-1.,-3.68127704936579));
#67286=CARTESIAN_POINT('Ctrl Pts',(-1.72534302437056,1.,-3.68127704936579));
#67287=CARTESIAN_POINT('Ctrl Pts',(-1.73103640956717,-1.,-3.68646597019332));
#67288=CARTESIAN_POINT('Ctrl Pts',(-1.73103640956717,1.,-3.68646597019332));
#67289=CARTESIAN_POINT('Ctrl Pts',(-1.73676193254557,-1.,-3.69163322648036));
#67290=CARTESIAN_POINT('Ctrl Pts',(-1.73676193254557,1.,-3.69163322648036));
#67291=CARTESIAN_POINT('Ctrl Pts',(-1.74251908492617,-1.,-3.69677856910517));
#67292=CARTESIAN_POINT('Ctrl Pts',(-1.74251908492617,1.,-3.69677856910517));
#67293=CARTESIAN_POINT('Ctrl Pts',(-1.74830738046057,-1.,-3.7019017567335));
#67294=CARTESIAN_POINT('Ctrl Pts',(-1.74830738046057,1.,-3.7019017567335));
#67295=CARTESIAN_POINT('Ctrl Pts',(-1.75412641804042,-1.,-3.70700269736659));
#67296=CARTESIAN_POINT('Ctrl Pts',(-1.75412641804042,1.,-3.70700269736659));
#67297=CARTESIAN_POINT('Ctrl Pts',(-1.75997588498865,-1.,-3.71208146346136));
#67298=CARTESIAN_POINT('Ctrl Pts',(-1.75997588498865,1.,-3.71208146346136));
#67299=CARTESIAN_POINT('Ctrl Pts',(-1.76585552124394,-1.,-3.71713822377359));
#67300=CARTESIAN_POINT('Ctrl Pts',(-1.76585552124394,1.,-3.71713822377359));
#67301=CARTESIAN_POINT('Ctrl Pts',(-1.77176509401761,-1.,-3.72217319911254));
#67302=CARTESIAN_POINT('Ctrl Pts',(-1.77176509401761,1.,-3.72217319911254));
#67303=CARTESIAN_POINT('Ctrl Pts',(-1.77770437039658,-1.,-3.72718661205609));
#67304=CARTESIAN_POINT('Ctrl Pts',(-1.77770437039658,1.,-3.72718661205609));
#67305=CARTESIAN_POINT('Ctrl Pts',(-1.78367308442901,-1.,-3.7321786309547));
#67306=CARTESIAN_POINT('Ctrl Pts',(-1.78367308442901,1.,-3.7321786309547));
#67307=CARTESIAN_POINT('Ctrl Pts',(-1.78967092823491,-1.,-3.73714934730681));
#67308=CARTESIAN_POINT('Ctrl Pts',(-1.78967092823491,1.,-3.73714934730681));
#67309=CARTESIAN_POINT('Ctrl Pts',(-1.79569757859422,-1.,-3.74209880352445));
#67310=CARTESIAN_POINT('Ctrl Pts',(-1.79569757859422,1.,-3.74209880352445));
#67311=CARTESIAN_POINT('Ctrl Pts',(-1.8017527148577,-1.,-3.74702700875467));
#67312=CARTESIAN_POINT('Ctrl Pts',(-1.8017527148577,1.,-3.74702700875467));
#67313=CARTESIAN_POINT('Ctrl Pts',(-1.80783603939617,-1.,-3.75193395887977));
#67314=CARTESIAN_POINT('Ctrl Pts',(-1.80783603939617,1.,-3.75193395887977));
#67315=CARTESIAN_POINT('Ctrl Pts',(-1.8139472983358,-1.,-3.75681965683071));
#67316=CARTESIAN_POINT('Ctrl Pts',(-1.8139472983358,1.,-3.75681965683071));
#67317=CARTESIAN_POINT('Ctrl Pts',(-1.82008629694091,-1.,-3.76168412707948));
#67318=CARTESIAN_POINT('Ctrl Pts',(-1.82008629694091,1.,-3.76168412707948));
#67319=CARTESIAN_POINT('Ctrl Pts',(-1.82625289220915,-1.,-3.76652740353775));
#67320=CARTESIAN_POINT('Ctrl Pts',(-1.82625289220915,1.,-3.76652740353775));
#67321=CARTESIAN_POINT('Ctrl Pts',(-1.83120816955645,-1.,-3.77038509817999));
#67322=CARTESIAN_POINT('Ctrl Pts',(-1.83120816955645,1.,-3.77038509817999));
#67323=CARTESIAN_POINT('Ctrl Pts',(-1.83493697934534,-1.,-3.77326886064398));
#67324=CARTESIAN_POINT('Ctrl Pts',(-1.83493697934534,1.,-3.77326886064398));
#67325=CARTESIAN_POINT('Ctrl Pts',(-1.83742834010626,-1.,-3.77518714457833));
#67326=CARTESIAN_POINT('Ctrl Pts',(-1.83742834010626,1.,-3.77518714457833));
#67327=CARTESIAN_POINT('Ctrl Pts',(-1.83867539237861,-1.,-3.77614523045147));
#67328=CARTESIAN_POINT('Ctrl Pts',(-1.83867539237861,1.,-3.77614523045147));
#67329=CARTESIAN_POINT('',(-1.5189508286633,1.,-3.42859860294306));
#67330=CARTESIAN_POINT('Ctrl Pts',(-1.5189508286633,-1.,-3.42859860294306));
#67331=CARTESIAN_POINT('Ctrl Pts',(-1.5189508286633,-0.666666666666667,
-3.42859860294306));
#67332=CARTESIAN_POINT('Ctrl Pts',(-1.5189508286633,-0.333333333333333,
-3.42859860294306));
#67333=CARTESIAN_POINT('Ctrl Pts',(-1.5189508286633,0.333333333333333,-3.42859860294306));
#67334=CARTESIAN_POINT('Ctrl Pts',(-1.5189508286633,0.666666666666667,-3.42859860294305));
#67335=CARTESIAN_POINT('Ctrl Pts',(-1.5189508286633,1.,-3.42859860294305));
#67336=CARTESIAN_POINT('',(-1.83867539237861,1.,-3.77614523045147));
#67337=CARTESIAN_POINT('',(-1.83867539237861,0.,-3.77614523045147));
#67338=CARTESIAN_POINT('Ctrl Pts',(-1.5189508286633,1.,-3.42859860294306));
#67339=CARTESIAN_POINT('Ctrl Pts',(-1.51893924967331,1.,-3.42864616361875));
#67340=CARTESIAN_POINT('Ctrl Pts',(-1.5189513329503,1.,-3.42884302333841));
#67341=CARTESIAN_POINT('Ctrl Pts',(-1.51914806898491,1.,-3.42946838852588));
#67342=CARTESIAN_POINT('Ctrl Pts',(-1.5198144909338,1.,-3.43101631893414));
#67343=CARTESIAN_POINT('Ctrl Pts',(-1.52134826724293,1.,-3.43417156977893));
#67344=CARTESIAN_POINT('Ctrl Pts',(-1.5237734895035,1.,-3.4388889597401));
#67345=CARTESIAN_POINT('Ctrl Pts',(-1.52686242875556,1.,-3.44469547526647));
#67346=CARTESIAN_POINT('Ctrl Pts',(-1.53046244461635,1.,-3.45127136828305));
#67347=CARTESIAN_POINT('Ctrl Pts',(-1.53440195378792,1.,-3.45825932955032));
#67348=CARTESIAN_POINT('Ctrl Pts',(-1.53851507915502,1.,-3.46531752207153));
#67349=CARTESIAN_POINT('Ctrl Pts',(-1.54266605398187,1.,-3.47217189224653));
#67350=CARTESIAN_POINT('Ctrl Pts',(-1.54678009290276,1.,-3.47868272898751));
#67351=CARTESIAN_POINT('Ctrl Pts',(-1.55084702970452,1.,-3.48485155928567));
#67352=CARTESIAN_POINT('Ctrl Pts',(-1.55489595901116,1.,-3.4907646087742));
#67353=CARTESIAN_POINT('Ctrl Pts',(-1.55897703097874,1.,-3.49655185179655));
#67354=CARTESIAN_POINT('Ctrl Pts',(-1.56314187758675,1.,-3.50234321621578));
#67355=CARTESIAN_POINT('Ctrl Pts',(-1.56742097575012,1.,-3.50821771695363));
#67356=CARTESIAN_POINT('Ctrl Pts',(-1.57181569799743,1.,-3.51418598431665));
#67357=CARTESIAN_POINT('Ctrl Pts',(-1.57631049988158,1.,-3.52021847865912));
#67358=CARTESIAN_POINT('Ctrl Pts',(-1.58088027227848,1.,-3.52626275334881));
#67359=CARTESIAN_POINT('Ctrl Pts',(-1.58549906268088,1.,-3.5322637814708));
#67360=CARTESIAN_POINT('Ctrl Pts',(-1.59014958368739,1.,-3.53818616861077));
#67361=CARTESIAN_POINT('Ctrl Pts',(-1.59482766949766,1.,-3.54402458182337));
#67362=CARTESIAN_POINT('Ctrl Pts',(-1.59953698113457,1.,-3.54979148634454));
#67363=CARTESIAN_POINT('Ctrl Pts',(-1.60428584699853,1.,-3.55550985096129));
#67364=CARTESIAN_POINT('Ctrl Pts',(-1.60908344685457,1.,-3.5612043248298));
#67365=CARTESIAN_POINT('Ctrl Pts',(-1.61393581747514,1.,-3.56689200468387));
#67366=CARTESIAN_POINT('Ctrl Pts',(-1.61884340915404,1.,-3.57257679609806));
#67367=CARTESIAN_POINT('Ctrl Pts',(-1.62380329464844,1.,-3.5782545595439));
#67368=CARTESIAN_POINT('Ctrl Pts',(-1.62881051550745,1.,-3.58391625774343));
#67369=CARTESIAN_POINT('Ctrl Pts',(-1.6338597145126,1.,-3.58955176627879));
#67370=CARTESIAN_POINT('Ctrl Pts',(-1.63894676675352,1.,-3.59515368334893));
#67371=CARTESIAN_POINT('Ctrl Pts',(-1.64407004385582,1.,-3.60072028513845));
#67372=CARTESIAN_POINT('Ctrl Pts',(-1.64922952425832,1.,-3.60625346556992));
#67373=CARTESIAN_POINT('Ctrl Pts',(-1.65442619244325,1.,-3.61175734965127));
#67374=CARTESIAN_POINT('Ctrl Pts',(-1.65966133399186,1.,-3.61723666482456));
#67375=CARTESIAN_POINT('Ctrl Pts',(-1.66493585923855,1.,-3.62269517989109));
#67376=CARTESIAN_POINT('Ctrl Pts',(-1.67024966008045,1.,-3.62813422105271));
#67377=CARTESIAN_POINT('Ctrl Pts',(-1.67560193613156,1.,-3.63355343201232));
#67378=CARTESIAN_POINT('Ctrl Pts',(-1.68099146651586,1.,-3.63895140887462));
#67379=CARTESIAN_POINT('Ctrl Pts',(-1.68641690471457,1.,-3.64432638915203));
#67380=CARTESIAN_POINT('Ctrl Pts',(-1.69187705481689,1.,-3.64967689827371));
#67381=CARTESIAN_POINT('Ctrl Pts',(-1.69737117722534,1.,-3.65500246526749));
#67382=CARTESIAN_POINT('Ctrl Pts',(-1.70289888566873,1.,-3.66030338774847));
#67383=CARTESIAN_POINT('Ctrl Pts',(-1.70846001610956,1.,-3.66558043198876));
#67384=CARTESIAN_POINT('Ctrl Pts',(-1.71405450210384,1.,-3.67083454901611));
#67385=CARTESIAN_POINT('Ctrl Pts',(-1.71968225581808,1.,-3.67606660374709));
#67386=CARTESIAN_POINT('Ctrl Pts',(-1.72534302437056,1.,-3.68127704936579));
#67387=CARTESIAN_POINT('Ctrl Pts',(-1.73103640956717,1.,-3.68646597019332));
#67388=CARTESIAN_POINT('Ctrl Pts',(-1.73676193254557,1.,-3.69163322648036));
#67389=CARTESIAN_POINT('Ctrl Pts',(-1.74251908492617,1.,-3.69677856910517));
#67390=CARTESIAN_POINT('Ctrl Pts',(-1.74830738046057,1.,-3.7019017567335));
#67391=CARTESIAN_POINT('Ctrl Pts',(-1.75412641804042,1.,-3.70700269736659));
#67392=CARTESIAN_POINT('Ctrl Pts',(-1.75997588498865,1.,-3.71208146346136));
#67393=CARTESIAN_POINT('Ctrl Pts',(-1.76585552124394,1.,-3.71713822377359));
#67394=CARTESIAN_POINT('Ctrl Pts',(-1.77176509401761,1.,-3.72217319911254));
#67395=CARTESIAN_POINT('Ctrl Pts',(-1.77770437039658,1.,-3.72718661205609));
#67396=CARTESIAN_POINT('Ctrl Pts',(-1.78367308442901,1.,-3.7321786309547));
#67397=CARTESIAN_POINT('Ctrl Pts',(-1.78967092823491,1.,-3.73714934730681));
#67398=CARTESIAN_POINT('Ctrl Pts',(-1.79569757859422,1.,-3.74209880352445));
#67399=CARTESIAN_POINT('Ctrl Pts',(-1.8017527148577,1.,-3.74702700875467));
#67400=CARTESIAN_POINT('Ctrl Pts',(-1.80783603939617,1.,-3.75193395887977));
#67401=CARTESIAN_POINT('Ctrl Pts',(-1.8139472983358,1.,-3.75681965683071));
#67402=CARTESIAN_POINT('Ctrl Pts',(-1.82008629694091,1.,-3.76168412707948));
#67403=CARTESIAN_POINT('Ctrl Pts',(-1.82625289220915,1.,-3.76652740353775));
#67404=CARTESIAN_POINT('Ctrl Pts',(-1.83120816955645,1.,-3.77038509817999));
#67405=CARTESIAN_POINT('Ctrl Pts',(-1.83493697934534,1.,-3.77326886064398));
#67406=CARTESIAN_POINT('Ctrl Pts',(-1.83742834010626,1.,-3.77518714457833));
#67407=CARTESIAN_POINT('Ctrl Pts',(-1.83867539237861,1.,-3.77614523045147));
#67408=CARTESIAN_POINT('Origin',(-1.83867539237861,0.,-3.77614523045147));
#67409=CARTESIAN_POINT('',(-1.97421938526992,1.,-3.70708211654725));
#67410=CARTESIAN_POINT('Origin',(0.,0.,0.));
#67411=CARTESIAN_POINT('',(-1.35032489087269,1.,-3.49844575334386));
#67412=CARTESIAN_POINT('Origin',(0.,1.,0.));
#67413=CARTESIAN_POINT('Ctrl Pts',(-1.35032489087269,1.,-3.49844575334386));
#67414=CARTESIAN_POINT('Ctrl Pts',(-1.35032489087269,0.666666666666667,
-3.49844575334386));
#67415=CARTESIAN_POINT('Ctrl Pts',(-1.35032489087269,0.333333333333333,
-3.49844575334386));
#67416=CARTESIAN_POINT('Ctrl Pts',(-1.35032489087269,-0.333333333333333,
-3.49844575334386));
#67417=CARTESIAN_POINT('Ctrl Pts',(-1.35032489087269,-0.666666666666667,
-3.49844575334386));
#67418=CARTESIAN_POINT('Ctrl Pts',(-1.35032489087269,-1.,-3.49844575334386));
#67419=CARTESIAN_POINT('Ctrl Pts',(-1.36999806084572,-1.,-3.97027773754922));
#67420=CARTESIAN_POINT('Ctrl Pts',(-1.36999806084572,1.,-3.97027773754922));
#67421=CARTESIAN_POINT('Ctrl Pts',(-1.37020239094758,-1.,-3.9687184694173));
#67422=CARTESIAN_POINT('Ctrl Pts',(-1.37020239094758,1.,-3.9687184694173));
#67423=CARTESIAN_POINT('Ctrl Pts',(-1.37060761746027,-1.,-3.96560037975788));
#67424=CARTESIAN_POINT('Ctrl Pts',(-1.37060761746027,1.,-3.96560037975788));
#67425=CARTESIAN_POINT('Ctrl Pts',(-1.37120515615663,-1.,-3.96092458508407));
#67426=CARTESIAN_POINT('Ctrl Pts',(-1.37120515615663,1.,-3.96092458508407));
#67427=CARTESIAN_POINT('Ctrl Pts',(-1.37198126433139,-1.,-3.95469287283105));
#67428=CARTESIAN_POINT('Ctrl Pts',(-1.37198126433139,1.,-3.95469287283105));
#67429=CARTESIAN_POINT('Ctrl Pts',(-1.37291699203423,-1.,-3.94690771786926));
#67430=CARTESIAN_POINT('Ctrl Pts',(-1.37291699203423,1.,-3.94690771786926));
#67431=CARTESIAN_POINT('Ctrl Pts',(-1.37381821967499,-1.,-3.93912709041791));
#67432=CARTESIAN_POINT('Ctrl Pts',(-1.37381821967499,1.,-3.93912709041791));
#67433=CARTESIAN_POINT('Ctrl Pts',(-1.37468482215784,-1.,-3.93135106761941));
#67434=CARTESIAN_POINT('Ctrl Pts',(-1.37468482215784,1.,-3.93135106761941));
#67435=CARTESIAN_POINT('Ctrl Pts',(-1.37551664448057,-1.,-3.92357976987132));
#67436=CARTESIAN_POINT('Ctrl Pts',(-1.37551664448057,1.,-3.92357976987132));
#67437=CARTESIAN_POINT('Ctrl Pts',(-1.37631350505516,-1.,-3.91581337461825));
#67438=CARTESIAN_POINT('Ctrl Pts',(-1.37631350505516,1.,-3.91581337461825));
#67439=CARTESIAN_POINT('Ctrl Pts',(-1.3770751963376,-1.,-3.90805209522729));
#67440=CARTESIAN_POINT('Ctrl Pts',(-1.3770751963376,1.,-3.90805209522729));
#67441=CARTESIAN_POINT('Ctrl Pts',(-1.3778014851263,-1.,-3.90029615196255));
#67442=CARTESIAN_POINT('Ctrl Pts',(-1.3778014851263,1.,-3.90029615196255));
#67443=CARTESIAN_POINT('Ctrl Pts',(-1.37849211287981,-1.,-3.89254574338385));
#67444=CARTESIAN_POINT('Ctrl Pts',(-1.37849211287981,1.,-3.89254574338385));
#67445=CARTESIAN_POINT('Ctrl Pts',(-1.37914679719446,-1.,-3.88480102249461));
#67446=CARTESIAN_POINT('Ctrl Pts',(-1.37914679719446,1.,-3.88480102249461));
#67447=CARTESIAN_POINT('Ctrl Pts',(-1.37976523097187,-1.,-3.87706205830865));
#67448=CARTESIAN_POINT('Ctrl Pts',(-1.37976523097187,1.,-3.87706205830865));
#67449=CARTESIAN_POINT('Ctrl Pts',(-1.38034709213129,-1.,-3.86932885813403));
#67450=CARTESIAN_POINT('Ctrl Pts',(-1.38034709213129,1.,-3.86932885813403));
#67451=CARTESIAN_POINT('Ctrl Pts',(-1.38089205993067,-1.,-3.86160143044187));
#67452=CARTESIAN_POINT('Ctrl Pts',(-1.38089205993067,1.,-3.86160143044187));
#67453=CARTESIAN_POINT('Ctrl Pts',(-1.38139983115075,-1.,-3.85387983979557));
#67454=CARTESIAN_POINT('Ctrl Pts',(-1.38139983115075,1.,-3.85387983979557));
#67455=CARTESIAN_POINT('Ctrl Pts',(-1.38187013346089,-1.,-3.84616425605705));
#67456=CARTESIAN_POINT('Ctrl Pts',(-1.38187013346089,1.,-3.84616425605705));
#67457=CARTESIAN_POINT('Ctrl Pts',(-1.38230274828774,-1.,-3.83845502790609));
#67458=CARTESIAN_POINT('Ctrl Pts',(-1.38230274828774,1.,-3.83845502790609));
#67459=CARTESIAN_POINT('Ctrl Pts',(-1.38269750245086,-1.,-3.83075266982138));
#67460=CARTESIAN_POINT('Ctrl Pts',(-1.38269750245086,1.,-3.83075266982138));
#67461=CARTESIAN_POINT('Ctrl Pts',(-1.38305421262724,-1.,-3.82305771743715));
#67462=CARTESIAN_POINT('Ctrl Pts',(-1.38305421262724,1.,-3.82305771743715));
#67463=CARTESIAN_POINT('Ctrl Pts',(-1.38337263902766,-1.,-3.81537060817765));
#67464=CARTESIAN_POINT('Ctrl Pts',(-1.38337263902766,1.,-3.81537060817765));
#67465=CARTESIAN_POINT('Ctrl Pts',(-1.38365244046226,-1.,-3.80769156398429));
#67466=CARTESIAN_POINT('Ctrl Pts',(-1.38365244046226,1.,-3.80769156398429));
#67467=CARTESIAN_POINT('Ctrl Pts',(-1.38389311766701,-1.,-3.80002044322169));
#67468=CARTESIAN_POINT('Ctrl Pts',(-1.38389311766701,1.,-3.80002044322169));
#67469=CARTESIAN_POINT('Ctrl Pts',(-1.38409399694589,-1.,-3.79235669640907));
#67470=CARTESIAN_POINT('Ctrl Pts',(-1.38409399694589,1.,-3.79235669640907));
#67471=CARTESIAN_POINT('Ctrl Pts',(-1.38425435883773,-1.,-3.78469969805134));
#67472=CARTESIAN_POINT('Ctrl Pts',(-1.38425435883773,1.,-3.78469969805134));
#67473=CARTESIAN_POINT('Ctrl Pts',(-1.38437354551435,-1.,-3.77704902230441));
#67474=CARTESIAN_POINT('Ctrl Pts',(-1.38437354551435,1.,-3.77704902230441));
#67475=CARTESIAN_POINT('Ctrl Pts',(-1.38445107339517,-1.,-3.76940473185775));
#67476=CARTESIAN_POINT('Ctrl Pts',(-1.38445107339517,1.,-3.76940473185775));
#67477=CARTESIAN_POINT('Ctrl Pts',(-1.38448675253343,-1.,-3.76176768271347));
#67478=CARTESIAN_POINT('Ctrl Pts',(-1.38448675253343,1.,-3.76176768271347));
#67479=CARTESIAN_POINT('Ctrl Pts',(-1.38448077997155,-1.,-3.75413976318727));
#67480=CARTESIAN_POINT('Ctrl Pts',(-1.38448077997155,1.,-3.75413976318727));
#67481=CARTESIAN_POINT('Ctrl Pts',(-1.38443344984389,-1.,-3.7465231716786));
#67482=CARTESIAN_POINT('Ctrl Pts',(-1.38443344984389,1.,-3.7465231716786));
#67483=CARTESIAN_POINT('Ctrl Pts',(-1.38434489156456,-1.,-3.73891976418099));
#67484=CARTESIAN_POINT('Ctrl Pts',(-1.38434489156456,1.,-3.73891976418099));
#67485=CARTESIAN_POINT('Ctrl Pts',(-1.38421479111531,-1.,-3.73133035859283));
#67486=CARTESIAN_POINT('Ctrl Pts',(-1.38421479111531,1.,-3.73133035859283));
#67487=CARTESIAN_POINT('Ctrl Pts',(-1.3840421342895,-1.,-3.72375409358805));
#67488=CARTESIAN_POINT('Ctrl Pts',(-1.3840421342895,1.,-3.72375409358805));
#67489=CARTESIAN_POINT('Ctrl Pts',(-1.38382489984585,-1.,-3.7161876605181));
#67490=CARTESIAN_POINT('Ctrl Pts',(-1.38382489984585,1.,-3.7161876605181));
#67491=CARTESIAN_POINT('Ctrl Pts',(-1.38356065402122,-1.,-3.70862680753343));
#67492=CARTESIAN_POINT('Ctrl Pts',(-1.38356065402122,1.,-3.70862680753343));
#67493=CARTESIAN_POINT('Ctrl Pts',(-1.38324717612862,-1.,-3.70106792167894));
#67494=CARTESIAN_POINT('Ctrl Pts',(-1.38324717612862,1.,-3.70106792167894));
#67495=CARTESIAN_POINT('Ctrl Pts',(-1.38288311171649,-1.,-3.69350967899523));
#67496=CARTESIAN_POINT('Ctrl Pts',(-1.38288311171649,1.,-3.69350967899523));
#67497=CARTESIAN_POINT('Ctrl Pts',(-1.38246852827185,-1.,-3.68595444983844));
#67498=CARTESIAN_POINT('Ctrl Pts',(-1.38246852827185,1.,-3.68595444983844));
#67499=CARTESIAN_POINT('Ctrl Pts',(-1.38200574290626,-1.,-3.6784103848243));
#67500=CARTESIAN_POINT('Ctrl Pts',(-1.38200574290626,1.,-3.6784103848243));
#67501=CARTESIAN_POINT('Ctrl Pts',(-1.38149812653876,-1.,-3.67088843112282));
#67502=CARTESIAN_POINT('Ctrl Pts',(-1.38149812653876,1.,-3.67088843112282));
#67503=CARTESIAN_POINT('Ctrl Pts',(-1.38094856333558,-1.,-3.66339848520874));
#67504=CARTESIAN_POINT('Ctrl Pts',(-1.38094856333558,1.,-3.66339848520874));
#67505=CARTESIAN_POINT('Ctrl Pts',(-1.38035791051215,-1.,-3.65594554404396));
#67506=CARTESIAN_POINT('Ctrl Pts',(-1.38035791051215,1.,-3.65594554404396));
#67507=CARTESIAN_POINT('Ctrl Pts',(-1.37972372481598,-1.,-3.64852652756444));
#67508=CARTESIAN_POINT('Ctrl Pts',(-1.37972372481598,1.,-3.64852652756444));
#67509=CARTESIAN_POINT('Ctrl Pts',(-1.37903818567347,-1.,-3.64112507791112));
#67510=CARTESIAN_POINT('Ctrl Pts',(-1.37903818567347,1.,-3.64112507791112));
#67511=CARTESIAN_POINT('Ctrl Pts',(-1.37829035457324,-1.,-3.63371727442448));
#67512=CARTESIAN_POINT('Ctrl Pts',(-1.37829035457324,1.,-3.63371727442448));
#67513=CARTESIAN_POINT('Ctrl Pts',(-1.37746987919868,-1.,-3.62628098665112));
#67514=CARTESIAN_POINT('Ctrl Pts',(-1.37746987919868,1.,-3.62628098665112));
#67515=CARTESIAN_POINT('Ctrl Pts',(-1.37657053403102,-1.,-3.61880481160408));
#67516=CARTESIAN_POINT('Ctrl Pts',(-1.37657053403102,1.,-3.61880481160408));
#67517=CARTESIAN_POINT('Ctrl Pts',(-1.37559314436641,-1.,-3.61129546591082));
#67518=CARTESIAN_POINT('Ctrl Pts',(-1.37559314436641,1.,-3.61129546591082));
#67519=CARTESIAN_POINT('Ctrl Pts',(-1.37455051379642,-1.,-3.60379020124038));
#67520=CARTESIAN_POINT('Ctrl Pts',(-1.37455051379642,1.,-3.60379020124038));
#67521=CARTESIAN_POINT('Ctrl Pts',(-1.37346320103184,-1.,-3.59634627869117));
#67522=CARTESIAN_POINT('Ctrl Pts',(-1.37346320103184,1.,-3.59634627869117));
#67523=CARTESIAN_POINT('Ctrl Pts',(-1.37235053661,-1.,-3.5890185384643));
#67524=CARTESIAN_POINT('Ctrl Pts',(-1.37235053661,1.,-3.5890185384643));
#67525=CARTESIAN_POINT('Ctrl Pts',(-1.37122241663073,-1.,-3.58183885982745));
#67526=CARTESIAN_POINT('Ctrl Pts',(-1.37122241663073,1.,-3.58183885982745));
#67527=CARTESIAN_POINT('Ctrl Pts',(-1.37007229485646,-1.,-3.57479875549453));
#67528=CARTESIAN_POINT('Ctrl Pts',(-1.37007229485646,1.,-3.57479875549453));
#67529=CARTESIAN_POINT('Ctrl Pts',(-1.36886584973349,-1.,-3.56782080304554));
#67530=CARTESIAN_POINT('Ctrl Pts',(-1.36886584973349,1.,-3.56782080304554));
#67531=CARTESIAN_POINT('Ctrl Pts',(-1.36754771771174,-1.,-3.56077662028492));
#67532=CARTESIAN_POINT('Ctrl Pts',(-1.36754771771174,1.,-3.56077662028492));
#67533=CARTESIAN_POINT('Ctrl Pts',(-1.36606145456711,-1.,-3.55353883995793));
#67534=CARTESIAN_POINT('Ctrl Pts',(-1.36606145456711,1.,-3.55353883995793));
#67535=CARTESIAN_POINT('Ctrl Pts',(-1.36436666257567,-1.,-3.54602591832893));
#67536=CARTESIAN_POINT('Ctrl Pts',(-1.36436666257567,1.,-3.54602591832893));
#67537=CARTESIAN_POINT('Ctrl Pts',(-1.36245507339334,-1.,-3.53824396425032));
#67538=CARTESIAN_POINT('Ctrl Pts',(-1.36245507339334,1.,-3.53824396425032));
#67539=CARTESIAN_POINT('Ctrl Pts',(-1.36037259643827,-1.,-3.53034464961849));
#67540=CARTESIAN_POINT('Ctrl Pts',(-1.36037259643827,1.,-3.53034464961849));
#67541=CARTESIAN_POINT('Ctrl Pts',(-1.35821701528975,-1.,-3.52261776117121));
#67542=CARTESIAN_POINT('Ctrl Pts',(-1.35821701528975,1.,-3.52261776117121));
#67543=CARTESIAN_POINT('Ctrl Pts',(-1.35611275237288,-1.,-3.51542230699919));
#67544=CARTESIAN_POINT('Ctrl Pts',(-1.35611275237288,1.,-3.51542230699919));
#67545=CARTESIAN_POINT('Ctrl Pts',(-1.35419113576022,-1.,-3.50913227060177));
#67546=CARTESIAN_POINT('Ctrl Pts',(-1.35419113576022,1.,-3.50913227060177));
#67547=CARTESIAN_POINT('Ctrl Pts',(-1.3525703284343,-1.,-3.50408168106113));
#67548=CARTESIAN_POINT('Ctrl Pts',(-1.3525703284343,1.,-3.50408168106113));
#67549=CARTESIAN_POINT('Ctrl Pts',(-1.35133076331065,-1.,-3.50049707063673));
#67550=CARTESIAN_POINT('Ctrl Pts',(-1.35133076331065,1.,-3.50049707063673));
#67551=CARTESIAN_POINT('Ctrl Pts',(-1.35067437417289,-1.,-3.49888720256612));
#67552=CARTESIAN_POINT('Ctrl Pts',(-1.35067437417289,1.,-3.49888720256612));
#67553=CARTESIAN_POINT('Ctrl Pts',(-1.35037650302887,-1.,-3.49840357193384));
#67554=CARTESIAN_POINT('Ctrl Pts',(-1.35037650302887,1.,-3.49840357193384));
#67555=CARTESIAN_POINT('Ctrl Pts',(-1.35026426118351,-1.,-3.49840260053616));
#67556=CARTESIAN_POINT('Ctrl Pts',(-1.35026426118351,1.,-3.49840260053616));
#67557=CARTESIAN_POINT('Ctrl Pts',(-1.35022972712301,-1.,-3.49848248301936));
#67558=CARTESIAN_POINT('Ctrl Pts',(-1.35022972712301,1.,-3.49848248301936));
#67559=CARTESIAN_POINT('',(-1.36999806084572,1.,-3.97027773754922));
#67560=CARTESIAN_POINT('Ctrl Pts',(-1.36999806084572,1.,-3.97027773754922));
#67561=CARTESIAN_POINT('Ctrl Pts',(-1.37020239094758,1.,-3.9687184694173));
#67562=CARTESIAN_POINT('Ctrl Pts',(-1.37060761746027,1.,-3.96560037975788));
#67563=CARTESIAN_POINT('Ctrl Pts',(-1.37120515615663,1.,-3.96092458508407));
#67564=CARTESIAN_POINT('Ctrl Pts',(-1.37198126433139,1.,-3.95469287283105));
#67565=CARTESIAN_POINT('Ctrl Pts',(-1.37291699203423,1.,-3.94690771786926));
#67566=CARTESIAN_POINT('Ctrl Pts',(-1.37381821967499,1.,-3.93912709041791));
#67567=CARTESIAN_POINT('Ctrl Pts',(-1.37468482215784,1.,-3.93135106761941));
#67568=CARTESIAN_POINT('Ctrl Pts',(-1.37551664448057,1.,-3.92357976987132));
#67569=CARTESIAN_POINT('Ctrl Pts',(-1.37631350505516,1.,-3.91581337461825));
#67570=CARTESIAN_POINT('Ctrl Pts',(-1.3770751963376,1.,-3.90805209522729));
#67571=CARTESIAN_POINT('Ctrl Pts',(-1.3778014851263,1.,-3.90029615196255));
#67572=CARTESIAN_POINT('Ctrl Pts',(-1.37849211287981,1.,-3.89254574338385));
#67573=CARTESIAN_POINT('Ctrl Pts',(-1.37914679719446,1.,-3.88480102249461));
#67574=CARTESIAN_POINT('Ctrl Pts',(-1.37976523097187,1.,-3.87706205830865));
#67575=CARTESIAN_POINT('Ctrl Pts',(-1.38034709213129,1.,-3.86932885813403));
#67576=CARTESIAN_POINT('Ctrl Pts',(-1.38089205993067,1.,-3.86160143044187));
#67577=CARTESIAN_POINT('Ctrl Pts',(-1.38139983115075,1.,-3.85387983979557));
#67578=CARTESIAN_POINT('Ctrl Pts',(-1.38187013346089,1.,-3.84616425605705));
#67579=CARTESIAN_POINT('Ctrl Pts',(-1.38230274828774,1.,-3.83845502790609));
#67580=CARTESIAN_POINT('Ctrl Pts',(-1.38269750245086,1.,-3.83075266982138));
#67581=CARTESIAN_POINT('Ctrl Pts',(-1.38305421262724,1.,-3.82305771743715));
#67582=CARTESIAN_POINT('Ctrl Pts',(-1.38337263902766,1.,-3.81537060817765));
#67583=CARTESIAN_POINT('Ctrl Pts',(-1.38365244046226,1.,-3.80769156398429));
#67584=CARTESIAN_POINT('Ctrl Pts',(-1.38389311766701,1.,-3.80002044322169));
#67585=CARTESIAN_POINT('Ctrl Pts',(-1.38409399694589,1.,-3.79235669640907));
#67586=CARTESIAN_POINT('Ctrl Pts',(-1.38425435883773,1.,-3.78469969805134));
#67587=CARTESIAN_POINT('Ctrl Pts',(-1.38437354551435,1.,-3.77704902230441));
#67588=CARTESIAN_POINT('Ctrl Pts',(-1.38445107339517,1.,-3.76940473185775));
#67589=CARTESIAN_POINT('Ctrl Pts',(-1.38448675253343,1.,-3.76176768271347));
#67590=CARTESIAN_POINT('Ctrl Pts',(-1.38448077997155,1.,-3.75413976318727));
#67591=CARTESIAN_POINT('Ctrl Pts',(-1.38443344984389,1.,-3.7465231716786));
#67592=CARTESIAN_POINT('Ctrl Pts',(-1.38434489156456,1.,-3.73891976418099));
#67593=CARTESIAN_POINT('Ctrl Pts',(-1.38421479111531,1.,-3.73133035859283));
#67594=CARTESIAN_POINT('Ctrl Pts',(-1.3840421342895,1.,-3.72375409358805));
#67595=CARTESIAN_POINT('Ctrl Pts',(-1.38382489984585,1.,-3.7161876605181));
#67596=CARTESIAN_POINT('Ctrl Pts',(-1.38356065402122,1.,-3.70862680753343));
#67597=CARTESIAN_POINT('Ctrl Pts',(-1.38324717612862,1.,-3.70106792167894));
#67598=CARTESIAN_POINT('Ctrl Pts',(-1.38288311171649,1.,-3.69350967899523));
#67599=CARTESIAN_POINT('Ctrl Pts',(-1.38246852827185,1.,-3.68595444983844));
#67600=CARTESIAN_POINT('Ctrl Pts',(-1.38200574290626,1.,-3.6784103848243));
#67601=CARTESIAN_POINT('Ctrl Pts',(-1.38149812653876,1.,-3.67088843112282));
#67602=CARTESIAN_POINT('Ctrl Pts',(-1.38094856333558,1.,-3.66339848520874));
#67603=CARTESIAN_POINT('Ctrl Pts',(-1.38035791051215,1.,-3.65594554404396));
#67604=CARTESIAN_POINT('Ctrl Pts',(-1.37972372481598,1.,-3.64852652756444));
#67605=CARTESIAN_POINT('Ctrl Pts',(-1.37903818567347,1.,-3.64112507791112));
#67606=CARTESIAN_POINT('Ctrl Pts',(-1.37829035457324,1.,-3.63371727442448));
#67607=CARTESIAN_POINT('Ctrl Pts',(-1.37746987919868,1.,-3.62628098665112));
#67608=CARTESIAN_POINT('Ctrl Pts',(-1.37657053403102,1.,-3.61880481160408));
#67609=CARTESIAN_POINT('Ctrl Pts',(-1.37559314436641,1.,-3.61129546591082));
#67610=CARTESIAN_POINT('Ctrl Pts',(-1.37455051379642,1.,-3.60379020124038));
#67611=CARTESIAN_POINT('Ctrl Pts',(-1.37346320103184,1.,-3.59634627869117));
#67612=CARTESIAN_POINT('Ctrl Pts',(-1.37235053661,1.,-3.5890185384643));
#67613=CARTESIAN_POINT('Ctrl Pts',(-1.37122241663073,1.,-3.58183885982745));
#67614=CARTESIAN_POINT('Ctrl Pts',(-1.37007229485646,1.,-3.57479875549453));
#67615=CARTESIAN_POINT('Ctrl Pts',(-1.36886584973349,1.,-3.56782080304554));
#67616=CARTESIAN_POINT('Ctrl Pts',(-1.36754771771174,1.,-3.56077662028492));
#67617=CARTESIAN_POINT('Ctrl Pts',(-1.36606145456711,1.,-3.55353883995793));
#67618=CARTESIAN_POINT('Ctrl Pts',(-1.36436666257567,1.,-3.54602591832893));
#67619=CARTESIAN_POINT('Ctrl Pts',(-1.36245507339334,1.,-3.53824396425032));
#67620=CARTESIAN_POINT('Ctrl Pts',(-1.36037259643827,1.,-3.53034464961849));
#67621=CARTESIAN_POINT('Ctrl Pts',(-1.35821701528975,1.,-3.52261776117121));
#67622=CARTESIAN_POINT('Ctrl Pts',(-1.35611275237288,1.,-3.51542230699919));
#67623=CARTESIAN_POINT('Ctrl Pts',(-1.35419113576022,1.,-3.50913227060177));
#67624=CARTESIAN_POINT('Ctrl Pts',(-1.3525703284343,1.,-3.50408168106113));
#67625=CARTESIAN_POINT('Ctrl Pts',(-1.35142377279535,1.,-3.5007660381658));
#67626=CARTESIAN_POINT('Ctrl Pts',(-1.35080045218652,1.,-3.49920025459856));
#67627=CARTESIAN_POINT('Ctrl Pts',(-1.35049736560633,1.,-3.49861894124915));
#67628=CARTESIAN_POINT('Ctrl Pts',(-1.35036670893102,1.,-3.49847119623841));
#67629=CARTESIAN_POINT('Ctrl Pts',(-1.35032489087269,1.,-3.49844575334386));
#67630=CARTESIAN_POINT('',(-1.36999806084572,0.,-3.97027773754922));
#67631=CARTESIAN_POINT('Ctrl Pts',(-0.96399761336957,-1.,-3.62397690409552));
#67632=CARTESIAN_POINT('Ctrl Pts',(-0.96399761336957,1.,-3.62397690409552));
#67633=CARTESIAN_POINT('Ctrl Pts',(-0.963922720982576,-1.,-3.62393257642191));
#67634=CARTESIAN_POINT('Ctrl Pts',(-0.963922720982576,1.,-3.62393257642191));
#67635=CARTESIAN_POINT('Ctrl Pts',(-0.963832486396055,-1.,-3.62399933640277));
#67636=CARTESIAN_POINT('Ctrl Pts',(-0.963832486396055,1.,-3.62399933640277));
#67637=CARTESIAN_POINT('Ctrl Pts',(-0.963875774532103,-1.,-3.62456568607055));
#67638=CARTESIAN_POINT('Ctrl Pts',(-0.963875774532103,1.,-3.62456568607055));
#67639=CARTESIAN_POINT('Ctrl Pts',(-0.964291001274618,-1.,-3.62625391255277));
#67640=CARTESIAN_POINT('Ctrl Pts',(-0.964291001274618,1.,-3.62625391255277));
#67641=CARTESIAN_POINT('Ctrl Pts',(-0.965395153165716,-1.,-3.62988252139998));
#67642=CARTESIAN_POINT('Ctrl Pts',(-0.965395153165716,1.,-3.62988252139998));
#67643=CARTESIAN_POINT('Ctrl Pts',(-0.967052554540877,-1.,-3.6349212208096));
#67644=CARTESIAN_POINT('Ctrl Pts',(-0.967052554540877,1.,-3.6349212208096));
#67645=CARTESIAN_POINT('Ctrl Pts',(-0.969195124674829,-1.,-3.64113946505393));
#67646=CARTESIAN_POINT('Ctrl Pts',(-0.969195124674829,1.,-3.64113946505393));
#67647=CARTESIAN_POINT('Ctrl Pts',(-0.971722122060277,-1.,-3.64819756447072));
#67648=CARTESIAN_POINT('Ctrl Pts',(-0.971722122060277,1.,-3.64819756447072));
#67649=CARTESIAN_POINT('Ctrl Pts',(-0.974519971354139,-1.,-3.6557157673487));
#67650=CARTESIAN_POINT('Ctrl Pts',(-0.974519971354139,1.,-3.6557157673487));
#67651=CARTESIAN_POINT('Ctrl Pts',(-0.977478312751416,-1.,-3.66333049637403));
#67652=CARTESIAN_POINT('Ctrl Pts',(-0.977478312751416,1.,-3.66333049637403));
#67653=CARTESIAN_POINT('Ctrl Pts',(-0.980505922458494,-1.,-3.67074983340444));
#67654=CARTESIAN_POINT('Ctrl Pts',(-0.980505922458494,1.,-3.67074983340444));
#67655=CARTESIAN_POINT('Ctrl Pts',(-0.983550791470864,-1.,-3.67782408841876));
#67656=CARTESIAN_POINT('Ctrl Pts',(-0.983550791470864,1.,-3.67782408841876));
#67657=CARTESIAN_POINT('Ctrl Pts',(-0.986602639864286,-1.,-3.6845531792623));
#67658=CARTESIAN_POINT('Ctrl Pts',(-0.986602639864286,1.,-3.6845531792623));
#67659=CARTESIAN_POINT('Ctrl Pts',(-0.989676715398858,-1.,-3.69102682138955));
#67660=CARTESIAN_POINT('Ctrl Pts',(-0.989676715398858,1.,-3.69102682138955));
#67661=CARTESIAN_POINT('Ctrl Pts',(-0.992802218332104,-1.,-3.69738123415696));
#67662=CARTESIAN_POINT('Ctrl Pts',(-0.992802218332104,1.,-3.69738123415696));
#67663=CARTESIAN_POINT('Ctrl Pts',(-0.996009819772432,-1.,-3.70375282282107));
#67664=CARTESIAN_POINT('Ctrl Pts',(-0.996009819772432,1.,-3.70375282282107));
#67665=CARTESIAN_POINT('Ctrl Pts',(-0.999317260756344,-1.,-3.7102243971387));
#67666=CARTESIAN_POINT('Ctrl Pts',(-0.999317260756344,1.,-3.7102243971387));
#67667=CARTESIAN_POINT('Ctrl Pts',(-1.00272423396802,-1.,-3.71680667125047));
#67668=CARTESIAN_POINT('Ctrl Pts',(-1.00272423396802,1.,-3.71680667125047));
#67669=CARTESIAN_POINT('Ctrl Pts',(-1.00622000735696,-1.,-3.72346803750544));
#67670=CARTESIAN_POINT('Ctrl Pts',(-1.00622000735696,1.,-3.72346803750544));
#67671=CARTESIAN_POINT('Ctrl Pts',(-1.00978798539491,-1.,-3.73015276704407));
#67672=CARTESIAN_POINT('Ctrl Pts',(-1.00978798539491,1.,-3.73015276704407));
#67673=CARTESIAN_POINT('Ctrl Pts',(-1.01341114319906,-1.,-3.73680245055747));
#67674=CARTESIAN_POINT('Ctrl Pts',(-1.01341114319906,1.,-3.73680245055747));
#67675=CARTESIAN_POINT('Ctrl Pts',(-1.01707794311088,-1.,-3.74337942504993));
#67676=CARTESIAN_POINT('Ctrl Pts',(-1.01707794311088,1.,-3.74337942504993));
#67677=CARTESIAN_POINT('Ctrl Pts',(-1.02078510487439,-1.,-3.74987777155873));
#67678=CARTESIAN_POINT('Ctrl Pts',(-1.02078510487439,1.,-3.74987777155873));
#67679=CARTESIAN_POINT('Ctrl Pts',(-1.02453429444668,-1.,-3.75631037456224));
#67680=CARTESIAN_POINT('Ctrl Pts',(-1.02453429444668,1.,-3.75631037456224));
#67681=CARTESIAN_POINT('Ctrl Pts',(-1.02833014458184,-1.,-3.76270122291245));
#67682=CARTESIAN_POINT('Ctrl Pts',(-1.02833014458184,1.,-3.76270122291245));
#67683=CARTESIAN_POINT('Ctrl Pts',(-1.03217786604919,-1.,-3.76907609832516));
#67684=CARTESIAN_POINT('Ctrl Pts',(-1.03217786604919,1.,-3.76907609832516));
#67685=CARTESIAN_POINT('Ctrl Pts',(-1.03608074678008,-1.,-3.77545283140427));
#67686=CARTESIAN_POINT('Ctrl Pts',(-1.03608074678008,1.,-3.77545283140427));
#67687=CARTESIAN_POINT('Ctrl Pts',(-1.04003862055798,-1.,-3.7818353500817));
#67688=CARTESIAN_POINT('Ctrl Pts',(-1.04003862055798,1.,-3.7818353500817));
#67689=CARTESIAN_POINT('Ctrl Pts',(-1.04404924374422,-1.,-3.78821910787179));
#67690=CARTESIAN_POINT('Ctrl Pts',(-1.04404924374422,1.,-3.78821910787179));
#67691=CARTESIAN_POINT('Ctrl Pts',(-1.04810913267639,-1.,-3.79459440308786));
#67692=CARTESIAN_POINT('Ctrl Pts',(-1.04810913267639,1.,-3.79459440308786));
#67693=CARTESIAN_POINT('Ctrl Pts',(-1.05221457990016,-1.,-3.80095039790681));
#67694=CARTESIAN_POINT('Ctrl Pts',(-1.05221457990016,1.,-3.80095039790681));
#67695=CARTESIAN_POINT('Ctrl Pts',(-1.05636266918644,-1.,-3.80727913637791));
#67696=CARTESIAN_POINT('Ctrl Pts',(-1.05636266918644,1.,-3.80727913637791));
#67697=CARTESIAN_POINT('Ctrl Pts',(-1.06055206187299,-1.,-3.8135786611749));
#67698=CARTESIAN_POINT('Ctrl Pts',(-1.06055206187299,1.,-3.8135786611749));
#67699=CARTESIAN_POINT('Ctrl Pts',(-1.0647824403893,-1.,-3.81985083953012));
#67700=CARTESIAN_POINT('Ctrl Pts',(-1.0647824403893,1.,-3.81985083953012));
#67701=CARTESIAN_POINT('Ctrl Pts',(-1.06905413180359,-1.,-3.82609989967276));
#67702=CARTESIAN_POINT('Ctrl Pts',(-1.06905413180359,1.,-3.82609989967276));
#67703=CARTESIAN_POINT('Ctrl Pts',(-1.07336766633459,-1.,-3.83233071195144));
#67704=CARTESIAN_POINT('Ctrl Pts',(-1.07336766633459,1.,-3.83233071195144));
#67705=CARTESIAN_POINT('Ctrl Pts',(-1.07772335353858,-1.,-3.83854714117491));
#67706=CARTESIAN_POINT('Ctrl Pts',(-1.07772335353858,1.,-3.83854714117491));
#67707=CARTESIAN_POINT('Ctrl Pts',(-1.08212087917991,-1.,-3.8447504803063));
#67708=CARTESIAN_POINT('Ctrl Pts',(-1.08212087917991,1.,-3.8447504803063));
#67709=CARTESIAN_POINT('Ctrl Pts',(-1.08655950846384,-1.,-3.85094025222713));
#67710=CARTESIAN_POINT('Ctrl Pts',(-1.08655950846384,1.,-3.85094025222713));
#67711=CARTESIAN_POINT('Ctrl Pts',(-1.09103825516294,-1.,-3.85711487933931));
#67712=CARTESIAN_POINT('Ctrl Pts',(-1.09103825516294,1.,-3.85711487933931));
#67713=CARTESIAN_POINT('Ctrl Pts',(-1.09555606505013,-1.,-3.86327241021247));
#67714=CARTESIAN_POINT('Ctrl Pts',(-1.09555606505013,1.,-3.86327241021247));
#67715=CARTESIAN_POINT('Ctrl Pts',(-1.10011198761195,-1.,-3.86941120134849));
#67716=CARTESIAN_POINT('Ctrl Pts',(-1.10011198761195,1.,-3.86941120134849));
#67717=CARTESIAN_POINT('Ctrl Pts',(-1.10470536603287,-1.,-3.87553067187514));
#67718=CARTESIAN_POINT('Ctrl Pts',(-1.10470536603287,1.,-3.87553067187514));
#67719=CARTESIAN_POINT('Ctrl Pts',(-1.10933577224008,-1.,-3.88163105531724));
#67720=CARTESIAN_POINT('Ctrl Pts',(-1.10933577224008,1.,-3.88163105531724));
#67721=CARTESIAN_POINT('Ctrl Pts',(-1.11400292434429,-1.,-3.88771308285171));
#67722=CARTESIAN_POINT('Ctrl Pts',(-1.11400292434429,1.,-3.88771308285171));
#67723=CARTESIAN_POINT('Ctrl Pts',(-1.11870660794603,-1.,-3.89377768340344));
#67724=CARTESIAN_POINT('Ctrl Pts',(-1.11870660794603,1.,-3.89377768340344));
#67725=CARTESIAN_POINT('Ctrl Pts',(-1.12344660099043,-1.,-3.89982569750025));
#67726=CARTESIAN_POINT('Ctrl Pts',(-1.12344660099043,1.,-3.89982569750025));
#67727=CARTESIAN_POINT('Ctrl Pts',(-1.12822258281553,-1.,-3.90585753318737));
#67728=CARTESIAN_POINT('Ctrl Pts',(-1.12822258281553,1.,-3.90585753318737));
#67729=CARTESIAN_POINT('Ctrl Pts',(-1.13303414693896,-1.,-3.91187321145649));
#67730=CARTESIAN_POINT('Ctrl Pts',(-1.13303414693896,1.,-3.91187321145649));
#67731=CARTESIAN_POINT('Ctrl Pts',(-1.13788084225554,-1.,-3.91787251936827));
#67732=CARTESIAN_POINT('Ctrl Pts',(-1.13788084225554,1.,-3.91787251936827));
#67733=CARTESIAN_POINT('Ctrl Pts',(-1.14276220561593,-1.,-3.92385513133997));
#67734=CARTESIAN_POINT('Ctrl Pts',(-1.14276220561593,1.,-3.92385513133997));
#67735=CARTESIAN_POINT('Ctrl Pts',(-1.14767779451123,-1.,-3.92982073294257));
#67736=CARTESIAN_POINT('Ctrl Pts',(-1.14767779451123,1.,-3.92982073294257));
#67737=CARTESIAN_POINT('Ctrl Pts',(-1.1526272271632,-1.,-3.9357691705628));
#67738=CARTESIAN_POINT('Ctrl Pts',(-1.1526272271632,1.,-3.9357691705628));
#67739=CARTESIAN_POINT('Ctrl Pts',(-1.15761018340956,-1.,-3.94170046685203));
#67740=CARTESIAN_POINT('Ctrl Pts',(-1.15761018340956,1.,-3.94170046685203));
#67741=CARTESIAN_POINT('Ctrl Pts',(-1.16262637999157,-1.,-3.94761474780583));
#67742=CARTESIAN_POINT('Ctrl Pts',(-1.16262637999157,1.,-3.94761474780583));
#67743=CARTESIAN_POINT('Ctrl Pts',(-1.16767555244438,-1.,-3.95351219509876));
#67744=CARTESIAN_POINT('Ctrl Pts',(-1.16767555244438,1.,-3.95351219509876));
#67745=CARTESIAN_POINT('Ctrl Pts',(-1.17275743590361,-1.,-3.95939299213276));
#67746=CARTESIAN_POINT('Ctrl Pts',(-1.17275743590361,1.,-3.95939299213276));
#67747=CARTESIAN_POINT('Ctrl Pts',(-1.17787174135592,-1.,-3.96525726358159));
#67748=CARTESIAN_POINT('Ctrl Pts',(-1.17787174135592,1.,-3.96525726358159));
#67749=CARTESIAN_POINT('Ctrl Pts',(-1.18301815039831,-1.,-3.97110505165415));
#67750=CARTESIAN_POINT('Ctrl Pts',(-1.18301815039831,1.,-3.97110505165415));
#67751=CARTESIAN_POINT('Ctrl Pts',(-1.18819633715539,-1.,-3.97693634767754));
#67752=CARTESIAN_POINT('Ctrl Pts',(-1.18819633715539,1.,-3.97693634767754));
#67753=CARTESIAN_POINT('Ctrl Pts',(-1.19340598349475,-1.,-3.98275111052561));
#67754=CARTESIAN_POINT('Ctrl Pts',(-1.19340598349475,1.,-3.98275111052561));
#67755=CARTESIAN_POINT('Ctrl Pts',(-1.19864679609566,-1.,-3.98854928957189));
#67756=CARTESIAN_POINT('Ctrl Pts',(-1.19864679609566,1.,-3.98854928957189));
#67757=CARTESIAN_POINT('Ctrl Pts',(-1.20391852375139,-1.,-3.99433084799666));
#67758=CARTESIAN_POINT('Ctrl Pts',(-1.20391852375139,1.,-3.99433084799666));
#67759=CARTESIAN_POINT('Ctrl Pts',(-1.20922097029551,-1.,-4.00009577950721));
#67760=CARTESIAN_POINT('Ctrl Pts',(-1.20922097029551,1.,-4.00009577950721));
#67761=CARTESIAN_POINT('Ctrl Pts',(-1.21455398918133,-1.,-4.00584409522722));
#67762=CARTESIAN_POINT('Ctrl Pts',(-1.21455398918133,1.,-4.00584409522722));
#67763=CARTESIAN_POINT('Ctrl Pts',(-1.21884478244403,-1.,-4.01042947140789));
#67764=CARTESIAN_POINT('Ctrl Pts',(-1.21884478244403,1.,-4.01042947140789));
#67765=CARTESIAN_POINT('Ctrl Pts',(-1.22207656455845,-1.,-4.01386104433519));
#67766=CARTESIAN_POINT('Ctrl Pts',(-1.22207656455845,1.,-4.01386104433519));
#67767=CARTESIAN_POINT('Ctrl Pts',(-1.22423716681317,-1.,-4.01614544569895));
#67768=CARTESIAN_POINT('Ctrl Pts',(-1.22423716681317,1.,-4.01614544569895));
#67769=CARTESIAN_POINT('Ctrl Pts',(-1.22531898815164,-1.,-4.01728681790024));
#67770=CARTESIAN_POINT('Ctrl Pts',(-1.22531898815164,1.,-4.01728681790024));
#67771=CARTESIAN_POINT('',(-0.963899035118984,1.,-3.62400312501199));
#67772=CARTESIAN_POINT('Ctrl Pts',(-0.963899035118985,-1.,-3.62400312501199));
#67773=CARTESIAN_POINT('Ctrl Pts',(-0.963899035118985,-0.666666666666667,
-3.62400312501199));
#67774=CARTESIAN_POINT('Ctrl Pts',(-0.963899035118985,-0.333333333333333,
-3.62400312501199));
#67775=CARTESIAN_POINT('Ctrl Pts',(-0.963899035118985,0.333333333333333,
-3.62400312501199));
#67776=CARTESIAN_POINT('Ctrl Pts',(-0.963899035118986,0.666666666666667,
-3.62400312501199));
#67777=CARTESIAN_POINT('Ctrl Pts',(-0.963899035118986,1.,-3.62400312501199));
#67778=CARTESIAN_POINT('',(-1.22531898815164,1.,-4.01728681790024));
#67779=CARTESIAN_POINT('',(-1.22531898815164,0.,-4.01728681790024));
#67780=CARTESIAN_POINT('Ctrl Pts',(-0.963899035118985,1.,-3.62400312501199));
#67781=CARTESIAN_POINT('Ctrl Pts',(-0.963880158556713,1.,-3.62404828878375));
#67782=CARTESIAN_POINT('Ctrl Pts',(-0.963861297423579,1.,-3.62424461507455));
#67783=CARTESIAN_POINT('Ctrl Pts',(-0.963957782642589,1.,-3.62489305727516));
#67784=CARTESIAN_POINT('Ctrl Pts',(-0.964373850166081,1.,-3.62652618145252));
#67785=CARTESIAN_POINT('Ctrl Pts',(-0.965395153165716,1.,-3.62988252139998));
#67786=CARTESIAN_POINT('Ctrl Pts',(-0.967052554540877,1.,-3.6349212208096));
#67787=CARTESIAN_POINT('Ctrl Pts',(-0.969195124674829,1.,-3.64113946505393));
#67788=CARTESIAN_POINT('Ctrl Pts',(-0.971722122060277,1.,-3.64819756447072));
#67789=CARTESIAN_POINT('Ctrl Pts',(-0.974519971354139,1.,-3.6557157673487));
#67790=CARTESIAN_POINT('Ctrl Pts',(-0.977478312751416,1.,-3.66333049637403));
#67791=CARTESIAN_POINT('Ctrl Pts',(-0.980505922458494,1.,-3.67074983340444));
#67792=CARTESIAN_POINT('Ctrl Pts',(-0.983550791470864,1.,-3.67782408841876));
#67793=CARTESIAN_POINT('Ctrl Pts',(-0.986602639864286,1.,-3.6845531792623));
#67794=CARTESIAN_POINT('Ctrl Pts',(-0.989676715398858,1.,-3.69102682138955));
#67795=CARTESIAN_POINT('Ctrl Pts',(-0.992802218332104,1.,-3.69738123415696));
#67796=CARTESIAN_POINT('Ctrl Pts',(-0.996009819772432,1.,-3.70375282282107));
#67797=CARTESIAN_POINT('Ctrl Pts',(-0.999317260756344,1.,-3.7102243971387));
#67798=CARTESIAN_POINT('Ctrl Pts',(-1.00272423396802,1.,-3.71680667125047));
#67799=CARTESIAN_POINT('Ctrl Pts',(-1.00622000735696,1.,-3.72346803750544));
#67800=CARTESIAN_POINT('Ctrl Pts',(-1.00978798539491,1.,-3.73015276704407));
#67801=CARTESIAN_POINT('Ctrl Pts',(-1.01341114319906,1.,-3.73680245055747));
#67802=CARTESIAN_POINT('Ctrl Pts',(-1.01707794311088,1.,-3.74337942504993));
#67803=CARTESIAN_POINT('Ctrl Pts',(-1.02078510487439,1.,-3.74987777155873));
#67804=CARTESIAN_POINT('Ctrl Pts',(-1.02453429444668,1.,-3.75631037456224));
#67805=CARTESIAN_POINT('Ctrl Pts',(-1.02833014458184,1.,-3.76270122291245));
#67806=CARTESIAN_POINT('Ctrl Pts',(-1.03217786604919,1.,-3.76907609832516));
#67807=CARTESIAN_POINT('Ctrl Pts',(-1.03608074678008,1.,-3.77545283140427));
#67808=CARTESIAN_POINT('Ctrl Pts',(-1.04003862055798,1.,-3.7818353500817));
#67809=CARTESIAN_POINT('Ctrl Pts',(-1.04404924374422,1.,-3.78821910787179));
#67810=CARTESIAN_POINT('Ctrl Pts',(-1.04810913267639,1.,-3.79459440308786));
#67811=CARTESIAN_POINT('Ctrl Pts',(-1.05221457990016,1.,-3.80095039790681));
#67812=CARTESIAN_POINT('Ctrl Pts',(-1.05636266918644,1.,-3.80727913637791));
#67813=CARTESIAN_POINT('Ctrl Pts',(-1.06055206187299,1.,-3.8135786611749));
#67814=CARTESIAN_POINT('Ctrl Pts',(-1.0647824403893,1.,-3.81985083953012));
#67815=CARTESIAN_POINT('Ctrl Pts',(-1.06905413180359,1.,-3.82609989967276));
#67816=CARTESIAN_POINT('Ctrl Pts',(-1.07336766633459,1.,-3.83233071195144));
#67817=CARTESIAN_POINT('Ctrl Pts',(-1.07772335353858,1.,-3.83854714117491));
#67818=CARTESIAN_POINT('Ctrl Pts',(-1.08212087917991,1.,-3.8447504803063));
#67819=CARTESIAN_POINT('Ctrl Pts',(-1.08655950846384,1.,-3.85094025222713));
#67820=CARTESIAN_POINT('Ctrl Pts',(-1.09103825516294,1.,-3.85711487933931));
#67821=CARTESIAN_POINT('Ctrl Pts',(-1.09555606505013,1.,-3.86327241021247));
#67822=CARTESIAN_POINT('Ctrl Pts',(-1.10011198761195,1.,-3.86941120134849));
#67823=CARTESIAN_POINT('Ctrl Pts',(-1.10470536603287,1.,-3.87553067187514));
#67824=CARTESIAN_POINT('Ctrl Pts',(-1.10933577224008,1.,-3.88163105531724));
#67825=CARTESIAN_POINT('Ctrl Pts',(-1.11400292434429,1.,-3.88771308285171));
#67826=CARTESIAN_POINT('Ctrl Pts',(-1.11870660794603,1.,-3.89377768340344));
#67827=CARTESIAN_POINT('Ctrl Pts',(-1.12344660099043,1.,-3.89982569750025));
#67828=CARTESIAN_POINT('Ctrl Pts',(-1.12822258281553,1.,-3.90585753318737));
#67829=CARTESIAN_POINT('Ctrl Pts',(-1.13303414693896,1.,-3.91187321145649));
#67830=CARTESIAN_POINT('Ctrl Pts',(-1.13788084225554,1.,-3.91787251936827));
#67831=CARTESIAN_POINT('Ctrl Pts',(-1.14276220561593,1.,-3.92385513133997));
#67832=CARTESIAN_POINT('Ctrl Pts',(-1.14767779451123,1.,-3.92982073294257));
#67833=CARTESIAN_POINT('Ctrl Pts',(-1.1526272271632,1.,-3.9357691705628));
#67834=CARTESIAN_POINT('Ctrl Pts',(-1.15761018340956,1.,-3.94170046685203));
#67835=CARTESIAN_POINT('Ctrl Pts',(-1.16262637999157,1.,-3.94761474780583));
#67836=CARTESIAN_POINT('Ctrl Pts',(-1.16767555244438,1.,-3.95351219509876));
#67837=CARTESIAN_POINT('Ctrl Pts',(-1.17275743590361,1.,-3.95939299213276));
#67838=CARTESIAN_POINT('Ctrl Pts',(-1.17787174135592,1.,-3.96525726358159));
#67839=CARTESIAN_POINT('Ctrl Pts',(-1.18301815039831,1.,-3.97110505165415));
#67840=CARTESIAN_POINT('Ctrl Pts',(-1.18819633715539,1.,-3.97693634767754));
#67841=CARTESIAN_POINT('Ctrl Pts',(-1.19340598349475,1.,-3.98275111052561));
#67842=CARTESIAN_POINT('Ctrl Pts',(-1.19864679609566,1.,-3.98854928957189));
#67843=CARTESIAN_POINT('Ctrl Pts',(-1.20391852375139,1.,-3.99433084799666));
#67844=CARTESIAN_POINT('Ctrl Pts',(-1.20922097029551,1.,-4.00009577950721));
#67845=CARTESIAN_POINT('Ctrl Pts',(-1.21455398918133,1.,-4.00584409522722));
#67846=CARTESIAN_POINT('Ctrl Pts',(-1.21884478244403,1.,-4.01042947140789));
#67847=CARTESIAN_POINT('Ctrl Pts',(-1.22207656455845,1.,-4.01386104433519));
#67848=CARTESIAN_POINT('Ctrl Pts',(-1.22423716681317,1.,-4.01614544569895));
#67849=CARTESIAN_POINT('Ctrl Pts',(-1.22531898815164,1.,-4.01728681790024));
#67850=CARTESIAN_POINT('Origin',(-1.22531898815164,0.,-4.01728681790024));
#67851=CARTESIAN_POINT('',(-1.36999806084572,1.,-3.97027773754922));
#67852=CARTESIAN_POINT('Origin',(0.,0.,0.));
#67853=CARTESIAN_POINT('',(-0.786422660833743,1.,-3.66661143271648));
#67854=CARTESIAN_POINT('Origin',(0.,1.,0.));
#67855=CARTESIAN_POINT('Ctrl Pts',(-0.786422660833742,1.,-3.66661143271648));
#67856=CARTESIAN_POINT('Ctrl Pts',(-0.786422660833742,0.666666666666667,
-3.66661143271648));
#67857=CARTESIAN_POINT('Ctrl Pts',(-0.786422660833742,0.333333333333333,
-3.66661143271648));
#67858=CARTESIAN_POINT('Ctrl Pts',(-0.786422660833742,-0.333333333333333,
-3.66661143271648));
#67859=CARTESIAN_POINT('Ctrl Pts',(-0.786422660833742,-0.666666666666667,
-3.66661143271648));
#67860=CARTESIAN_POINT('Ctrl Pts',(-0.786422660833742,-1.,-3.66661143271648));
#67861=CARTESIAN_POINT('Ctrl Pts',(-0.732042837400619,-1.,-4.13571194405636));
#67862=CARTESIAN_POINT('Ctrl Pts',(-0.732042837400619,1.,-4.13571194405636));
#67863=CARTESIAN_POINT('Ctrl Pts',(-0.732488575135926,-1.,-4.13420383737278));
#67864=CARTESIAN_POINT('Ctrl Pts',(-0.732488575135926,1.,-4.13420383737278));
#67865=CARTESIAN_POINT('Ctrl Pts',(-0.733376589325634,-1.,-4.13118752796397));
#67866=CARTESIAN_POINT('Ctrl Pts',(-0.733376589325634,1.,-4.13118752796397));
#67867=CARTESIAN_POINT('Ctrl Pts',(-0.734698226767512,-1.,-4.12666277572794));
#67868=CARTESIAN_POINT('Ctrl Pts',(-0.734698226767512,1.,-4.12666277572794));
#67869=CARTESIAN_POINT('Ctrl Pts',(-0.736439634335347,-1.,-4.12062919626082));
#67870=CARTESIAN_POINT('Ctrl Pts',(-0.736439634335347,1.,-4.12062919626082));
#67871=CARTESIAN_POINT('Ctrl Pts',(-0.738581708229119,-1.,-4.11308626953795));
#67872=CARTESIAN_POINT('Ctrl Pts',(-0.738581708229119,1.,-4.11308626953795));
#67873=CARTESIAN_POINT('Ctrl Pts',(-0.740688998555152,-1.,-4.1055424175856));
#67874=CARTESIAN_POINT('Ctrl Pts',(-0.740688998555152,1.,-4.1055424175856));
#67875=CARTESIAN_POINT('Ctrl Pts',(-0.742761369690018,-1.,-4.09799769702712));
#67876=CARTESIAN_POINT('Ctrl Pts',(-0.742761369690018,1.,-4.09799769702712));
#67877=CARTESIAN_POINT('Ctrl Pts',(-0.744798649705514,-1.,-4.09045220253011));
#67878=CARTESIAN_POINT('Ctrl Pts',(-0.744798649705514,1.,-4.09045220253011));
#67879=CARTESIAN_POINT('Ctrl Pts',(-0.746800631490822,-1.,-4.08290608094789));
#67880=CARTESIAN_POINT('Ctrl Pts',(-0.746800631490822,1.,-4.08290608094789));
#67881=CARTESIAN_POINT('Ctrl Pts',(-0.748767076679177,-1.,-4.07535951055363));
#67882=CARTESIAN_POINT('Ctrl Pts',(-0.748767076679177,1.,-4.07535951055363));
#67883=CARTESIAN_POINT('Ctrl Pts',(-0.750697720483176,-1.,-4.06781267241886));
#67884=CARTESIAN_POINT('Ctrl Pts',(-0.750697720483176,1.,-4.06781267241886));
#67885=CARTESIAN_POINT('Ctrl Pts',(-0.752592276482869,-1.,-4.06026572221399));
#67886=CARTESIAN_POINT('Ctrl Pts',(-0.752592276482869,1.,-4.06026572221399));
#67887=CARTESIAN_POINT('Ctrl Pts',(-0.754450441816412,-1.,-4.05271876688106));
#67888=CARTESIAN_POINT('Ctrl Pts',(-0.754450441816412,1.,-4.05271876688106));
#67889=CARTESIAN_POINT('Ctrl Pts',(-0.756271902370187,-1.,-4.04517182654344));
#67890=CARTESIAN_POINT('Ctrl Pts',(-0.756271902370187,1.,-4.04517182654344));
#67891=CARTESIAN_POINT('Ctrl Pts',(-0.758056338885554,-1.,-4.03762485803468));
#67892=CARTESIAN_POINT('Ctrl Pts',(-0.758056338885554,1.,-4.03762485803468));
#67893=CARTESIAN_POINT('Ctrl Pts',(-0.759803433244166,-1.,-4.0300778195465));
#67894=CARTESIAN_POINT('Ctrl Pts',(-0.759803433244166,1.,-4.0300778195465));
#67895=CARTESIAN_POINT('Ctrl Pts',(-0.761512875859942,-1.,-4.02253072741347));
#67896=CARTESIAN_POINT('Ctrl Pts',(-0.761512875859942,1.,-4.02253072741347));
#67897=CARTESIAN_POINT('Ctrl Pts',(-0.763184371182827,-1.,-4.01498370680434));
#67898=CARTESIAN_POINT('Ctrl Pts',(-0.763184371182827,1.,-4.01498370680434));
#67899=CARTESIAN_POINT('Ctrl Pts',(-0.764817648784946,-1.,-4.00743706791366));
#67900=CARTESIAN_POINT('Ctrl Pts',(-0.764817648784946,1.,-4.00743706791366));
#67901=CARTESIAN_POINT('Ctrl Pts',(-0.766412457135786,-1.,-3.99989129179464));
#67902=CARTESIAN_POINT('Ctrl Pts',(-0.766412457135786,1.,-3.99989129179464));
#67903=CARTESIAN_POINT('Ctrl Pts',(-0.767968531377708,-1.,-3.99234687880892));
#67904=CARTESIAN_POINT('Ctrl Pts',(-0.767968531377708,1.,-3.99234687880892));
#67905=CARTESIAN_POINT('Ctrl Pts',(-0.769485566245459,-1.,-3.98480422348403));
#67906=CARTESIAN_POINT('Ctrl Pts',(-0.769485566245459,1.,-3.98480422348403));
#67907=CARTESIAN_POINT('Ctrl Pts',(-0.770963190030504,-1.,-3.97726349165507));
#67908=CARTESIAN_POINT('Ctrl Pts',(-0.770963190030504,1.,-3.97726349165507));
#67909=CARTESIAN_POINT('Ctrl Pts',(-0.772400931772239,-1.,-3.96972446532832));
#67910=CARTESIAN_POINT('Ctrl Pts',(-0.772400931772239,1.,-3.96972446532832));
#67911=CARTESIAN_POINT('Ctrl Pts',(-0.773798212026683,-1.,-3.96218649639876));
#67912=CARTESIAN_POINT('Ctrl Pts',(-0.773798212026683,1.,-3.96218649639876));
#67913=CARTESIAN_POINT('Ctrl Pts',(-0.775154418039441,-1.,-3.95464885452364));
#67914=CARTESIAN_POINT('Ctrl Pts',(-0.775154418039441,1.,-3.95464885452364));
#67915=CARTESIAN_POINT('Ctrl Pts',(-0.77646896669796,-1.,-3.94711101619471));
#67916=CARTESIAN_POINT('Ctrl Pts',(-0.77646896669796,1.,-3.94711101619471));
#67917=CARTESIAN_POINT('Ctrl Pts',(-0.77774137056855,-1.,-3.93957296768098));
#67918=CARTESIAN_POINT('Ctrl Pts',(-0.77774137056855,1.,-3.93957296768098));
#67919=CARTESIAN_POINT('Ctrl Pts',(-0.778971308134786,-1.,-3.93203552473153));
#67920=CARTESIAN_POINT('Ctrl Pts',(-0.778971308134786,1.,-3.93203552473153));
#67921=CARTESIAN_POINT('Ctrl Pts',(-0.780158678615507,-1.,-3.92450058323799));
#67922=CARTESIAN_POINT('Ctrl Pts',(-0.780158678615507,1.,-3.92450058323799));
#67923=CARTESIAN_POINT('Ctrl Pts',(-0.781303428618344,-1.,-3.9169703605466));
#67924=CARTESIAN_POINT('Ctrl Pts',(-0.781303428618344,1.,-3.9169703605466));
#67925=CARTESIAN_POINT('Ctrl Pts',(-0.782405395622759,-1.,-3.90944671004536));
#67926=CARTESIAN_POINT('Ctrl Pts',(-0.782405395622759,1.,-3.90944671004536));
#67927=CARTESIAN_POINT('Ctrl Pts',(-0.783464141529082,-1.,-3.90193039043971));
#67928=CARTESIAN_POINT('Ctrl Pts',(-0.783464141529082,1.,-3.90193039043971));
#67929=CARTESIAN_POINT('Ctrl Pts',(-0.784478799358336,-1.,-3.89442039235105));
#67930=CARTESIAN_POINT('Ctrl Pts',(-0.784478799358336,1.,-3.89442039235105));
#67931=CARTESIAN_POINT('Ctrl Pts',(-0.785447890340723,-1.,-3.88691313167399));
#67932=CARTESIAN_POINT('Ctrl Pts',(-0.785447890340723,1.,-3.88691313167399));
#67933=CARTESIAN_POINT('Ctrl Pts',(-0.786369675812592,-1.,-3.87940402818186));
#67934=CARTESIAN_POINT('Ctrl Pts',(-0.786369675812592,1.,-3.87940402818186));
#67935=CARTESIAN_POINT('Ctrl Pts',(-0.78724252761798,-1.,-3.87188916600905));
#67936=CARTESIAN_POINT('Ctrl Pts',(-0.78724252761798,1.,-3.87188916600905));
#67937=CARTESIAN_POINT('Ctrl Pts',(-0.788065315093771,-1.,-3.86436702561342));
#67938=CARTESIAN_POINT('Ctrl Pts',(-0.788065315093771,1.,-3.86436702561342));
#67939=CARTESIAN_POINT('Ctrl Pts',(-0.788837734090688,-1.,-3.85683995872536));
#67940=CARTESIAN_POINT('Ctrl Pts',(-0.788837734090688,1.,-3.85683995872536));
#67941=CARTESIAN_POINT('Ctrl Pts',(-0.789560798155619,-1.,-3.8493163780891));
#67942=CARTESIAN_POINT('Ctrl Pts',(-0.789560798155619,1.,-3.8493163780891));
#67943=CARTESIAN_POINT('Ctrl Pts',(-0.790236124191289,-1.,-3.84180762342476));
#67944=CARTESIAN_POINT('Ctrl Pts',(-0.790236124191289,1.,-3.84180762342476));
#67945=CARTESIAN_POINT('Ctrl Pts',(-0.79086501270534,-1.,-3.83432392054804));
#67946=CARTESIAN_POINT('Ctrl Pts',(-0.79086501270534,1.,-3.83432392054804));
#67947=CARTESIAN_POINT('Ctrl Pts',(-0.791447528662381,-1.,-3.82687033899799));
#67948=CARTESIAN_POINT('Ctrl Pts',(-0.791447528662381,1.,-3.82687033899799));
#67949=CARTESIAN_POINT('Ctrl Pts',(-0.791981740718606,-1.,-3.81944345442237));
#67950=CARTESIAN_POINT('Ctrl Pts',(-0.791981740718606,1.,-3.81944345442237));
#67951=CARTESIAN_POINT('Ctrl Pts',(-0.792462483517568,-1.,-3.81202588694726));
#67952=CARTESIAN_POINT('Ctrl Pts',(-0.792462483517568,1.,-3.81202588694726));
#67953=CARTESIAN_POINT('Ctrl Pts',(-0.792882695234693,-1.,-3.80459229925598));
#67954=CARTESIAN_POINT('Ctrl Pts',(-0.792882695234693,1.,-3.80459229925598));
#67955=CARTESIAN_POINT('Ctrl Pts',(-0.7932356129732,-1.,-3.79711921389862));
#67956=CARTESIAN_POINT('Ctrl Pts',(-0.7932356129732,1.,-3.79711921389862));
#67957=CARTESIAN_POINT('Ctrl Pts',(-0.793516871680966,-1.,-3.78959439439222));
#67958=CARTESIAN_POINT('Ctrl Pts',(-0.793516871680966,1.,-3.78959439439222));
#67959=CARTESIAN_POINT('Ctrl Pts',(-0.793726235781339,-1.,-3.78202460377617));
#67960=CARTESIAN_POINT('Ctrl Pts',(-0.793726235781339,1.,-3.78202460377617));
#67961=CARTESIAN_POINT('Ctrl Pts',(-0.793870523787515,-1.,-3.77444863801264));
#67962=CARTESIAN_POINT('Ctrl Pts',(-0.793870523787515,1.,-3.77444863801264));
#67963=CARTESIAN_POINT('Ctrl Pts',(-0.793961083689141,-1.,-3.76692626931184));
#67964=CARTESIAN_POINT('Ctrl Pts',(-0.793961083689141,1.,-3.76692626931184));
#67965=CARTESIAN_POINT('Ctrl Pts',(-0.794008429135047,-1.,-3.75951468666325));
#67966=CARTESIAN_POINT('Ctrl Pts',(-0.794008429135047,1.,-3.75951468666325));
#67967=CARTESIAN_POINT('Ctrl Pts',(-0.794017347371441,-1.,-3.75224692493895));
#67968=CARTESIAN_POINT('Ctrl Pts',(-0.794017347371441,1.,-3.75224692493895));
#67969=CARTESIAN_POINT('Ctrl Pts',(-0.79398270045988,-1.,-3.74511357728827));
#67970=CARTESIAN_POINT('Ctrl Pts',(-0.79398270045988,1.,-3.74511357728827));
#67971=CARTESIAN_POINT('Ctrl Pts',(-0.79388270093679,-1.,-3.73803280541576));
#67972=CARTESIAN_POINT('Ctrl Pts',(-0.79388270093679,1.,-3.73803280541576));
#67973=CARTESIAN_POINT('Ctrl Pts',(-0.793682750269347,-1.,-3.7308691469564));
#67974=CARTESIAN_POINT('Ctrl Pts',(-0.793682750269347,1.,-3.7308691469564));
#67975=CARTESIAN_POINT('Ctrl Pts',(-0.79334702378387,-1.,-3.7234879729357));
#67976=CARTESIAN_POINT('Ctrl Pts',(-0.79334702378387,1.,-3.7234879729357));
#67977=CARTESIAN_POINT('Ctrl Pts',(-0.792848377370115,-1.,-3.7158024239604));
#67978=CARTESIAN_POINT('Ctrl Pts',(-0.792848377370115,1.,-3.7158024239604));
#67979=CARTESIAN_POINT('Ctrl Pts',(-0.792177688845968,-1.,-3.70781724021879));
#67980=CARTESIAN_POINT('Ctrl Pts',(-0.792177688845968,1.,-3.70781724021879));
#67981=CARTESIAN_POINT('Ctrl Pts',(-0.791356575696509,-1.,-3.69968940808982));
#67982=CARTESIAN_POINT('Ctrl Pts',(-0.791356575696509,1.,-3.69968940808982));
#67983=CARTESIAN_POINT('Ctrl Pts',(-0.79043628498958,-1.,-3.69172044327754));
#67984=CARTESIAN_POINT('Ctrl Pts',(-0.79043628498958,1.,-3.69172044327754));
#67985=CARTESIAN_POINT('Ctrl Pts',(-0.789483546065158,-1.,-3.68428439784285));
#67986=CARTESIAN_POINT('Ctrl Pts',(-0.789483546065158,1.,-3.68428439784285));
#67987=CARTESIAN_POINT('Ctrl Pts',(-0.788569566220662,-1.,-3.67777119516438));
#67988=CARTESIAN_POINT('Ctrl Pts',(-0.788569566220662,1.,-3.67777119516438));
#67989=CARTESIAN_POINT('Ctrl Pts',(-0.787758799995426,-1.,-3.672529236635));
#67990=CARTESIAN_POINT('Ctrl Pts',(-0.787758799995426,1.,-3.672529236635));
#67991=CARTESIAN_POINT('Ctrl Pts',(-0.787095252589508,-1.,-3.66879484800625));
#67992=CARTESIAN_POINT('Ctrl Pts',(-0.787095252589508,1.,-3.66879484800625));
#67993=CARTESIAN_POINT('Ctrl Pts',(-0.786698783541658,-1.,-3.66710211819938));
#67994=CARTESIAN_POINT('Ctrl Pts',(-0.786698783541658,1.,-3.66710211819938));
#67995=CARTESIAN_POINT('Ctrl Pts',(-0.786480236184947,-1.,-3.66657784454965));
#67996=CARTESIAN_POINT('Ctrl Pts',(-0.786480236184947,1.,-3.66657784454965));
#67997=CARTESIAN_POINT('Ctrl Pts',(-0.786369528183039,-1.,-3.66655932661846));
#67998=CARTESIAN_POINT('Ctrl Pts',(-0.786369528183039,1.,-3.66655932661846));
#67999=CARTESIAN_POINT('Ctrl Pts',(-0.786322922920599,-1.,-3.66663282329846));
#68000=CARTESIAN_POINT('Ctrl Pts',(-0.786322922920599,1.,-3.66663282329846));
#68001=CARTESIAN_POINT('',(-0.732042837400619,1.,-4.13571194405636));
#68002=CARTESIAN_POINT('Ctrl Pts',(-0.732042837400619,1.,-4.13571194405636));
#68003=CARTESIAN_POINT('Ctrl Pts',(-0.732488575135926,1.,-4.13420383737278));
#68004=CARTESIAN_POINT('Ctrl Pts',(-0.733376589325634,1.,-4.13118752796397));
#68005=CARTESIAN_POINT('Ctrl Pts',(-0.734698226767512,1.,-4.12666277572794));
#68006=CARTESIAN_POINT('Ctrl Pts',(-0.736439634335347,1.,-4.12062919626082));
#68007=CARTESIAN_POINT('Ctrl Pts',(-0.738581708229119,1.,-4.11308626953795));
#68008=CARTESIAN_POINT('Ctrl Pts',(-0.740688998555152,1.,-4.1055424175856));
#68009=CARTESIAN_POINT('Ctrl Pts',(-0.742761369690018,1.,-4.09799769702712));
#68010=CARTESIAN_POINT('Ctrl Pts',(-0.744798649705514,1.,-4.09045220253011));
#68011=CARTESIAN_POINT('Ctrl Pts',(-0.746800631490822,1.,-4.08290608094789));
#68012=CARTESIAN_POINT('Ctrl Pts',(-0.748767076679177,1.,-4.07535951055363));
#68013=CARTESIAN_POINT('Ctrl Pts',(-0.750697720483176,1.,-4.06781267241886));
#68014=CARTESIAN_POINT('Ctrl Pts',(-0.752592276482869,1.,-4.06026572221399));
#68015=CARTESIAN_POINT('Ctrl Pts',(-0.754450441816412,1.,-4.05271876688106));
#68016=CARTESIAN_POINT('Ctrl Pts',(-0.756271902370187,1.,-4.04517182654344));
#68017=CARTESIAN_POINT('Ctrl Pts',(-0.758056338885554,1.,-4.03762485803468));
#68018=CARTESIAN_POINT('Ctrl Pts',(-0.759803433244166,1.,-4.0300778195465));
#68019=CARTESIAN_POINT('Ctrl Pts',(-0.761512875859942,1.,-4.02253072741347));
#68020=CARTESIAN_POINT('Ctrl Pts',(-0.763184371182827,1.,-4.01498370680434));
#68021=CARTESIAN_POINT('Ctrl Pts',(-0.764817648784946,1.,-4.00743706791366));
#68022=CARTESIAN_POINT('Ctrl Pts',(-0.766412457135786,1.,-3.99989129179464));
#68023=CARTESIAN_POINT('Ctrl Pts',(-0.767968531377708,1.,-3.99234687880892));
#68024=CARTESIAN_POINT('Ctrl Pts',(-0.769485566245459,1.,-3.98480422348403));
#68025=CARTESIAN_POINT('Ctrl Pts',(-0.770963190030504,1.,-3.97726349165507));
#68026=CARTESIAN_POINT('Ctrl Pts',(-0.772400931772239,1.,-3.96972446532832));
#68027=CARTESIAN_POINT('Ctrl Pts',(-0.773798212026683,1.,-3.96218649639876));
#68028=CARTESIAN_POINT('Ctrl Pts',(-0.775154418039441,1.,-3.95464885452364));
#68029=CARTESIAN_POINT('Ctrl Pts',(-0.77646896669796,1.,-3.94711101619471));
#68030=CARTESIAN_POINT('Ctrl Pts',(-0.77774137056855,1.,-3.93957296768098));
#68031=CARTESIAN_POINT('Ctrl Pts',(-0.778971308134786,1.,-3.93203552473153));
#68032=CARTESIAN_POINT('Ctrl Pts',(-0.780158678615507,1.,-3.92450058323799));
#68033=CARTESIAN_POINT('Ctrl Pts',(-0.781303428618344,1.,-3.9169703605466));
#68034=CARTESIAN_POINT('Ctrl Pts',(-0.782405395622759,1.,-3.90944671004536));
#68035=CARTESIAN_POINT('Ctrl Pts',(-0.783464141529082,1.,-3.90193039043971));
#68036=CARTESIAN_POINT('Ctrl Pts',(-0.784478799358336,1.,-3.89442039235105));
#68037=CARTESIAN_POINT('Ctrl Pts',(-0.785447890340723,1.,-3.88691313167399));
#68038=CARTESIAN_POINT('Ctrl Pts',(-0.786369675812592,1.,-3.87940402818186));
#68039=CARTESIAN_POINT('Ctrl Pts',(-0.78724252761798,1.,-3.87188916600905));
#68040=CARTESIAN_POINT('Ctrl Pts',(-0.788065315093771,1.,-3.86436702561342));
#68041=CARTESIAN_POINT('Ctrl Pts',(-0.788837734090688,1.,-3.85683995872536));
#68042=CARTESIAN_POINT('Ctrl Pts',(-0.789560798155619,1.,-3.8493163780891));
#68043=CARTESIAN_POINT('Ctrl Pts',(-0.790236124191289,1.,-3.84180762342476));
#68044=CARTESIAN_POINT('Ctrl Pts',(-0.79086501270534,1.,-3.83432392054804));
#68045=CARTESIAN_POINT('Ctrl Pts',(-0.791447528662381,1.,-3.82687033899799));
#68046=CARTESIAN_POINT('Ctrl Pts',(-0.791981740718606,1.,-3.81944345442237));
#68047=CARTESIAN_POINT('Ctrl Pts',(-0.792462483517568,1.,-3.81202588694726));
#68048=CARTESIAN_POINT('Ctrl Pts',(-0.792882695234693,1.,-3.80459229925598));
#68049=CARTESIAN_POINT('Ctrl Pts',(-0.7932356129732,1.,-3.79711921389862));
#68050=CARTESIAN_POINT('Ctrl Pts',(-0.793516871680966,1.,-3.78959439439222));
#68051=CARTESIAN_POINT('Ctrl Pts',(-0.793726235781339,1.,-3.78202460377617));
#68052=CARTESIAN_POINT('Ctrl Pts',(-0.793870523787515,1.,-3.77444863801264));
#68053=CARTESIAN_POINT('Ctrl Pts',(-0.793961083689141,1.,-3.76692626931184));
#68054=CARTESIAN_POINT('Ctrl Pts',(-0.794008429135047,1.,-3.75951468666325));
#68055=CARTESIAN_POINT('Ctrl Pts',(-0.794017347371441,1.,-3.75224692493895));
#68056=CARTESIAN_POINT('Ctrl Pts',(-0.79398270045988,1.,-3.74511357728827));
#68057=CARTESIAN_POINT('Ctrl Pts',(-0.79388270093679,1.,-3.73803280541576));
#68058=CARTESIAN_POINT('Ctrl Pts',(-0.793682750269347,1.,-3.7308691469564));
#68059=CARTESIAN_POINT('Ctrl Pts',(-0.79334702378387,1.,-3.7234879729357));
#68060=CARTESIAN_POINT('Ctrl Pts',(-0.792848377370115,1.,-3.7158024239604));
#68061=CARTESIAN_POINT('Ctrl Pts',(-0.792177688845968,1.,-3.70781724021879));
#68062=CARTESIAN_POINT('Ctrl Pts',(-0.791356575696509,1.,-3.69968940808982));
#68063=CARTESIAN_POINT('Ctrl Pts',(-0.79043628498958,1.,-3.69172044327754));
#68064=CARTESIAN_POINT('Ctrl Pts',(-0.789483546065158,1.,-3.68428439784285));
#68065=CARTESIAN_POINT('Ctrl Pts',(-0.788569566220662,1.,-3.67777119516438));
#68066=CARTESIAN_POINT('Ctrl Pts',(-0.787758799995426,1.,-3.672529236635));
#68067=CARTESIAN_POINT('Ctrl Pts',(-0.787145041181589,1.,-3.66907505398769));
#68068=CARTESIAN_POINT('Ctrl Pts',(-0.7867743371985,1.,-3.66743103898844));
#68069=CARTESIAN_POINT('Ctrl Pts',(-0.78656591955989,1.,-3.66680946938396));
#68070=CARTESIAN_POINT('Ctrl Pts',(-0.786459983896781,1.,-3.66664310415236));
#68071=CARTESIAN_POINT('Ctrl Pts',(-0.786422660833743,1.,-3.66661143271648));
#68072=CARTESIAN_POINT('',(-0.732042837400619,0.,-4.13571194405636));
#68073=CARTESIAN_POINT('Ctrl Pts',(-0.385214314776329,-1.,-3.73016218570874));
#68074=CARTESIAN_POINT('Ctrl Pts',(-0.385214314776329,1.,-3.73016218570874));
#68075=CARTESIAN_POINT('Ctrl Pts',(-0.385147278814804,-1.,-3.73010668803185));
#68076=CARTESIAN_POINT('Ctrl Pts',(-0.385147278814804,1.,-3.73010668803185));
#68077=CARTESIAN_POINT('Ctrl Pts',(-0.385047711603887,-1.,-3.73015851028729));
#68078=CARTESIAN_POINT('Ctrl Pts',(-0.385047711603887,1.,-3.73015851028729));
#68079=CARTESIAN_POINT('Ctrl Pts',(-0.385001870183841,-1.,-3.73072465900727));
#68080=CARTESIAN_POINT('Ctrl Pts',(-0.385001870183841,1.,-3.73072465900727));
#68081=CARTESIAN_POINT('Ctrl Pts',(-0.385147887989515,-1.,-3.73245705639337));
#68082=CARTESIAN_POINT('Ctrl Pts',(-0.385147887989515,1.,-3.73245705639337));
#68083=CARTESIAN_POINT('Ctrl Pts',(-0.385670806454744,-1.,-3.73621371845475));
#68084=CARTESIAN_POINT('Ctrl Pts',(-0.385670806454744,1.,-3.73621371845475));
#68085=CARTESIAN_POINT('Ctrl Pts',(-0.386519576222035,-1.,-3.74144965781088));
#68086=CARTESIAN_POINT('Ctrl Pts',(-0.386519576222035,1.,-3.74144965781088));
#68087=CARTESIAN_POINT('Ctrl Pts',(-0.387663020050396,-1.,-3.74792651696269));
#68088=CARTESIAN_POINT('Ctrl Pts',(-0.387663020050396,1.,-3.74792651696269));
#68089=CARTESIAN_POINT('Ctrl Pts',(-0.389054775898251,-1.,-3.75529302894757));
#68090=CARTESIAN_POINT('Ctrl Pts',(-0.389054775898251,1.,-3.75529302894757));
#68091=CARTESIAN_POINT('Ctrl Pts',(-0.390642072979259,-1.,-3.76315635032993));
#68092=CARTESIAN_POINT('Ctrl Pts',(-0.390642072979259,1.,-3.76315635032993));
#68093=CARTESIAN_POINT('Ctrl Pts',(-0.392372786223347,-1.,-3.77114011595892));
#68094=CARTESIAN_POINT('Ctrl Pts',(-0.392372786223347,1.,-3.77114011595892));
#68095=CARTESIAN_POINT('Ctrl Pts',(-0.394202481011595,-1.,-3.77894173114368));
#68096=CARTESIAN_POINT('Ctrl Pts',(-0.394202481011595,1.,-3.77894173114368));
#68097=CARTESIAN_POINT('Ctrl Pts',(-0.396103205335029,-1.,-3.78640521279479));
#68098=CARTESIAN_POINT('Ctrl Pts',(-0.396103205335029,1.,-3.78640521279479));
#68099=CARTESIAN_POINT('Ctrl Pts',(-0.398064818684158,-1.,-3.79352887163457));
#68100=CARTESIAN_POINT('Ctrl Pts',(-0.398064818684158,1.,-3.79352887163457));
#68101=CARTESIAN_POINT('Ctrl Pts',(-0.400088346504727,-1.,-3.80040370384659));
#68102=CARTESIAN_POINT('Ctrl Pts',(-0.400088346504727,1.,-3.80040370384659));
#68103=CARTESIAN_POINT('Ctrl Pts',(-0.402181320148475,-1.,-3.80716881962763));
#68104=CARTESIAN_POINT('Ctrl Pts',(-0.402181320148475,1.,-3.80716881962763));
#68105=CARTESIAN_POINT('Ctrl Pts',(-0.404352694628236,-1.,-3.81396374287762));
#68106=CARTESIAN_POINT('Ctrl Pts',(-0.404352694628236,1.,-3.81396374287762));
#68107=CARTESIAN_POINT('Ctrl Pts',(-0.406607038258906,-1.,-3.82087303913741));
#68108=CARTESIAN_POINT('Ctrl Pts',(-0.406607038258906,1.,-3.82087303913741));
#68109=CARTESIAN_POINT('Ctrl Pts',(-0.408942371447377,-1.,-3.82790724256397));
#68110=CARTESIAN_POINT('Ctrl Pts',(-0.408942371447377,1.,-3.82790724256397));
#68111=CARTESIAN_POINT('Ctrl Pts',(-0.41135303879846,-1.,-3.83503345578645));
#68112=CARTESIAN_POINT('Ctrl Pts',(-0.41135303879846,1.,-3.83503345578645));
#68113=CARTESIAN_POINT('Ctrl Pts',(-0.413831367016727,-1.,-3.84219403994742));
#68114=CARTESIAN_POINT('Ctrl Pts',(-0.413831367016727,1.,-3.84219403994742));
#68115=CARTESIAN_POINT('Ctrl Pts',(-0.41636967805292,-1.,-3.8493286415751));
#68116=CARTESIAN_POINT('Ctrl Pts',(-0.41636967805292,1.,-3.8493286415751));
#68117=CARTESIAN_POINT('Ctrl Pts',(-0.41896246808681,-1.,-3.85639825648031));
#68118=CARTESIAN_POINT('Ctrl Pts',(-0.41896246808681,1.,-3.85639825648031));
#68119=CARTESIAN_POINT('Ctrl Pts',(-0.421607423177576,-1.,-3.86339652542749));
#68120=CARTESIAN_POINT('Ctrl Pts',(-0.421607423177576,1.,-3.86339652542749));
#68121=CARTESIAN_POINT('Ctrl Pts',(-0.424304173195142,-1.,-3.87033643487882));
#68122=CARTESIAN_POINT('Ctrl Pts',(-0.424304173195142,1.,-3.87033643487882));
#68123=CARTESIAN_POINT('Ctrl Pts',(-0.427053541173469,-1.,-3.87724240306609));
#68124=CARTESIAN_POINT('Ctrl Pts',(-0.427053541173469,1.,-3.87724240306609));
#68125=CARTESIAN_POINT('Ctrl Pts',(-0.429856640579734,-1.,-3.88414070943334));
#68126=CARTESIAN_POINT('Ctrl Pts',(-0.429856640579734,1.,-3.88414070943334));
#68127=CARTESIAN_POINT('Ctrl Pts',(-0.432713929544439,-1.,-3.89104947940592));
#68128=CARTESIAN_POINT('Ctrl Pts',(-0.432713929544439,1.,-3.89104947940592));
#68129=CARTESIAN_POINT('Ctrl Pts',(-0.435624629433506,-1.,-3.8979725665544));
#68130=CARTESIAN_POINT('Ctrl Pts',(-0.435624629433506,1.,-3.8979725665544));
#68131=CARTESIAN_POINT('Ctrl Pts',(-0.438587235458233,-1.,-3.90490512938546));
#68132=CARTESIAN_POINT('Ctrl Pts',(-0.438587235458233,1.,-3.90490512938546));
#68133=CARTESIAN_POINT('Ctrl Pts',(-0.441599824524047,-1.,-3.91183704069146));
#68134=CARTESIAN_POINT('Ctrl Pts',(-0.441599824524047,1.,-3.91183704069146));
#68135=CARTESIAN_POINT('Ctrl Pts',(-0.444660430230593,-1.,-3.91875701610721));
#68136=CARTESIAN_POINT('Ctrl Pts',(-0.444660430230593,1.,-3.91875701610721));
#68137=CARTESIAN_POINT('Ctrl Pts',(-0.447767416837297,-1.,-3.92565674143424));
#68138=CARTESIAN_POINT('Ctrl Pts',(-0.447767416837297,1.,-3.92565674143424));
#68139=CARTESIAN_POINT('Ctrl Pts',(-0.450919768356347,-1.,-3.93253407403128));
#68140=CARTESIAN_POINT('Ctrl Pts',(-0.450919768356347,1.,-3.93253407403128));
#68141=CARTESIAN_POINT('Ctrl Pts',(-0.454116879027576,-1.,-3.93939080846298));
#68142=CARTESIAN_POINT('Ctrl Pts',(-0.454116879027576,1.,-3.93939080846298));
#68143=CARTESIAN_POINT('Ctrl Pts',(-0.457358410451674,-1.,-3.94623117206675));
#68144=CARTESIAN_POINT('Ctrl Pts',(-0.457358410451674,1.,-3.94623117206675));
#68145=CARTESIAN_POINT('Ctrl Pts',(-0.460644124429119,-1.,-3.95306005817363));
#68146=CARTESIAN_POINT('Ctrl Pts',(-0.460644124429119,1.,-3.95306005817363));
#68147=CARTESIAN_POINT('Ctrl Pts',(-0.463973722115744,-1.,-3.95988133243543));
#68148=CARTESIAN_POINT('Ctrl Pts',(-0.463973722115744,1.,-3.95988133243543));
#68149=CARTESIAN_POINT('Ctrl Pts',(-0.467346690880672,-1.,-3.96669622273946));
#68150=CARTESIAN_POINT('Ctrl Pts',(-0.467346690880672,1.,-3.96669622273946));
#68151=CARTESIAN_POINT('Ctrl Pts',(-0.470762379613477,-1.,-3.97350414289415));
#68152=CARTESIAN_POINT('Ctrl Pts',(-0.470762379613477,1.,-3.97350414289415));
#68153=CARTESIAN_POINT('Ctrl Pts',(-0.474220061019542,-1.,-3.9803033804443));
#68154=CARTESIAN_POINT('Ctrl Pts',(-0.474220061019542,1.,-3.9803033804443));
#68155=CARTESIAN_POINT('Ctrl Pts',(-0.477718999122033,-1.,-3.98709184306743));
#68156=CARTESIAN_POINT('Ctrl Pts',(-0.477718999122033,1.,-3.98709184306743));
#68157=CARTESIAN_POINT('Ctrl Pts',(-0.481258512209638,-1.,-3.99386775880655));
#68158=CARTESIAN_POINT('Ctrl Pts',(-0.481258512209638,1.,-3.99386775880655));
#68159=CARTESIAN_POINT('Ctrl Pts',(-0.484838042421754,-1.,-4.00063045119234));
#68160=CARTESIAN_POINT('Ctrl Pts',(-0.484838042421754,1.,-4.00063045119234));
#68161=CARTESIAN_POINT('Ctrl Pts',(-0.488457130424531,-1.,-4.0073800839092));
#68162=CARTESIAN_POINT('Ctrl Pts',(-0.488457130424531,1.,-4.0073800839092));
#68163=CARTESIAN_POINT('Ctrl Pts',(-0.492115383417931,-1.,-4.01411733503486));
#68164=CARTESIAN_POINT('Ctrl Pts',(-0.492115383417931,1.,-4.01411733503486));
#68165=CARTESIAN_POINT('Ctrl Pts',(-0.495812444326223,-1.,-4.02084308851813));
#68166=CARTESIAN_POINT('Ctrl Pts',(-0.495812444326223,1.,-4.02084308851813));
#68167=CARTESIAN_POINT('Ctrl Pts',(-0.49954796234089,-1.,-4.0275581398015));
#68168=CARTESIAN_POINT('Ctrl Pts',(-0.49954796234089,1.,-4.0275581398015));
#68169=CARTESIAN_POINT('Ctrl Pts',(-0.503321556915514,-1.,-4.0342628417439));
#68170=CARTESIAN_POINT('Ctrl Pts',(-0.503321556915514,1.,-4.0342628417439));
#68171=CARTESIAN_POINT('Ctrl Pts',(-0.507132823288362,-1.,-4.04095715149074));
#68172=CARTESIAN_POINT('Ctrl Pts',(-0.507132823288362,1.,-4.04095715149074));
#68173=CARTESIAN_POINT('Ctrl Pts',(-0.510981349219174,-1.,-4.04764078815591));
#68174=CARTESIAN_POINT('Ctrl Pts',(-0.510981349219174,1.,-4.04764078815591));
#68175=CARTESIAN_POINT('Ctrl Pts',(-0.514866728193104,-1.,-4.05431335771261));
#68176=CARTESIAN_POINT('Ctrl Pts',(-0.514866728193104,1.,-4.05431335771261));
#68177=CARTESIAN_POINT('Ctrl Pts',(-0.51878857233681,-1.,-4.06097448037934));
#68178=CARTESIAN_POINT('Ctrl Pts',(-0.51878857233681,1.,-4.06097448037934));
#68179=CARTESIAN_POINT('Ctrl Pts',(-0.522746528602768,-1.,-4.06762394471075));
#68180=CARTESIAN_POINT('Ctrl Pts',(-0.522746528602768,1.,-4.06762394471075));
#68181=CARTESIAN_POINT('Ctrl Pts',(-0.526740277227,-1.,-4.07426172299496));
#68182=CARTESIAN_POINT('Ctrl Pts',(-0.526740277227,1.,-4.07426172299496));
#68183=CARTESIAN_POINT('Ctrl Pts',(-0.530769518728075,-1.,-4.08088789536488));
#68184=CARTESIAN_POINT('Ctrl Pts',(-0.530769518728075,1.,-4.08088789536488));
#68185=CARTESIAN_POINT('Ctrl Pts',(-0.534833963476999,-1.,-4.08750259988693));
#68186=CARTESIAN_POINT('Ctrl Pts',(-0.534833963476999,1.,-4.08750259988693));
#68187=CARTESIAN_POINT('Ctrl Pts',(-0.538933321179921,-1.,-4.09410597627116));
#68188=CARTESIAN_POINT('Ctrl Pts',(-0.538933321179921,1.,-4.09410597627116));
#68189=CARTESIAN_POINT('Ctrl Pts',(-0.543067286878457,-1.,-4.10069810244473));
#68190=CARTESIAN_POINT('Ctrl Pts',(-0.543067286878457,1.,-4.10069810244473));
#68191=CARTESIAN_POINT('Ctrl Pts',(-0.54723553948676,-1.,-4.1072789702877));
#68192=CARTESIAN_POINT('Ctrl Pts',(-0.54723553948676,1.,-4.1072789702877));
#68193=CARTESIAN_POINT('Ctrl Pts',(-0.551437758498247,-1.,-4.11384852025578));
#68194=CARTESIAN_POINT('Ctrl Pts',(-0.551437758498247,1.,-4.11384852025578));
#68195=CARTESIAN_POINT('Ctrl Pts',(-0.555673636130778,-1.,-4.1204066619623));
#68196=CARTESIAN_POINT('Ctrl Pts',(-0.555673636130778,1.,-4.1204066619623));
#68197=CARTESIAN_POINT('Ctrl Pts',(-0.559942890594628,-1.,-4.12695329951859));
#68198=CARTESIAN_POINT('Ctrl Pts',(-0.559942890594628,1.,-4.12695329951859));
#68199=CARTESIAN_POINT('Ctrl Pts',(-0.564245279535705,-1.,-4.13348835726086));
#68200=CARTESIAN_POINT('Ctrl Pts',(-0.564245279535705,1.,-4.13348835726086));
#68201=CARTESIAN_POINT('Ctrl Pts',(-0.568580610187116,-1.,-4.14001179828669));
#68202=CARTESIAN_POINT('Ctrl Pts',(-0.568580610187116,1.,-4.14001179828669));
#68203=CARTESIAN_POINT('Ctrl Pts',(-0.572948736066277,-1.,-4.14652361065787));
#68204=CARTESIAN_POINT('Ctrl Pts',(-0.572948736066277,1.,-4.14652361065787));
#68205=CARTESIAN_POINT('Ctrl Pts',(-0.576469391673917,-1.,-4.1517237611974));
#68206=CARTESIAN_POINT('Ctrl Pts',(-0.576469391673917,1.,-4.1517237611974));
#68207=CARTESIAN_POINT('Ctrl Pts',(-0.579124568912543,-1.,-4.15561864787379));
#68208=CARTESIAN_POINT('Ctrl Pts',(-0.579124568912543,1.,-4.15561864787379));
#68209=CARTESIAN_POINT('Ctrl Pts',(-0.580901211462913,-1.,-4.15821291712391));
#68210=CARTESIAN_POINT('Ctrl Pts',(-0.580901211462913,1.,-4.15821291712391));
#68211=CARTESIAN_POINT('Ctrl Pts',(-0.581791163835814,-1.,-4.15950947128175));
#68212=CARTESIAN_POINT('Ctrl Pts',(-0.581791163835814,1.,-4.15950947128175));
#68213=CARTESIAN_POINT('',(-0.385112848332548,1.,-3.73017266276632));
#68214=CARTESIAN_POINT('Ctrl Pts',(-0.385112848332549,-1.,-3.73017266276632));
#68215=CARTESIAN_POINT('Ctrl Pts',(-0.385112848332549,-0.666666666666667,
-3.73017266276632));
#68216=CARTESIAN_POINT('Ctrl Pts',(-0.385112848332549,-0.333333333333333,
-3.73017266276632));
#68217=CARTESIAN_POINT('Ctrl Pts',(-0.385112848332549,0.333333333333333,
-3.73017266276632));
#68218=CARTESIAN_POINT('Ctrl Pts',(-0.385112848332549,0.666666666666667,
-3.73017266276632));
#68219=CARTESIAN_POINT('Ctrl Pts',(-0.385112848332549,1.,-3.73017266276632));
#68220=CARTESIAN_POINT('',(-0.581791163835814,1.,-4.15950947128175));
#68221=CARTESIAN_POINT('',(-0.581791163835814,0.,-4.15950947128175));
#68222=CARTESIAN_POINT('Ctrl Pts',(-0.385112848332549,1.,-3.73017266276632));
#68223=CARTESIAN_POINT('Ctrl Pts',(-0.385087139001609,1.,-3.73021431755218));
#68224=CARTESIAN_POINT('Ctrl Pts',(-0.385037797882046,1.,-3.73040527620929));
#68225=CARTESIAN_POINT('Ctrl Pts',(-0.385031656499142,1.,-3.731060828624));
#68226=CARTESIAN_POINT('Ctrl Pts',(-0.385187124633965,1.,-3.73273893363318));
#68227=CARTESIAN_POINT('Ctrl Pts',(-0.385670806454744,1.,-3.73621371845475));
#68228=CARTESIAN_POINT('Ctrl Pts',(-0.386519576222035,1.,-3.74144965781088));
#68229=CARTESIAN_POINT('Ctrl Pts',(-0.387663020050396,1.,-3.74792651696269));
#68230=CARTESIAN_POINT('Ctrl Pts',(-0.389054775898251,1.,-3.75529302894757));
#68231=CARTESIAN_POINT('Ctrl Pts',(-0.390642072979259,1.,-3.76315635032993));
#68232=CARTESIAN_POINT('Ctrl Pts',(-0.392372786223347,1.,-3.77114011595892));
#68233=CARTESIAN_POINT('Ctrl Pts',(-0.394202481011595,1.,-3.77894173114368));
#68234=CARTESIAN_POINT('Ctrl Pts',(-0.396103205335029,1.,-3.78640521279479));
#68235=CARTESIAN_POINT('Ctrl Pts',(-0.398064818684158,1.,-3.79352887163457));
#68236=CARTESIAN_POINT('Ctrl Pts',(-0.400088346504727,1.,-3.80040370384659));
#68237=CARTESIAN_POINT('Ctrl Pts',(-0.402181320148475,1.,-3.80716881962763));
#68238=CARTESIAN_POINT('Ctrl Pts',(-0.404352694628236,1.,-3.81396374287762));
#68239=CARTESIAN_POINT('Ctrl Pts',(-0.406607038258906,1.,-3.82087303913741));
#68240=CARTESIAN_POINT('Ctrl Pts',(-0.408942371447377,1.,-3.82790724256397));
#68241=CARTESIAN_POINT('Ctrl Pts',(-0.41135303879846,1.,-3.83503345578645));
#68242=CARTESIAN_POINT('Ctrl Pts',(-0.413831367016727,1.,-3.84219403994742));
#68243=CARTESIAN_POINT('Ctrl Pts',(-0.41636967805292,1.,-3.8493286415751));
#68244=CARTESIAN_POINT('Ctrl Pts',(-0.41896246808681,1.,-3.85639825648031));
#68245=CARTESIAN_POINT('Ctrl Pts',(-0.421607423177576,1.,-3.86339652542749));
#68246=CARTESIAN_POINT('Ctrl Pts',(-0.424304173195142,1.,-3.87033643487882));
#68247=CARTESIAN_POINT('Ctrl Pts',(-0.427053541173469,1.,-3.87724240306609));
#68248=CARTESIAN_POINT('Ctrl Pts',(-0.429856640579734,1.,-3.88414070943334));
#68249=CARTESIAN_POINT('Ctrl Pts',(-0.432713929544439,1.,-3.89104947940592));
#68250=CARTESIAN_POINT('Ctrl Pts',(-0.435624629433506,1.,-3.8979725665544));
#68251=CARTESIAN_POINT('Ctrl Pts',(-0.438587235458233,1.,-3.90490512938546));
#68252=CARTESIAN_POINT('Ctrl Pts',(-0.441599824524047,1.,-3.91183704069146));
#68253=CARTESIAN_POINT('Ctrl Pts',(-0.444660430230593,1.,-3.91875701610721));
#68254=CARTESIAN_POINT('Ctrl Pts',(-0.447767416837297,1.,-3.92565674143424));
#68255=CARTESIAN_POINT('Ctrl Pts',(-0.450919768356347,1.,-3.93253407403128));
#68256=CARTESIAN_POINT('Ctrl Pts',(-0.454116879027576,1.,-3.93939080846298));
#68257=CARTESIAN_POINT('Ctrl Pts',(-0.457358410451674,1.,-3.94623117206675));
#68258=CARTESIAN_POINT('Ctrl Pts',(-0.460644124429119,1.,-3.95306005817363));
#68259=CARTESIAN_POINT('Ctrl Pts',(-0.463973722115744,1.,-3.95988133243543));
#68260=CARTESIAN_POINT('Ctrl Pts',(-0.467346690880672,1.,-3.96669622273946));
#68261=CARTESIAN_POINT('Ctrl Pts',(-0.470762379613477,1.,-3.97350414289415));
#68262=CARTESIAN_POINT('Ctrl Pts',(-0.474220061019542,1.,-3.9803033804443));
#68263=CARTESIAN_POINT('Ctrl Pts',(-0.477718999122033,1.,-3.98709184306743));
#68264=CARTESIAN_POINT('Ctrl Pts',(-0.481258512209638,1.,-3.99386775880655));
#68265=CARTESIAN_POINT('Ctrl Pts',(-0.484838042421754,1.,-4.00063045119234));
#68266=CARTESIAN_POINT('Ctrl Pts',(-0.488457130424531,1.,-4.0073800839092));
#68267=CARTESIAN_POINT('Ctrl Pts',(-0.492115383417931,1.,-4.01411733503486));
#68268=CARTESIAN_POINT('Ctrl Pts',(-0.495812444326223,1.,-4.02084308851813));
#68269=CARTESIAN_POINT('Ctrl Pts',(-0.49954796234089,1.,-4.0275581398015));
#68270=CARTESIAN_POINT('Ctrl Pts',(-0.503321556915514,1.,-4.0342628417439));
#68271=CARTESIAN_POINT('Ctrl Pts',(-0.507132823288362,1.,-4.04095715149074));
#68272=CARTESIAN_POINT('Ctrl Pts',(-0.510981349219174,1.,-4.04764078815591));
#68273=CARTESIAN_POINT('Ctrl Pts',(-0.514866728193104,1.,-4.05431335771261));
#68274=CARTESIAN_POINT('Ctrl Pts',(-0.51878857233681,1.,-4.06097448037934));
#68275=CARTESIAN_POINT('Ctrl Pts',(-0.522746528602768,1.,-4.06762394471075));
#68276=CARTESIAN_POINT('Ctrl Pts',(-0.526740277227,1.,-4.07426172299496));
#68277=CARTESIAN_POINT('Ctrl Pts',(-0.530769518728075,1.,-4.08088789536488));
#68278=CARTESIAN_POINT('Ctrl Pts',(-0.534833963476999,1.,-4.08750259988693));
#68279=CARTESIAN_POINT('Ctrl Pts',(-0.538933321179921,1.,-4.09410597627116));
#68280=CARTESIAN_POINT('Ctrl Pts',(-0.543067286878457,1.,-4.10069810244473));
#68281=CARTESIAN_POINT('Ctrl Pts',(-0.54723553948676,1.,-4.1072789702877));
#68282=CARTESIAN_POINT('Ctrl Pts',(-0.551437758498247,1.,-4.11384852025578));
#68283=CARTESIAN_POINT('Ctrl Pts',(-0.555673636130778,1.,-4.1204066619623));
#68284=CARTESIAN_POINT('Ctrl Pts',(-0.559942890594628,1.,-4.12695329951859));
#68285=CARTESIAN_POINT('Ctrl Pts',(-0.564245279535705,1.,-4.13348835726086));
#68286=CARTESIAN_POINT('Ctrl Pts',(-0.568580610187116,1.,-4.14001179828669));
#68287=CARTESIAN_POINT('Ctrl Pts',(-0.572948736066277,1.,-4.14652361065787));
#68288=CARTESIAN_POINT('Ctrl Pts',(-0.576469391673917,1.,-4.1517237611974));
#68289=CARTESIAN_POINT('Ctrl Pts',(-0.579124568912543,1.,-4.15561864787379));
#68290=CARTESIAN_POINT('Ctrl Pts',(-0.580901211462913,1.,-4.15821291712391));
#68291=CARTESIAN_POINT('Ctrl Pts',(-0.581791163835814,1.,-4.15950947128175));
#68292=CARTESIAN_POINT('Origin',(-0.581791163835814,0.,-4.15950947128175));
#68293=CARTESIAN_POINT('',(-0.732042837400619,1.,-4.13571194405636));
#68294=CARTESIAN_POINT('Origin',(0.,0.,0.));
#68295=CARTESIAN_POINT('',(-0.203156094897896,1.,-3.74449296982994));
#68296=CARTESIAN_POINT('Origin',(0.,1.,0.));
#68297=CARTESIAN_POINT('Ctrl Pts',(-0.203156094897896,1.,-3.74449296982994));
#68298=CARTESIAN_POINT('Ctrl Pts',(-0.203156094897896,0.666666666666667,
-3.74449296982994));
#68299=CARTESIAN_POINT('Ctrl Pts',(-0.203156094897896,0.333333333333333,
-3.74449296982994));
#68300=CARTESIAN_POINT('Ctrl Pts',(-0.203156094897896,-0.333333333333333,
-3.74449296982994));
#68301=CARTESIAN_POINT('Ctrl Pts',(-0.203156094897896,-0.666666666666667,
-3.74449296982994));
#68302=CARTESIAN_POINT('Ctrl Pts',(-0.203156094897896,-1.,-3.74449296982994));
#68303=CARTESIAN_POINT('Ctrl Pts',(-0.0760622897878238,-1.,-4.19931119685982));
#68304=CARTESIAN_POINT('Ctrl Pts',(-0.0760622897878238,1.,-4.19931119685982));
#68305=CARTESIAN_POINT('Ctrl Pts',(-0.0767384596142197,-1.,-4.19789138621624));
#68306=CARTESIAN_POINT('Ctrl Pts',(-0.0767384596142197,1.,-4.19789138621624));
#68307=CARTESIAN_POINT('Ctrl Pts',(-0.0780873956244405,-1.,-4.19505112860624));
#68308=CARTESIAN_POINT('Ctrl Pts',(-0.0780873956244405,1.,-4.19505112860624));
#68309=CARTESIAN_POINT('Ctrl Pts',(-0.0801005887117605,-1.,-4.19078883322483));
#68310=CARTESIAN_POINT('Ctrl Pts',(-0.0801005887117605,1.,-4.19078883322483));
#68311=CARTESIAN_POINT('Ctrl Pts',(-0.0827644164389512,-1.,-4.1851019532944));
#68312=CARTESIAN_POINT('Ctrl Pts',(-0.0827644164389512,1.,-4.1851019532944));
#68313=CARTESIAN_POINT('Ctrl Pts',(-0.0860600915552517,-1.,-4.17798698669991));
#68314=CARTESIAN_POINT('Ctrl Pts',(-0.0860600915552517,1.,-4.17798698669991));
#68315=CARTESIAN_POINT('Ctrl Pts',(-0.089321556085033,-1.,-4.17086566491823));
#68316=CARTESIAN_POINT('Ctrl Pts',(-0.089321556085033,1.,-4.17086566491823));
#68317=CARTESIAN_POINT('Ctrl Pts',(-0.0925486672167692,-1.,-4.16373802265942));
#68318=CARTESIAN_POINT('Ctrl Pts',(-0.0925486672167692,1.,-4.16373802265942));
#68319=CARTESIAN_POINT('Ctrl Pts',(-0.095741240329707,-1.,-4.15660412653006));
#68320=CARTESIAN_POINT('Ctrl Pts',(-0.095741240329707,1.,-4.15660412653006));
#68321=CARTESIAN_POINT('Ctrl Pts',(-0.0988990478899814,-1.,-4.1494640891762));
#68322=CARTESIAN_POINT('Ctrl Pts',(-0.0988990478899814,1.,-4.1494640891762));
#68323=CARTESIAN_POINT('Ctrl Pts',(-0.102021826577454,-1.,-4.14231804938737));
#68324=CARTESIAN_POINT('Ctrl Pts',(-0.102021826577454,1.,-4.14231804938737));
#68325=CARTESIAN_POINT('Ctrl Pts',(-0.105109286538864,-1.,-4.13516614458396));
#68326=CARTESIAN_POINT('Ctrl Pts',(-0.105109286538864,1.,-4.13516614458396));
#68327=CARTESIAN_POINT('Ctrl Pts',(-0.10816112052835,-1.,-4.12800848371386));
#68328=CARTESIAN_POINT('Ctrl Pts',(-0.10816112052835,1.,-4.12800848371386));
#68329=CARTESIAN_POINT('Ctrl Pts',(-0.111177012683377,-1.,-4.12084512502444));
#68330=CARTESIAN_POINT('Ctrl Pts',(-0.111177012683377,1.,-4.12084512502444));
#68331=CARTESIAN_POINT('Ctrl Pts',(-0.114156649609602,-1.,-4.11367603925313));
#68332=CARTESIAN_POINT('Ctrl Pts',(-0.114156649609602,1.,-4.11367603925313));
#68333=CARTESIAN_POINT('Ctrl Pts',(-0.117099722731705,-1.,-4.10650113382187));
#68334=CARTESIAN_POINT('Ctrl Pts',(-0.117099722731705,1.,-4.10650113382187));
#68335=CARTESIAN_POINT('Ctrl Pts',(-0.120005924388162,-1.,-4.09932031767243));
#68336=CARTESIAN_POINT('Ctrl Pts',(-0.120005924388162,1.,-4.09932031767243));
#68337=CARTESIAN_POINT('Ctrl Pts',(-0.122874946249119,-1.,-4.09213355850836));
#68338=CARTESIAN_POINT('Ctrl Pts',(-0.122874946249119,1.,-4.09213355850836));
#68339=CARTESIAN_POINT('Ctrl Pts',(-0.125706476822529,-1.,-4.08494093372315));
#68340=CARTESIAN_POINT('Ctrl Pts',(-0.125706476822529,1.,-4.08494093372315));
#68341=CARTESIAN_POINT('Ctrl Pts',(-0.128500200484814,-1.,-4.07774270738809));
#68342=CARTESIAN_POINT('Ctrl Pts',(-0.128500200484814,1.,-4.07774270738809));
#68343=CARTESIAN_POINT('Ctrl Pts',(-0.131255793548914,-1.,-4.07053931528579));
#68344=CARTESIAN_POINT('Ctrl Pts',(-0.131255793548914,1.,-4.07053931528579));
#68345=CARTESIAN_POINT('Ctrl Pts',(-0.133972916144225,-1.,-4.06333121018476));
#68346=CARTESIAN_POINT('Ctrl Pts',(-0.133972916144225,1.,-4.06333121018476));
#68347=CARTESIAN_POINT('Ctrl Pts',(-0.136651205046111,-1.,-4.05611873400122));
#68348=CARTESIAN_POINT('Ctrl Pts',(-0.136651205046111,1.,-4.05611873400122));
#68349=CARTESIAN_POINT('Ctrl Pts',(-0.13929026718006,-1.,-4.04890199238056));
#68350=CARTESIAN_POINT('Ctrl Pts',(-0.13929026718006,1.,-4.04890199238056));
#68351=CARTESIAN_POINT('Ctrl Pts',(-0.141889671485508,-1.,-4.04168069633842));
#68352=CARTESIAN_POINT('Ctrl Pts',(-0.141889671485508,1.,-4.04168069633842));
#68353=CARTESIAN_POINT('Ctrl Pts',(-0.144448947038352,-1.,-4.03445411510403));
#68354=CARTESIAN_POINT('Ctrl Pts',(-0.144448947038352,1.,-4.03445411510403));
#68355=CARTESIAN_POINT('Ctrl Pts',(-0.146967602878999,-1.,-4.02722143147048));
#68356=CARTESIAN_POINT('Ctrl Pts',(-0.146967602878999,1.,-4.02722143147048));
#68357=CARTESIAN_POINT('Ctrl Pts',(-0.149445144968708,-1.,-4.01998203715588));
#68358=CARTESIAN_POINT('Ctrl Pts',(-0.149445144968708,1.,-4.01998203715588));
#68359=CARTESIAN_POINT('Ctrl Pts',(-0.151881094022909,-1.,-4.01273584234684));
#68360=CARTESIAN_POINT('Ctrl Pts',(-0.151881094022909,1.,-4.01273584234684));
#68361=CARTESIAN_POINT('Ctrl Pts',(-0.15427500487231,-1.,-4.00548360245297));
#68362=CARTESIAN_POINT('Ctrl Pts',(-0.15427500487231,1.,-4.00548360245297));
#68363=CARTESIAN_POINT('Ctrl Pts',(-0.156626481393736,-1.,-3.99822717425869));
#68364=CARTESIAN_POINT('Ctrl Pts',(-0.156626481393736,1.,-3.99822717425869));
#68365=CARTESIAN_POINT('Ctrl Pts',(-0.158935123982796,-1.,-3.99096873945862));
#68366=CARTESIAN_POINT('Ctrl Pts',(-0.158935123982796,1.,-3.99096873945862));
#68367=CARTESIAN_POINT('Ctrl Pts',(-0.161200482186088,-1.,-3.98371010319866));
#68368=CARTESIAN_POINT('Ctrl Pts',(-0.161200482186088,1.,-3.98371010319866));
#68369=CARTESIAN_POINT('Ctrl Pts',(-0.163422004609999,-1.,-3.97645194630944));
#68370=CARTESIAN_POINT('Ctrl Pts',(-0.163422004609999,1.,-3.97645194630944));
#68371=CARTESIAN_POINT('Ctrl Pts',(-0.165598992851098,-1.,-3.9691931362141));
#68372=CARTESIAN_POINT('Ctrl Pts',(-0.165598992851098,1.,-3.9691931362141));
#68373=CARTESIAN_POINT('Ctrl Pts',(-0.167730547023312,-1.,-3.96192990160296));
#68374=CARTESIAN_POINT('Ctrl Pts',(-0.167730547023312,1.,-3.96192990160296));
#68375=CARTESIAN_POINT('Ctrl Pts',(-0.16981566637413,-1.,-3.95465744665263));
#68376=CARTESIAN_POINT('Ctrl Pts',(-0.16981566637413,1.,-3.95465744665263));
#68377=CARTESIAN_POINT('Ctrl Pts',(-0.171853355369233,-1.,-3.94737164900861));
#68378=CARTESIAN_POINT('Ctrl Pts',(-0.171853355369233,1.,-3.94737164900861));
#68379=CARTESIAN_POINT('Ctrl Pts',(-0.173842734974607,-1.,-3.94007083096214));
#68380=CARTESIAN_POINT('Ctrl Pts',(-0.173842734974607,1.,-3.94007083096214));
#68381=CARTESIAN_POINT('Ctrl Pts',(-0.175783136893873,-1.,-3.93275726771049));
#68382=CARTESIAN_POINT('Ctrl Pts',(-0.175783136893873,1.,-3.93275726771049));
#68383=CARTESIAN_POINT('Ctrl Pts',(-0.177674246152328,-1.,-3.92543942697672));
#68384=CARTESIAN_POINT('Ctrl Pts',(-0.177674246152328,1.,-3.92543942697672));
#68385=CARTESIAN_POINT('Ctrl Pts',(-0.179515885822895,-1.,-3.91812876180948));
#68386=CARTESIAN_POINT('Ctrl Pts',(-0.179515885822895,1.,-3.91812876180948));
#68387=CARTESIAN_POINT('Ctrl Pts',(-0.181307740731796,-1.,-3.91083557557193));
#68388=CARTESIAN_POINT('Ctrl Pts',(-0.181307740731796,1.,-3.91083557557193));
#68389=CARTESIAN_POINT('Ctrl Pts',(-0.183049081993193,-1.,-3.90356488555138));
#68390=CARTESIAN_POINT('Ctrl Pts',(-0.183049081993193,1.,-3.90356488555138));
#68391=CARTESIAN_POINT('Ctrl Pts',(-0.184738537728035,-1.,-3.89631300742633));
#68392=CARTESIAN_POINT('Ctrl Pts',(-0.184738537728035,1.,-3.89631300742633));
#68393=CARTESIAN_POINT('Ctrl Pts',(-0.186373724985263,-1.,-3.88906196725817));
#68394=CARTESIAN_POINT('Ctrl Pts',(-0.186373724985263,1.,-3.88906196725817));
#68395=CARTESIAN_POINT('Ctrl Pts',(-0.187951632512663,-1.,-3.88178563496187));
#68396=CARTESIAN_POINT('Ctrl Pts',(-0.187951632512663,1.,-3.88178563496187));
#68397=CARTESIAN_POINT('Ctrl Pts',(-0.189469253358254,-1.,-3.87445976418377));
#68398=CARTESIAN_POINT('Ctrl Pts',(-0.189469253358254,1.,-3.87445976418377));
#68399=CARTESIAN_POINT('Ctrl Pts',(-0.190924190418613,-1.,-3.8670715862477));
#68400=CARTESIAN_POINT('Ctrl Pts',(-0.190924190418613,1.,-3.8670715862477));
#68401=CARTESIAN_POINT('Ctrl Pts',(-0.19231515304498,-1.,-3.85962774407652));
#68402=CARTESIAN_POINT('Ctrl Pts',(-0.19231515304498,1.,-3.85962774407652));
#68403=CARTESIAN_POINT('Ctrl Pts',(-0.193642806777748,-1.,-3.85216762264019));
#68404=CARTESIAN_POINT('Ctrl Pts',(-0.193642806777748,1.,-3.85216762264019));
#68405=CARTESIAN_POINT('Ctrl Pts',(-0.194909009460255,-1.,-3.84475203347052));
#68406=CARTESIAN_POINT('Ctrl Pts',(-0.194909009460255,1.,-3.84475203347052));
#68407=CARTESIAN_POINT('Ctrl Pts',(-0.19611519897189,-1.,-3.83743910616265));
#68408=CARTESIAN_POINT('Ctrl Pts',(-0.19611519897189,1.,-3.83743910616265));
#68409=CARTESIAN_POINT('Ctrl Pts',(-0.197260935827375,-1.,-3.83026221776488));
#68410=CARTESIAN_POINT('Ctrl Pts',(-0.197260935827375,1.,-3.83026221776488));
#68411=CARTESIAN_POINT('Ctrl Pts',(-0.19834261690047,-1.,-3.82321127348981));
#68412=CARTESIAN_POINT('Ctrl Pts',(-0.19834261690047,1.,-3.82321127348981));
#68413=CARTESIAN_POINT('Ctrl Pts',(-0.199351525297396,-1.,-3.81620203429702));
#68414=CARTESIAN_POINT('Ctrl Pts',(-0.199351525297396,1.,-3.81620203429702));
#68415=CARTESIAN_POINT('Ctrl Pts',(-0.20027467943329,-1.,-3.80909529318501));
#68416=CARTESIAN_POINT('Ctrl Pts',(-0.20027467943329,1.,-3.80909529318501));
#68417=CARTESIAN_POINT('Ctrl Pts',(-0.201097756307252,-1.,-3.80175247447171));
#68418=CARTESIAN_POINT('Ctrl Pts',(-0.201097756307252,1.,-3.80175247447171));
#68419=CARTESIAN_POINT('Ctrl Pts',(-0.201807533800799,-1.,-3.79408354187274));
#68420=CARTESIAN_POINT('Ctrl Pts',(-0.201807533800799,1.,-3.79408354187274));
#68421=CARTESIAN_POINT('Ctrl Pts',(-0.202394260512193,-1.,-3.78609175019317));
#68422=CARTESIAN_POINT('Ctrl Pts',(-0.202394260512193,1.,-3.78609175019317));
#68423=CARTESIAN_POINT('Ctrl Pts',(-0.202854729699197,-1.,-3.77793553476879));
#68424=CARTESIAN_POINT('Ctrl Pts',(-0.202854729699197,1.,-3.77793553476879));
#68425=CARTESIAN_POINT('Ctrl Pts',(-0.203192390045337,-1.,-3.76992071595267));
#68426=CARTESIAN_POINT('Ctrl Pts',(-0.203192390045337,1.,-3.76992071595267));
#68427=CARTESIAN_POINT('Ctrl Pts',(-0.203414634707646,-1.,-3.76242717937273));
#68428=CARTESIAN_POINT('Ctrl Pts',(-0.203414634707646,1.,-3.76242717937273));
#68429=CARTESIAN_POINT('Ctrl Pts',(-0.203530796848404,-1.,-3.75585118707924));
#68430=CARTESIAN_POINT('Ctrl Pts',(-0.203530796848404,1.,-3.75585118707924));
#68431=CARTESIAN_POINT('Ctrl Pts',(-0.203550035479097,-1.,-3.75054693397716));
#68432=CARTESIAN_POINT('Ctrl Pts',(-0.203550035479097,1.,-3.75054693397716));
#68433=CARTESIAN_POINT('Ctrl Pts',(-0.20347884453023,-1.,-3.74675472018582));
#68434=CARTESIAN_POINT('Ctrl Pts',(-0.20347884453023,1.,-3.74675472018582));
#68435=CARTESIAN_POINT('Ctrl Pts',(-0.203352057956055,-1.,-3.7450208092684));
#68436=CARTESIAN_POINT('Ctrl Pts',(-0.203352057956055,1.,-3.7450208092684));
#68437=CARTESIAN_POINT('Ctrl Pts',(-0.203218215747895,-1.,-3.74446880195845));
#68438=CARTESIAN_POINT('Ctrl Pts',(-0.203218215747895,1.,-3.74446880195845));
#68439=CARTESIAN_POINT('Ctrl Pts',(-0.20311176758786,-1.,-3.74443319346666));
#68440=CARTESIAN_POINT('Ctrl Pts',(-0.20311176758786,1.,-3.74443319346666));
#68441=CARTESIAN_POINT('Ctrl Pts',(-0.203054238699719,-1.,-3.74449849461127));
#68442=CARTESIAN_POINT('Ctrl Pts',(-0.203054238699719,1.,-3.74449849461127));
#68443=CARTESIAN_POINT('',(-0.0760622897878238,1.,-4.19931119685982));
#68444=CARTESIAN_POINT('Ctrl Pts',(-0.0760622897878238,1.,-4.19931119685982));
#68445=CARTESIAN_POINT('Ctrl Pts',(-0.0767384596142197,1.,-4.19789138621624));
#68446=CARTESIAN_POINT('Ctrl Pts',(-0.0780873956244405,1.,-4.19505112860624));
#68447=CARTESIAN_POINT('Ctrl Pts',(-0.0801005887117605,1.,-4.19078883322483));
#68448=CARTESIAN_POINT('Ctrl Pts',(-0.0827644164389512,1.,-4.1851019532944));
#68449=CARTESIAN_POINT('Ctrl Pts',(-0.0860600915552517,1.,-4.17798698669991));
#68450=CARTESIAN_POINT('Ctrl Pts',(-0.089321556085033,1.,-4.17086566491823));
#68451=CARTESIAN_POINT('Ctrl Pts',(-0.0925486672167692,1.,-4.16373802265942));
#68452=CARTESIAN_POINT('Ctrl Pts',(-0.095741240329707,1.,-4.15660412653006));
#68453=CARTESIAN_POINT('Ctrl Pts',(-0.0988990478899814,1.,-4.1494640891762));
#68454=CARTESIAN_POINT('Ctrl Pts',(-0.102021826577454,1.,-4.14231804938737));
#68455=CARTESIAN_POINT('Ctrl Pts',(-0.105109286538864,1.,-4.13516614458396));
#68456=CARTESIAN_POINT('Ctrl Pts',(-0.10816112052835,1.,-4.12800848371386));
#68457=CARTESIAN_POINT('Ctrl Pts',(-0.111177012683377,1.,-4.12084512502444));
#68458=CARTESIAN_POINT('Ctrl Pts',(-0.114156649609602,1.,-4.11367603925313));
#68459=CARTESIAN_POINT('Ctrl Pts',(-0.117099722731705,1.,-4.10650113382187));
#68460=CARTESIAN_POINT('Ctrl Pts',(-0.120005924388162,1.,-4.09932031767243));
#68461=CARTESIAN_POINT('Ctrl Pts',(-0.122874946249119,1.,-4.09213355850836));
#68462=CARTESIAN_POINT('Ctrl Pts',(-0.125706476822529,1.,-4.08494093372315));
#68463=CARTESIAN_POINT('Ctrl Pts',(-0.128500200484814,1.,-4.07774270738809));
#68464=CARTESIAN_POINT('Ctrl Pts',(-0.131255793548914,1.,-4.07053931528579));
#68465=CARTESIAN_POINT('Ctrl Pts',(-0.133972916144225,1.,-4.06333121018476));
#68466=CARTESIAN_POINT('Ctrl Pts',(-0.136651205046111,1.,-4.05611873400122));
#68467=CARTESIAN_POINT('Ctrl Pts',(-0.13929026718006,1.,-4.04890199238056));
#68468=CARTESIAN_POINT('Ctrl Pts',(-0.141889671485508,1.,-4.04168069633842));
#68469=CARTESIAN_POINT('Ctrl Pts',(-0.144448947038352,1.,-4.03445411510403));
#68470=CARTESIAN_POINT('Ctrl Pts',(-0.146967602878999,1.,-4.02722143147048));
#68471=CARTESIAN_POINT('Ctrl Pts',(-0.149445144968708,1.,-4.01998203715588));
#68472=CARTESIAN_POINT('Ctrl Pts',(-0.151881094022909,1.,-4.01273584234684));
#68473=CARTESIAN_POINT('Ctrl Pts',(-0.15427500487231,1.,-4.00548360245297));
#68474=CARTESIAN_POINT('Ctrl Pts',(-0.156626481393736,1.,-3.99822717425869));
#68475=CARTESIAN_POINT('Ctrl Pts',(-0.158935123982796,1.,-3.99096873945862));
#68476=CARTESIAN_POINT('Ctrl Pts',(-0.161200482186088,1.,-3.98371010319866));
#68477=CARTESIAN_POINT('Ctrl Pts',(-0.163422004609999,1.,-3.97645194630944));
#68478=CARTESIAN_POINT('Ctrl Pts',(-0.165598992851098,1.,-3.9691931362141));
#68479=CARTESIAN_POINT('Ctrl Pts',(-0.167730547023312,1.,-3.96192990160296));
#68480=CARTESIAN_POINT('Ctrl Pts',(-0.16981566637413,1.,-3.95465744665263));
#68481=CARTESIAN_POINT('Ctrl Pts',(-0.171853355369233,1.,-3.94737164900861));
#68482=CARTESIAN_POINT('Ctrl Pts',(-0.173842734974607,1.,-3.94007083096214));
#68483=CARTESIAN_POINT('Ctrl Pts',(-0.175783136893873,1.,-3.93275726771049));
#68484=CARTESIAN_POINT('Ctrl Pts',(-0.177674246152328,1.,-3.92543942697672));
#68485=CARTESIAN_POINT('Ctrl Pts',(-0.179515885822895,1.,-3.91812876180948));
#68486=CARTESIAN_POINT('Ctrl Pts',(-0.181307740731796,1.,-3.91083557557193));
#68487=CARTESIAN_POINT('Ctrl Pts',(-0.183049081993193,1.,-3.90356488555138));
#68488=CARTESIAN_POINT('Ctrl Pts',(-0.184738537728035,1.,-3.89631300742633));
#68489=CARTESIAN_POINT('Ctrl Pts',(-0.186373724985263,1.,-3.88906196725817));
#68490=CARTESIAN_POINT('Ctrl Pts',(-0.187951632512663,1.,-3.88178563496187));
#68491=CARTESIAN_POINT('Ctrl Pts',(-0.189469253358254,1.,-3.87445976418377));
#68492=CARTESIAN_POINT('Ctrl Pts',(-0.190924190418613,1.,-3.8670715862477));
#68493=CARTESIAN_POINT('Ctrl Pts',(-0.19231515304498,1.,-3.85962774407652));
#68494=CARTESIAN_POINT('Ctrl Pts',(-0.193642806777748,1.,-3.85216762264019));
#68495=CARTESIAN_POINT('Ctrl Pts',(-0.194909009460255,1.,-3.84475203347052));
#68496=CARTESIAN_POINT('Ctrl Pts',(-0.19611519897189,1.,-3.83743910616265));
#68497=CARTESIAN_POINT('Ctrl Pts',(-0.197260935827375,1.,-3.83026221776488));
#68498=CARTESIAN_POINT('Ctrl Pts',(-0.19834261690047,1.,-3.82321127348981));
#68499=CARTESIAN_POINT('Ctrl Pts',(-0.199351525297396,1.,-3.81620203429702));
#68500=CARTESIAN_POINT('Ctrl Pts',(-0.20027467943329,1.,-3.80909529318501));
#68501=CARTESIAN_POINT('Ctrl Pts',(-0.201097756307252,1.,-3.80175247447171));
#68502=CARTESIAN_POINT('Ctrl Pts',(-0.201807533800799,1.,-3.79408354187274));
#68503=CARTESIAN_POINT('Ctrl Pts',(-0.202394260512193,1.,-3.78609175019317));
#68504=CARTESIAN_POINT('Ctrl Pts',(-0.202854729699197,1.,-3.77793553476879));
#68505=CARTESIAN_POINT('Ctrl Pts',(-0.203192390045337,1.,-3.76992071595267));
#68506=CARTESIAN_POINT('Ctrl Pts',(-0.203414634707646,1.,-3.76242717937273));
#68507=CARTESIAN_POINT('Ctrl Pts',(-0.203530796848404,1.,-3.75585118707924));
#68508=CARTESIAN_POINT('Ctrl Pts',(-0.203550035479097,1.,-3.75054693397716));
#68509=CARTESIAN_POINT('Ctrl Pts',(-0.203484186269315,1.,-3.74703926501843));
#68510=CARTESIAN_POINT('Ctrl Pts',(-0.203375226874331,1.,-3.74535749969262));
#68511=CARTESIAN_POINT('Ctrl Pts',(-0.203266610111264,1.,-3.74471097893961));
#68512=CARTESIAN_POINT('Ctrl Pts',(-0.203188003947965,1.,-3.74453008995129));
#68513=CARTESIAN_POINT('Ctrl Pts',(-0.203156094897896,1.,-3.74449296982994));
#68514=CARTESIAN_POINT('',(-0.0760622897878238,0.,-4.19931119685982));
#68515=CARTESIAN_POINT('Ctrl Pts',(0.20305423869972,-1.,-3.74449849461127));
#68516=CARTESIAN_POINT('Ctrl Pts',(0.20305423869972,1.,-3.74449849461127));
#68517=CARTESIAN_POINT('Ctrl Pts',(0.203111767587923,-1.,-3.7444331934681));
#68518=CARTESIAN_POINT('Ctrl Pts',(0.203111767587923,1.,-3.7444331934681));
#68519=CARTESIAN_POINT('Ctrl Pts',(0.203218215748058,-1.,-3.7444688019622));
#68520=CARTESIAN_POINT('Ctrl Pts',(0.203218215748058,1.,-3.7444688019622));
#68521=CARTESIAN_POINT('Ctrl Pts',(0.203352057956297,-1.,-3.74502080927395));
#68522=CARTESIAN_POINT('Ctrl Pts',(0.203352057956297,1.,-3.74502080927395));
#68523=CARTESIAN_POINT('Ctrl Pts',(0.203478844530447,-1.,-3.7467547201908));
#68524=CARTESIAN_POINT('Ctrl Pts',(0.203478844530447,1.,-3.7467547201908));
#68525=CARTESIAN_POINT('Ctrl Pts',(0.203550035479166,-1.,-3.75054693397875));
#68526=CARTESIAN_POINT('Ctrl Pts',(0.203550035479166,1.,-3.75054693397875));
#68527=CARTESIAN_POINT('Ctrl Pts',(0.203530796848321,-1.,-3.75585118707734));
#68528=CARTESIAN_POINT('Ctrl Pts',(0.203530796848321,1.,-3.75585118707734));
#68529=CARTESIAN_POINT('Ctrl Pts',(0.203414634707478,-1.,-3.76242717936885));
#68530=CARTESIAN_POINT('Ctrl Pts',(0.203414634707478,1.,-3.76242717936885));
#68531=CARTESIAN_POINT('Ctrl Pts',(0.203192390045164,-1.,-3.7699207159487));
#68532=CARTESIAN_POINT('Ctrl Pts',(0.203192390045164,1.,-3.7699207159487));
#68533=CARTESIAN_POINT('Ctrl Pts',(0.202854729699081,-1.,-3.77793553476614));
#68534=CARTESIAN_POINT('Ctrl Pts',(0.202854729699081,1.,-3.77793553476614));
#68535=CARTESIAN_POINT('Ctrl Pts',(0.20239426051216,-1.,-3.78609175019242));
#68536=CARTESIAN_POINT('Ctrl Pts',(0.20239426051216,1.,-3.78609175019242));
#68537=CARTESIAN_POINT('Ctrl Pts',(0.201807533800837,-1.,-3.7940835418736));
#68538=CARTESIAN_POINT('Ctrl Pts',(0.201807533800837,1.,-3.7940835418736));
#68539=CARTESIAN_POINT('Ctrl Pts',(0.201097756307326,-1.,-3.80175247447337));
#68540=CARTESIAN_POINT('Ctrl Pts',(0.201097756307326,1.,-3.80175247447337));
#68541=CARTESIAN_POINT('Ctrl Pts',(0.200274679433364,-1.,-3.80909529318669));
#68542=CARTESIAN_POINT('Ctrl Pts',(0.200274679433364,1.,-3.80909529318669));
#68543=CARTESIAN_POINT('Ctrl Pts',(0.199351525297447,-1.,-3.81620203429815));
#68544=CARTESIAN_POINT('Ctrl Pts',(0.199351525297447,1.,-3.81620203429815));
#68545=CARTESIAN_POINT('Ctrl Pts',(0.198342616900486,-1.,-3.82321127349016));
#68546=CARTESIAN_POINT('Ctrl Pts',(0.198342616900486,1.,-3.82321127349016));
#68547=CARTESIAN_POINT('Ctrl Pts',(0.197260935827361,-1.,-3.83026221776456));
#68548=CARTESIAN_POINT('Ctrl Pts',(0.197260935827361,1.,-3.83026221776456));
#68549=CARTESIAN_POINT('Ctrl Pts',(0.196115198971859,-1.,-3.83743910616195));
#68550=CARTESIAN_POINT('Ctrl Pts',(0.196115198971859,1.,-3.83743910616195));
#68551=CARTESIAN_POINT('Ctrl Pts',(0.19490900946022,-1.,-3.84475203346977));
#68552=CARTESIAN_POINT('Ctrl Pts',(0.19490900946022,1.,-3.84475203346977));
#68553=CARTESIAN_POINT('Ctrl Pts',(0.193642806777723,-1.,-3.85216762263966));
#68554=CARTESIAN_POINT('Ctrl Pts',(0.193642806777723,1.,-3.85216762263966));
#68555=CARTESIAN_POINT('Ctrl Pts',(0.19231515304497,-1.,-3.85962774407633));
#68556=CARTESIAN_POINT('Ctrl Pts',(0.19231515304497,1.,-3.85962774407633));
#68557=CARTESIAN_POINT('Ctrl Pts',(0.19092419041862,-1.,-3.86707158624783));
#68558=CARTESIAN_POINT('Ctrl Pts',(0.19092419041862,1.,-3.86707158624783));
#68559=CARTESIAN_POINT('Ctrl Pts',(0.189469253358272,-1.,-3.87445976418412));
#68560=CARTESIAN_POINT('Ctrl Pts',(0.189469253358272,1.,-3.87445976418412));
#68561=CARTESIAN_POINT('Ctrl Pts',(0.187951632512685,-1.,-3.88178563496228));
#68562=CARTESIAN_POINT('Ctrl Pts',(0.187951632512685,1.,-3.88178563496228));
#68563=CARTESIAN_POINT('Ctrl Pts',(0.18637372498528,-1.,-3.88906196725848));
#68564=CARTESIAN_POINT('Ctrl Pts',(0.18637372498528,1.,-3.88906196725848));
#68565=CARTESIAN_POINT('Ctrl Pts',(0.184738537728043,-1.,-3.89631300742646));
#68566=CARTESIAN_POINT('Ctrl Pts',(0.184738537728043,1.,-3.89631300742646));
#68567=CARTESIAN_POINT('Ctrl Pts',(0.18304908199319,-1.,-3.90356488555132));
#68568=CARTESIAN_POINT('Ctrl Pts',(0.18304908199319,1.,-3.90356488555132));
#68569=CARTESIAN_POINT('Ctrl Pts',(0.181307740731785,-1.,-3.91083557557175));
#68570=CARTESIAN_POINT('Ctrl Pts',(0.181307740731785,1.,-3.91083557557175));
#68571=CARTESIAN_POINT('Ctrl Pts',(0.179515885822881,-1.,-3.91812876180926));
#68572=CARTESIAN_POINT('Ctrl Pts',(0.179515885822881,1.,-3.91812876180926));
#68573=CARTESIAN_POINT('Ctrl Pts',(0.177674246152317,-1.,-3.92543942697655));
#68574=CARTESIAN_POINT('Ctrl Pts',(0.177674246152317,1.,-3.92543942697655));
#68575=CARTESIAN_POINT('Ctrl Pts',(0.175783136893868,-1.,-3.93275726771042));
#68576=CARTESIAN_POINT('Ctrl Pts',(0.175783136893868,1.,-3.93275726771042));
#68577=CARTESIAN_POINT('Ctrl Pts',(0.173842734974609,-1.,-3.94007083096217));
#68578=CARTESIAN_POINT('Ctrl Pts',(0.173842734974609,1.,-3.94007083096217));
#68579=CARTESIAN_POINT('Ctrl Pts',(0.17185335536924,-1.,-3.94737164900868));
#68580=CARTESIAN_POINT('Ctrl Pts',(0.17185335536924,1.,-3.94737164900868));
#68581=CARTESIAN_POINT('Ctrl Pts',(0.169815666374139,-1.,-3.95465744665268));
#68582=CARTESIAN_POINT('Ctrl Pts',(0.169815666374139,1.,-3.95465744665268));
#68583=CARTESIAN_POINT('Ctrl Pts',(0.167730547023319,-1.,-3.96192990160296));
#68584=CARTESIAN_POINT('Ctrl Pts',(0.167730547023319,1.,-3.96192990160296));
#68585=CARTESIAN_POINT('Ctrl Pts',(0.165598992851102,-1.,-3.96919313621407));
#68586=CARTESIAN_POINT('Ctrl Pts',(0.165598992851102,1.,-3.96919313621407));
#68587=CARTESIAN_POINT('Ctrl Pts',(0.163422004609999,-1.,-3.97645194630943));
#68588=CARTESIAN_POINT('Ctrl Pts',(0.163422004609999,1.,-3.97645194630943));
#68589=CARTESIAN_POINT('Ctrl Pts',(0.161200482186084,-1.,-3.98371010319872));
#68590=CARTESIAN_POINT('Ctrl Pts',(0.161200482186084,1.,-3.98371010319872));
#68591=CARTESIAN_POINT('Ctrl Pts',(0.158935123982793,-1.,-3.99096873945878));
#68592=CARTESIAN_POINT('Ctrl Pts',(0.158935123982793,1.,-3.99096873945878));
#68593=CARTESIAN_POINT('Ctrl Pts',(0.156626481393734,-1.,-3.99822717425893));
#68594=CARTESIAN_POINT('Ctrl Pts',(0.156626481393734,1.,-3.99822717425893));
#68595=CARTESIAN_POINT('Ctrl Pts',(0.15427500487231,-1.,-4.00548360245319));
#68596=CARTESIAN_POINT('Ctrl Pts',(0.15427500487231,1.,-4.00548360245319));
#68597=CARTESIAN_POINT('Ctrl Pts',(0.15188109402291,-1.,-4.01273584234689));
#68598=CARTESIAN_POINT('Ctrl Pts',(0.15188109402291,1.,-4.01273584234689));
#68599=CARTESIAN_POINT('Ctrl Pts',(0.149445144968707,-1.,-4.01998203715564));
#68600=CARTESIAN_POINT('Ctrl Pts',(0.149445144968707,1.,-4.01998203715564));
#68601=CARTESIAN_POINT('Ctrl Pts',(0.146967602878994,-1.,-4.02722143146994));
#68602=CARTESIAN_POINT('Ctrl Pts',(0.146967602878994,1.,-4.02722143146994));
#68603=CARTESIAN_POINT('Ctrl Pts',(0.144448947038344,-1.,-4.03445411510333));
#68604=CARTESIAN_POINT('Ctrl Pts',(0.144448947038344,1.,-4.03445411510333));
#68605=CARTESIAN_POINT('Ctrl Pts',(0.1418896714855,-1.,-4.04168069633781));
#68606=CARTESIAN_POINT('Ctrl Pts',(0.1418896714855,1.,-4.04168069633781));
#68607=CARTESIAN_POINT('Ctrl Pts',(0.139290267180057,-1.,-4.04890199238036));
#68608=CARTESIAN_POINT('Ctrl Pts',(0.139290267180057,1.,-4.04890199238036));
#68609=CARTESIAN_POINT('Ctrl Pts',(0.136651205046119,-1.,-4.05611873400172));
#68610=CARTESIAN_POINT('Ctrl Pts',(0.136651205046119,1.,-4.05611873400172));
#68611=CARTESIAN_POINT('Ctrl Pts',(0.133972916144245,-1.,-4.06333121018596));
#68612=CARTESIAN_POINT('Ctrl Pts',(0.133972916144245,1.,-4.06333121018596));
#68613=CARTESIAN_POINT('Ctrl Pts',(0.13125579354894,-1.,-4.0705393152874));
#68614=CARTESIAN_POINT('Ctrl Pts',(0.13125579354894,1.,-4.0705393152874));
#68615=CARTESIAN_POINT('Ctrl Pts',(0.128500200484837,-1.,-4.07774270738954));
#68616=CARTESIAN_POINT('Ctrl Pts',(0.128500200484837,1.,-4.07774270738954));
#68617=CARTESIAN_POINT('Ctrl Pts',(0.12570647682254,-1.,-4.08494093372377));
#68618=CARTESIAN_POINT('Ctrl Pts',(0.12570647682254,1.,-4.08494093372377));
#68619=CARTESIAN_POINT('Ctrl Pts',(0.122874946249107,-1.,-4.09213355850756));
#68620=CARTESIAN_POINT('Ctrl Pts',(0.122874946249107,1.,-4.09213355850756));
#68621=CARTESIAN_POINT('Ctrl Pts',(0.120005924388124,-1.,-4.09932031767002));
#68622=CARTESIAN_POINT('Ctrl Pts',(0.120005924388124,1.,-4.09932031767002));
#68623=CARTESIAN_POINT('Ctrl Pts',(0.117099722731648,-1.,-4.10650113381833));
#68624=CARTESIAN_POINT('Ctrl Pts',(0.117099722731648,1.,-4.10650113381833));
#68625=CARTESIAN_POINT('Ctrl Pts',(0.114156649609545,-1.,-4.11367603924961));
#68626=CARTESIAN_POINT('Ctrl Pts',(0.114156649609545,1.,-4.11367603924961));
#68627=CARTESIAN_POINT('Ctrl Pts',(0.111177012683346,-1.,-4.1208451250225));
#68628=CARTESIAN_POINT('Ctrl Pts',(0.111177012683346,1.,-4.1208451250225));
#68629=CARTESIAN_POINT('Ctrl Pts',(0.108161120528369,-1.,-4.12800848371504));
#68630=CARTESIAN_POINT('Ctrl Pts',(0.108161120528369,1.,-4.12800848371504));
#68631=CARTESIAN_POINT('Ctrl Pts',(0.105109286538945,-1.,-4.13516614458895));
#68632=CARTESIAN_POINT('Ctrl Pts',(0.105109286538945,1.,-4.13516614458895));
#68633=CARTESIAN_POINT('Ctrl Pts',(0.102021826577584,-1.,-4.14231804939538));
#68634=CARTESIAN_POINT('Ctrl Pts',(0.102021826577584,1.,-4.14231804939538));
#68635=CARTESIAN_POINT('Ctrl Pts',(0.0988990478901223,-1.,-4.14946408918485));
#68636=CARTESIAN_POINT('Ctrl Pts',(0.0988990478901223,1.,-4.14946408918485));
#68637=CARTESIAN_POINT('Ctrl Pts',(0.0957412403298004,-1.,-4.15660412653577));
#68638=CARTESIAN_POINT('Ctrl Pts',(0.0957412403298004,1.,-4.15660412653577));
#68639=CARTESIAN_POINT('Ctrl Pts',(0.0925486672167528,-1.,-4.16373802265839));
#68640=CARTESIAN_POINT('Ctrl Pts',(0.0925486672167528,1.,-4.16373802265839));
#68641=CARTESIAN_POINT('Ctrl Pts',(0.0893215560848647,-1.,-4.17086566490794));
#68642=CARTESIAN_POINT('Ctrl Pts',(0.0893215560848647,1.,-4.17086566490794));
#68643=CARTESIAN_POINT('Ctrl Pts',(0.0860600915549394,-1.,-4.17798698668094));
#68644=CARTESIAN_POINT('Ctrl Pts',(0.0860600915549394,1.,-4.17798698668094));
#68645=CARTESIAN_POINT('Ctrl Pts',(0.0827644164385676,-1.,-4.18510195327123));
#68646=CARTESIAN_POINT('Ctrl Pts',(0.0827644164385676,1.,-4.18510195327123));
#68647=CARTESIAN_POINT('Ctrl Pts',(0.0801005887114317,-1.,-4.19078883320504));
#68648=CARTESIAN_POINT('Ctrl Pts',(0.0801005887114317,1.,-4.19078883320504));
#68649=CARTESIAN_POINT('Ctrl Pts',(0.0780873956242395,-1.,-4.19505112859416));
#68650=CARTESIAN_POINT('Ctrl Pts',(0.0780873956242395,1.,-4.19505112859416));
#68651=CARTESIAN_POINT('Ctrl Pts',(0.0767384596141462,-1.,-4.1978913862118));
#68652=CARTESIAN_POINT('Ctrl Pts',(0.0767384596141462,1.,-4.1978913862118));
#68653=CARTESIAN_POINT('Ctrl Pts',(0.0760622897878244,-1.,-4.19931119685982));
#68654=CARTESIAN_POINT('Ctrl Pts',(0.0760622897878244,1.,-4.19931119685982));
#68655=CARTESIAN_POINT('',(0.203156094896102,1.,-3.74449296983004));
#68656=CARTESIAN_POINT('Ctrl Pts',(0.2031560948961,-1.,-3.74449296983004));
#68657=CARTESIAN_POINT('Ctrl Pts',(0.2031560948961,-0.666666666666667,-3.74449296983004));
#68658=CARTESIAN_POINT('Ctrl Pts',(0.2031560948961,-0.333333333333333,-3.74449296983004));
#68659=CARTESIAN_POINT('Ctrl Pts',(0.2031560948961,0.333333333333333,-3.74449296983004));
#68660=CARTESIAN_POINT('Ctrl Pts',(0.203156094896101,0.666666666666667,
-3.74449296983004));
#68661=CARTESIAN_POINT('Ctrl Pts',(0.203156094896101,1.,-3.74449296983004));
#68662=CARTESIAN_POINT('',(0.0760622897878244,1.,-4.19931119685982));
#68663=CARTESIAN_POINT('',(0.0760622897878244,0.,-4.19931119685982));
#68664=CARTESIAN_POINT('Ctrl Pts',(0.203156094896101,1.,-3.74449296983004));
#68665=CARTESIAN_POINT('Ctrl Pts',(0.203188003946657,1.,-3.74453008995093));
#68666=CARTESIAN_POINT('Ctrl Pts',(0.203266610110531,1.,-3.74471097893845));
#68667=CARTESIAN_POINT('Ctrl Pts',(0.203375226874121,1.,-3.74535749969115));
#68668=CARTESIAN_POINT('Ctrl Pts',(0.203484186269415,1.,-3.74703926501752));
#68669=CARTESIAN_POINT('Ctrl Pts',(0.203550035479166,1.,-3.75054693397875));
#68670=CARTESIAN_POINT('Ctrl Pts',(0.203530796848321,1.,-3.75585118707734));
#68671=CARTESIAN_POINT('Ctrl Pts',(0.203414634707478,1.,-3.76242717936885));
#68672=CARTESIAN_POINT('Ctrl Pts',(0.203192390045164,1.,-3.7699207159487));
#68673=CARTESIAN_POINT('Ctrl Pts',(0.202854729699081,1.,-3.77793553476614));
#68674=CARTESIAN_POINT('Ctrl Pts',(0.20239426051216,1.,-3.78609175019242));
#68675=CARTESIAN_POINT('Ctrl Pts',(0.201807533800837,1.,-3.7940835418736));
#68676=CARTESIAN_POINT('Ctrl Pts',(0.201097756307326,1.,-3.80175247447337));
#68677=CARTESIAN_POINT('Ctrl Pts',(0.200274679433364,1.,-3.80909529318669));
#68678=CARTESIAN_POINT('Ctrl Pts',(0.199351525297447,1.,-3.81620203429815));
#68679=CARTESIAN_POINT('Ctrl Pts',(0.198342616900486,1.,-3.82321127349016));
#68680=CARTESIAN_POINT('Ctrl Pts',(0.197260935827361,1.,-3.83026221776456));
#68681=CARTESIAN_POINT('Ctrl Pts',(0.196115198971859,1.,-3.83743910616195));
#68682=CARTESIAN_POINT('Ctrl Pts',(0.19490900946022,1.,-3.84475203346977));
#68683=CARTESIAN_POINT('Ctrl Pts',(0.193642806777723,1.,-3.85216762263966));
#68684=CARTESIAN_POINT('Ctrl Pts',(0.19231515304497,1.,-3.85962774407633));
#68685=CARTESIAN_POINT('Ctrl Pts',(0.19092419041862,1.,-3.86707158624783));
#68686=CARTESIAN_POINT('Ctrl Pts',(0.189469253358272,1.,-3.87445976418412));
#68687=CARTESIAN_POINT('Ctrl Pts',(0.187951632512685,1.,-3.88178563496228));
#68688=CARTESIAN_POINT('Ctrl Pts',(0.18637372498528,1.,-3.88906196725848));
#68689=CARTESIAN_POINT('Ctrl Pts',(0.184738537728043,1.,-3.89631300742646));
#68690=CARTESIAN_POINT('Ctrl Pts',(0.18304908199319,1.,-3.90356488555132));
#68691=CARTESIAN_POINT('Ctrl Pts',(0.181307740731785,1.,-3.91083557557175));
#68692=CARTESIAN_POINT('Ctrl Pts',(0.179515885822881,1.,-3.91812876180926));
#68693=CARTESIAN_POINT('Ctrl Pts',(0.177674246152317,1.,-3.92543942697655));
#68694=CARTESIAN_POINT('Ctrl Pts',(0.175783136893868,1.,-3.93275726771042));
#68695=CARTESIAN_POINT('Ctrl Pts',(0.173842734974609,1.,-3.94007083096217));
#68696=CARTESIAN_POINT('Ctrl Pts',(0.17185335536924,1.,-3.94737164900868));
#68697=CARTESIAN_POINT('Ctrl Pts',(0.169815666374139,1.,-3.95465744665268));
#68698=CARTESIAN_POINT('Ctrl Pts',(0.167730547023319,1.,-3.96192990160296));
#68699=CARTESIAN_POINT('Ctrl Pts',(0.165598992851102,1.,-3.96919313621407));
#68700=CARTESIAN_POINT('Ctrl Pts',(0.163422004609999,1.,-3.97645194630943));
#68701=CARTESIAN_POINT('Ctrl Pts',(0.161200482186084,1.,-3.98371010319872));
#68702=CARTESIAN_POINT('Ctrl Pts',(0.158935123982793,1.,-3.99096873945878));
#68703=CARTESIAN_POINT('Ctrl Pts',(0.156626481393734,1.,-3.99822717425893));
#68704=CARTESIAN_POINT('Ctrl Pts',(0.15427500487231,1.,-4.00548360245319));
#68705=CARTESIAN_POINT('Ctrl Pts',(0.15188109402291,1.,-4.01273584234689));
#68706=CARTESIAN_POINT('Ctrl Pts',(0.149445144968707,1.,-4.01998203715564));
#68707=CARTESIAN_POINT('Ctrl Pts',(0.146967602878994,1.,-4.02722143146994));
#68708=CARTESIAN_POINT('Ctrl Pts',(0.144448947038344,1.,-4.03445411510333));
#68709=CARTESIAN_POINT('Ctrl Pts',(0.1418896714855,1.,-4.04168069633781));
#68710=CARTESIAN_POINT('Ctrl Pts',(0.139290267180057,1.,-4.04890199238036));
#68711=CARTESIAN_POINT('Ctrl Pts',(0.136651205046119,1.,-4.05611873400172));
#68712=CARTESIAN_POINT('Ctrl Pts',(0.133972916144245,1.,-4.06333121018596));
#68713=CARTESIAN_POINT('Ctrl Pts',(0.13125579354894,1.,-4.0705393152874));
#68714=CARTESIAN_POINT('Ctrl Pts',(0.128500200484837,1.,-4.07774270738954));
#68715=CARTESIAN_POINT('Ctrl Pts',(0.12570647682254,1.,-4.08494093372377));
#68716=CARTESIAN_POINT('Ctrl Pts',(0.122874946249107,1.,-4.09213355850756));
#68717=CARTESIAN_POINT('Ctrl Pts',(0.120005924388124,1.,-4.09932031767002));
#68718=CARTESIAN_POINT('Ctrl Pts',(0.117099722731648,1.,-4.10650113381833));
#68719=CARTESIAN_POINT('Ctrl Pts',(0.114156649609545,1.,-4.11367603924961));
#68720=CARTESIAN_POINT('Ctrl Pts',(0.111177012683346,1.,-4.1208451250225));
#68721=CARTESIAN_POINT('Ctrl Pts',(0.108161120528369,1.,-4.12800848371504));
#68722=CARTESIAN_POINT('Ctrl Pts',(0.105109286538945,1.,-4.13516614458895));
#68723=CARTESIAN_POINT('Ctrl Pts',(0.102021826577584,1.,-4.14231804939538));
#68724=CARTESIAN_POINT('Ctrl Pts',(0.0988990478901223,1.,-4.14946408918485));
#68725=CARTESIAN_POINT('Ctrl Pts',(0.0957412403298004,1.,-4.15660412653577));
#68726=CARTESIAN_POINT('Ctrl Pts',(0.0925486672167528,1.,-4.16373802265839));
#68727=CARTESIAN_POINT('Ctrl Pts',(0.0893215560848647,1.,-4.17086566490794));
#68728=CARTESIAN_POINT('Ctrl Pts',(0.0860600915549394,1.,-4.17798698668094));
#68729=CARTESIAN_POINT('Ctrl Pts',(0.0827644164385676,1.,-4.18510195327123));
#68730=CARTESIAN_POINT('Ctrl Pts',(0.0801005887114317,1.,-4.19078883320504));
#68731=CARTESIAN_POINT('Ctrl Pts',(0.0780873956242395,1.,-4.19505112859416));
#68732=CARTESIAN_POINT('Ctrl Pts',(0.0767384596141462,1.,-4.1978913862118));
#68733=CARTESIAN_POINT('Ctrl Pts',(0.0760622897878244,1.,-4.19931119685982));
#68734=CARTESIAN_POINT('Origin',(0.0760622897878244,0.,-4.19931119685982));
#68735=CARTESIAN_POINT('',(-0.0760622897878238,1.,-4.19931119685982));
#68736=CARTESIAN_POINT('Origin',(0.,0.,0.));
#68737=CARTESIAN_POINT('',(0.385112848330761,1.,-3.73017266276651));
#68738=CARTESIAN_POINT('Origin',(0.,1.,0.));
#68739=CARTESIAN_POINT('Ctrl Pts',(0.385112848330762,1.,-3.73017266276651));
#68740=CARTESIAN_POINT('Ctrl Pts',(0.385112848330762,0.666666666666667,
-3.73017266276651));
#68741=CARTESIAN_POINT('Ctrl Pts',(0.385112848330762,0.333333333333333,
-3.73017266276651));
#68742=CARTESIAN_POINT('Ctrl Pts',(0.385112848330762,-0.333333333333333,
-3.73017266276651));
#68743=CARTESIAN_POINT('Ctrl Pts',(0.385112848330762,-0.666666666666667,
-3.73017266276651));
#68744=CARTESIAN_POINT('Ctrl Pts',(0.385112848330762,-1.,-3.73017266276651));
#68745=CARTESIAN_POINT('Ctrl Pts',(0.581791163835815,-1.,-4.15950947128175));
#68746=CARTESIAN_POINT('Ctrl Pts',(0.581791163835815,1.,-4.15950947128175));
#68747=CARTESIAN_POINT('Ctrl Pts',(0.580901211463535,-1.,-4.1582129171283));
#68748=CARTESIAN_POINT('Ctrl Pts',(0.580901211463535,1.,-4.1582129171283));
#68749=CARTESIAN_POINT('Ctrl Pts',(0.579124568914235,-1.,-4.15561864788576));
#68750=CARTESIAN_POINT('Ctrl Pts',(0.579124568914235,1.,-4.15561864788576));
#68751=CARTESIAN_POINT('Ctrl Pts',(0.576469391676688,-1.,-4.151723761217));
#68752=CARTESIAN_POINT('Ctrl Pts',(0.576469391676688,1.,-4.151723761217));
#68753=CARTESIAN_POINT('Ctrl Pts',(0.572948736069522,-1.,-4.14652361068081));
#68754=CARTESIAN_POINT('Ctrl Pts',(0.572948736069522,1.,-4.14652361068081));
#68755=CARTESIAN_POINT('Ctrl Pts',(0.568580610189774,-1.,-4.14001179830547));
#68756=CARTESIAN_POINT('Ctrl Pts',(0.568580610189774,1.,-4.14001179830547));
#68757=CARTESIAN_POINT('Ctrl Pts',(0.564245279537148,-1.,-4.13348835727104));
#68758=CARTESIAN_POINT('Ctrl Pts',(0.564245279537148,1.,-4.13348835727104));
#68759=CARTESIAN_POINT('Ctrl Pts',(0.559942890594773,-1.,-4.12695329951961));
#68760=CARTESIAN_POINT('Ctrl Pts',(0.559942890594773,1.,-4.12695329951961));
#68761=CARTESIAN_POINT('Ctrl Pts',(0.555673636129977,-1.,-4.12040666195664));
#68762=CARTESIAN_POINT('Ctrl Pts',(0.555673636129977,1.,-4.12040666195664));
#68763=CARTESIAN_POINT('Ctrl Pts',(0.551437758497032,-1.,-4.11384852024721));
#68764=CARTESIAN_POINT('Ctrl Pts',(0.551437758497032,1.,-4.11384852024721));
#68765=CARTESIAN_POINT('Ctrl Pts',(0.547235539485636,-1.,-4.10727897027977));
#68766=CARTESIAN_POINT('Ctrl Pts',(0.547235539485636,1.,-4.10727897027977));
#68767=CARTESIAN_POINT('Ctrl Pts',(0.543067286877757,-1.,-4.10069810243979));
#68768=CARTESIAN_POINT('Ctrl Pts',(0.543067286877757,1.,-4.10069810243979));
#68769=CARTESIAN_POINT('Ctrl Pts',(0.538933321179755,-1.,-4.09410597627));
#68770=CARTESIAN_POINT('Ctrl Pts',(0.538933321179755,1.,-4.09410597627));
#68771=CARTESIAN_POINT('Ctrl Pts',(0.534833963477273,-1.,-4.08750259988885));
#68772=CARTESIAN_POINT('Ctrl Pts',(0.534833963477273,1.,-4.08750259988885));
#68773=CARTESIAN_POINT('Ctrl Pts',(0.53076951872857,-1.,-4.08088789536836));
#68774=CARTESIAN_POINT('Ctrl Pts',(0.53076951872857,1.,-4.08088789536836));
#68775=CARTESIAN_POINT('Ctrl Pts',(0.526740277227498,-1.,-4.07426172299847));
#68776=CARTESIAN_POINT('Ctrl Pts',(0.526740277227498,1.,-4.07426172299847));
#68777=CARTESIAN_POINT('Ctrl Pts',(0.522746528603107,-1.,-4.06762394471314));
#68778=CARTESIAN_POINT('Ctrl Pts',(0.522746528603107,1.,-4.06762394471314));
#68779=CARTESIAN_POINT('Ctrl Pts',(0.518788572336923,-1.,-4.06097448038013));
#68780=CARTESIAN_POINT('Ctrl Pts',(0.518788572336923,1.,-4.06097448038013));
#68781=CARTESIAN_POINT('Ctrl Pts',(0.514866728193016,-1.,-4.05431335771199));
#68782=CARTESIAN_POINT('Ctrl Pts',(0.514866728193016,1.,-4.05431335771199));
#68783=CARTESIAN_POINT('Ctrl Pts',(0.51098134921897,-1.,-4.04764078815447));
#68784=CARTESIAN_POINT('Ctrl Pts',(0.51098134921897,1.,-4.04764078815447));
#68785=CARTESIAN_POINT('Ctrl Pts',(0.507132823288136,-1.,-4.04095715148915));
#68786=CARTESIAN_POINT('Ctrl Pts',(0.507132823288136,1.,-4.04095715148915));
#68787=CARTESIAN_POINT('Ctrl Pts',(0.503321556915346,-1.,-4.03426284174272));
#68788=CARTESIAN_POINT('Ctrl Pts',(0.503321556915346,1.,-4.03426284174272));
#68789=CARTESIAN_POINT('Ctrl Pts',(0.499547962340821,-1.,-4.02755813980101));
#68790=CARTESIAN_POINT('Ctrl Pts',(0.499547962340821,1.,-4.02755813980101));
#68791=CARTESIAN_POINT('Ctrl Pts',(0.495812444326251,-1.,-4.02084308851832));
#68792=CARTESIAN_POINT('Ctrl Pts',(0.495812444326251,1.,-4.02084308851832));
#68793=CARTESIAN_POINT('Ctrl Pts',(0.492115383418018,-1.,-4.01411733503546));
#68794=CARTESIAN_POINT('Ctrl Pts',(0.492115383418018,1.,-4.01411733503546));
#68795=CARTESIAN_POINT('Ctrl Pts',(0.488457130424633,-1.,-4.0073800839099));
#68796=CARTESIAN_POINT('Ctrl Pts',(0.488457130424633,1.,-4.0073800839099));
#68797=CARTESIAN_POINT('Ctrl Pts',(0.484838042421834,-1.,-4.00063045119288));
#68798=CARTESIAN_POINT('Ctrl Pts',(0.484838042421834,1.,-4.00063045119288));
#68799=CARTESIAN_POINT('Ctrl Pts',(0.481258512209675,-1.,-3.99386775880679));
#68800=CARTESIAN_POINT('Ctrl Pts',(0.481258512209675,1.,-3.99386775880679));
#68801=CARTESIAN_POINT('Ctrl Pts',(0.477718999122027,-1.,-3.98709184306738));
#68802=CARTESIAN_POINT('Ctrl Pts',(0.477718999122027,1.,-3.98709184306738));
#68803=CARTESIAN_POINT('Ctrl Pts',(0.474220061019509,-1.,-3.98030338044409));
#68804=CARTESIAN_POINT('Ctrl Pts',(0.474220061019509,1.,-3.98030338044409));
#68805=CARTESIAN_POINT('Ctrl Pts',(0.470762379613439,-1.,-3.97350414289392));
#68806=CARTESIAN_POINT('Ctrl Pts',(0.470762379613439,1.,-3.97350414289392));
#68807=CARTESIAN_POINT('Ctrl Pts',(0.467346690880643,-1.,-3.9666962227393));
#68808=CARTESIAN_POINT('Ctrl Pts',(0.467346690880643,1.,-3.9666962227393));
#68809=CARTESIAN_POINT('Ctrl Pts',(0.463973722115733,-1.,-3.95988133243538));
#68810=CARTESIAN_POINT('Ctrl Pts',(0.463973722115733,1.,-3.95988133243538));
#68811=CARTESIAN_POINT('Ctrl Pts',(0.460644124429121,-1.,-3.95306005817364));
#68812=CARTESIAN_POINT('Ctrl Pts',(0.460644124429121,1.,-3.95306005817364));
#68813=CARTESIAN_POINT('Ctrl Pts',(0.457358410451682,-1.,-3.94623117206678));
#68814=CARTESIAN_POINT('Ctrl Pts',(0.457358410451682,1.,-3.94623117206678));
#68815=CARTESIAN_POINT('Ctrl Pts',(0.454116879027584,-1.,-3.93939080846298));
#68816=CARTESIAN_POINT('Ctrl Pts',(0.454116879027584,1.,-3.93939080846298));
#68817=CARTESIAN_POINT('Ctrl Pts',(0.450919768356348,-1.,-3.93253407403123));
#68818=CARTESIAN_POINT('Ctrl Pts',(0.450919768356348,1.,-3.93253407403123));
#68819=CARTESIAN_POINT('Ctrl Pts',(0.447767416837292,-1.,-3.92565674143416));
#68820=CARTESIAN_POINT('Ctrl Pts',(0.447767416837292,1.,-3.92565674143416));
#68821=CARTESIAN_POINT('Ctrl Pts',(0.44466043023059,-1.,-3.91875701610719));
#68822=CARTESIAN_POINT('Ctrl Pts',(0.44466043023059,1.,-3.91875701610719));
#68823=CARTESIAN_POINT('Ctrl Pts',(0.441599824524054,-1.,-3.91183704069153));
#68824=CARTESIAN_POINT('Ctrl Pts',(0.441599824524054,1.,-3.91183704069153));
#68825=CARTESIAN_POINT('Ctrl Pts',(0.438587235458249,-1.,-3.90490512938563));
#68826=CARTESIAN_POINT('Ctrl Pts',(0.438587235458249,1.,-3.90490512938563));
#68827=CARTESIAN_POINT('Ctrl Pts',(0.435624629433527,-1.,-3.89797256655462));
#68828=CARTESIAN_POINT('Ctrl Pts',(0.435624629433527,1.,-3.89797256655462));
#68829=CARTESIAN_POINT('Ctrl Pts',(0.432713929544458,-1.,-3.89104947940611));
#68830=CARTESIAN_POINT('Ctrl Pts',(0.432713929544458,1.,-3.89104947940611));
#68831=CARTESIAN_POINT('Ctrl Pts',(0.429856640579741,-1.,-3.88414070943341));
#68832=CARTESIAN_POINT('Ctrl Pts',(0.429856640579741,1.,-3.88414070943341));
#68833=CARTESIAN_POINT('Ctrl Pts',(0.427053541173457,-1.,-3.87724240306597));
#68834=CARTESIAN_POINT('Ctrl Pts',(0.427053541173457,1.,-3.87724240306597));
#68835=CARTESIAN_POINT('Ctrl Pts',(0.42430417319511,-1.,-3.87033643487851));
#68836=CARTESIAN_POINT('Ctrl Pts',(0.42430417319511,1.,-3.87033643487851));
#68837=CARTESIAN_POINT('Ctrl Pts',(0.421607423177534,-1.,-3.86339652542709));
#68838=CARTESIAN_POINT('Ctrl Pts',(0.421607423177534,1.,-3.86339652542709));
#68839=CARTESIAN_POINT('Ctrl Pts',(0.418962468086773,-1.,-3.85639825647996));
#68840=CARTESIAN_POINT('Ctrl Pts',(0.418962468086773,1.,-3.85639825647996));
#68841=CARTESIAN_POINT('Ctrl Pts',(0.416369678052906,-1.,-3.84932864157497));
#68842=CARTESIAN_POINT('Ctrl Pts',(0.416369678052906,1.,-3.84932864157497));
#68843=CARTESIAN_POINT('Ctrl Pts',(0.413831367016748,-1.,-3.84219403994762));
#68844=CARTESIAN_POINT('Ctrl Pts',(0.413831367016748,1.,-3.84219403994762));
#68845=CARTESIAN_POINT('Ctrl Pts',(0.411353038798518,-1.,-3.83503345578698));
#68846=CARTESIAN_POINT('Ctrl Pts',(0.411353038798518,1.,-3.83503345578698));
#68847=CARTESIAN_POINT('Ctrl Pts',(0.408942371447459,-1.,-3.82790724256471));
#68848=CARTESIAN_POINT('Ctrl Pts',(0.408942371447459,1.,-3.82790724256471));
#68849=CARTESIAN_POINT('Ctrl Pts',(0.406607038258985,-1.,-3.8208730391381));
#68850=CARTESIAN_POINT('Ctrl Pts',(0.406607038258985,1.,-3.8208730391381));
#68851=CARTESIAN_POINT('Ctrl Pts',(0.404352694628273,-1.,-3.81396374287793));
#68852=CARTESIAN_POINT('Ctrl Pts',(0.404352694628273,1.,-3.81396374287793));
#68853=CARTESIAN_POINT('Ctrl Pts',(0.402181320148435,-1.,-3.80716881962728));
#68854=CARTESIAN_POINT('Ctrl Pts',(0.402181320148435,1.,-3.80716881962728));
#68855=CARTESIAN_POINT('Ctrl Pts',(0.4000883465046,-1.,-3.80040370384546));
#68856=CARTESIAN_POINT('Ctrl Pts',(0.4000883465046,1.,-3.80040370384546));
#68857=CARTESIAN_POINT('Ctrl Pts',(0.398064818683969,-1.,-3.7935288716329));
#68858=CARTESIAN_POINT('Ctrl Pts',(0.398064818683969,1.,-3.7935288716329));
#68859=CARTESIAN_POINT('Ctrl Pts',(0.39610320533484,-1.,-3.78640521279313));
#68860=CARTESIAN_POINT('Ctrl Pts',(0.39610320533484,1.,-3.78640521279313));
#68861=CARTESIAN_POINT('Ctrl Pts',(0.394202481011499,-1.,-3.77894173114283));
#68862=CARTESIAN_POINT('Ctrl Pts',(0.394202481011499,1.,-3.77894173114283));
#68863=CARTESIAN_POINT('Ctrl Pts',(0.392372786223432,-1.,-3.77114011595967));
#68864=CARTESIAN_POINT('Ctrl Pts',(0.392372786223432,1.,-3.77114011595967));
#68865=CARTESIAN_POINT('Ctrl Pts',(0.390642072979559,-1.,-3.76315635033257));
#68866=CARTESIAN_POINT('Ctrl Pts',(0.390642072979559,1.,-3.76315635033257));
#68867=CARTESIAN_POINT('Ctrl Pts',(0.389054775898701,-1.,-3.75529302895152));
#68868=CARTESIAN_POINT('Ctrl Pts',(0.389054775898701,1.,-3.75529302895152));
#68869=CARTESIAN_POINT('Ctrl Pts',(0.387663020050836,-1.,-3.74792651696654));
#68870=CARTESIAN_POINT('Ctrl Pts',(0.387663020050836,1.,-3.74792651696654));
#68871=CARTESIAN_POINT('Ctrl Pts',(0.386519576222251,-1.,-3.74144965781276));
#68872=CARTESIAN_POINT('Ctrl Pts',(0.386519576222251,1.,-3.74144965781276));
#68873=CARTESIAN_POINT('Ctrl Pts',(0.385670806454565,-1.,-3.73621371845318));
#68874=CARTESIAN_POINT('Ctrl Pts',(0.385670806454565,1.,-3.73621371845318));
#68875=CARTESIAN_POINT('Ctrl Pts',(0.385147887988951,-1.,-3.73245705638843));
#68876=CARTESIAN_POINT('Ctrl Pts',(0.385147887988951,1.,-3.73245705638843));
#68877=CARTESIAN_POINT('Ctrl Pts',(0.385001870183213,-1.,-3.73072465900175));
#68878=CARTESIAN_POINT('Ctrl Pts',(0.385001870183213,1.,-3.73072465900175));
#68879=CARTESIAN_POINT('Ctrl Pts',(0.385047711603462,-1.,-3.73015851028356));
#68880=CARTESIAN_POINT('Ctrl Pts',(0.385047711603462,1.,-3.73015851028356));
#68881=CARTESIAN_POINT('Ctrl Pts',(0.385147278814642,-1.,-3.73010668803042));
#68882=CARTESIAN_POINT('Ctrl Pts',(0.385147278814642,1.,-3.73010668803042));
#68883=CARTESIAN_POINT('Ctrl Pts',(0.385214314776329,-1.,-3.73016218570874));
#68884=CARTESIAN_POINT('Ctrl Pts',(0.385214314776329,1.,-3.73016218570874));
#68885=CARTESIAN_POINT('',(0.581791163835815,1.,-4.15950947128175));
#68886=CARTESIAN_POINT('Ctrl Pts',(0.581791163835815,1.,-4.15950947128175));
#68887=CARTESIAN_POINT('Ctrl Pts',(0.580901211463535,1.,-4.1582129171283));
#68888=CARTESIAN_POINT('Ctrl Pts',(0.579124568914235,1.,-4.15561864788576));
#68889=CARTESIAN_POINT('Ctrl Pts',(0.576469391676688,1.,-4.151723761217));
#68890=CARTESIAN_POINT('Ctrl Pts',(0.572948736069522,1.,-4.14652361068081));
#68891=CARTESIAN_POINT('Ctrl Pts',(0.568580610189774,1.,-4.14001179830547));
#68892=CARTESIAN_POINT('Ctrl Pts',(0.564245279537148,1.,-4.13348835727104));
#68893=CARTESIAN_POINT('Ctrl Pts',(0.559942890594773,1.,-4.12695329951961));
#68894=CARTESIAN_POINT('Ctrl Pts',(0.555673636129977,1.,-4.12040666195664));
#68895=CARTESIAN_POINT('Ctrl Pts',(0.551437758497032,1.,-4.11384852024721));
#68896=CARTESIAN_POINT('Ctrl Pts',(0.547235539485636,1.,-4.10727897027977));
#68897=CARTESIAN_POINT('Ctrl Pts',(0.543067286877757,1.,-4.10069810243979));
#68898=CARTESIAN_POINT('Ctrl Pts',(0.538933321179755,1.,-4.09410597627));
#68899=CARTESIAN_POINT('Ctrl Pts',(0.534833963477273,1.,-4.08750259988885));
#68900=CARTESIAN_POINT('Ctrl Pts',(0.53076951872857,1.,-4.08088789536836));
#68901=CARTESIAN_POINT('Ctrl Pts',(0.526740277227498,1.,-4.07426172299847));
#68902=CARTESIAN_POINT('Ctrl Pts',(0.522746528603107,1.,-4.06762394471314));
#68903=CARTESIAN_POINT('Ctrl Pts',(0.518788572336923,1.,-4.06097448038013));
#68904=CARTESIAN_POINT('Ctrl Pts',(0.514866728193016,1.,-4.05431335771199));
#68905=CARTESIAN_POINT('Ctrl Pts',(0.51098134921897,1.,-4.04764078815447));
#68906=CARTESIAN_POINT('Ctrl Pts',(0.507132823288136,1.,-4.04095715148915));
#68907=CARTESIAN_POINT('Ctrl Pts',(0.503321556915346,1.,-4.03426284174272));
#68908=CARTESIAN_POINT('Ctrl Pts',(0.499547962340821,1.,-4.02755813980101));
#68909=CARTESIAN_POINT('Ctrl Pts',(0.495812444326251,1.,-4.02084308851832));
#68910=CARTESIAN_POINT('Ctrl Pts',(0.492115383418018,1.,-4.01411733503546));
#68911=CARTESIAN_POINT('Ctrl Pts',(0.488457130424633,1.,-4.0073800839099));
#68912=CARTESIAN_POINT('Ctrl Pts',(0.484838042421834,1.,-4.00063045119288));
#68913=CARTESIAN_POINT('Ctrl Pts',(0.481258512209675,1.,-3.99386775880679));
#68914=CARTESIAN_POINT('Ctrl Pts',(0.477718999122027,1.,-3.98709184306738));
#68915=CARTESIAN_POINT('Ctrl Pts',(0.474220061019509,1.,-3.98030338044409));
#68916=CARTESIAN_POINT('Ctrl Pts',(0.470762379613439,1.,-3.97350414289392));
#68917=CARTESIAN_POINT('Ctrl Pts',(0.467346690880643,1.,-3.9666962227393));
#68918=CARTESIAN_POINT('Ctrl Pts',(0.463973722115733,1.,-3.95988133243538));
#68919=CARTESIAN_POINT('Ctrl Pts',(0.460644124429121,1.,-3.95306005817364));
#68920=CARTESIAN_POINT('Ctrl Pts',(0.457358410451682,1.,-3.94623117206678));
#68921=CARTESIAN_POINT('Ctrl Pts',(0.454116879027584,1.,-3.93939080846298));
#68922=CARTESIAN_POINT('Ctrl Pts',(0.450919768356348,1.,-3.93253407403123));
#68923=CARTESIAN_POINT('Ctrl Pts',(0.447767416837292,1.,-3.92565674143416));
#68924=CARTESIAN_POINT('Ctrl Pts',(0.44466043023059,1.,-3.91875701610719));
#68925=CARTESIAN_POINT('Ctrl Pts',(0.441599824524054,1.,-3.91183704069153));
#68926=CARTESIAN_POINT('Ctrl Pts',(0.438587235458249,1.,-3.90490512938563));
#68927=CARTESIAN_POINT('Ctrl Pts',(0.435624629433527,1.,-3.89797256655462));
#68928=CARTESIAN_POINT('Ctrl Pts',(0.432713929544458,1.,-3.89104947940611));
#68929=CARTESIAN_POINT('Ctrl Pts',(0.429856640579741,1.,-3.88414070943341));
#68930=CARTESIAN_POINT('Ctrl Pts',(0.427053541173457,1.,-3.87724240306597));
#68931=CARTESIAN_POINT('Ctrl Pts',(0.42430417319511,1.,-3.87033643487851));
#68932=CARTESIAN_POINT('Ctrl Pts',(0.421607423177534,1.,-3.86339652542709));
#68933=CARTESIAN_POINT('Ctrl Pts',(0.418962468086773,1.,-3.85639825647996));
#68934=CARTESIAN_POINT('Ctrl Pts',(0.416369678052906,1.,-3.84932864157497));
#68935=CARTESIAN_POINT('Ctrl Pts',(0.413831367016748,1.,-3.84219403994762));
#68936=CARTESIAN_POINT('Ctrl Pts',(0.411353038798518,1.,-3.83503345578698));
#68937=CARTESIAN_POINT('Ctrl Pts',(0.408942371447459,1.,-3.82790724256471));
#68938=CARTESIAN_POINT('Ctrl Pts',(0.406607038258985,1.,-3.8208730391381));
#68939=CARTESIAN_POINT('Ctrl Pts',(0.404352694628273,1.,-3.81396374287793));
#68940=CARTESIAN_POINT('Ctrl Pts',(0.402181320148435,1.,-3.80716881962728));
#68941=CARTESIAN_POINT('Ctrl Pts',(0.4000883465046,1.,-3.80040370384546));
#68942=CARTESIAN_POINT('Ctrl Pts',(0.398064818683969,1.,-3.7935288716329));
#68943=CARTESIAN_POINT('Ctrl Pts',(0.39610320533484,1.,-3.78640521279313));
#68944=CARTESIAN_POINT('Ctrl Pts',(0.394202481011499,1.,-3.77894173114283));
#68945=CARTESIAN_POINT('Ctrl Pts',(0.392372786223432,1.,-3.77114011595967));
#68946=CARTESIAN_POINT('Ctrl Pts',(0.390642072979559,1.,-3.76315635033257));
#68947=CARTESIAN_POINT('Ctrl Pts',(0.389054775898701,1.,-3.75529302895152));
#68948=CARTESIAN_POINT('Ctrl Pts',(0.387663020050836,1.,-3.74792651696654));
#68949=CARTESIAN_POINT('Ctrl Pts',(0.386519576222251,1.,-3.74144965781276));
#68950=CARTESIAN_POINT('Ctrl Pts',(0.385670806454565,1.,-3.73621371845318));
#68951=CARTESIAN_POINT('Ctrl Pts',(0.385187124634206,1.,-3.73273893363406));
#68952=CARTESIAN_POINT('Ctrl Pts',(0.385031656499163,1.,-3.73106082862548));
#68953=CARTESIAN_POINT('Ctrl Pts',(0.385037797881504,1.,-3.73040527621055));
#68954=CARTESIAN_POINT('Ctrl Pts',(0.385087139000374,1.,-3.73021431755274));
#68955=CARTESIAN_POINT('Ctrl Pts',(0.385112848330761,1.,-3.73017266276651));
#68956=CARTESIAN_POINT('',(0.581791163835815,0.,-4.15950947128175));
#68957=CARTESIAN_POINT('Ctrl Pts',(0.786322922920599,-1.,-3.66663282329846));
#68958=CARTESIAN_POINT('Ctrl Pts',(0.786322922920599,1.,-3.66663282329846));
#68959=CARTESIAN_POINT('Ctrl Pts',(0.786369528183326,-1.,-3.66655932661986));
#68960=CARTESIAN_POINT('Ctrl Pts',(0.786369528183326,1.,-3.66655932661986));
#68961=CARTESIAN_POINT('Ctrl Pts',(0.786480236185696,-1.,-3.66657784455334));
#68962=CARTESIAN_POINT('Ctrl Pts',(0.786480236185696,1.,-3.66657784455334));
#68963=CARTESIAN_POINT('Ctrl Pts',(0.786698783542764,-1.,-3.66710211820482));
#68964=CARTESIAN_POINT('Ctrl Pts',(0.786698783542764,1.,-3.66710211820482));
#68965=CARTESIAN_POINT('Ctrl Pts',(0.787095252590501,-1.,-3.66879484801113));
#68966=CARTESIAN_POINT('Ctrl Pts',(0.787095252590501,1.,-3.66879484801113));
#68967=CARTESIAN_POINT('Ctrl Pts',(0.787758799995742,-1.,-3.67252923663655));
#68968=CARTESIAN_POINT('Ctrl Pts',(0.787758799995742,1.,-3.67252923663655));
#68969=CARTESIAN_POINT('Ctrl Pts',(0.788569566220285,-1.,-3.67777119516252));
#68970=CARTESIAN_POINT('Ctrl Pts',(0.788569566220285,1.,-3.67777119516252));
#68971=CARTESIAN_POINT('Ctrl Pts',(0.789483546064386,-1.,-3.68428439783905));
#68972=CARTESIAN_POINT('Ctrl Pts',(0.789483546064386,1.,-3.68428439783905));
#68973=CARTESIAN_POINT('Ctrl Pts',(0.790436284988787,-1.,-3.69172044327364));
#68974=CARTESIAN_POINT('Ctrl Pts',(0.790436284988787,1.,-3.69172044327364));
#68975=CARTESIAN_POINT('Ctrl Pts',(0.79135657569598,-1.,-3.69968940808721));
#68976=CARTESIAN_POINT('Ctrl Pts',(0.79135657569598,1.,-3.69968940808721));
#68977=CARTESIAN_POINT('Ctrl Pts',(0.792177688845817,-1.,-3.70781724021806));
#68978=CARTESIAN_POINT('Ctrl Pts',(0.792177688845817,1.,-3.70781724021806));
#68979=CARTESIAN_POINT('Ctrl Pts',(0.792848377370287,-1.,-3.71580242396124));
#68980=CARTESIAN_POINT('Ctrl Pts',(0.792848377370287,1.,-3.71580242396124));
#68981=CARTESIAN_POINT('Ctrl Pts',(0.793347023784204,-1.,-3.72348797293734));
#68982=CARTESIAN_POINT('Ctrl Pts',(0.793347023784204,1.,-3.72348797293734));
#68983=CARTESIAN_POINT('Ctrl Pts',(0.793682750269684,-1.,-3.73086914695805));
#68984=CARTESIAN_POINT('Ctrl Pts',(0.793682750269684,1.,-3.73086914695805));
#68985=CARTESIAN_POINT('Ctrl Pts',(0.793882700937016,-1.,-3.73803280541687));
#68986=CARTESIAN_POINT('Ctrl Pts',(0.793882700937016,1.,-3.73803280541687));
#68987=CARTESIAN_POINT('Ctrl Pts',(0.793982700459951,-1.,-3.74511357728861));
#68988=CARTESIAN_POINT('Ctrl Pts',(0.793982700459951,1.,-3.74511357728861));
#68989=CARTESIAN_POINT('Ctrl Pts',(0.794017347371377,-1.,-3.75224692493864));
#68990=CARTESIAN_POINT('Ctrl Pts',(0.794017347371377,1.,-3.75224692493864));
#68991=CARTESIAN_POINT('Ctrl Pts',(0.794008429134907,-1.,-3.75951468666257));
#68992=CARTESIAN_POINT('Ctrl Pts',(0.794008429134907,1.,-3.75951468666257));
#68993=CARTESIAN_POINT('Ctrl Pts',(0.793961083688991,-1.,-3.76692626931111));
#68994=CARTESIAN_POINT('Ctrl Pts',(0.793961083688991,1.,-3.76692626931111));
#68995=CARTESIAN_POINT('Ctrl Pts',(0.793870523787407,-1.,-3.77444863801212));
#68996=CARTESIAN_POINT('Ctrl Pts',(0.793870523787407,1.,-3.77444863801212));
#68997=CARTESIAN_POINT('Ctrl Pts',(0.7937262357813,-1.,-3.78202460377598));
#68998=CARTESIAN_POINT('Ctrl Pts',(0.7937262357813,1.,-3.78202460377598));
#68999=CARTESIAN_POINT('Ctrl Pts',(0.793516871680993,-1.,-3.78959439439235));
#69000=CARTESIAN_POINT('Ctrl Pts',(0.793516871680993,1.,-3.78959439439235));
#69001=CARTESIAN_POINT('Ctrl Pts',(0.793235612973273,-1.,-3.79711921389897));
#69002=CARTESIAN_POINT('Ctrl Pts',(0.793235612973273,1.,-3.79711921389897));
#69003=CARTESIAN_POINT('Ctrl Pts',(0.792882695234777,-1.,-3.80459229925637));
#69004=CARTESIAN_POINT('Ctrl Pts',(0.792882695234777,1.,-3.80459229925637));
#69005=CARTESIAN_POINT('Ctrl Pts',(0.792462483517634,-1.,-3.81202588694756));
#69006=CARTESIAN_POINT('Ctrl Pts',(0.792462483517634,1.,-3.81202588694756));
#69007=CARTESIAN_POINT('Ctrl Pts',(0.791981740718634,-1.,-3.81944345442249));
#69008=CARTESIAN_POINT('Ctrl Pts',(0.791981740718634,1.,-3.81944345442249));
#69009=CARTESIAN_POINT('Ctrl Pts',(0.791447528662369,-1.,-3.82687033899792));
#69010=CARTESIAN_POINT('Ctrl Pts',(0.791447528662369,1.,-3.82687033899792));
#69011=CARTESIAN_POINT('Ctrl Pts',(0.7908650127053,-1.,-3.83432392054786));
#69012=CARTESIAN_POINT('Ctrl Pts',(0.7908650127053,1.,-3.83432392054786));
#69013=CARTESIAN_POINT('Ctrl Pts',(0.790236124191242,-1.,-3.84180762342454));
#69014=CARTESIAN_POINT('Ctrl Pts',(0.790236124191242,1.,-3.84180762342454));
#69015=CARTESIAN_POINT('Ctrl Pts',(0.789560798155582,-1.,-3.84931637808894));
#69016=CARTESIAN_POINT('Ctrl Pts',(0.789560798155582,1.,-3.84931637808894));
#69017=CARTESIAN_POINT('Ctrl Pts',(0.788837734090671,-1.,-3.85683995872529));
#69018=CARTESIAN_POINT('Ctrl Pts',(0.788837734090671,1.,-3.85683995872529));
#69019=CARTESIAN_POINT('Ctrl Pts',(0.788065315093777,-1.,-3.86436702561345));
#69020=CARTESIAN_POINT('Ctrl Pts',(0.788065315093777,1.,-3.86436702561345));
#69021=CARTESIAN_POINT('Ctrl Pts',(0.787242527617999,-1.,-3.87188916600912));
#69022=CARTESIAN_POINT('Ctrl Pts',(0.787242527617999,1.,-3.87188916600912));
#69023=CARTESIAN_POINT('Ctrl Pts',(0.786369675812608,-1.,-3.8794040281819));
#69024=CARTESIAN_POINT('Ctrl Pts',(0.786369675812608,1.,-3.8794040281819));
#69025=CARTESIAN_POINT('Ctrl Pts',(0.78544789034073,-1.,-3.88691313167398));
#69026=CARTESIAN_POINT('Ctrl Pts',(0.78544789034073,1.,-3.88691313167398));
#69027=CARTESIAN_POINT('Ctrl Pts',(0.784478799358336,-1.,-3.89442039235103));
#69028=CARTESIAN_POINT('Ctrl Pts',(0.784478799358336,1.,-3.89442039235103));
#69029=CARTESIAN_POINT('Ctrl Pts',(0.783464141529081,-1.,-3.9019303904397));
#69030=CARTESIAN_POINT('Ctrl Pts',(0.783464141529081,1.,-3.9019303904397));
#69031=CARTESIAN_POINT('Ctrl Pts',(0.782405395622764,-1.,-3.90944671004542));
#69032=CARTESIAN_POINT('Ctrl Pts',(0.782405395622764,1.,-3.90944671004542));
#69033=CARTESIAN_POINT('Ctrl Pts',(0.781303428618366,-1.,-3.91697036054676));
#69034=CARTESIAN_POINT('Ctrl Pts',(0.781303428618366,1.,-3.91697036054676));
#69035=CARTESIAN_POINT('Ctrl Pts',(0.780158678615542,-1.,-3.92450058323823));
#69036=CARTESIAN_POINT('Ctrl Pts',(0.780158678615542,1.,-3.92450058323823));
#69037=CARTESIAN_POINT('Ctrl Pts',(0.77897130813482,-1.,-3.93203552473174));
#69038=CARTESIAN_POINT('Ctrl Pts',(0.77897130813482,1.,-3.93203552473174));
#69039=CARTESIAN_POINT('Ctrl Pts',(0.777741370568558,-1.,-3.93957296768103));
#69040=CARTESIAN_POINT('Ctrl Pts',(0.777741370568558,1.,-3.93957296768103));
#69041=CARTESIAN_POINT('Ctrl Pts',(0.776468966697921,-1.,-3.94711101619447));
#69042=CARTESIAN_POINT('Ctrl Pts',(0.776468966697921,1.,-3.94711101619447));
#69043=CARTESIAN_POINT('Ctrl Pts',(0.775154418039351,-1.,-3.9546488545231));
#69044=CARTESIAN_POINT('Ctrl Pts',(0.775154418039351,1.,-3.9546488545231));
#69045=CARTESIAN_POINT('Ctrl Pts',(0.773798212026565,-1.,-3.96218649639807));
#69046=CARTESIAN_POINT('Ctrl Pts',(0.773798212026565,1.,-3.96218649639807));
#69047=CARTESIAN_POINT('Ctrl Pts',(0.772400931772136,-1.,-3.96972446532772));
#69048=CARTESIAN_POINT('Ctrl Pts',(0.772400931772136,1.,-3.96972446532772));
#69049=CARTESIAN_POINT('Ctrl Pts',(0.77096319003047,-1.,-3.97726349165488));
#69050=CARTESIAN_POINT('Ctrl Pts',(0.77096319003047,1.,-3.97726349165488));
#69051=CARTESIAN_POINT('Ctrl Pts',(0.769485566245544,-1.,-3.98480422348451));
#69052=CARTESIAN_POINT('Ctrl Pts',(0.769485566245544,1.,-3.98480422348451));
#69053=CARTESIAN_POINT('Ctrl Pts',(0.767968531377914,-1.,-3.9923468788101));
#69054=CARTESIAN_POINT('Ctrl Pts',(0.767968531377914,1.,-3.9923468788101));
#69055=CARTESIAN_POINT('Ctrl Pts',(0.766412457136063,-1.,-3.99989129179622));
#69056=CARTESIAN_POINT('Ctrl Pts',(0.766412457136063,1.,-3.99989129179622));
#69057=CARTESIAN_POINT('Ctrl Pts',(0.764817648785197,-1.,-4.00743706791509));
#69058=CARTESIAN_POINT('Ctrl Pts',(0.764817648785197,1.,-4.00743706791509));
#69059=CARTESIAN_POINT('Ctrl Pts',(0.763184371182935,-1.,-4.01498370680496));
#69060=CARTESIAN_POINT('Ctrl Pts',(0.763184371182935,1.,-4.01498370680496));
#69061=CARTESIAN_POINT('Ctrl Pts',(0.761512875859804,-1.,-4.02253072741268));
#69062=CARTESIAN_POINT('Ctrl Pts',(0.761512875859804,1.,-4.02253072741268));
#69063=CARTESIAN_POINT('Ctrl Pts',(0.759803433243751,-1.,-4.03007781954412));
#69064=CARTESIAN_POINT('Ctrl Pts',(0.759803433243751,1.,-4.03007781954412));
#69065=CARTESIAN_POINT('Ctrl Pts',(0.758056338884944,-1.,-4.03762485803119));
#69066=CARTESIAN_POINT('Ctrl Pts',(0.758056338884944,1.,-4.03762485803119));
#69067=CARTESIAN_POINT('Ctrl Pts',(0.75627190236958,-1.,-4.04517182653997));
#69068=CARTESIAN_POINT('Ctrl Pts',(0.75627190236958,1.,-4.04517182653997));
#69069=CARTESIAN_POINT('Ctrl Pts',(0.754450441816078,-1.,-4.05271876687915));
#69070=CARTESIAN_POINT('Ctrl Pts',(0.754450441816078,1.,-4.05271876687915));
#69071=CARTESIAN_POINT('Ctrl Pts',(0.752592276483072,-1.,-4.06026572221515));
#69072=CARTESIAN_POINT('Ctrl Pts',(0.752592276483072,1.,-4.06026572221515));
#69073=CARTESIAN_POINT('Ctrl Pts',(0.750697720484036,-1.,-4.06781267242378));
#69074=CARTESIAN_POINT('Ctrl Pts',(0.750697720484036,1.,-4.06781267242378));
#69075=CARTESIAN_POINT('Ctrl Pts',(0.748767076680557,-1.,-4.07535951056152));
#69076=CARTESIAN_POINT('Ctrl Pts',(0.748767076680557,1.,-4.07535951056152));
#69077=CARTESIAN_POINT('Ctrl Pts',(0.746800631492315,-1.,-4.08290608095642));
#69078=CARTESIAN_POINT('Ctrl Pts',(0.746800631492315,1.,-4.08290608095642));
#69079=CARTESIAN_POINT('Ctrl Pts',(0.7447986497065,-1.,-4.09045220253573));
#69080=CARTESIAN_POINT('Ctrl Pts',(0.7447986497065,1.,-4.09045220253573));
#69081=CARTESIAN_POINT('Ctrl Pts',(0.742761369689841,-1.,-4.09799769702611));
#69082=CARTESIAN_POINT('Ctrl Pts',(0.742761369689841,1.,-4.09799769702611));
#69083=CARTESIAN_POINT('Ctrl Pts',(0.740688998553376,-1.,-4.10554241757547));
#69084=CARTESIAN_POINT('Ctrl Pts',(0.740688998553376,1.,-4.10554241757547));
#69085=CARTESIAN_POINT('Ctrl Pts',(0.738581708225843,-1.,-4.11308626951927));
#69086=CARTESIAN_POINT('Ctrl Pts',(0.738581708225843,1.,-4.11308626951927));
#69087=CARTESIAN_POINT('Ctrl Pts',(0.736439634331344,-1.,-4.120629196238));
#69088=CARTESIAN_POINT('Ctrl Pts',(0.736439634331344,1.,-4.120629196238));
#69089=CARTESIAN_POINT('Ctrl Pts',(0.734698226764092,-1.,-4.12666277570844));
#69090=CARTESIAN_POINT('Ctrl Pts',(0.734698226764092,1.,-4.12666277570844));
#69091=CARTESIAN_POINT('Ctrl Pts',(0.733376589323546,-1.,-4.13118752795207));
#69092=CARTESIAN_POINT('Ctrl Pts',(0.733376589323546,1.,-4.13118752795207));
#69093=CARTESIAN_POINT('Ctrl Pts',(0.732488575135159,-1.,-4.1342038373684));
#69094=CARTESIAN_POINT('Ctrl Pts',(0.732488575135159,1.,-4.1342038373684));
#69095=CARTESIAN_POINT('Ctrl Pts',(0.73204283740062,-1.,-4.13571194405636));
#69096=CARTESIAN_POINT('Ctrl Pts',(0.73204283740062,1.,-4.13571194405636));
#69097=CARTESIAN_POINT('',(0.786422660831986,1.,-3.66661143271685));
#69098=CARTESIAN_POINT('Ctrl Pts',(0.786422660831985,-1.,-3.66661143271685));
#69099=CARTESIAN_POINT('Ctrl Pts',(0.786422660831985,-0.666666666666667,
-3.66661143271685));
#69100=CARTESIAN_POINT('Ctrl Pts',(0.786422660831985,-0.333333333333333,
-3.66661143271685));
#69101=CARTESIAN_POINT('Ctrl Pts',(0.786422660831985,0.333333333333333,
-3.66661143271685));
#69102=CARTESIAN_POINT('Ctrl Pts',(0.786422660831985,0.666666666666667,
-3.66661143271685));
#69103=CARTESIAN_POINT('Ctrl Pts',(0.786422660831985,1.,-3.66661143271685));
#69104=CARTESIAN_POINT('',(0.73204283740062,1.,-4.13571194405636));
#69105=CARTESIAN_POINT('',(0.73204283740062,0.,-4.13571194405636));
#69106=CARTESIAN_POINT('Ctrl Pts',(0.786422660831986,1.,-3.66661143271685));
#69107=CARTESIAN_POINT('Ctrl Pts',(0.786459983895432,1.,-3.6666431041522));
#69108=CARTESIAN_POINT('Ctrl Pts',(0.786565919558984,1.,-3.66680946938293));
#69109=CARTESIAN_POINT('Ctrl Pts',(0.786774337198062,1.,-3.66743103898702));
#69110=CARTESIAN_POINT('Ctrl Pts',(0.787145041181546,1.,-3.66907505398677));
#69111=CARTESIAN_POINT('Ctrl Pts',(0.787758799995742,1.,-3.67252923663655));
#69112=CARTESIAN_POINT('Ctrl Pts',(0.788569566220285,1.,-3.67777119516252));
#69113=CARTESIAN_POINT('Ctrl Pts',(0.789483546064386,1.,-3.68428439783905));
#69114=CARTESIAN_POINT('Ctrl Pts',(0.790436284988787,1.,-3.69172044327364));
#69115=CARTESIAN_POINT('Ctrl Pts',(0.79135657569598,1.,-3.69968940808721));
#69116=CARTESIAN_POINT('Ctrl Pts',(0.792177688845817,1.,-3.70781724021806));
#69117=CARTESIAN_POINT('Ctrl Pts',(0.792848377370287,1.,-3.71580242396124));
#69118=CARTESIAN_POINT('Ctrl Pts',(0.793347023784204,1.,-3.72348797293734));
#69119=CARTESIAN_POINT('Ctrl Pts',(0.793682750269684,1.,-3.73086914695805));
#69120=CARTESIAN_POINT('Ctrl Pts',(0.793882700937016,1.,-3.73803280541687));
#69121=CARTESIAN_POINT('Ctrl Pts',(0.793982700459951,1.,-3.74511357728861));
#69122=CARTESIAN_POINT('Ctrl Pts',(0.794017347371377,1.,-3.75224692493864));
#69123=CARTESIAN_POINT('Ctrl Pts',(0.794008429134907,1.,-3.75951468666257));
#69124=CARTESIAN_POINT('Ctrl Pts',(0.793961083688991,1.,-3.76692626931111));
#69125=CARTESIAN_POINT('Ctrl Pts',(0.793870523787407,1.,-3.77444863801212));
#69126=CARTESIAN_POINT('Ctrl Pts',(0.7937262357813,1.,-3.78202460377598));
#69127=CARTESIAN_POINT('Ctrl Pts',(0.793516871680993,1.,-3.78959439439235));
#69128=CARTESIAN_POINT('Ctrl Pts',(0.793235612973273,1.,-3.79711921389897));
#69129=CARTESIAN_POINT('Ctrl Pts',(0.792882695234777,1.,-3.80459229925637));
#69130=CARTESIAN_POINT('Ctrl Pts',(0.792462483517634,1.,-3.81202588694756));
#69131=CARTESIAN_POINT('Ctrl Pts',(0.791981740718634,1.,-3.81944345442249));
#69132=CARTESIAN_POINT('Ctrl Pts',(0.791447528662369,1.,-3.82687033899792));
#69133=CARTESIAN_POINT('Ctrl Pts',(0.7908650127053,1.,-3.83432392054786));
#69134=CARTESIAN_POINT('Ctrl Pts',(0.790236124191242,1.,-3.84180762342454));
#69135=CARTESIAN_POINT('Ctrl Pts',(0.789560798155582,1.,-3.84931637808894));
#69136=CARTESIAN_POINT('Ctrl Pts',(0.788837734090671,1.,-3.85683995872529));
#69137=CARTESIAN_POINT('Ctrl Pts',(0.788065315093777,1.,-3.86436702561345));
#69138=CARTESIAN_POINT('Ctrl Pts',(0.787242527617999,1.,-3.87188916600912));
#69139=CARTESIAN_POINT('Ctrl Pts',(0.786369675812608,1.,-3.8794040281819));
#69140=CARTESIAN_POINT('Ctrl Pts',(0.78544789034073,1.,-3.88691313167398));
#69141=CARTESIAN_POINT('Ctrl Pts',(0.784478799358336,1.,-3.89442039235103));
#69142=CARTESIAN_POINT('Ctrl Pts',(0.783464141529081,1.,-3.9019303904397));
#69143=CARTESIAN_POINT('Ctrl Pts',(0.782405395622764,1.,-3.90944671004542));
#69144=CARTESIAN_POINT('Ctrl Pts',(0.781303428618366,1.,-3.91697036054676));
#69145=CARTESIAN_POINT('Ctrl Pts',(0.780158678615542,1.,-3.92450058323823));
#69146=CARTESIAN_POINT('Ctrl Pts',(0.77897130813482,1.,-3.93203552473174));
#69147=CARTESIAN_POINT('Ctrl Pts',(0.777741370568558,1.,-3.93957296768103));
#69148=CARTESIAN_POINT('Ctrl Pts',(0.776468966697921,1.,-3.94711101619447));
#69149=CARTESIAN_POINT('Ctrl Pts',(0.775154418039351,1.,-3.9546488545231));
#69150=CARTESIAN_POINT('Ctrl Pts',(0.773798212026565,1.,-3.96218649639807));
#69151=CARTESIAN_POINT('Ctrl Pts',(0.772400931772136,1.,-3.96972446532772));
#69152=CARTESIAN_POINT('Ctrl Pts',(0.77096319003047,1.,-3.97726349165488));
#69153=CARTESIAN_POINT('Ctrl Pts',(0.769485566245544,1.,-3.98480422348451));
#69154=CARTESIAN_POINT('Ctrl Pts',(0.767968531377914,1.,-3.9923468788101));
#69155=CARTESIAN_POINT('Ctrl Pts',(0.766412457136063,1.,-3.99989129179622));
#69156=CARTESIAN_POINT('Ctrl Pts',(0.764817648785197,1.,-4.00743706791509));
#69157=CARTESIAN_POINT('Ctrl Pts',(0.763184371182935,1.,-4.01498370680496));
#69158=CARTESIAN_POINT('Ctrl Pts',(0.761512875859804,1.,-4.02253072741268));
#69159=CARTESIAN_POINT('Ctrl Pts',(0.759803433243751,1.,-4.03007781954412));
#69160=CARTESIAN_POINT('Ctrl Pts',(0.758056338884944,1.,-4.03762485803119));
#69161=CARTESIAN_POINT('Ctrl Pts',(0.75627190236958,1.,-4.04517182653997));
#69162=CARTESIAN_POINT('Ctrl Pts',(0.754450441816078,1.,-4.05271876687915));
#69163=CARTESIAN_POINT('Ctrl Pts',(0.752592276483072,1.,-4.06026572221515));
#69164=CARTESIAN_POINT('Ctrl Pts',(0.750697720484036,1.,-4.06781267242378));
#69165=CARTESIAN_POINT('Ctrl Pts',(0.748767076680557,1.,-4.07535951056152));
#69166=CARTESIAN_POINT('Ctrl Pts',(0.746800631492315,1.,-4.08290608095642));
#69167=CARTESIAN_POINT('Ctrl Pts',(0.7447986497065,1.,-4.09045220253573));
#69168=CARTESIAN_POINT('Ctrl Pts',(0.742761369689841,1.,-4.09799769702611));
#69169=CARTESIAN_POINT('Ctrl Pts',(0.740688998553376,1.,-4.10554241757547));
#69170=CARTESIAN_POINT('Ctrl Pts',(0.738581708225843,1.,-4.11308626951927));
#69171=CARTESIAN_POINT('Ctrl Pts',(0.736439634331344,1.,-4.120629196238));
#69172=CARTESIAN_POINT('Ctrl Pts',(0.734698226764092,1.,-4.12666277570844));
#69173=CARTESIAN_POINT('Ctrl Pts',(0.733376589323546,1.,-4.13118752795207));
#69174=CARTESIAN_POINT('Ctrl Pts',(0.732488575135159,1.,-4.1342038373684));
#69175=CARTESIAN_POINT('Ctrl Pts',(0.73204283740062,1.,-4.13571194405636));
#69176=CARTESIAN_POINT('Origin',(0.73204283740062,0.,-4.13571194405636));
#69177=CARTESIAN_POINT('',(0.581791163835815,1.,-4.15950947128175));
#69178=CARTESIAN_POINT('Origin',(0.,0.,0.));
#69179=CARTESIAN_POINT('',(0.963899035117248,1.,-3.62400312501245));
#69180=CARTESIAN_POINT('Origin',(0.,1.,0.));
#69181=CARTESIAN_POINT('Ctrl Pts',(0.963899035117248,1.,-3.62400312501246));
#69182=CARTESIAN_POINT('Ctrl Pts',(0.963899035117248,0.666666666666667,
-3.62400312501246));
#69183=CARTESIAN_POINT('Ctrl Pts',(0.963899035117248,0.333333333333333,
-3.62400312501246));
#69184=CARTESIAN_POINT('Ctrl Pts',(0.963899035117248,-0.333333333333333,
-3.62400312501246));
#69185=CARTESIAN_POINT('Ctrl Pts',(0.963899035117249,-0.666666666666667,
-3.62400312501246));
#69186=CARTESIAN_POINT('Ctrl Pts',(0.963899035117249,-1.,-3.62400312501246));
#69187=CARTESIAN_POINT('Ctrl Pts',(1.22531898815164,-1.,-4.01728681790024));
#69188=CARTESIAN_POINT('Ctrl Pts',(1.22531898815164,1.,-4.01728681790024));
#69189=CARTESIAN_POINT('Ctrl Pts',(1.22423716681447,-1.,-4.0161454457032));
#69190=CARTESIAN_POINT('Ctrl Pts',(1.22423716681447,1.,-4.0161454457032));
#69191=CARTESIAN_POINT('Ctrl Pts',(1.22207656456199,-1.,-4.01386104434674));
#69192=CARTESIAN_POINT('Ctrl Pts',(1.22207656456199,1.,-4.01386104434674));
#69193=CARTESIAN_POINT('Ctrl Pts',(1.21884478244983,-1.,-4.01042947142681));
#69194=CARTESIAN_POINT('Ctrl Pts',(1.21884478244983,1.,-4.01042947142681));
#69195=CARTESIAN_POINT('Ctrl Pts',(1.21455398918813,-1.,-4.00584409524937));
#69196=CARTESIAN_POINT('Ctrl Pts',(1.21455398918813,1.,-4.00584409524937));
#69197=CARTESIAN_POINT('Ctrl Pts',(1.20922097030107,-1.,-4.00009577952534));
#69198=CARTESIAN_POINT('Ctrl Pts',(1.20922097030107,1.,-4.00009577952534));
#69199=CARTESIAN_POINT('Ctrl Pts',(1.2039185237544,-1.,-3.99433084800649));
#69200=CARTESIAN_POINT('Ctrl Pts',(1.2039185237544,1.,-3.99433084800649));
#69201=CARTESIAN_POINT('Ctrl Pts',(1.19864679609596,-1.,-3.98854928957287));
#69202=CARTESIAN_POINT('Ctrl Pts',(1.19864679609596,1.,-3.98854928957287));
#69203=CARTESIAN_POINT('Ctrl Pts',(1.19340598349307,-1.,-3.98275111052015));
#69204=CARTESIAN_POINT('Ctrl Pts',(1.19340598349307,1.,-3.98275111052015));
#69205=CARTESIAN_POINT('Ctrl Pts',(1.18819633715285,-1.,-3.97693634766926));
#69206=CARTESIAN_POINT('Ctrl Pts',(1.18819633715285,1.,-3.97693634766926));
#69207=CARTESIAN_POINT('Ctrl Pts',(1.18301815039596,-1.,-3.9711050516465));
#69208=CARTESIAN_POINT('Ctrl Pts',(1.18301815039596,1.,-3.9711050516465));
#69209=CARTESIAN_POINT('Ctrl Pts',(1.17787174135445,-1.,-3.96525726357682));
#69210=CARTESIAN_POINT('Ctrl Pts',(1.17787174135445,1.,-3.96525726357682));
#69211=CARTESIAN_POINT('Ctrl Pts',(1.17275743590327,-1.,-3.95939299213164));
#69212=CARTESIAN_POINT('Ctrl Pts',(1.17275743590327,1.,-3.95939299213164));
#69213=CARTESIAN_POINT('Ctrl Pts',(1.16767555244495,-1.,-3.95351219510062));
#69214=CARTESIAN_POINT('Ctrl Pts',(1.16767555244495,1.,-3.95351219510062));
#69215=CARTESIAN_POINT('Ctrl Pts',(1.16262637999261,-1.,-3.9476147478092));
#69216=CARTESIAN_POINT('Ctrl Pts',(1.16262637999261,1.,-3.9476147478092));
#69217=CARTESIAN_POINT('Ctrl Pts',(1.1576101834106,-1.,-3.94170046685542));
#69218=CARTESIAN_POINT('Ctrl Pts',(1.1576101834106,1.,-3.94170046685542));
#69219=CARTESIAN_POINT('Ctrl Pts',(1.1526272271639,-1.,-3.9357691705651));
#69220=CARTESIAN_POINT('Ctrl Pts',(1.1526272271639,1.,-3.9357691705651));
#69221=CARTESIAN_POINT('Ctrl Pts',(1.14767779451147,-1.,-3.92982073294334));
#69222=CARTESIAN_POINT('Ctrl Pts',(1.14767779451147,1.,-3.92982073294334));
#69223=CARTESIAN_POINT('Ctrl Pts',(1.14276220561575,-1.,-3.92385513133937));
#69224=CARTESIAN_POINT('Ctrl Pts',(1.14276220561575,1.,-3.92385513133937));
#69225=CARTESIAN_POINT('Ctrl Pts',(1.13788084225511,-1.,-3.91787251936688));
#69226=CARTESIAN_POINT('Ctrl Pts',(1.13788084225511,1.,-3.91787251936688));
#69227=CARTESIAN_POINT('Ctrl Pts',(1.13303414693849,-1.,-3.91187321145495));
#69228=CARTESIAN_POINT('Ctrl Pts',(1.13303414693849,1.,-3.91187321145495));
#69229=CARTESIAN_POINT('Ctrl Pts',(1.12822258281518,-1.,-3.90585753318622));
#69230=CARTESIAN_POINT('Ctrl Pts',(1.12822258281518,1.,-3.90585753318622));
#69231=CARTESIAN_POINT('Ctrl Pts',(1.12344660099029,-1.,-3.89982569749978));
#69232=CARTESIAN_POINT('Ctrl Pts',(1.12344660099029,1.,-3.89982569749978));
#69233=CARTESIAN_POINT('Ctrl Pts',(1.11870660794609,-1.,-3.89377768340362));
#69234=CARTESIAN_POINT('Ctrl Pts',(1.11870660794609,1.,-3.89377768340362));
#69235=CARTESIAN_POINT('Ctrl Pts',(1.11400292434447,-1.,-3.88771308285229));
#69236=CARTESIAN_POINT('Ctrl Pts',(1.11400292434447,1.,-3.88771308285229));
#69237=CARTESIAN_POINT('Ctrl Pts',(1.10933577224029,-1.,-3.88163105531791));
#69238=CARTESIAN_POINT('Ctrl Pts',(1.10933577224029,1.,-3.88163105531791));
#69239=CARTESIAN_POINT('Ctrl Pts',(1.10470536603303,-1.,-3.87553067187566));
#69240=CARTESIAN_POINT('Ctrl Pts',(1.10470536603303,1.,-3.87553067187566));
#69241=CARTESIAN_POINT('Ctrl Pts',(1.10011198761202,-1.,-3.86941120134872));
#69242=CARTESIAN_POINT('Ctrl Pts',(1.10011198761202,1.,-3.86941120134872));
#69243=CARTESIAN_POINT('Ctrl Pts',(1.09555606505012,-1.,-3.86327241021242));
#69244=CARTESIAN_POINT('Ctrl Pts',(1.09555606505012,1.,-3.86327241021242));
#69245=CARTESIAN_POINT('Ctrl Pts',(1.09103825516288,-1.,-3.85711487933911));
#69246=CARTESIAN_POINT('Ctrl Pts',(1.09103825516288,1.,-3.85711487933911));
#69247=CARTESIAN_POINT('Ctrl Pts',(1.08655950846377,-1.,-3.85094025222691));
#69248=CARTESIAN_POINT('Ctrl Pts',(1.08655950846377,1.,-3.85094025222691));
#69249=CARTESIAN_POINT('Ctrl Pts',(1.08212087917986,-1.,-3.84475048030615));
#69250=CARTESIAN_POINT('Ctrl Pts',(1.08212087917986,1.,-3.84475048030615));
#69251=CARTESIAN_POINT('Ctrl Pts',(1.07772335353856,-1.,-3.83854714117486));
#69252=CARTESIAN_POINT('Ctrl Pts',(1.07772335353856,1.,-3.83854714117486));
#69253=CARTESIAN_POINT('Ctrl Pts',(1.0733676663346,-1.,-3.83233071195145));
#69254=CARTESIAN_POINT('Ctrl Pts',(1.0733676663346,1.,-3.83233071195145));
#69255=CARTESIAN_POINT('Ctrl Pts',(1.0690541318036,-1.,-3.82609989967278));
#69256=CARTESIAN_POINT('Ctrl Pts',(1.0690541318036,1.,-3.82609989967278));
#69257=CARTESIAN_POINT('Ctrl Pts',(1.06478244038931,-1.,-3.81985083953012));
#69258=CARTESIAN_POINT('Ctrl Pts',(1.06478244038931,1.,-3.81985083953012));
#69259=CARTESIAN_POINT('Ctrl Pts',(1.06055206187298,-1.,-3.81357866117485));
#69260=CARTESIAN_POINT('Ctrl Pts',(1.06055206187298,1.,-3.81357866117485));
#69261=CARTESIAN_POINT('Ctrl Pts',(1.05636266918643,-1.,-3.80727913637784));
#69262=CARTESIAN_POINT('Ctrl Pts',(1.05636266918643,1.,-3.80727913637784));
#69263=CARTESIAN_POINT('Ctrl Pts',(1.05221457990015,-1.,-3.80095039790678));
#69264=CARTESIAN_POINT('Ctrl Pts',(1.05221457990015,1.,-3.80095039790678));
#69265=CARTESIAN_POINT('Ctrl Pts',(1.04810913267641,-1.,-3.79459440308793));
#69266=CARTESIAN_POINT('Ctrl Pts',(1.04810913267641,1.,-3.79459440308793));
#69267=CARTESIAN_POINT('Ctrl Pts',(1.04404924374426,-1.,-3.78821910787195));
#69268=CARTESIAN_POINT('Ctrl Pts',(1.04404924374426,1.,-3.78821910787195));
#69269=CARTESIAN_POINT('Ctrl Pts',(1.04003862055804,-1.,-3.78183535008192));
#69270=CARTESIAN_POINT('Ctrl Pts',(1.04003862055804,1.,-3.78183535008192));
#69271=CARTESIAN_POINT('Ctrl Pts',(1.03608074678013,-1.,-3.77545283140445));
#69272=CARTESIAN_POINT('Ctrl Pts',(1.03608074678013,1.,-3.77545283140445));
#69273=CARTESIAN_POINT('Ctrl Pts',(1.0321778660492,-1.,-3.76907609832522));
#69274=CARTESIAN_POINT('Ctrl Pts',(1.0321778660492,1.,-3.76907609832522));
#69275=CARTESIAN_POINT('Ctrl Pts',(1.02833014458181,-1.,-3.76270122291232));
#69276=CARTESIAN_POINT('Ctrl Pts',(1.02833014458181,1.,-3.76270122291232));
#69277=CARTESIAN_POINT('Ctrl Pts',(1.0245342944466,-1.,-3.75631037456194));
#69278=CARTESIAN_POINT('Ctrl Pts',(1.0245342944466,1.,-3.75631037456194));
#69279=CARTESIAN_POINT('Ctrl Pts',(1.02078510487428,-1.,-3.74987777155834));
#69280=CARTESIAN_POINT('Ctrl Pts',(1.02078510487428,1.,-3.74987777155834));
#69281=CARTESIAN_POINT('Ctrl Pts',(1.01707794311079,-1.,-3.74337942504959));
#69282=CARTESIAN_POINT('Ctrl Pts',(1.01707794311079,1.,-3.74337942504959));
#69283=CARTESIAN_POINT('Ctrl Pts',(1.01341114319903,-1.,-3.73680245055734));
#69284=CARTESIAN_POINT('Ctrl Pts',(1.01341114319903,1.,-3.73680245055734));
#69285=CARTESIAN_POINT('Ctrl Pts',(1.00978798539496,-1.,-3.73015276704426));
#69286=CARTESIAN_POINT('Ctrl Pts',(1.00978798539496,1.,-3.73015276704426));
#69287=CARTESIAN_POINT('Ctrl Pts',(1.0062200073571,-1.,-3.72346803750596));
#69288=CARTESIAN_POINT('Ctrl Pts',(1.0062200073571,1.,-3.72346803750596));
#69289=CARTESIAN_POINT('Ctrl Pts',(1.00272423396822,-1.,-3.71680667125119));
#69290=CARTESIAN_POINT('Ctrl Pts',(1.00272423396822,1.,-3.71680667125119));
#69291=CARTESIAN_POINT('Ctrl Pts',(0.99931726075653,-1.,-3.71022439713938));
#69292=CARTESIAN_POINT('Ctrl Pts',(0.99931726075653,1.,-3.71022439713938));
#69293=CARTESIAN_POINT('Ctrl Pts',(0.996009819772518,-1.,-3.70375282282138));
#69294=CARTESIAN_POINT('Ctrl Pts',(0.996009819772518,1.,-3.70375282282138));
#69295=CARTESIAN_POINT('Ctrl Pts',(0.99280221833201,-1.,-3.69738123415662));
#69296=CARTESIAN_POINT('Ctrl Pts',(0.99280221833201,1.,-3.69738123415662));
#69297=CARTESIAN_POINT('Ctrl Pts',(0.989676715398558,-1.,-3.69102682138847));
#69298=CARTESIAN_POINT('Ctrl Pts',(0.989676715398558,1.,-3.69102682138847));
#69299=CARTESIAN_POINT('Ctrl Pts',(0.986602639863837,-1.,-3.68455317926068));
#69300=CARTESIAN_POINT('Ctrl Pts',(0.986602639863837,1.,-3.68455317926068));
#69301=CARTESIAN_POINT('Ctrl Pts',(0.983550791470419,-1.,-3.67782408841715));
#69302=CARTESIAN_POINT('Ctrl Pts',(0.983550791470419,1.,-3.67782408841715));
#69303=CARTESIAN_POINT('Ctrl Pts',(0.980505922458267,-1.,-3.67074983340361));
#69304=CARTESIAN_POINT('Ctrl Pts',(0.980505922458267,1.,-3.67074983340361));
#69305=CARTESIAN_POINT('Ctrl Pts',(0.977478312751618,-1.,-3.66333049637475));
#69306=CARTESIAN_POINT('Ctrl Pts',(0.977478312751618,1.,-3.66333049637475));
#69307=CARTESIAN_POINT('Ctrl Pts',(0.974519971354848,-1.,-3.65571576735126));
#69308=CARTESIAN_POINT('Ctrl Pts',(0.974519971354848,1.,-3.65571576735126));
#69309=CARTESIAN_POINT('Ctrl Pts',(0.971722122061341,-1.,-3.64819756447455));
#69310=CARTESIAN_POINT('Ctrl Pts',(0.971722122061341,1.,-3.64819756447455));
#69311=CARTESIAN_POINT('Ctrl Pts',(0.969195124675865,-1.,-3.64113946505766));
#69312=CARTESIAN_POINT('Ctrl Pts',(0.969195124675865,1.,-3.64113946505766));
#69313=CARTESIAN_POINT('Ctrl Pts',(0.967052554541385,-1.,-3.63492122081143));
#69314=CARTESIAN_POINT('Ctrl Pts',(0.967052554541385,1.,-3.63492122081143));
#69315=CARTESIAN_POINT('Ctrl Pts',(0.965395153165293,-1.,-3.62988252139846));
#69316=CARTESIAN_POINT('Ctrl Pts',(0.965395153165293,1.,-3.62988252139846));
#69317=CARTESIAN_POINT('Ctrl Pts',(0.964291001273287,-1.,-3.62625391254797));
#69318=CARTESIAN_POINT('Ctrl Pts',(0.964291001273287,1.,-3.62625391254797));
#69319=CARTESIAN_POINT('Ctrl Pts',(0.963875774530619,-1.,-3.6245656860652));
#69320=CARTESIAN_POINT('Ctrl Pts',(0.963875774530619,1.,-3.6245656860652));
#69321=CARTESIAN_POINT('Ctrl Pts',(0.963832486395051,-1.,-3.62399933639915));
#69322=CARTESIAN_POINT('Ctrl Pts',(0.963832486395051,1.,-3.62399933639915));
#69323=CARTESIAN_POINT('Ctrl Pts',(0.963922720982193,-1.,-3.62393257642052));
#69324=CARTESIAN_POINT('Ctrl Pts',(0.963922720982193,1.,-3.62393257642052));
#69325=CARTESIAN_POINT('Ctrl Pts',(0.963997613369571,-1.,-3.62397690409552));
#69326=CARTESIAN_POINT('Ctrl Pts',(0.963997613369571,1.,-3.62397690409552));
#69327=CARTESIAN_POINT('',(1.22531898815164,1.,-4.01728681790024));
#69328=CARTESIAN_POINT('Ctrl Pts',(1.22531898815164,1.,-4.01728681790024));
#69329=CARTESIAN_POINT('Ctrl Pts',(1.22423716681447,1.,-4.0161454457032));
#69330=CARTESIAN_POINT('Ctrl Pts',(1.22207656456199,1.,-4.01386104434674));
#69331=CARTESIAN_POINT('Ctrl Pts',(1.21884478244983,1.,-4.01042947142681));
#69332=CARTESIAN_POINT('Ctrl Pts',(1.21455398918813,1.,-4.00584409524937));
#69333=CARTESIAN_POINT('Ctrl Pts',(1.20922097030107,1.,-4.00009577952534));
#69334=CARTESIAN_POINT('Ctrl Pts',(1.2039185237544,1.,-3.99433084800649));
#69335=CARTESIAN_POINT('Ctrl Pts',(1.19864679609596,1.,-3.98854928957287));
#69336=CARTESIAN_POINT('Ctrl Pts',(1.19340598349307,1.,-3.98275111052015));
#69337=CARTESIAN_POINT('Ctrl Pts',(1.18819633715285,1.,-3.97693634766926));
#69338=CARTESIAN_POINT('Ctrl Pts',(1.18301815039596,1.,-3.9711050516465));
#69339=CARTESIAN_POINT('Ctrl Pts',(1.17787174135445,1.,-3.96525726357682));
#69340=CARTESIAN_POINT('Ctrl Pts',(1.17275743590327,1.,-3.95939299213164));
#69341=CARTESIAN_POINT('Ctrl Pts',(1.16767555244495,1.,-3.95351219510062));
#69342=CARTESIAN_POINT('Ctrl Pts',(1.16262637999261,1.,-3.9476147478092));
#69343=CARTESIAN_POINT('Ctrl Pts',(1.1576101834106,1.,-3.94170046685542));
#69344=CARTESIAN_POINT('Ctrl Pts',(1.1526272271639,1.,-3.9357691705651));
#69345=CARTESIAN_POINT('Ctrl Pts',(1.14767779451147,1.,-3.92982073294334));
#69346=CARTESIAN_POINT('Ctrl Pts',(1.14276220561575,1.,-3.92385513133937));
#69347=CARTESIAN_POINT('Ctrl Pts',(1.13788084225511,1.,-3.91787251936688));
#69348=CARTESIAN_POINT('Ctrl Pts',(1.13303414693849,1.,-3.91187321145495));
#69349=CARTESIAN_POINT('Ctrl Pts',(1.12822258281518,1.,-3.90585753318622));
#69350=CARTESIAN_POINT('Ctrl Pts',(1.12344660099029,1.,-3.89982569749978));
#69351=CARTESIAN_POINT('Ctrl Pts',(1.11870660794609,1.,-3.89377768340362));
#69352=CARTESIAN_POINT('Ctrl Pts',(1.11400292434447,1.,-3.88771308285229));
#69353=CARTESIAN_POINT('Ctrl Pts',(1.10933577224029,1.,-3.88163105531791));
#69354=CARTESIAN_POINT('Ctrl Pts',(1.10470536603303,1.,-3.87553067187566));
#69355=CARTESIAN_POINT('Ctrl Pts',(1.10011198761202,1.,-3.86941120134872));
#69356=CARTESIAN_POINT('Ctrl Pts',(1.09555606505012,1.,-3.86327241021242));
#69357=CARTESIAN_POINT('Ctrl Pts',(1.09103825516288,1.,-3.85711487933911));
#69358=CARTESIAN_POINT('Ctrl Pts',(1.08655950846377,1.,-3.85094025222691));
#69359=CARTESIAN_POINT('Ctrl Pts',(1.08212087917986,1.,-3.84475048030615));
#69360=CARTESIAN_POINT('Ctrl Pts',(1.07772335353856,1.,-3.83854714117486));
#69361=CARTESIAN_POINT('Ctrl Pts',(1.0733676663346,1.,-3.83233071195145));
#69362=CARTESIAN_POINT('Ctrl Pts',(1.0690541318036,1.,-3.82609989967278));
#69363=CARTESIAN_POINT('Ctrl Pts',(1.06478244038931,1.,-3.81985083953012));
#69364=CARTESIAN_POINT('Ctrl Pts',(1.06055206187298,1.,-3.81357866117485));
#69365=CARTESIAN_POINT('Ctrl Pts',(1.05636266918643,1.,-3.80727913637784));
#69366=CARTESIAN_POINT('Ctrl Pts',(1.05221457990015,1.,-3.80095039790678));
#69367=CARTESIAN_POINT('Ctrl Pts',(1.04810913267641,1.,-3.79459440308793));
#69368=CARTESIAN_POINT('Ctrl Pts',(1.04404924374426,1.,-3.78821910787195));
#69369=CARTESIAN_POINT('Ctrl Pts',(1.04003862055804,1.,-3.78183535008192));
#69370=CARTESIAN_POINT('Ctrl Pts',(1.03608074678013,1.,-3.77545283140445));
#69371=CARTESIAN_POINT('Ctrl Pts',(1.0321778660492,1.,-3.76907609832522));
#69372=CARTESIAN_POINT('Ctrl Pts',(1.02833014458181,1.,-3.76270122291232));
#69373=CARTESIAN_POINT('Ctrl Pts',(1.0245342944466,1.,-3.75631037456194));
#69374=CARTESIAN_POINT('Ctrl Pts',(1.02078510487428,1.,-3.74987777155834));
#69375=CARTESIAN_POINT('Ctrl Pts',(1.01707794311079,1.,-3.74337942504959));
#69376=CARTESIAN_POINT('Ctrl Pts',(1.01341114319903,1.,-3.73680245055734));
#69377=CARTESIAN_POINT('Ctrl Pts',(1.00978798539496,1.,-3.73015276704426));
#69378=CARTESIAN_POINT('Ctrl Pts',(1.0062200073571,1.,-3.72346803750596));
#69379=CARTESIAN_POINT('Ctrl Pts',(1.00272423396822,1.,-3.71680667125119));
#69380=CARTESIAN_POINT('Ctrl Pts',(0.99931726075653,1.,-3.71022439713938));
#69381=CARTESIAN_POINT('Ctrl Pts',(0.996009819772518,1.,-3.70375282282138));
#69382=CARTESIAN_POINT('Ctrl Pts',(0.99280221833201,1.,-3.69738123415662));
#69383=CARTESIAN_POINT('Ctrl Pts',(0.989676715398558,1.,-3.69102682138847));
#69384=CARTESIAN_POINT('Ctrl Pts',(0.986602639863837,1.,-3.68455317926068));
#69385=CARTESIAN_POINT('Ctrl Pts',(0.983550791470419,1.,-3.67782408841715));
#69386=CARTESIAN_POINT('Ctrl Pts',(0.980505922458267,1.,-3.67074983340361));
#69387=CARTESIAN_POINT('Ctrl Pts',(0.977478312751618,1.,-3.66333049637475));
#69388=CARTESIAN_POINT('Ctrl Pts',(0.974519971354848,1.,-3.65571576735126));
#69389=CARTESIAN_POINT('Ctrl Pts',(0.971722122061341,1.,-3.64819756447455));
#69390=CARTESIAN_POINT('Ctrl Pts',(0.969195124675865,1.,-3.64113946505766));
#69391=CARTESIAN_POINT('Ctrl Pts',(0.967052554541385,1.,-3.63492122081143));
#69392=CARTESIAN_POINT('Ctrl Pts',(0.965395153165293,1.,-3.62988252139846));
#69393=CARTESIAN_POINT('Ctrl Pts',(0.964373850166457,1.,-3.62652618145335));
#69394=CARTESIAN_POINT('Ctrl Pts',(0.963957782642843,1.,-3.62489305727662));
#69395=CARTESIAN_POINT('Ctrl Pts',(0.963861297423241,1.,-3.62424461507588));
#69396=CARTESIAN_POINT('Ctrl Pts',(0.963880158555582,1.,-3.6240482887845));
#69397=CARTESIAN_POINT('Ctrl Pts',(0.963899035117249,1.,-3.62400312501246));
#69398=CARTESIAN_POINT('',(1.22531898815164,0.,-4.01728681790024));
#69399=CARTESIAN_POINT('Ctrl Pts',(1.35022972712301,-1.,-3.49848248301936));
#69400=CARTESIAN_POINT('Ctrl Pts',(1.35022972712301,1.,-3.49848248301936));
#69401=CARTESIAN_POINT('Ctrl Pts',(1.35026426118402,-1.,-3.4984026005375));
#69402=CARTESIAN_POINT('Ctrl Pts',(1.35026426118402,1.,-3.4984026005375));
#69403=CARTESIAN_POINT('Ctrl Pts',(1.35037650303019,-1.,-3.49840357193736));
#69404=CARTESIAN_POINT('Ctrl Pts',(1.35037650303019,1.,-3.49840357193736));
#69405=CARTESIAN_POINT('Ctrl Pts',(1.35067437417483,-1.,-3.49888720257132));
#69406=CARTESIAN_POINT('Ctrl Pts',(1.35067437417483,1.,-3.49888720257132));
#69407=CARTESIAN_POINT('Ctrl Pts',(1.3513307633124,-1.,-3.5004970706414));
#69408=CARTESIAN_POINT('Ctrl Pts',(1.3513307633124,1.,-3.5004970706414));
#69409=CARTESIAN_POINT('Ctrl Pts',(1.35257032843486,-1.,-3.50408168106261));
#69410=CARTESIAN_POINT('Ctrl Pts',(1.35257032843486,1.,-3.50408168106261));
#69411=CARTESIAN_POINT('Ctrl Pts',(1.35419113575956,-1.,-3.50913227059999));
#69412=CARTESIAN_POINT('Ctrl Pts',(1.35419113575956,1.,-3.50913227059999));
#69413=CARTESIAN_POINT('Ctrl Pts',(1.35611275237152,-1.,-3.51542230699556));
#69414=CARTESIAN_POINT('Ctrl Pts',(1.35611275237152,1.,-3.51542230699556));
#69415=CARTESIAN_POINT('Ctrl Pts',(1.35821701528836,-1.,-3.52261776116748));
#69416=CARTESIAN_POINT('Ctrl Pts',(1.35821701528836,1.,-3.52261776116748));
#69417=CARTESIAN_POINT('Ctrl Pts',(1.36037259643734,-1.,-3.530344649616));
#69418=CARTESIAN_POINT('Ctrl Pts',(1.36037259643734,1.,-3.530344649616));
#69419=CARTESIAN_POINT('Ctrl Pts',(1.36245507339307,-1.,-3.53824396424961));
#69420=CARTESIAN_POINT('Ctrl Pts',(1.36245507339307,1.,-3.53824396424961));
#69421=CARTESIAN_POINT('Ctrl Pts',(1.36436666257597,-1.,-3.54602591832973));
#69422=CARTESIAN_POINT('Ctrl Pts',(1.36436666257597,1.,-3.54602591832973));
#69423=CARTESIAN_POINT('Ctrl Pts',(1.3660614545677,-1.,-3.55353883995949));
#69424=CARTESIAN_POINT('Ctrl Pts',(1.3660614545677,1.,-3.55353883995949));
#69425=CARTESIAN_POINT('Ctrl Pts',(1.36754771771233,-1.,-3.56077662028649));
#69426=CARTESIAN_POINT('Ctrl Pts',(1.36754771771233,1.,-3.56077662028649));
#69427=CARTESIAN_POINT('Ctrl Pts',(1.36886584973389,-1.,-3.5678208030466));
#69428=CARTESIAN_POINT('Ctrl Pts',(1.36886584973389,1.,-3.5678208030466));
#69429=CARTESIAN_POINT('Ctrl Pts',(1.37007229485659,-1.,-3.57479875549486));
#69430=CARTESIAN_POINT('Ctrl Pts',(1.37007229485659,1.,-3.57479875549486));
#69431=CARTESIAN_POINT('Ctrl Pts',(1.37122241663062,-1.,-3.58183885982715));
#69432=CARTESIAN_POINT('Ctrl Pts',(1.37122241663062,1.,-3.58183885982715));
#69433=CARTESIAN_POINT('Ctrl Pts',(1.37235053660976,-1.,-3.58901853846365));
#69434=CARTESIAN_POINT('Ctrl Pts',(1.37235053660976,1.,-3.58901853846365));
#69435=CARTESIAN_POINT('Ctrl Pts',(1.37346320103157,-1.,-3.59634627869048));
#69436=CARTESIAN_POINT('Ctrl Pts',(1.37346320103157,1.,-3.59634627869048));
#69437=CARTESIAN_POINT('Ctrl Pts',(1.37455051379623,-1.,-3.60379020123988));
#69438=CARTESIAN_POINT('Ctrl Pts',(1.37455051379623,1.,-3.60379020123988));
#69439=CARTESIAN_POINT('Ctrl Pts',(1.37559314436634,-1.,-3.61129546591064));
#69440=CARTESIAN_POINT('Ctrl Pts',(1.37559314436634,1.,-3.61129546591064));
#69441=CARTESIAN_POINT('Ctrl Pts',(1.37657053403107,-1.,-3.61880481160421));
#69442=CARTESIAN_POINT('Ctrl Pts',(1.37657053403107,1.,-3.61880481160421));
#69443=CARTESIAN_POINT('Ctrl Pts',(1.37746987919881,-1.,-3.62628098665145));
#69444=CARTESIAN_POINT('Ctrl Pts',(1.37746987919881,1.,-3.62628098665145));
#69445=CARTESIAN_POINT('Ctrl Pts',(1.37829035457339,-1.,-3.63371727442486));
#69446=CARTESIAN_POINT('Ctrl Pts',(1.37829035457339,1.,-3.63371727442486));
#69447=CARTESIAN_POINT('Ctrl Pts',(1.37903818567359,-1.,-3.64112507791141));
#69448=CARTESIAN_POINT('Ctrl Pts',(1.37903818567359,1.,-3.64112507791141));
#69449=CARTESIAN_POINT('Ctrl Pts',(1.37972372481603,-1.,-3.64852652756456));
#69450=CARTESIAN_POINT('Ctrl Pts',(1.37972372481603,1.,-3.64852652756456));
#69451=CARTESIAN_POINT('Ctrl Pts',(1.38035791051212,-1.,-3.6559455440439));
#69452=CARTESIAN_POINT('Ctrl Pts',(1.38035791051212,1.,-3.6559455440439));
#69453=CARTESIAN_POINT('Ctrl Pts',(1.38094856333552,-1.,-3.66339848520857));
#69454=CARTESIAN_POINT('Ctrl Pts',(1.38094856333552,1.,-3.66339848520857));
#69455=CARTESIAN_POINT('Ctrl Pts',(1.38149812653868,-1.,-3.67088843112262));
#69456=CARTESIAN_POINT('Ctrl Pts',(1.38149812653868,1.,-3.67088843112262));
#69457=CARTESIAN_POINT('Ctrl Pts',(1.3820057429062,-1.,-3.67841038482414));
#69458=CARTESIAN_POINT('Ctrl Pts',(1.3820057429062,1.,-3.67841038482414));
#69459=CARTESIAN_POINT('Ctrl Pts',(1.38246852827182,-1.,-3.68595444983838));
#69460=CARTESIAN_POINT('Ctrl Pts',(1.38246852827182,1.,-3.68595444983838));
#69461=CARTESIAN_POINT('Ctrl Pts',(1.3828831117165,-1.,-3.69350967899526));
#69462=CARTESIAN_POINT('Ctrl Pts',(1.3828831117165,1.,-3.69350967899526));
#69463=CARTESIAN_POINT('Ctrl Pts',(1.38324717612865,-1.,-3.701067921679));
#69464=CARTESIAN_POINT('Ctrl Pts',(1.38324717612865,1.,-3.701067921679));
#69465=CARTESIAN_POINT('Ctrl Pts',(1.38356065402124,-1.,-3.70862680753347));
#69466=CARTESIAN_POINT('Ctrl Pts',(1.38356065402124,1.,-3.70862680753347));
#69467=CARTESIAN_POINT('Ctrl Pts',(1.38382489984586,-1.,-3.7161876605181));
#69468=CARTESIAN_POINT('Ctrl Pts',(1.38382489984586,1.,-3.7161876605181));
#69469=CARTESIAN_POINT('Ctrl Pts',(1.3840421342895,-1.,-3.72375409358803));
#69470=CARTESIAN_POINT('Ctrl Pts',(1.3840421342895,1.,-3.72375409358803));
#69471=CARTESIAN_POINT('Ctrl Pts',(1.38421479111531,-1.,-3.73133035859282));
#69472=CARTESIAN_POINT('Ctrl Pts',(1.38421479111531,1.,-3.73133035859282));
#69473=CARTESIAN_POINT('Ctrl Pts',(1.38434489156458,-1.,-3.73891976418104));
#69474=CARTESIAN_POINT('Ctrl Pts',(1.38434489156458,1.,-3.73891976418104));
#69475=CARTESIAN_POINT('Ctrl Pts',(1.38443344984394,-1.,-3.74652317167876));
#69476=CARTESIAN_POINT('Ctrl Pts',(1.38443344984394,1.,-3.74652317167876));
#69477=CARTESIAN_POINT('Ctrl Pts',(1.38448077997163,-1.,-3.7541397631875));
#69478=CARTESIAN_POINT('Ctrl Pts',(1.38448077997163,1.,-3.7541397631875));
#69479=CARTESIAN_POINT('Ctrl Pts',(1.3844867525335,-1.,-3.76176768271367));
#69480=CARTESIAN_POINT('Ctrl Pts',(1.3844867525335,1.,-3.76176768271367));
#69481=CARTESIAN_POINT('Ctrl Pts',(1.38445107339518,-1.,-3.76940473185779));
#69482=CARTESIAN_POINT('Ctrl Pts',(1.38445107339518,1.,-3.76940473185779));
#69483=CARTESIAN_POINT('Ctrl Pts',(1.38437354551428,-1.,-3.77704902230418));
#69484=CARTESIAN_POINT('Ctrl Pts',(1.38437354551428,1.,-3.77704902230418));
#69485=CARTESIAN_POINT('Ctrl Pts',(1.38425435883756,-1.,-3.78469969805082));
#69486=CARTESIAN_POINT('Ctrl Pts',(1.38425435883756,1.,-3.78469969805082));
#69487=CARTESIAN_POINT('Ctrl Pts',(1.38409399694566,-1.,-3.79235669640841));
#69488=CARTESIAN_POINT('Ctrl Pts',(1.38409399694566,1.,-3.79235669640841));
#69489=CARTESIAN_POINT('Ctrl Pts',(1.38389311766682,-1.,-3.80002044322111));
#69490=CARTESIAN_POINT('Ctrl Pts',(1.38389311766682,1.,-3.80002044322111));
#69491=CARTESIAN_POINT('Ctrl Pts',(1.3836524404622,-1.,-3.80769156398411));
#69492=CARTESIAN_POINT('Ctrl Pts',(1.3836524404622,1.,-3.80769156398411));
#69493=CARTESIAN_POINT('Ctrl Pts',(1.38337263902782,-1.,-3.81537060817811));
#69494=CARTESIAN_POINT('Ctrl Pts',(1.38337263902782,1.,-3.81537060817811));
#69495=CARTESIAN_POINT('Ctrl Pts',(1.38305421262763,-1.,-3.82305771743829));
#69496=CARTESIAN_POINT('Ctrl Pts',(1.38305421262763,1.,-3.82305771743829));
#69497=CARTESIAN_POINT('Ctrl Pts',(1.38269750245138,-1.,-3.8307526698229));
#69498=CARTESIAN_POINT('Ctrl Pts',(1.38269750245138,1.,-3.8307526698229));
#69499=CARTESIAN_POINT('Ctrl Pts',(1.38230274828821,-1.,-3.83845502790746));
#69500=CARTESIAN_POINT('Ctrl Pts',(1.38230274828821,1.,-3.83845502790746));
#69501=CARTESIAN_POINT('Ctrl Pts',(1.38187013346109,-1.,-3.84616425605764));
#69502=CARTESIAN_POINT('Ctrl Pts',(1.38187013346109,1.,-3.84616425605764));
#69503=CARTESIAN_POINT('Ctrl Pts',(1.38139983115049,-1.,-3.85387983979481));
#69504=CARTESIAN_POINT('Ctrl Pts',(1.38139983115049,1.,-3.85387983979481));
#69505=CARTESIAN_POINT('Ctrl Pts',(1.38089205992989,-1.,-3.86160143043959));
#69506=CARTESIAN_POINT('Ctrl Pts',(1.38089205992989,1.,-3.86160143043959));
#69507=CARTESIAN_POINT('Ctrl Pts',(1.38034709213014,-1.,-3.86932885813068));
#69508=CARTESIAN_POINT('Ctrl Pts',(1.38034709213014,1.,-3.86932885813068));
#69509=CARTESIAN_POINT('Ctrl Pts',(1.37976523097073,-1.,-3.87706205830532));
#69510=CARTESIAN_POINT('Ctrl Pts',(1.37976523097073,1.,-3.87706205830532));
#69511=CARTESIAN_POINT('Ctrl Pts',(1.37914679719383,-1.,-3.88480102249278));
#69512=CARTESIAN_POINT('Ctrl Pts',(1.37914679719383,1.,-3.88480102249278));
#69513=CARTESIAN_POINT('Ctrl Pts',(1.3784921128802,-1.,-3.89254574338496));
#69514=CARTESIAN_POINT('Ctrl Pts',(1.3784921128802,1.,-3.89254574338496));
#69515=CARTESIAN_POINT('Ctrl Pts',(1.37780148512792,-1.,-3.90029615196727));
#69516=CARTESIAN_POINT('Ctrl Pts',(1.37780148512792,1.,-3.90029615196727));
#69517=CARTESIAN_POINT('Ctrl Pts',(1.3770751963402,-1.,-3.90805209523486));
#69518=CARTESIAN_POINT('Ctrl Pts',(1.3770751963402,1.,-3.90805209523486));
#69519=CARTESIAN_POINT('Ctrl Pts',(1.37631350505797,-1.,-3.91581337462644));
#69520=CARTESIAN_POINT('Ctrl Pts',(1.37631350505797,1.,-3.91581337462644));
#69521=CARTESIAN_POINT('Ctrl Pts',(1.37551664448242,-1.,-3.92357976987672));
#69522=CARTESIAN_POINT('Ctrl Pts',(1.37551664448242,1.,-3.92357976987672));
#69523=CARTESIAN_POINT('Ctrl Pts',(1.37468482215751,-1.,-3.93135106761844));
#69524=CARTESIAN_POINT('Ctrl Pts',(1.37468482215751,1.,-3.93135106761844));
#69525=CARTESIAN_POINT('Ctrl Pts',(1.37381821967165,-1.,-3.93912709040818));
#69526=CARTESIAN_POINT('Ctrl Pts',(1.37381821967165,1.,-3.93912709040818));
#69527=CARTESIAN_POINT('Ctrl Pts',(1.37291699202807,-1.,-3.94690771785133));
#69528=CARTESIAN_POINT('Ctrl Pts',(1.37291699202807,1.,-3.94690771785133));
#69529=CARTESIAN_POINT('Ctrl Pts',(1.37198126432386,-1.,-3.95469287280914));
#69530=CARTESIAN_POINT('Ctrl Pts',(1.37198126432386,1.,-3.95469287280914));
#69531=CARTESIAN_POINT('Ctrl Pts',(1.3712051561502,-1.,-3.96092458506535));
#69532=CARTESIAN_POINT('Ctrl Pts',(1.3712051561502,1.,-3.96092458506535));
#69533=CARTESIAN_POINT('Ctrl Pts',(1.37060761745635,-1.,-3.96560037974645));
#69534=CARTESIAN_POINT('Ctrl Pts',(1.37060761745635,1.,-3.96560037974645));
#69535=CARTESIAN_POINT('Ctrl Pts',(1.37020239094614,-1.,-3.9687184694131));
#69536=CARTESIAN_POINT('Ctrl Pts',(1.37020239094614,1.,-3.9687184694131));
#69537=CARTESIAN_POINT('Ctrl Pts',(1.36999806084572,-1.,-3.97027773754922));
#69538=CARTESIAN_POINT('Ctrl Pts',(1.36999806084572,1.,-3.97027773754922));
#69539=CARTESIAN_POINT('',(1.35032489087101,1.,-3.4984457533445));
#69540=CARTESIAN_POINT('Ctrl Pts',(1.35032489087101,-1.,-3.4984457533445));
#69541=CARTESIAN_POINT('Ctrl Pts',(1.35032489087101,-0.666666666666667,
-3.4984457533445));
#69542=CARTESIAN_POINT('Ctrl Pts',(1.35032489087101,-0.333333333333333,
-3.4984457533445));
#69543=CARTESIAN_POINT('Ctrl Pts',(1.35032489087101,0.333333333333333,-3.4984457533445));
#69544=CARTESIAN_POINT('Ctrl Pts',(1.35032489087101,0.666666666666667,-3.4984457533445));
#69545=CARTESIAN_POINT('Ctrl Pts',(1.35032489087101,1.,-3.4984457533445));
#69546=CARTESIAN_POINT('',(1.36999806084572,1.,-3.97027773754922));
#69547=CARTESIAN_POINT('',(1.36999806084572,0.,-3.97027773754922));
#69548=CARTESIAN_POINT('Ctrl Pts',(1.35032489087101,1.,-3.49844575334451));
#69549=CARTESIAN_POINT('Ctrl Pts',(1.35036670892966,1.,-3.49847119623846));
#69550=CARTESIAN_POINT('Ctrl Pts',(1.35049736560527,1.,-3.49861894124827));
#69551=CARTESIAN_POINT('Ctrl Pts',(1.35080045218587,1.,-3.49920025459723));
#69552=CARTESIAN_POINT('Ctrl Pts',(1.35142377279517,1.,-3.50076603816491));
#69553=CARTESIAN_POINT('Ctrl Pts',(1.35257032843486,1.,-3.50408168106261));
#69554=CARTESIAN_POINT('Ctrl Pts',(1.35419113575956,1.,-3.50913227059999));
#69555=CARTESIAN_POINT('Ctrl Pts',(1.35611275237152,1.,-3.51542230699556));
#69556=CARTESIAN_POINT('Ctrl Pts',(1.35821701528836,1.,-3.52261776116748));
#69557=CARTESIAN_POINT('Ctrl Pts',(1.36037259643734,1.,-3.530344649616));
#69558=CARTESIAN_POINT('Ctrl Pts',(1.36245507339307,1.,-3.53824396424961));
#69559=CARTESIAN_POINT('Ctrl Pts',(1.36436666257597,1.,-3.54602591832973));
#69560=CARTESIAN_POINT('Ctrl Pts',(1.3660614545677,1.,-3.55353883995949));
#69561=CARTESIAN_POINT('Ctrl Pts',(1.36754771771233,1.,-3.56077662028649));
#69562=CARTESIAN_POINT('Ctrl Pts',(1.36886584973389,1.,-3.5678208030466));
#69563=CARTESIAN_POINT('Ctrl Pts',(1.37007229485659,1.,-3.57479875549486));
#69564=CARTESIAN_POINT('Ctrl Pts',(1.37122241663062,1.,-3.58183885982715));
#69565=CARTESIAN_POINT('Ctrl Pts',(1.37235053660976,1.,-3.58901853846365));
#69566=CARTESIAN_POINT('Ctrl Pts',(1.37346320103157,1.,-3.59634627869048));
#69567=CARTESIAN_POINT('Ctrl Pts',(1.37455051379623,1.,-3.60379020123988));
#69568=CARTESIAN_POINT('Ctrl Pts',(1.37559314436634,1.,-3.61129546591064));
#69569=CARTESIAN_POINT('Ctrl Pts',(1.37657053403107,1.,-3.61880481160421));
#69570=CARTESIAN_POINT('Ctrl Pts',(1.37746987919881,1.,-3.62628098665145));
#69571=CARTESIAN_POINT('Ctrl Pts',(1.37829035457339,1.,-3.63371727442486));
#69572=CARTESIAN_POINT('Ctrl Pts',(1.37903818567359,1.,-3.64112507791141));
#69573=CARTESIAN_POINT('Ctrl Pts',(1.37972372481603,1.,-3.64852652756456));
#69574=CARTESIAN_POINT('Ctrl Pts',(1.38035791051212,1.,-3.6559455440439));
#69575=CARTESIAN_POINT('Ctrl Pts',(1.38094856333552,1.,-3.66339848520857));
#69576=CARTESIAN_POINT('Ctrl Pts',(1.38149812653868,1.,-3.67088843112262));
#69577=CARTESIAN_POINT('Ctrl Pts',(1.3820057429062,1.,-3.67841038482414));
#69578=CARTESIAN_POINT('Ctrl Pts',(1.38246852827182,1.,-3.68595444983838));
#69579=CARTESIAN_POINT('Ctrl Pts',(1.3828831117165,1.,-3.69350967899526));
#69580=CARTESIAN_POINT('Ctrl Pts',(1.38324717612865,1.,-3.701067921679));
#69581=CARTESIAN_POINT('Ctrl Pts',(1.38356065402124,1.,-3.70862680753347));
#69582=CARTESIAN_POINT('Ctrl Pts',(1.38382489984586,1.,-3.7161876605181));
#69583=CARTESIAN_POINT('Ctrl Pts',(1.3840421342895,1.,-3.72375409358803));
#69584=CARTESIAN_POINT('Ctrl Pts',(1.38421479111531,1.,-3.73133035859282));
#69585=CARTESIAN_POINT('Ctrl Pts',(1.38434489156458,1.,-3.73891976418104));
#69586=CARTESIAN_POINT('Ctrl Pts',(1.38443344984394,1.,-3.74652317167876));
#69587=CARTESIAN_POINT('Ctrl Pts',(1.38448077997163,1.,-3.7541397631875));
#69588=CARTESIAN_POINT('Ctrl Pts',(1.3844867525335,1.,-3.76176768271367));
#69589=CARTESIAN_POINT('Ctrl Pts',(1.38445107339518,1.,-3.76940473185779));
#69590=CARTESIAN_POINT('Ctrl Pts',(1.38437354551428,1.,-3.77704902230418));
#69591=CARTESIAN_POINT('Ctrl Pts',(1.38425435883756,1.,-3.78469969805082));
#69592=CARTESIAN_POINT('Ctrl Pts',(1.38409399694566,1.,-3.79235669640841));
#69593=CARTESIAN_POINT('Ctrl Pts',(1.38389311766682,1.,-3.80002044322111));
#69594=CARTESIAN_POINT('Ctrl Pts',(1.3836524404622,1.,-3.80769156398411));
#69595=CARTESIAN_POINT('Ctrl Pts',(1.38337263902782,1.,-3.81537060817811));
#69596=CARTESIAN_POINT('Ctrl Pts',(1.38305421262763,1.,-3.82305771743829));
#69597=CARTESIAN_POINT('Ctrl Pts',(1.38269750245138,1.,-3.8307526698229));
#69598=CARTESIAN_POINT('Ctrl Pts',(1.38230274828821,1.,-3.83845502790746));
#69599=CARTESIAN_POINT('Ctrl Pts',(1.38187013346109,1.,-3.84616425605764));
#69600=CARTESIAN_POINT('Ctrl Pts',(1.38139983115049,1.,-3.85387983979481));
#69601=CARTESIAN_POINT('Ctrl Pts',(1.38089205992989,1.,-3.86160143043959));
#69602=CARTESIAN_POINT('Ctrl Pts',(1.38034709213014,1.,-3.86932885813068));
#69603=CARTESIAN_POINT('Ctrl Pts',(1.37976523097073,1.,-3.87706205830532));
#69604=CARTESIAN_POINT('Ctrl Pts',(1.37914679719383,1.,-3.88480102249278));
#69605=CARTESIAN_POINT('Ctrl Pts',(1.3784921128802,1.,-3.89254574338496));
#69606=CARTESIAN_POINT('Ctrl Pts',(1.37780148512792,1.,-3.90029615196727));
#69607=CARTESIAN_POINT('Ctrl Pts',(1.3770751963402,1.,-3.90805209523486));
#69608=CARTESIAN_POINT('Ctrl Pts',(1.37631350505797,1.,-3.91581337462644));
#69609=CARTESIAN_POINT('Ctrl Pts',(1.37551664448242,1.,-3.92357976987672));
#69610=CARTESIAN_POINT('Ctrl Pts',(1.37468482215751,1.,-3.93135106761844));
#69611=CARTESIAN_POINT('Ctrl Pts',(1.37381821967165,1.,-3.93912709040818));
#69612=CARTESIAN_POINT('Ctrl Pts',(1.37291699202807,1.,-3.94690771785133));
#69613=CARTESIAN_POINT('Ctrl Pts',(1.37198126432386,1.,-3.95469287280914));
#69614=CARTESIAN_POINT('Ctrl Pts',(1.3712051561502,1.,-3.96092458506535));
#69615=CARTESIAN_POINT('Ctrl Pts',(1.37060761745635,1.,-3.96560037974645));
#69616=CARTESIAN_POINT('Ctrl Pts',(1.37020239094614,1.,-3.9687184694131));
#69617=CARTESIAN_POINT('Ctrl Pts',(1.36999806084572,1.,-3.97027773754922));
#69618=CARTESIAN_POINT('Origin',(1.36999806084572,0.,-3.97027773754922));
#69619=CARTESIAN_POINT('',(1.22531898815164,1.,-4.01728681790024));
#69620=CARTESIAN_POINT('Origin',(0.,0.,0.));
#69621=CARTESIAN_POINT('',(1.51895082866166,1.,-3.42859860294378));
#69622=CARTESIAN_POINT('Origin',(0.,1.,0.));
#69623=CARTESIAN_POINT('Ctrl Pts',(1.51895082866166,1.,-3.42859860294378));
#69624=CARTESIAN_POINT('Ctrl Pts',(1.51895082866166,0.666666666666667,-3.42859860294378));
#69625=CARTESIAN_POINT('Ctrl Pts',(1.51895082866166,0.333333333333333,-3.42859860294378));
#69626=CARTESIAN_POINT('Ctrl Pts',(1.51895082866166,-0.333333333333333,
-3.42859860294378));
#69627=CARTESIAN_POINT('Ctrl Pts',(1.51895082866166,-0.666666666666667,
-3.42859860294378));
#69628=CARTESIAN_POINT('Ctrl Pts',(1.51895082866166,-1.,-3.42859860294378));
#69629=CARTESIAN_POINT('Ctrl Pts',(1.83867539237861,-1.,-3.77614523045147));
#69630=CARTESIAN_POINT('Ctrl Pts',(1.83867539237861,1.,-3.77614523045147));
#69631=CARTESIAN_POINT('Ctrl Pts',(1.83742834010821,-1.,-3.77518714458232));
#69632=CARTESIAN_POINT('Ctrl Pts',(1.83742834010821,1.,-3.77518714458232));
#69633=CARTESIAN_POINT('Ctrl Pts',(1.83493697935064,-1.,-3.77326886065484));
#69634=CARTESIAN_POINT('Ctrl Pts',(1.83493697935064,1.,-3.77326886065484));
#69635=CARTESIAN_POINT('Ctrl Pts',(1.83120816956515,-1.,-3.77038509819777));
#69636=CARTESIAN_POINT('Ctrl Pts',(1.83120816956515,1.,-3.77038509819777));
#69637=CARTESIAN_POINT('Ctrl Pts',(1.82625289221933,-1.,-3.76652740355856));
#69638=CARTESIAN_POINT('Ctrl Pts',(1.82625289221933,1.,-3.76652740355856));
#69639=CARTESIAN_POINT('Ctrl Pts',(1.82008629694924,-1.,-3.76168412709652));
#69640=CARTESIAN_POINT('Ctrl Pts',(1.82008629694924,1.,-3.76168412709652));
#69641=CARTESIAN_POINT('Ctrl Pts',(1.81394729834032,-1.,-3.75681965683995));
#69642=CARTESIAN_POINT('Ctrl Pts',(1.81394729834032,1.,-3.75681965683995));
#69643=CARTESIAN_POINT('Ctrl Pts',(1.80783603939662,-1.,-3.75193395888069));
#69644=CARTESIAN_POINT('Ctrl Pts',(1.80783603939662,1.,-3.75193395888069));
#69645=CARTESIAN_POINT('Ctrl Pts',(1.80175271485519,-1.,-3.74702700874954));
#69646=CARTESIAN_POINT('Ctrl Pts',(1.80175271485519,1.,-3.74702700874954));
#69647=CARTESIAN_POINT('Ctrl Pts',(1.79569757859041,-1.,-3.74209880351667));
#69648=CARTESIAN_POINT('Ctrl Pts',(1.79569757859041,1.,-3.74209880351667));
#69649=CARTESIAN_POINT('Ctrl Pts',(1.78967092823139,-1.,-3.73714934729962));
#69650=CARTESIAN_POINT('Ctrl Pts',(1.78967092823139,1.,-3.73714934729962));
#69651=CARTESIAN_POINT('Ctrl Pts',(1.78367308442682,-1.,-3.73217863095022));
#69652=CARTESIAN_POINT('Ctrl Pts',(1.78367308442682,1.,-3.73217863095022));
#69653=CARTESIAN_POINT('Ctrl Pts',(1.77770437039606,-1.,-3.72718661205504));
#69654=CARTESIAN_POINT('Ctrl Pts',(1.77770437039606,1.,-3.72718661205504));
#69655=CARTESIAN_POINT('Ctrl Pts',(1.77176509401846,-1.,-3.72217319911429));
#69656=CARTESIAN_POINT('Ctrl Pts',(1.77176509401846,1.,-3.72217319911429));
#69657=CARTESIAN_POINT('Ctrl Pts',(1.76585552124549,-1.,-3.71713822377676));
#69658=CARTESIAN_POINT('Ctrl Pts',(1.76585552124549,1.,-3.71713822377676));
#69659=CARTESIAN_POINT('Ctrl Pts',(1.75997588499021,-1.,-3.71208146346455));
#69660=CARTESIAN_POINT('Ctrl Pts',(1.75997588499021,1.,-3.71208146346455));
#69661=CARTESIAN_POINT('Ctrl Pts',(1.75412641804148,-1.,-3.70700269736876));
#69662=CARTESIAN_POINT('Ctrl Pts',(1.75412641804148,1.,-3.70700269736876));
#69663=CARTESIAN_POINT('Ctrl Pts',(1.74830738046092,-1.,-3.70190175673422));
#69664=CARTESIAN_POINT('Ctrl Pts',(1.74830738046092,1.,-3.70190175673422));
#69665=CARTESIAN_POINT('Ctrl Pts',(1.74251908492589,-1.,-3.6967785691046));
#69666=CARTESIAN_POINT('Ctrl Pts',(1.74251908492589,1.,-3.6967785691046));
#69667=CARTESIAN_POINT('Ctrl Pts',(1.73676193254493,-1.,-3.69163322647906));
#69668=CARTESIAN_POINT('Ctrl Pts',(1.73676193254493,1.,-3.69163322647906));
#69669=CARTESIAN_POINT('Ctrl Pts',(1.73103640956647,-1.,-3.68646597019188));
#69670=CARTESIAN_POINT('Ctrl Pts',(1.73103640956647,1.,-3.68646597019188));
#69671=CARTESIAN_POINT('Ctrl Pts',(1.72534302437003,-1.,-3.68127704936472));
#69672=CARTESIAN_POINT('Ctrl Pts',(1.72534302437003,1.,-3.68127704936472));
#69673=CARTESIAN_POINT('Ctrl Pts',(1.71968225581787,-1.,-3.67606660374665));
#69674=CARTESIAN_POINT('Ctrl Pts',(1.71968225581787,1.,-3.67606660374665));
#69675=CARTESIAN_POINT('Ctrl Pts',(1.71405450210392,-1.,-3.67083454901629));
#69676=CARTESIAN_POINT('Ctrl Pts',(1.71405450210392,1.,-3.67083454901629));
#69677=CARTESIAN_POINT('Ctrl Pts',(1.70846001610983,-1.,-3.6655804319893));
#69678=CARTESIAN_POINT('Ctrl Pts',(1.70846001610983,1.,-3.6655804319893));
#69679=CARTESIAN_POINT('Ctrl Pts',(1.70289888566904,-1.,-3.6603033877491));
#69680=CARTESIAN_POINT('Ctrl Pts',(1.70289888566904,1.,-3.6603033877491));
#69681=CARTESIAN_POINT('Ctrl Pts',(1.69737117722558,-1.,-3.65500246526798));
#69682=CARTESIAN_POINT('Ctrl Pts',(1.69737117722558,1.,-3.65500246526798));
#69683=CARTESIAN_POINT('Ctrl Pts',(1.691877054817,-1.,-3.64967689827393));
#69684=CARTESIAN_POINT('Ctrl Pts',(1.691877054817,1.,-3.64967689827393));
#69685=CARTESIAN_POINT('Ctrl Pts',(1.68641690471455,-1.,-3.64432638915199));
#69686=CARTESIAN_POINT('Ctrl Pts',(1.68641690471455,1.,-3.64432638915199));
#69687=CARTESIAN_POINT('Ctrl Pts',(1.68099146651577,-1.,-3.63895140887443));
#69688=CARTESIAN_POINT('Ctrl Pts',(1.68099146651577,1.,-3.63895140887443));
#69689=CARTESIAN_POINT('Ctrl Pts',(1.67560193613145,-1.,-3.63355343201211));
#69690=CARTESIAN_POINT('Ctrl Pts',(1.67560193613145,1.,-3.63355343201211));
#69691=CARTESIAN_POINT('Ctrl Pts',(1.67024966008037,-1.,-3.62813422105257));
#69692=CARTESIAN_POINT('Ctrl Pts',(1.67024966008037,1.,-3.62813422105257));
#69693=CARTESIAN_POINT('Ctrl Pts',(1.66493585923853,-1.,-3.62269517989104));
#69694=CARTESIAN_POINT('Ctrl Pts',(1.66493585923853,1.,-3.62269517989104));
#69695=CARTESIAN_POINT('Ctrl Pts',(1.65966133399186,-1.,-3.61723666482457));
#69696=CARTESIAN_POINT('Ctrl Pts',(1.65966133399186,1.,-3.61723666482457));
#69697=CARTESIAN_POINT('Ctrl Pts',(1.65442619244327,-1.,-3.61175734965129));
#69698=CARTESIAN_POINT('Ctrl Pts',(1.65442619244327,1.,-3.61175734965129));
#69699=CARTESIAN_POINT('Ctrl Pts',(1.64922952425833,-1.,-3.60625346556992));
#69700=CARTESIAN_POINT('Ctrl Pts',(1.64922952425833,1.,-3.60625346556992));
#69701=CARTESIAN_POINT('Ctrl Pts',(1.6440700438558,-1.,-3.6007202851384));
#69702=CARTESIAN_POINT('Ctrl Pts',(1.6440700438558,1.,-3.6007202851384));
#69703=CARTESIAN_POINT('Ctrl Pts',(1.63894676675349,-1.,-3.59515368334887));
#69704=CARTESIAN_POINT('Ctrl Pts',(1.63894676675349,1.,-3.59515368334887));
#69705=CARTESIAN_POINT('Ctrl Pts',(1.63385971451259,-1.,-3.58955176627876));
#69706=CARTESIAN_POINT('Ctrl Pts',(1.63385971451259,1.,-3.58955176627876));
#69707=CARTESIAN_POINT('Ctrl Pts',(1.62881051550748,-1.,-3.5839162577435));
#69708=CARTESIAN_POINT('Ctrl Pts',(1.62881051550748,1.,-3.5839162577435));
#69709=CARTESIAN_POINT('Ctrl Pts',(1.62380329464851,-1.,-3.57825455954405));
#69710=CARTESIAN_POINT('Ctrl Pts',(1.62380329464851,1.,-3.57825455954405));
#69711=CARTESIAN_POINT('Ctrl Pts',(1.61884340915412,-1.,-3.57257679609826));
#69712=CARTESIAN_POINT('Ctrl Pts',(1.61884340915412,1.,-3.57257679609826));
#69713=CARTESIAN_POINT('Ctrl Pts',(1.61393581747522,-1.,-3.56689200468404));
#69714=CARTESIAN_POINT('Ctrl Pts',(1.61393581747522,1.,-3.56689200468404));
#69715=CARTESIAN_POINT('Ctrl Pts',(1.60908344685459,-1.,-3.56120432482986));
#69716=CARTESIAN_POINT('Ctrl Pts',(1.60908344685459,1.,-3.56120432482986));
#69717=CARTESIAN_POINT('Ctrl Pts',(1.60428584699848,-1.,-3.55550985096117));
#69718=CARTESIAN_POINT('Ctrl Pts',(1.60428584699848,1.,-3.55550985096117));
#69719=CARTESIAN_POINT('Ctrl Pts',(1.59953698113444,-1.,-3.54979148634426));
#69720=CARTESIAN_POINT('Ctrl Pts',(1.59953698113444,1.,-3.54979148634426));
#69721=CARTESIAN_POINT('Ctrl Pts',(1.5948276694975,-1.,-3.544024581823));
#69722=CARTESIAN_POINT('Ctrl Pts',(1.5948276694975,1.,-3.544024581823));
#69723=CARTESIAN_POINT('Ctrl Pts',(1.59014958368725,-1.,-3.53818616861045));
#69724=CARTESIAN_POINT('Ctrl Pts',(1.59014958368725,1.,-3.53818616861045));
#69725=CARTESIAN_POINT('Ctrl Pts',(1.58549906268083,-1.,-3.53226378147068));
#69726=CARTESIAN_POINT('Ctrl Pts',(1.58549906268083,1.,-3.53226378147068));
#69727=CARTESIAN_POINT('Ctrl Pts',(1.58088027227856,-1.,-3.52626275334899));
#69728=CARTESIAN_POINT('Ctrl Pts',(1.58088027227856,1.,-3.52626275334899));
#69729=CARTESIAN_POINT('Ctrl Pts',(1.5763104998818,-1.,-3.52021847865961));
#69730=CARTESIAN_POINT('Ctrl Pts',(1.5763104998818,1.,-3.52021847865961));
#69731=CARTESIAN_POINT('Ctrl Pts',(1.57181569799774,-1.,-3.51418598431733));
#69732=CARTESIAN_POINT('Ctrl Pts',(1.57181569799774,1.,-3.51418598431733));
#69733=CARTESIAN_POINT('Ctrl Pts',(1.56742097575041,-1.,-3.50821771695427));
#69734=CARTESIAN_POINT('Ctrl Pts',(1.56742097575041,1.,-3.50821771695427));
#69735=CARTESIAN_POINT('Ctrl Pts',(1.56314187758689,-1.,-3.50234321621607));
#69736=CARTESIAN_POINT('Ctrl Pts',(1.56314187758689,1.,-3.50234321621607));
#69737=CARTESIAN_POINT('Ctrl Pts',(1.55897703097859,-1.,-3.49655185179623));
#69738=CARTESIAN_POINT('Ctrl Pts',(1.55897703097859,1.,-3.49655185179623));
#69739=CARTESIAN_POINT('Ctrl Pts',(1.5548959590107,-1.,-3.49076460877317));
#69740=CARTESIAN_POINT('Ctrl Pts',(1.5548959590107,1.,-3.49076460877317));
#69741=CARTESIAN_POINT('Ctrl Pts',(1.55084702970382,-1.,-3.48485155928414));
#69742=CARTESIAN_POINT('Ctrl Pts',(1.55084702970382,1.,-3.48485155928414));
#69743=CARTESIAN_POINT('Ctrl Pts',(1.54678009290206,-1.,-3.47868272898599));
#69744=CARTESIAN_POINT('Ctrl Pts',(1.54678009290206,1.,-3.47868272898599));
#69745=CARTESIAN_POINT('Ctrl Pts',(1.54266605398152,-1.,-3.47217189224576));
#69746=CARTESIAN_POINT('Ctrl Pts',(1.54266605398152,1.,-3.47217189224576));
#69747=CARTESIAN_POINT('Ctrl Pts',(1.53851507915533,-1.,-3.46531752207222));
#69748=CARTESIAN_POINT('Ctrl Pts',(1.53851507915533,1.,-3.46531752207222));
#69749=CARTESIAN_POINT('Ctrl Pts',(1.53440195378902,-1.,-3.45825932955273));
#69750=CARTESIAN_POINT('Ctrl Pts',(1.53440195378902,1.,-3.45825932955273));
#69751=CARTESIAN_POINT('Ctrl Pts',(1.530462444618,-1.,-3.45127136828667));
#69752=CARTESIAN_POINT('Ctrl Pts',(1.530462444618,1.,-3.45127136828667));
#69753=CARTESIAN_POINT('Ctrl Pts',(1.52686242875717,-1.,-3.44469547527));
#69754=CARTESIAN_POINT('Ctrl Pts',(1.52686242875717,1.,-3.44469547527));
#69755=CARTESIAN_POINT('Ctrl Pts',(1.52377348950429,-1.,-3.43888895974182));
#69756=CARTESIAN_POINT('Ctrl Pts',(1.52377348950429,1.,-3.43888895974182));
#69757=CARTESIAN_POINT('Ctrl Pts',(1.52134826724227,-1.,-3.43417156977749));
#69758=CARTESIAN_POINT('Ctrl Pts',(1.52134826724227,1.,-3.43417156977749));
#69759=CARTESIAN_POINT('Ctrl Pts',(1.51969006980792,-1.,-3.43076036253384));
#69760=CARTESIAN_POINT('Ctrl Pts',(1.51969006980792,1.,-3.43076036253384));
#69761=CARTESIAN_POINT('Ctrl Pts',(1.51901585838879,-1.,-3.42915787669388));
#69762=CARTESIAN_POINT('Ctrl Pts',(1.51901585838879,1.,-3.42915787669388));
#69763=CARTESIAN_POINT('Ctrl Pts',(1.51888450659497,-1.,-3.42860527148835));
#69764=CARTESIAN_POINT('Ctrl Pts',(1.51888450659497,1.,-3.42860527148835));
#69765=CARTESIAN_POINT('Ctrl Pts',(1.51896318668306,-1.,-3.42852521763648));
#69766=CARTESIAN_POINT('Ctrl Pts',(1.51896318668306,1.,-3.42852521763648));
#69767=CARTESIAN_POINT('Ctrl Pts',(1.519044091397,-1.,-3.42855728381368));
#69768=CARTESIAN_POINT('Ctrl Pts',(1.519044091397,1.,-3.42855728381368));
#69769=CARTESIAN_POINT('',(1.83867539237861,1.,-3.77614523045147));
#69770=CARTESIAN_POINT('Ctrl Pts',(1.83867539237861,1.,-3.77614523045147));
#69771=CARTESIAN_POINT('Ctrl Pts',(1.83742834010821,1.,-3.77518714458232));
#69772=CARTESIAN_POINT('Ctrl Pts',(1.83493697935064,1.,-3.77326886065484));
#69773=CARTESIAN_POINT('Ctrl Pts',(1.83120816956515,1.,-3.77038509819777));
#69774=CARTESIAN_POINT('Ctrl Pts',(1.82625289221933,1.,-3.76652740355856));
#69775=CARTESIAN_POINT('Ctrl Pts',(1.82008629694924,1.,-3.76168412709652));
#69776=CARTESIAN_POINT('Ctrl Pts',(1.81394729834032,1.,-3.75681965683995));
#69777=CARTESIAN_POINT('Ctrl Pts',(1.80783603939662,1.,-3.75193395888069));
#69778=CARTESIAN_POINT('Ctrl Pts',(1.80175271485519,1.,-3.74702700874954));
#69779=CARTESIAN_POINT('Ctrl Pts',(1.79569757859041,1.,-3.74209880351667));
#69780=CARTESIAN_POINT('Ctrl Pts',(1.78967092823139,1.,-3.73714934729962));
#69781=CARTESIAN_POINT('Ctrl Pts',(1.78367308442682,1.,-3.73217863095022));
#69782=CARTESIAN_POINT('Ctrl Pts',(1.77770437039606,1.,-3.72718661205504));
#69783=CARTESIAN_POINT('Ctrl Pts',(1.77176509401846,1.,-3.72217319911429));
#69784=CARTESIAN_POINT('Ctrl Pts',(1.76585552124549,1.,-3.71713822377676));
#69785=CARTESIAN_POINT('Ctrl Pts',(1.75997588499021,1.,-3.71208146346455));
#69786=CARTESIAN_POINT('Ctrl Pts',(1.75412641804148,1.,-3.70700269736876));
#69787=CARTESIAN_POINT('Ctrl Pts',(1.74830738046092,1.,-3.70190175673422));
#69788=CARTESIAN_POINT('Ctrl Pts',(1.74251908492589,1.,-3.6967785691046));
#69789=CARTESIAN_POINT('Ctrl Pts',(1.73676193254493,1.,-3.69163322647906));
#69790=CARTESIAN_POINT('Ctrl Pts',(1.73103640956647,1.,-3.68646597019188));
#69791=CARTESIAN_POINT('Ctrl Pts',(1.72534302437003,1.,-3.68127704936472));
#69792=CARTESIAN_POINT('Ctrl Pts',(1.71968225581787,1.,-3.67606660374665));
#69793=CARTESIAN_POINT('Ctrl Pts',(1.71405450210392,1.,-3.67083454901629));
#69794=CARTESIAN_POINT('Ctrl Pts',(1.70846001610983,1.,-3.6655804319893));
#69795=CARTESIAN_POINT('Ctrl Pts',(1.70289888566904,1.,-3.6603033877491));
#69796=CARTESIAN_POINT('Ctrl Pts',(1.69737117722558,1.,-3.65500246526798));
#69797=CARTESIAN_POINT('Ctrl Pts',(1.691877054817,1.,-3.64967689827393));
#69798=CARTESIAN_POINT('Ctrl Pts',(1.68641690471455,1.,-3.64432638915199));
#69799=CARTESIAN_POINT('Ctrl Pts',(1.68099146651577,1.,-3.63895140887443));
#69800=CARTESIAN_POINT('Ctrl Pts',(1.67560193613145,1.,-3.63355343201211));
#69801=CARTESIAN_POINT('Ctrl Pts',(1.67024966008037,1.,-3.62813422105257));
#69802=CARTESIAN_POINT('Ctrl Pts',(1.66493585923853,1.,-3.62269517989104));
#69803=CARTESIAN_POINT('Ctrl Pts',(1.65966133399186,1.,-3.61723666482457));
#69804=CARTESIAN_POINT('Ctrl Pts',(1.65442619244327,1.,-3.61175734965129));
#69805=CARTESIAN_POINT('Ctrl Pts',(1.64922952425833,1.,-3.60625346556992));
#69806=CARTESIAN_POINT('Ctrl Pts',(1.6440700438558,1.,-3.6007202851384));
#69807=CARTESIAN_POINT('Ctrl Pts',(1.63894676675349,1.,-3.59515368334887));
#69808=CARTESIAN_POINT('Ctrl Pts',(1.63385971451259,1.,-3.58955176627876));
#69809=CARTESIAN_POINT('Ctrl Pts',(1.62881051550748,1.,-3.5839162577435));
#69810=CARTESIAN_POINT('Ctrl Pts',(1.62380329464851,1.,-3.57825455954405));
#69811=CARTESIAN_POINT('Ctrl Pts',(1.61884340915412,1.,-3.57257679609826));
#69812=CARTESIAN_POINT('Ctrl Pts',(1.61393581747522,1.,-3.56689200468404));
#69813=CARTESIAN_POINT('Ctrl Pts',(1.60908344685459,1.,-3.56120432482986));
#69814=CARTESIAN_POINT('Ctrl Pts',(1.60428584699848,1.,-3.55550985096117));
#69815=CARTESIAN_POINT('Ctrl Pts',(1.59953698113444,1.,-3.54979148634426));
#69816=CARTESIAN_POINT('Ctrl Pts',(1.5948276694975,1.,-3.544024581823));
#69817=CARTESIAN_POINT('Ctrl Pts',(1.59014958368725,1.,-3.53818616861045));
#69818=CARTESIAN_POINT('Ctrl Pts',(1.58549906268083,1.,-3.53226378147068));
#69819=CARTESIAN_POINT('Ctrl Pts',(1.58088027227856,1.,-3.52626275334899));
#69820=CARTESIAN_POINT('Ctrl Pts',(1.5763104998818,1.,-3.52021847865961));
#69821=CARTESIAN_POINT('Ctrl Pts',(1.57181569799774,1.,-3.51418598431733));
#69822=CARTESIAN_POINT('Ctrl Pts',(1.56742097575041,1.,-3.50821771695427));
#69823=CARTESIAN_POINT('Ctrl Pts',(1.56314187758689,1.,-3.50234321621607));
#69824=CARTESIAN_POINT('Ctrl Pts',(1.55897703097859,1.,-3.49655185179623));
#69825=CARTESIAN_POINT('Ctrl Pts',(1.5548959590107,1.,-3.49076460877317));
#69826=CARTESIAN_POINT('Ctrl Pts',(1.55084702970382,1.,-3.48485155928414));
#69827=CARTESIAN_POINT('Ctrl Pts',(1.54678009290206,1.,-3.47868272898599));
#69828=CARTESIAN_POINT('Ctrl Pts',(1.54266605398152,1.,-3.47217189224576));
#69829=CARTESIAN_POINT('Ctrl Pts',(1.53851507915533,1.,-3.46531752207222));
#69830=CARTESIAN_POINT('Ctrl Pts',(1.53440195378902,1.,-3.45825932955273));
#69831=CARTESIAN_POINT('Ctrl Pts',(1.530462444618,1.,-3.45127136828667));
#69832=CARTESIAN_POINT('Ctrl Pts',(1.52686242875717,1.,-3.44469547527));
#69833=CARTESIAN_POINT('Ctrl Pts',(1.52377348950429,1.,-3.43888895974182));
#69834=CARTESIAN_POINT('Ctrl Pts',(1.52134826724227,1.,-3.43417156977749));
#69835=CARTESIAN_POINT('Ctrl Pts',(1.5198144909343,1.,-3.43101631893491));
#69836=CARTESIAN_POINT('Ctrl Pts',(1.51914806898539,1.,-3.42946838852728));
#69837=CARTESIAN_POINT('Ctrl Pts',(1.51895133295017,1.,-3.42884302333978));
#69838=CARTESIAN_POINT('Ctrl Pts',(1.51893924967231,1.,-3.42864616361967));
#69839=CARTESIAN_POINT('Ctrl Pts',(1.51895082866166,1.,-3.42859860294378));
#69840=CARTESIAN_POINT('',(1.83867539237861,0.,-3.77614523045147));
#69841=CARTESIAN_POINT('Ctrl Pts',(1.8808893942881,-1.,-3.24418789321065));
#69842=CARTESIAN_POINT('Ctrl Pts',(1.8808893942881,1.,-3.24418789321065));
#69843=CARTESIAN_POINT('Ctrl Pts',(1.8809110068042,-1.,-3.24410359189733));
#69844=CARTESIAN_POINT('Ctrl Pts',(1.8809110068042,1.,-3.24410359189733));
#69845=CARTESIAN_POINT('Ctrl Pts',(1.8810220187274,-1.,-3.24408699284449));
#69846=CARTESIAN_POINT('Ctrl Pts',(1.8810220187274,1.,-3.24408699284449));
#69847=CARTESIAN_POINT('Ctrl Pts',(1.88139187908347,-1.,-3.24451807186964));
#69848=CARTESIAN_POINT('Ctrl Pts',(1.88139187908347,1.,-3.24451807186964));
#69849=CARTESIAN_POINT('Ctrl Pts',(1.88229202583187,-1.,-3.24600543790876));
#69850=CARTESIAN_POINT('Ctrl Pts',(1.88229202583187,1.,-3.24600543790876));
#69851=CARTESIAN_POINT('Ctrl Pts',(1.88407708646435,-1.,-3.24935200512055));
#69852=CARTESIAN_POINT('Ctrl Pts',(1.88407708646435,1.,-3.24935200512055));
#69853=CARTESIAN_POINT('Ctrl Pts',(1.88646802523372,-1.,-3.25408686339298));
#69854=CARTESIAN_POINT('Ctrl Pts',(1.88646802523372,1.,-3.25408686339298));
#69855=CARTESIAN_POINT('Ctrl Pts',(1.88934996203508,-1.,-3.2599988519361));
#69856=CARTESIAN_POINT('Ctrl Pts',(1.88934996203508,1.,-3.2599988519361));
#69857=CARTESIAN_POINT('Ctrl Pts',(1.89255393500769,-1.,-3.2667765388833));
#69858=CARTESIAN_POINT('Ctrl Pts',(1.89255393500769,1.,-3.2667765388833));
#69859=CARTESIAN_POINT('Ctrl Pts',(1.89589172903662,-1.,-3.27407108932908));
#69860=CARTESIAN_POINT('Ctrl Pts',(1.89589172903662,1.,-3.27407108932908));
#69861=CARTESIAN_POINT('Ctrl Pts',(1.89918429230424,-1.,-3.28154737912287));
#69862=CARTESIAN_POINT('Ctrl Pts',(1.89918429230424,1.,-3.28154737912287));
#69863=CARTESIAN_POINT('Ctrl Pts',(1.9022897124757,-1.,-3.28893448600364));
#69864=CARTESIAN_POINT('Ctrl Pts',(1.9022897124757,1.,-3.28893448600364));
#69865=CARTESIAN_POINT('Ctrl Pts',(1.9051389186417,-1.,-3.29608978722258));
#69866=CARTESIAN_POINT('Ctrl Pts',(1.9051389186417,1.,-3.29608978722258));
#69867=CARTESIAN_POINT('Ctrl Pts',(1.90773912171424,-1.,-3.30300595568341));
#69868=CARTESIAN_POINT('Ctrl Pts',(1.90773912171424,1.,-3.30300595568341));
#69869=CARTESIAN_POINT('Ctrl Pts',(1.91014297830502,-1.,-3.30975721158694));
#69870=CARTESIAN_POINT('Ctrl Pts',(1.91014297830502,1.,-3.30975721158694));
#69871=CARTESIAN_POINT('Ctrl Pts',(1.91242616234459,-1.,-3.31646052426395));
#69872=CARTESIAN_POINT('Ctrl Pts',(1.91242616234459,1.,-3.31646052426395));
#69873=CARTESIAN_POINT('Ctrl Pts',(1.91466343916612,-1.,-3.32323403454507));
#69874=CARTESIAN_POINT('Ctrl Pts',(1.91466343916612,1.,-3.32323403454507));
#69875=CARTESIAN_POINT('Ctrl Pts',(1.91690081930297,-1.,-3.33014884257812));
#69876=CARTESIAN_POINT('Ctrl Pts',(1.91690081930297,1.,-3.33014884257812));
#69877=CARTESIAN_POINT('Ctrl Pts',(1.91914609610173,-1.,-3.33721230709948));
#69878=CARTESIAN_POINT('Ctrl Pts',(1.91914609610173,1.,-3.33721230709948));
#69879=CARTESIAN_POINT('Ctrl Pts',(1.92138450828378,-1.,-3.34439448941915));
#69880=CARTESIAN_POINT('Ctrl Pts',(1.92138450828378,1.,-3.34439448941915));
#69881=CARTESIAN_POINT('Ctrl Pts',(1.92358838440518,-1.,-3.35164424847207));
#69882=CARTESIAN_POINT('Ctrl Pts',(1.92358838440518,1.,-3.35164424847207));
#69883=CARTESIAN_POINT('Ctrl Pts',(1.92572846125763,-1.,-3.35890824422976));
#69884=CARTESIAN_POINT('Ctrl Pts',(1.92572846125763,1.,-3.35890824422976));
#69885=CARTESIAN_POINT('Ctrl Pts',(1.92778626543803,-1.,-3.36615168657597));
#69886=CARTESIAN_POINT('Ctrl Pts',(1.92778626543803,1.,-3.36615168657597));
#69887=CARTESIAN_POINT('Ctrl Pts',(1.92975993109897,-1.,-3.37336807068078));
#69888=CARTESIAN_POINT('Ctrl Pts',(1.92975993109897,1.,-3.37336807068078));
#69889=CARTESIAN_POINT('Ctrl Pts',(1.93165739093292,-1.,-3.38056768525577));
#69890=CARTESIAN_POINT('Ctrl Pts',(1.93165739093292,1.,-3.38056768525577));
#69891=CARTESIAN_POINT('Ctrl Pts',(1.93349233176794,-1.,-3.38777076883267));
#69892=CARTESIAN_POINT('Ctrl Pts',(1.93349233176794,1.,-3.38777076883267));
#69893=CARTESIAN_POINT('Ctrl Pts',(1.93527929945982,-1.,-3.39499923640789));
#69894=CARTESIAN_POINT('Ctrl Pts',(1.93527929945982,1.,-3.39499923640789));
#69895=CARTESIAN_POINT('Ctrl Pts',(1.93702857723089,-1.,-3.40226802104093));
#69896=CARTESIAN_POINT('Ctrl Pts',(1.93702857723089,1.,-3.40226802104093));
#69897=CARTESIAN_POINT('Ctrl Pts',(1.93874306008132,-1.,-3.40957978266623));
#69898=CARTESIAN_POINT('Ctrl Pts',(1.93874306008132,1.,-3.40957978266623));
#69899=CARTESIAN_POINT('Ctrl Pts',(1.94042111965237,-1.,-3.41692971994082));
#69900=CARTESIAN_POINT('Ctrl Pts',(1.94042111965237,1.,-3.41692971994082));
#69901=CARTESIAN_POINT('Ctrl Pts',(1.94205835913692,-1.,-3.42430850941497));
#69902=CARTESIAN_POINT('Ctrl Pts',(1.94205835913692,1.,-3.42430850941497));
#69903=CARTESIAN_POINT('Ctrl Pts',(1.94364973660285,-1.,-3.43170586602436));
#69904=CARTESIAN_POINT('Ctrl Pts',(1.94364973660285,1.,-3.43170586602436));
#69905=CARTESIAN_POINT('Ctrl Pts',(1.94519168842883,-1.,-3.43911410197693));
#69906=CARTESIAN_POINT('Ctrl Pts',(1.94519168842883,1.,-3.43911410197693));
#69907=CARTESIAN_POINT('Ctrl Pts',(1.94668377715332,-1.,-3.44653088665685));
#69908=CARTESIAN_POINT('Ctrl Pts',(1.94668377715332,1.,-3.44653088665685));
#69909=CARTESIAN_POINT('Ctrl Pts',(1.94812754766524,-1.,-3.45395731584051));
#69910=CARTESIAN_POINT('Ctrl Pts',(1.94812754766524,1.,-3.45395731584051));
#69911=CARTESIAN_POINT('Ctrl Pts',(1.94952575850196,-1.,-3.46139661060959));
#69912=CARTESIAN_POINT('Ctrl Pts',(1.94952575850196,1.,-3.46139661060959));
#69913=CARTESIAN_POINT('Ctrl Pts',(1.95088147859876,-1.,-3.4688525897419));
#69914=CARTESIAN_POINT('Ctrl Pts',(1.95088147859876,1.,-3.4688525897419));
#69915=CARTESIAN_POINT('Ctrl Pts',(1.95219722189878,-1.,-3.47632820495926));
#69916=CARTESIAN_POINT('Ctrl Pts',(1.95219722189878,1.,-3.47632820495926));
#69917=CARTESIAN_POINT('Ctrl Pts',(1.95347412486316,-1.,-3.48382414832649));
#69918=CARTESIAN_POINT('Ctrl Pts',(1.95347412486316,1.,-3.48382414832649));
#69919=CARTESIAN_POINT('Ctrl Pts',(1.95471236969653,-1.,-3.49133956289154));
#69920=CARTESIAN_POINT('Ctrl Pts',(1.95471236969653,1.,-3.49133956289154));
#69921=CARTESIAN_POINT('Ctrl Pts',(1.9559115382367,-1.,-3.49887263575602));
#69922=CARTESIAN_POINT('Ctrl Pts',(1.9559115382367,1.,-3.49887263575602));
#69923=CARTESIAN_POINT('Ctrl Pts',(1.95707099606513,-1.,-3.50642124159913));
#69924=CARTESIAN_POINT('Ctrl Pts',(1.95707099606513,1.,-3.50642124159913));
#69925=CARTESIAN_POINT('Ctrl Pts',(1.95819025316768,-1.,-3.51398354617773));
#69926=CARTESIAN_POINT('Ctrl Pts',(1.95819025316768,1.,-3.51398354617773));
#69927=CARTESIAN_POINT('Ctrl Pts',(1.95926936324436,-1.,-3.52155867431438));
#69928=CARTESIAN_POINT('Ctrl Pts',(1.95926936324436,1.,-3.52155867431438));
#69929=CARTESIAN_POINT('Ctrl Pts',(1.96030879411534,-1.,-3.52914648844289));
#69930=CARTESIAN_POINT('Ctrl Pts',(1.96030879411534,1.,-3.52914648844289));
#69931=CARTESIAN_POINT('Ctrl Pts',(1.96130926212661,-1.,-3.53674730625759));
#69932=CARTESIAN_POINT('Ctrl Pts',(1.96130926212661,1.,-3.53674730625759));
#69933=CARTESIAN_POINT('Ctrl Pts',(1.96227157573058,-1.,-3.54436163300425));
#69934=CARTESIAN_POINT('Ctrl Pts',(1.96227157573058,1.,-3.54436163300425));
#69935=CARTESIAN_POINT('Ctrl Pts',(1.96319648628667,-1.,-3.55198990600929));
#69936=CARTESIAN_POINT('Ctrl Pts',(1.96319648628667,1.,-3.55198990600929));
#69937=CARTESIAN_POINT('Ctrl Pts',(1.96408450906868,-1.,-3.55963218706201));
#69938=CARTESIAN_POINT('Ctrl Pts',(1.96408450906868,1.,-3.55963218706201));
#69939=CARTESIAN_POINT('Ctrl Pts',(1.96493594634643,-1.,-3.56728820357933));
#69940=CARTESIAN_POINT('Ctrl Pts',(1.96493594634643,1.,-3.56728820357933));
#69941=CARTESIAN_POINT('Ctrl Pts',(1.96575096652857,-1.,-3.57495748601088));
#69942=CARTESIAN_POINT('Ctrl Pts',(1.96575096652857,1.,-3.57495748601088));
#69943=CARTESIAN_POINT('Ctrl Pts',(1.9665296668894,-1.,-3.58263947663884));
#69944=CARTESIAN_POINT('Ctrl Pts',(1.9665296668894,1.,-3.58263947663884));
#69945=CARTESIAN_POINT('Ctrl Pts',(1.96727213799507,-1.,-3.5903336402273));
#69946=CARTESIAN_POINT('Ctrl Pts',(1.96727213799507,1.,-3.5903336402273));
#69947=CARTESIAN_POINT('Ctrl Pts',(1.96797854118257,-1.,-3.59803959819725));
#69948=CARTESIAN_POINT('Ctrl Pts',(1.96797854118257,1.,-3.59803959819725));
#69949=CARTESIAN_POINT('Ctrl Pts',(1.96864911885775,-1.,-3.60575714017676));
#69950=CARTESIAN_POINT('Ctrl Pts',(1.96864911885775,1.,-3.60575714017676));
#69951=CARTESIAN_POINT('Ctrl Pts',(1.96928416040712,-1.,-3.61348615496393));
#69952=CARTESIAN_POINT('Ctrl Pts',(1.96928416040712,1.,-3.61348615496393));
#69953=CARTESIAN_POINT('Ctrl Pts',(1.96988398129888,-1.,-3.62122658401722));
#69954=CARTESIAN_POINT('Ctrl Pts',(1.96988398129888,1.,-3.62122658401722));
#69955=CARTESIAN_POINT('Ctrl Pts',(1.97044889850518,-1.,-3.62897836973397));
#69956=CARTESIAN_POINT('Ctrl Pts',(1.97044889850518,1.,-3.62897836973397));
#69957=CARTESIAN_POINT('Ctrl Pts',(1.97097920454698,-1.,-3.63674139590853));
#69958=CARTESIAN_POINT('Ctrl Pts',(1.97097920454698,1.,-3.63674139590853));
#69959=CARTESIAN_POINT('Ctrl Pts',(1.97147515441539,-1.,-3.64451546724222));
#69960=CARTESIAN_POINT('Ctrl Pts',(1.97147515441539,1.,-3.64451546724222));
#69961=CARTESIAN_POINT('Ctrl Pts',(1.97193697240645,-1.,-3.65230034717364));
#69962=CARTESIAN_POINT('Ctrl Pts',(1.97193697240645,1.,-3.65230034717364));
#69963=CARTESIAN_POINT('Ctrl Pts',(1.97236485439317,-1.,-3.66009578166865));
#69964=CARTESIAN_POINT('Ctrl Pts',(1.97236485439317,1.,-3.66009578166865));
#69965=CARTESIAN_POINT('Ctrl Pts',(1.9727589719863,-1.,-3.66790152751984));
#69966=CARTESIAN_POINT('Ctrl Pts',(1.9727589719863,1.,-3.66790152751984));
#69967=CARTESIAN_POINT('Ctrl Pts',(1.97311947678035,-1.,-3.67571738106175));
#69968=CARTESIAN_POINT('Ctrl Pts',(1.97311947678035,1.,-3.67571738106175));
#69969=CARTESIAN_POINT('Ctrl Pts',(1.9734465030363,-1.,-3.68354319913416));
#69970=CARTESIAN_POINT('Ctrl Pts',(1.9734465030363,1.,-3.68354319913416));
#69971=CARTESIAN_POINT('Ctrl Pts',(1.97374016224397,-1.,-3.69137888597855));
#69972=CARTESIAN_POINT('Ctrl Pts',(1.97374016224397,1.,-3.69137888597855));
#69973=CARTESIAN_POINT('Ctrl Pts',(1.97394846382288,-1.,-3.69765528558292));
#69974=CARTESIAN_POINT('Ctrl Pts',(1.97394846382288,1.,-3.69765528558292));
#69975=CARTESIAN_POINT('Ctrl Pts',(1.97408973726149,-1.,-3.70236698911837));
#69976=CARTESIAN_POINT('Ctrl Pts',(1.97408973726149,1.,-3.70236698911837));
#69977=CARTESIAN_POINT('Ctrl Pts',(1.974177276451,-1.,-3.7055100813194));
#69978=CARTESIAN_POINT('Ctrl Pts',(1.974177276451,1.,-3.7055100813194));
#69979=CARTESIAN_POINT('Ctrl Pts',(1.97421938526992,-1.,-3.70708211654725));
#69980=CARTESIAN_POINT('Ctrl Pts',(1.97421938526992,1.,-3.70708211654725));
#69981=CARTESIAN_POINT('',(1.88097764062542,1.,-3.24413672884902));
#69982=CARTESIAN_POINT('Ctrl Pts',(1.88097764062541,-1.,-3.24413672884902));
#69983=CARTESIAN_POINT('Ctrl Pts',(1.88097764062541,-0.666666666666667,
-3.24413672884902));
#69984=CARTESIAN_POINT('Ctrl Pts',(1.88097764062541,-0.333333333333333,
-3.24413672884902));
#69985=CARTESIAN_POINT('Ctrl Pts',(1.88097764062541,0.333333333333333,-3.24413672884902));
#69986=CARTESIAN_POINT('Ctrl Pts',(1.88097764062541,0.666666666666667,-3.24413672884902));
#69987=CARTESIAN_POINT('Ctrl Pts',(1.88097764062541,1.,-3.24413672884902));
#69988=CARTESIAN_POINT('',(1.97421938526992,1.,-3.70708211654725));
#69989=CARTESIAN_POINT('',(1.97421938526992,0.,-3.70708211654725));
#69990=CARTESIAN_POINT('Ctrl Pts',(1.88097764062542,1.,-3.24413672884902));
#69991=CARTESIAN_POINT('Ctrl Pts',(1.88102292397987,1.,-3.24415531671311));
#69992=CARTESIAN_POINT('Ctrl Pts',(1.88117508446657,1.,-3.24428080352952));
#69993=CARTESIAN_POINT('Ctrl Pts',(1.88156537699118,1.,-3.24480754675942));
#69994=CARTESIAN_POINT('Ctrl Pts',(1.88242596600422,1.,-3.24625654410705));
#69995=CARTESIAN_POINT('Ctrl Pts',(1.88407708646435,1.,-3.24935200512055));
#69996=CARTESIAN_POINT('Ctrl Pts',(1.88646802523372,1.,-3.25408686339298));
#69997=CARTESIAN_POINT('Ctrl Pts',(1.88934996203508,1.,-3.2599988519361));
#69998=CARTESIAN_POINT('Ctrl Pts',(1.89255393500769,1.,-3.2667765388833));
#69999=CARTESIAN_POINT('Ctrl Pts',(1.89589172903662,1.,-3.27407108932908));
#70000=CARTESIAN_POINT('Ctrl Pts',(1.89918429230424,1.,-3.28154737912287));
#70001=CARTESIAN_POINT('Ctrl Pts',(1.9022897124757,1.,-3.28893448600364));
#70002=CARTESIAN_POINT('Ctrl Pts',(1.9051389186417,1.,-3.29608978722258));
#70003=CARTESIAN_POINT('Ctrl Pts',(1.90773912171424,1.,-3.30300595568341));
#70004=CARTESIAN_POINT('Ctrl Pts',(1.91014297830502,1.,-3.30975721158694));
#70005=CARTESIAN_POINT('Ctrl Pts',(1.91242616234459,1.,-3.31646052426395));
#70006=CARTESIAN_POINT('Ctrl Pts',(1.91466343916612,1.,-3.32323403454507));
#70007=CARTESIAN_POINT('Ctrl Pts',(1.91690081930297,1.,-3.33014884257812));
#70008=CARTESIAN_POINT('Ctrl Pts',(1.91914609610173,1.,-3.33721230709948));
#70009=CARTESIAN_POINT('Ctrl Pts',(1.92138450828378,1.,-3.34439448941915));
#70010=CARTESIAN_POINT('Ctrl Pts',(1.92358838440518,1.,-3.35164424847207));
#70011=CARTESIAN_POINT('Ctrl Pts',(1.92572846125763,1.,-3.35890824422976));
#70012=CARTESIAN_POINT('Ctrl Pts',(1.92778626543803,1.,-3.36615168657597));
#70013=CARTESIAN_POINT('Ctrl Pts',(1.92975993109897,1.,-3.37336807068078));
#70014=CARTESIAN_POINT('Ctrl Pts',(1.93165739093292,1.,-3.38056768525577));
#70015=CARTESIAN_POINT('Ctrl Pts',(1.93349233176794,1.,-3.38777076883267));
#70016=CARTESIAN_POINT('Ctrl Pts',(1.93527929945982,1.,-3.39499923640789));
#70017=CARTESIAN_POINT('Ctrl Pts',(1.93702857723089,1.,-3.40226802104093));
#70018=CARTESIAN_POINT('Ctrl Pts',(1.93874306008132,1.,-3.40957978266623));
#70019=CARTESIAN_POINT('Ctrl Pts',(1.94042111965237,1.,-3.41692971994082));
#70020=CARTESIAN_POINT('Ctrl Pts',(1.94205835913692,1.,-3.42430850941497));
#70021=CARTESIAN_POINT('Ctrl Pts',(1.94364973660285,1.,-3.43170586602436));
#70022=CARTESIAN_POINT('Ctrl Pts',(1.94519168842883,1.,-3.43911410197693));
#70023=CARTESIAN_POINT('Ctrl Pts',(1.94668377715332,1.,-3.44653088665685));
#70024=CARTESIAN_POINT('Ctrl Pts',(1.94812754766524,1.,-3.45395731584051));
#70025=CARTESIAN_POINT('Ctrl Pts',(1.94952575850196,1.,-3.46139661060959));
#70026=CARTESIAN_POINT('Ctrl Pts',(1.95088147859876,1.,-3.4688525897419));
#70027=CARTESIAN_POINT('Ctrl Pts',(1.95219722189878,1.,-3.47632820495926));
#70028=CARTESIAN_POINT('Ctrl Pts',(1.95347412486316,1.,-3.48382414832649));
#70029=CARTESIAN_POINT('Ctrl Pts',(1.95471236969653,1.,-3.49133956289154));
#70030=CARTESIAN_POINT('Ctrl Pts',(1.9559115382367,1.,-3.49887263575602));
#70031=CARTESIAN_POINT('Ctrl Pts',(1.95707099606513,1.,-3.50642124159913));
#70032=CARTESIAN_POINT('Ctrl Pts',(1.95819025316768,1.,-3.51398354617773));
#70033=CARTESIAN_POINT('Ctrl Pts',(1.95926936324436,1.,-3.52155867431438));
#70034=CARTESIAN_POINT('Ctrl Pts',(1.96030879411534,1.,-3.52914648844289));
#70035=CARTESIAN_POINT('Ctrl Pts',(1.96130926212661,1.,-3.53674730625759));
#70036=CARTESIAN_POINT('Ctrl Pts',(1.96227157573058,1.,-3.54436163300425));
#70037=CARTESIAN_POINT('Ctrl Pts',(1.96319648628667,1.,-3.55198990600929));
#70038=CARTESIAN_POINT('Ctrl Pts',(1.96408450906868,1.,-3.55963218706201));
#70039=CARTESIAN_POINT('Ctrl Pts',(1.96493594634643,1.,-3.56728820357933));
#70040=CARTESIAN_POINT('Ctrl Pts',(1.96575096652857,1.,-3.57495748601088));
#70041=CARTESIAN_POINT('Ctrl Pts',(1.9665296668894,1.,-3.58263947663884));
#70042=CARTESIAN_POINT('Ctrl Pts',(1.96727213799507,1.,-3.5903336402273));
#70043=CARTESIAN_POINT('Ctrl Pts',(1.96797854118257,1.,-3.59803959819725));
#70044=CARTESIAN_POINT('Ctrl Pts',(1.96864911885775,1.,-3.60575714017676));
#70045=CARTESIAN_POINT('Ctrl Pts',(1.96928416040712,1.,-3.61348615496393));
#70046=CARTESIAN_POINT('Ctrl Pts',(1.96988398129888,1.,-3.62122658401722));
#70047=CARTESIAN_POINT('Ctrl Pts',(1.97044889850518,1.,-3.62897836973397));
#70048=CARTESIAN_POINT('Ctrl Pts',(1.97097920454698,1.,-3.63674139590853));
#70049=CARTESIAN_POINT('Ctrl Pts',(1.97147515441539,1.,-3.64451546724222));
#70050=CARTESIAN_POINT('Ctrl Pts',(1.97193697240645,1.,-3.65230034717364));
#70051=CARTESIAN_POINT('Ctrl Pts',(1.97236485439317,1.,-3.66009578166865));
#70052=CARTESIAN_POINT('Ctrl Pts',(1.9727589719863,1.,-3.66790152751984));
#70053=CARTESIAN_POINT('Ctrl Pts',(1.97311947678035,1.,-3.67571738106175));
#70054=CARTESIAN_POINT('Ctrl Pts',(1.9734465030363,1.,-3.68354319913416));
#70055=CARTESIAN_POINT('Ctrl Pts',(1.97374016224397,1.,-3.69137888597855));
#70056=CARTESIAN_POINT('Ctrl Pts',(1.97394846382288,1.,-3.69765528558292));
#70057=CARTESIAN_POINT('Ctrl Pts',(1.97408973726149,1.,-3.70236698911837));
#70058=CARTESIAN_POINT('Ctrl Pts',(1.974177276451,1.,-3.7055100813194));
#70059=CARTESIAN_POINT('Ctrl Pts',(1.97421938526992,1.,-3.70708211654725));
#70060=CARTESIAN_POINT('Origin',(1.97421938526992,0.,-3.70708211654725));
#70061=CARTESIAN_POINT('',(1.83867539237861,1.,-3.77614523045147));
#70062=CARTESIAN_POINT('Origin',(0.,0.,0.));
#70063=CARTESIAN_POINT('',(2.03660101169564,1.,-3.14877060440425));
#70064=CARTESIAN_POINT('Origin',(0.,1.,0.));
#70065=CARTESIAN_POINT('Ctrl Pts',(2.03660101169564,1.,-3.14877060440425));
#70066=CARTESIAN_POINT('Ctrl Pts',(2.03660101169564,0.666666666666667,-3.14877060440425));
#70067=CARTESIAN_POINT('Ctrl Pts',(2.03660101169564,0.333333333333333,-3.14877060440425));
#70068=CARTESIAN_POINT('Ctrl Pts',(2.03660101169564,-0.333333333333333,
-3.14877060440425));
#70069=CARTESIAN_POINT('Ctrl Pts',(2.03660101169564,-0.666666666666667,
-3.14877060440425));
#70070=CARTESIAN_POINT('Ctrl Pts',(2.03660101169564,-1.,-3.14877060440425));
#70071=CARTESIAN_POINT('Ctrl Pts',(2.40675750623143,-1.,-3.44202241512147));
#70072=CARTESIAN_POINT('Ctrl Pts',(2.40675750623143,1.,-3.44202241512147));
#70073=CARTESIAN_POINT('Ctrl Pts',(2.40537592959345,-1.,-3.44127120683402));
#70074=CARTESIAN_POINT('Ctrl Pts',(2.40537592959345,1.,-3.44127120683402));
#70075=CARTESIAN_POINT('Ctrl Pts',(2.40261515590099,-1.,-3.43976627485223));
#70076=CARTESIAN_POINT('Ctrl Pts',(2.40261515590099,1.,-3.43976627485223));
#70077=CARTESIAN_POINT('Ctrl Pts',(2.39848113411428,-1.,-3.43750133066037));
#70078=CARTESIAN_POINT('Ctrl Pts',(2.39848113411428,1.,-3.43750133066037));
#70079=CARTESIAN_POINT('Ctrl Pts',(2.39298338805823,-1.,-3.43446630680436));
#70080=CARTESIAN_POINT('Ctrl Pts',(2.39298338805823,1.,-3.43446630680436));
#70081=CARTESIAN_POINT('Ctrl Pts',(2.38613505844641,-1.,-3.43064732714472));
#70082=CARTESIAN_POINT('Ctrl Pts',(2.38613505844641,1.,-3.43064732714472));
#70083=CARTESIAN_POINT('Ctrl Pts',(2.37931067029517,-1.,-3.42680309755241));
#70084=CARTESIAN_POINT('Ctrl Pts',(2.37931067029517,1.,-3.42680309755241));
#70085=CARTESIAN_POINT('Ctrl Pts',(2.37251035954351,-1.,-3.42293356216595));
#70086=CARTESIAN_POINT('Ctrl Pts',(2.37251035954351,1.,-3.42293356216595));
#70087=CARTESIAN_POINT('Ctrl Pts',(2.36573431470313,-1.,-3.41903866635384));
#70088=CARTESIAN_POINT('Ctrl Pts',(2.36573431470313,1.,-3.41903866635384));
#70089=CARTESIAN_POINT('Ctrl Pts',(2.35898278606449,-1.,-3.4151183675076));
#70090=CARTESIAN_POINT('Ctrl Pts',(2.35898278606449,1.,-3.4151183675076));
#70091=CARTESIAN_POINT('Ctrl Pts',(2.35225606823649,-1.,-3.41117262313464));
#70092=CARTESIAN_POINT('Ctrl Pts',(2.35225606823649,1.,-3.41117262313464));
#70093=CARTESIAN_POINT('Ctrl Pts',(2.34555447648901,-1.,-3.40720137403888));
#70094=CARTESIAN_POINT('Ctrl Pts',(2.34555447648901,1.,-3.40720137403888));
#70095=CARTESIAN_POINT('Ctrl Pts',(2.33887832342715,-1.,-3.40320452776646));
#70096=CARTESIAN_POINT('Ctrl Pts',(2.33887832342715,1.,-3.40320452776646));
#70097=CARTESIAN_POINT('Ctrl Pts',(2.33222789882601,-1.,-3.39918194578115));
#70098=CARTESIAN_POINT('Ctrl Pts',(2.33222789882601,1.,-3.39918194578115));
#70099=CARTESIAN_POINT('Ctrl Pts',(2.32560343902683,-1.,-3.39513342020045));
#70100=CARTESIAN_POINT('Ctrl Pts',(2.32560343902683,1.,-3.39513342020045));
#70101=CARTESIAN_POINT('Ctrl Pts',(2.31900513925627,-1.,-3.39105869475112));
#70102=CARTESIAN_POINT('Ctrl Pts',(2.31900513925627,1.,-3.39105869475112));
#70103=CARTESIAN_POINT('Ctrl Pts',(2.31243319489505,-1.,-3.38695751492659));
#70104=CARTESIAN_POINT('Ctrl Pts',(2.31243319489505,1.,-3.38695751492659));
#70105=CARTESIAN_POINT('Ctrl Pts',(2.30588783640389,-1.,-3.38282967336676));
#70106=CARTESIAN_POINT('Ctrl Pts',(2.30588783640389,1.,-3.38282967336676));
#70107=CARTESIAN_POINT('Ctrl Pts',(2.29936936127588,-1.,-3.37867504959382));
#70108=CARTESIAN_POINT('Ctrl Pts',(2.29936936127588,1.,-3.37867504959382));
#70109=CARTESIAN_POINT('Ctrl Pts',(2.2928781800731,-1.,-3.37449367172707));
#70110=CARTESIAN_POINT('Ctrl Pts',(2.2928781800731,1.,-3.37449367172707));
#70111=CARTESIAN_POINT('Ctrl Pts',(2.28641481081045,-1.,-3.37028570206357));
#70112=CARTESIAN_POINT('Ctrl Pts',(2.28641481081045,1.,-3.37028570206357));
#70113=CARTESIAN_POINT('Ctrl Pts',(2.27997979457968,-1.,-3.36605130712978));
#70114=CARTESIAN_POINT('Ctrl Pts',(2.27997979457968,1.,-3.36605130712978));
#70115=CARTESIAN_POINT('Ctrl Pts',(2.27357362620902,-1.,-3.36179055004369));
#70116=CARTESIAN_POINT('Ctrl Pts',(2.27357362620902,1.,-3.36179055004369));
#70117=CARTESIAN_POINT('Ctrl Pts',(2.26719668579921,-1.,-3.35750328523077));
#70118=CARTESIAN_POINT('Ctrl Pts',(2.26719668579921,1.,-3.35750328523077));
#70119=CARTESIAN_POINT('Ctrl Pts',(2.26084915222484,-1.,-3.35318902552676));
#70120=CARTESIAN_POINT('Ctrl Pts',(2.26084915222484,1.,-3.35318902552676));
#70121=CARTESIAN_POINT('Ctrl Pts',(2.25453097693524,-1.,-3.34884690292342));
#70122=CARTESIAN_POINT('Ctrl Pts',(2.25453097693524,1.,-3.34884690292342));
#70123=CARTESIAN_POINT('Ctrl Pts',(2.24824207678287,-1.,-3.34447596770768));
#70124=CARTESIAN_POINT('Ctrl Pts',(2.24824207678287,1.,-3.34447596770768));
#70125=CARTESIAN_POINT('Ctrl Pts',(2.24198249391437,-1.,-3.34007543738044));
#70126=CARTESIAN_POINT('Ctrl Pts',(2.24198249391437,1.,-3.34007543738044));
#70127=CARTESIAN_POINT('Ctrl Pts',(2.23575256328809,-1.,-3.33564495756478));
#70128=CARTESIAN_POINT('Ctrl Pts',(2.23575256328809,1.,-3.33564495756478));
#70129=CARTESIAN_POINT('Ctrl Pts',(2.22955308907221,-1.,-3.33118487773593));
#70130=CARTESIAN_POINT('Ctrl Pts',(2.22955308907221,1.,-3.33118487773593));
#70131=CARTESIAN_POINT('Ctrl Pts',(2.22338548312758,-1.,-3.32669646722871));
#70132=CARTESIAN_POINT('Ctrl Pts',(2.22338548312758,1.,-3.32669646722871));
#70133=CARTESIAN_POINT('Ctrl Pts',(2.21725135110889,-1.,-3.32218125618955));
#70134=CARTESIAN_POINT('Ctrl Pts',(2.21725135110889,1.,-3.32218125618955));
#70135=CARTESIAN_POINT('Ctrl Pts',(2.21115211847872,-1.,-3.31764044024231));
#70136=CARTESIAN_POINT('Ctrl Pts',(2.21115211847872,1.,-3.31764044024231));
#70137=CARTESIAN_POINT('Ctrl Pts',(2.20508863150608,-1.,-3.3130742460895));
#70138=CARTESIAN_POINT('Ctrl Pts',(2.20508863150608,1.,-3.3130742460895));
#70139=CARTESIAN_POINT('Ctrl Pts',(2.19906078949924,-1.,-3.30848134694597));
#70140=CARTESIAN_POINT('Ctrl Pts',(2.19906078949924,1.,-3.30848134694597));
#70141=CARTESIAN_POINT('Ctrl Pts',(2.19306710376112,-1.,-3.30385816281831));
#70142=CARTESIAN_POINT('Ctrl Pts',(2.19306710376112,1.,-3.30385816281831));
#70143=CARTESIAN_POINT('Ctrl Pts',(2.18710556500325,-1.,-3.29920022557635));
#70144=CARTESIAN_POINT('Ctrl Pts',(2.18710556500325,1.,-3.29920022557635));
#70145=CARTESIAN_POINT('Ctrl Pts',(2.18117455557062,-1.,-3.29450361500484));
#70146=CARTESIAN_POINT('Ctrl Pts',(2.18117455557062,1.,-3.29450361500484));
#70147=CARTESIAN_POINT('Ctrl Pts',(2.17527380048422,-1.,-3.28976645712566));
#70148=CARTESIAN_POINT('Ctrl Pts',(2.17527380048422,1.,-3.28976645712566));
#70149=CARTESIAN_POINT('Ctrl Pts',(2.16940517773459,-1.,-3.2849901997973));
#70150=CARTESIAN_POINT('Ctrl Pts',(2.16940517773459,1.,-3.2849901997973));
#70151=CARTESIAN_POINT('Ctrl Pts',(2.16357391934434,-1.,-3.28018150841414));
#70152=CARTESIAN_POINT('Ctrl Pts',(2.16357391934434,1.,-3.28018150841414));
#70153=CARTESIAN_POINT('Ctrl Pts',(2.15778690038359,-1.,-3.27534954469206));
#70154=CARTESIAN_POINT('Ctrl Pts',(2.15778690038359,1.,-3.27534954469206));
#70155=CARTESIAN_POINT('Ctrl Pts',(2.15205043199818,-1.,-3.27050245897244));
#70156=CARTESIAN_POINT('Ctrl Pts',(2.15205043199818,1.,-3.27050245897244));
#70157=CARTESIAN_POINT('Ctrl Pts',(2.14636805295663,-1.,-3.26564388189764));
#70158=CARTESIAN_POINT('Ctrl Pts',(2.14636805295663,1.,-3.26564388189764));
#70159=CARTESIAN_POINT('Ctrl Pts',(2.14073870754257,-1.,-3.26077002641868));
#70160=CARTESIAN_POINT('Ctrl Pts',(2.14073870754257,1.,-3.26077002641868));
#70161=CARTESIAN_POINT('Ctrl Pts',(2.13515375878786,-1.,-3.25586495065027));
#70162=CARTESIAN_POINT('Ctrl Pts',(2.13515375878786,1.,-3.25586495065027));
#70163=CARTESIAN_POINT('Ctrl Pts',(2.1296002839681,-1.,-3.25090574493994));
#70164=CARTESIAN_POINT('Ctrl Pts',(2.1296002839681,1.,-3.25090574493994));
#70165=CARTESIAN_POINT('Ctrl Pts',(2.12406646410943,-1.,-3.24587102613347));
#70166=CARTESIAN_POINT('Ctrl Pts',(2.12406646410943,1.,-3.24587102613347));
#70167=CARTESIAN_POINT('Ctrl Pts',(2.11854673326972,-1.,-3.24074905517282));
#70168=CARTESIAN_POINT('Ctrl Pts',(2.11854673326972,1.,-3.24074905517282));
#70169=CARTESIAN_POINT('Ctrl Pts',(2.11304604021784,-1.,-3.23554444767115));
#70170=CARTESIAN_POINT('Ctrl Pts',(2.11304604021784,1.,-3.23554444767115));
#70171=CARTESIAN_POINT('Ctrl Pts',(2.1075869964248,-1.,-3.23028945793334));
#70172=CARTESIAN_POINT('Ctrl Pts',(2.1075869964248,1.,-3.23028945793334));
#70173=CARTESIAN_POINT('Ctrl Pts',(2.10220384298533,-1.,-3.22503437553496));
#70174=CARTESIAN_POINT('Ctrl Pts',(2.10220384298533,1.,-3.22503437553496));
#70175=CARTESIAN_POINT('Ctrl Pts',(2.09692958434933,-1.,-3.21982707347067));
#70176=CARTESIAN_POINT('Ctrl Pts',(2.09692958434933,1.,-3.21982707347067));
#70177=CARTESIAN_POINT('Ctrl Pts',(2.0917841946046,-1.,-3.2146942960168));
#70178=CARTESIAN_POINT('Ctrl Pts',(2.0917841946046,1.,-3.2146942960168));
#70179=CARTESIAN_POINT('Ctrl Pts',(2.08676465517435,-1.,-3.20962575845433));
#70180=CARTESIAN_POINT('Ctrl Pts',(2.08676465517435,1.,-3.20962575845433));
#70181=CARTESIAN_POINT('Ctrl Pts',(2.08182850370816,-1.,-3.20454818630635));
#70182=CARTESIAN_POINT('Ctrl Pts',(2.08182850370816,1.,-3.20454818630635));
#70183=CARTESIAN_POINT('Ctrl Pts',(2.0769044187063,-1.,-3.19934132835879));
#70184=CARTESIAN_POINT('Ctrl Pts',(2.0769044187063,1.,-3.19934132835879));
#70185=CARTESIAN_POINT('Ctrl Pts',(2.07192253497765,-1.,-3.19388465568113));
#70186=CARTESIAN_POINT('Ctrl Pts',(2.07192253497765,1.,-3.19388465568113));
#70187=CARTESIAN_POINT('Ctrl Pts',(2.06684062744065,-1.,-3.18809755562297));
#70188=CARTESIAN_POINT('Ctrl Pts',(2.06684062744065,1.,-3.18809755562297));
#70189=CARTESIAN_POINT('Ctrl Pts',(2.06166849827143,-1.,-3.18197692964677));
#70190=CARTESIAN_POINT('Ctrl Pts',(2.06166849827143,1.,-3.18197692964677));
#70191=CARTESIAN_POINT('Ctrl Pts',(2.05650186773279,-1.,-3.17564906975592));
#70192=CARTESIAN_POINT('Ctrl Pts',(2.05650186773279,1.,-3.17564906975592));
#70193=CARTESIAN_POINT('Ctrl Pts',(2.05151770247452,-1.,-3.16936341689859));
#70194=CARTESIAN_POINT('Ctrl Pts',(2.05151770247452,1.,-3.16936341689859));
#70195=CARTESIAN_POINT('Ctrl Pts',(2.0469333124766,-1.,-3.16343165059235));
#70196=CARTESIAN_POINT('Ctrl Pts',(2.0469333124766,1.,-3.16343165059235));
#70197=CARTESIAN_POINT('Ctrl Pts',(2.04297406404132,-1.,-3.15817983946525));
#70198=CARTESIAN_POINT('Ctrl Pts',(2.04297406404132,1.,-3.15817983946525));
#70199=CARTESIAN_POINT('Ctrl Pts',(2.03984073791432,-1.,-3.1538999167466));
#70200=CARTESIAN_POINT('Ctrl Pts',(2.03984073791432,1.,-3.1538999167466));
#70201=CARTESIAN_POINT('Ctrl Pts',(2.03766932526171,-1.,-3.15079010635326));
#70202=CARTESIAN_POINT('Ctrl Pts',(2.03766932526171,1.,-3.15079010635326));
#70203=CARTESIAN_POINT('Ctrl Pts',(2.03675273048882,-1.,-3.14931281967585));
#70204=CARTESIAN_POINT('Ctrl Pts',(2.03675273048882,1.,-3.14931281967585));
#70205=CARTESIAN_POINT('Ctrl Pts',(2.03653654935384,-1.,-3.14878756590499));
#70206=CARTESIAN_POINT('Ctrl Pts',(2.03653654935384,1.,-3.14878756590499));
#70207=CARTESIAN_POINT('Ctrl Pts',(2.036601737578,-1.,-3.14869618937139));
#70208=CARTESIAN_POINT('Ctrl Pts',(2.036601737578,1.,-3.14869618937139));
#70209=CARTESIAN_POINT('Ctrl Pts',(2.03668666247593,-1.,-3.1487152044751));
#70210=CARTESIAN_POINT('Ctrl Pts',(2.03668666247593,1.,-3.1487152044751));
#70211=CARTESIAN_POINT('',(2.40675750623143,1.,-3.44202241512147));
#70212=CARTESIAN_POINT('Ctrl Pts',(2.40675750623143,1.,-3.44202241512147));
#70213=CARTESIAN_POINT('Ctrl Pts',(2.40537592959345,1.,-3.44127120683402));
#70214=CARTESIAN_POINT('Ctrl Pts',(2.40261515590099,1.,-3.43976627485223));
#70215=CARTESIAN_POINT('Ctrl Pts',(2.39848113411428,1.,-3.43750133066037));
#70216=CARTESIAN_POINT('Ctrl Pts',(2.39298338805823,1.,-3.43446630680436));
#70217=CARTESIAN_POINT('Ctrl Pts',(2.38613505844641,1.,-3.43064732714472));
#70218=CARTESIAN_POINT('Ctrl Pts',(2.37931067029517,1.,-3.42680309755241));
#70219=CARTESIAN_POINT('Ctrl Pts',(2.37251035954351,1.,-3.42293356216595));
#70220=CARTESIAN_POINT('Ctrl Pts',(2.36573431470313,1.,-3.41903866635384));
#70221=CARTESIAN_POINT('Ctrl Pts',(2.35898278606449,1.,-3.4151183675076));
#70222=CARTESIAN_POINT('Ctrl Pts',(2.35225606823649,1.,-3.41117262313464));
#70223=CARTESIAN_POINT('Ctrl Pts',(2.34555447648901,1.,-3.40720137403888));
#70224=CARTESIAN_POINT('Ctrl Pts',(2.33887832342715,1.,-3.40320452776646));
#70225=CARTESIAN_POINT('Ctrl Pts',(2.33222789882601,1.,-3.39918194578115));
#70226=CARTESIAN_POINT('Ctrl Pts',(2.32560343902683,1.,-3.39513342020045));
#70227=CARTESIAN_POINT('Ctrl Pts',(2.31900513925627,1.,-3.39105869475112));
#70228=CARTESIAN_POINT('Ctrl Pts',(2.31243319489505,1.,-3.38695751492659));
#70229=CARTESIAN_POINT('Ctrl Pts',(2.30588783640389,1.,-3.38282967336676));
#70230=CARTESIAN_POINT('Ctrl Pts',(2.29936936127588,1.,-3.37867504959382));
#70231=CARTESIAN_POINT('Ctrl Pts',(2.2928781800731,1.,-3.37449367172707));
#70232=CARTESIAN_POINT('Ctrl Pts',(2.28641481081045,1.,-3.37028570206357));
#70233=CARTESIAN_POINT('Ctrl Pts',(2.27997979457968,1.,-3.36605130712978));
#70234=CARTESIAN_POINT('Ctrl Pts',(2.27357362620902,1.,-3.36179055004369));
#70235=CARTESIAN_POINT('Ctrl Pts',(2.26719668579921,1.,-3.35750328523077));
#70236=CARTESIAN_POINT('Ctrl Pts',(2.26084915222484,1.,-3.35318902552676));
#70237=CARTESIAN_POINT('Ctrl Pts',(2.25453097693524,1.,-3.34884690292342));
#70238=CARTESIAN_POINT('Ctrl Pts',(2.24824207678287,1.,-3.34447596770768));
#70239=CARTESIAN_POINT('Ctrl Pts',(2.24198249391437,1.,-3.34007543738044));
#70240=CARTESIAN_POINT('Ctrl Pts',(2.23575256328809,1.,-3.33564495756478));
#70241=CARTESIAN_POINT('Ctrl Pts',(2.22955308907221,1.,-3.33118487773593));
#70242=CARTESIAN_POINT('Ctrl Pts',(2.22338548312758,1.,-3.32669646722871));
#70243=CARTESIAN_POINT('Ctrl Pts',(2.21725135110889,1.,-3.32218125618955));
#70244=CARTESIAN_POINT('Ctrl Pts',(2.21115211847872,1.,-3.31764044024231));
#70245=CARTESIAN_POINT('Ctrl Pts',(2.20508863150608,1.,-3.3130742460895));
#70246=CARTESIAN_POINT('Ctrl Pts',(2.19906078949924,1.,-3.30848134694597));
#70247=CARTESIAN_POINT('Ctrl Pts',(2.19306710376112,1.,-3.30385816281831));
#70248=CARTESIAN_POINT('Ctrl Pts',(2.18710556500325,1.,-3.29920022557635));
#70249=CARTESIAN_POINT('Ctrl Pts',(2.18117455557062,1.,-3.29450361500484));
#70250=CARTESIAN_POINT('Ctrl Pts',(2.17527380048422,1.,-3.28976645712566));
#70251=CARTESIAN_POINT('Ctrl Pts',(2.16940517773459,1.,-3.2849901997973));
#70252=CARTESIAN_POINT('Ctrl Pts',(2.16357391934434,1.,-3.28018150841414));
#70253=CARTESIAN_POINT('Ctrl Pts',(2.15778690038359,1.,-3.27534954469206));
#70254=CARTESIAN_POINT('Ctrl Pts',(2.15205043199818,1.,-3.27050245897244));
#70255=CARTESIAN_POINT('Ctrl Pts',(2.14636805295663,1.,-3.26564388189764));
#70256=CARTESIAN_POINT('Ctrl Pts',(2.14073870754257,1.,-3.26077002641868));
#70257=CARTESIAN_POINT('Ctrl Pts',(2.13515375878786,1.,-3.25586495065027));
#70258=CARTESIAN_POINT('Ctrl Pts',(2.1296002839681,1.,-3.25090574493994));
#70259=CARTESIAN_POINT('Ctrl Pts',(2.12406646410943,1.,-3.24587102613347));
#70260=CARTESIAN_POINT('Ctrl Pts',(2.11854673326972,1.,-3.24074905517282));
#70261=CARTESIAN_POINT('Ctrl Pts',(2.11304604021784,1.,-3.23554444767115));
#70262=CARTESIAN_POINT('Ctrl Pts',(2.1075869964248,1.,-3.23028945793334));
#70263=CARTESIAN_POINT('Ctrl Pts',(2.10220384298533,1.,-3.22503437553496));
#70264=CARTESIAN_POINT('Ctrl Pts',(2.09692958434933,1.,-3.21982707347067));
#70265=CARTESIAN_POINT('Ctrl Pts',(2.0917841946046,1.,-3.2146942960168));
#70266=CARTESIAN_POINT('Ctrl Pts',(2.08676465517435,1.,-3.20962575845433));
#70267=CARTESIAN_POINT('Ctrl Pts',(2.08182850370816,1.,-3.20454818630635));
#70268=CARTESIAN_POINT('Ctrl Pts',(2.0769044187063,1.,-3.19934132835879));
#70269=CARTESIAN_POINT('Ctrl Pts',(2.07192253497765,1.,-3.19388465568113));
#70270=CARTESIAN_POINT('Ctrl Pts',(2.06684062744065,1.,-3.18809755562297));
#70271=CARTESIAN_POINT('Ctrl Pts',(2.06166849827143,1.,-3.18197692964677));
#70272=CARTESIAN_POINT('Ctrl Pts',(2.05650186773279,1.,-3.17564906975592));
#70273=CARTESIAN_POINT('Ctrl Pts',(2.05151770247452,1.,-3.16936341689859));
#70274=CARTESIAN_POINT('Ctrl Pts',(2.0469333124766,1.,-3.16343165059235));
#70275=CARTESIAN_POINT('Ctrl Pts',(2.04297406404132,1.,-3.15817983946525));
#70276=CARTESIAN_POINT('Ctrl Pts',(2.03984073791432,1.,-3.1538999167466));
#70277=CARTESIAN_POINT('Ctrl Pts',(2.03783225496023,1.,-3.15102344775396));
#70278=CARTESIAN_POINT('Ctrl Pts',(2.03693188810614,1.,-3.14959882629936));
#70279=CARTESIAN_POINT('Ctrl Pts',(2.03663974554941,1.,-3.14901193669147));
#70280=CARTESIAN_POINT('Ctrl Pts',(2.03659701539175,1.,-3.1488193908823));
#70281=CARTESIAN_POINT('Ctrl Pts',(2.03660101169564,1.,-3.14877060440425));
#70282=CARTESIAN_POINT('',(2.40675750623143,0.,-3.44202241512147));
#70283=CARTESIAN_POINT('Ctrl Pts',(2.36523532225181,-1.,-2.91001063062876));
#70284=CARTESIAN_POINT('Ctrl Pts',(2.36523532225181,1.,-2.91001063062876));
#70285=CARTESIAN_POINT('Ctrl Pts',(2.36524348105112,-1.,-2.90992398626211));
#70286=CARTESIAN_POINT('Ctrl Pts',(2.36524348105112,1.,-2.90992398626211));
#70287=CARTESIAN_POINT('Ctrl Pts',(2.36535052956938,-1.,-2.90989022548032));
#70288=CARTESIAN_POINT('Ctrl Pts',(2.36535052956938,1.,-2.90989022548032));
#70289=CARTESIAN_POINT('Ctrl Pts',(2.36578327194741,-1.,-2.91025813830041));
#70290=CARTESIAN_POINT('Ctrl Pts',(2.36578327194741,1.,-2.91025813830041));
#70291=CARTESIAN_POINT('Ctrl Pts',(2.36690501170627,-1.,-2.9115863784204));
#70292=CARTESIAN_POINT('Ctrl Pts',(2.36690501170627,1.,-2.9115863784204));
#70293=CARTESIAN_POINT('Ctrl Pts',(2.36919161373173,-1.,-2.9146124988314));
#70294=CARTESIAN_POINT('Ctrl Pts',(2.36919161373173,1.,-2.9146124988314));
#70295=CARTESIAN_POINT('Ctrl Pts',(2.37229381109821,-1.,-2.91891503791411));
#70296=CARTESIAN_POINT('Ctrl Pts',(2.37229381109821,1.,-2.91891503791411));
#70297=CARTESIAN_POINT('Ctrl Pts',(2.3760651052403,-1.,-2.92430340582608));
#70298=CARTESIAN_POINT('Ctrl Pts',(2.3760651052403,1.,-2.92430340582608));
#70299=CARTESIAN_POINT('Ctrl Pts',(2.38028989582073,-1.,-2.93049643640206));
#70300=CARTESIAN_POINT('Ctrl Pts',(2.38028989582073,1.,-2.93049643640206));
#70301=CARTESIAN_POINT('Ctrl Pts',(2.38472771516311,-1.,-2.93717903280391));
#70302=CARTESIAN_POINT('Ctrl Pts',(2.38472771516311,1.,-2.93717903280391));
#70303=CARTESIAN_POINT('Ctrl Pts',(2.38914929090759,-1.,-2.94404820669076));
#70304=CARTESIAN_POINT('Ctrl Pts',(2.38914929090759,1.,-2.94404820669076));
#70305=CARTESIAN_POINT('Ctrl Pts',(2.39337207631667,-1.,-2.95085857128439));
#70306=CARTESIAN_POINT('Ctrl Pts',(2.39337207631667,1.,-2.95085857128439));
#70307=CARTESIAN_POINT('Ctrl Pts',(2.39730553974516,-1.,-2.95748006482942));
#70308=CARTESIAN_POINT('Ctrl Pts',(2.39730553974516,1.,-2.95748006482942));
#70309=CARTESIAN_POINT('Ctrl Pts',(2.4009556571164,-1.,-2.96390432240312));
#70310=CARTESIAN_POINT('Ctrl Pts',(2.4009556571164,1.,-2.96390432240312));
#70311=CARTESIAN_POINT('Ctrl Pts',(2.40438604734919,-1.,-2.9701964131236));
#70312=CARTESIAN_POINT('Ctrl Pts',(2.40438604734919,1.,-2.9701964131236));
#70313=CARTESIAN_POINT('Ctrl Pts',(2.40768975073713,-1.,-2.97646002822422));
#70314=CARTESIAN_POINT('Ctrl Pts',(2.40768975073713,1.,-2.97646002822422));
#70315=CARTESIAN_POINT('Ctrl Pts',(2.41095909342571,-1.,-2.98280015815107));
#70316=CARTESIAN_POINT('Ctrl Pts',(2.41095909342571,1.,-2.98280015815107));
#70317=CARTESIAN_POINT('Ctrl Pts',(2.41425064199586,-1.,-2.98927983005796));
#70318=CARTESIAN_POINT('Ctrl Pts',(2.41425064199586,1.,-2.98927983005796));
#70319=CARTESIAN_POINT('Ctrl Pts',(2.41757324500514,-1.,-2.99590509293503));
#70320=CARTESIAN_POINT('Ctrl Pts',(2.41757324500514,1.,-2.99590509293503));
#70321=CARTESIAN_POINT('Ctrl Pts',(2.42090763946779,-1.,-3.00264868585996));
#70322=CARTESIAN_POINT('Ctrl Pts',(2.42090763946779,1.,-3.00264868585996));
#70323=CARTESIAN_POINT('Ctrl Pts',(2.42421849439613,-1.,-3.00946442616659));
#70324=CARTESIAN_POINT('Ctrl Pts',(2.42421849439613,1.,-3.00946442616659));
#70325=CARTESIAN_POINT('Ctrl Pts',(2.42746856264168,-1.,-3.01630420830504));
#70326=CARTESIAN_POINT('Ctrl Pts',(2.42746856264168,1.,-3.01630420830504));
#70327=CARTESIAN_POINT('Ctrl Pts',(2.43063415586637,-1.,-3.02313656036004));
#70328=CARTESIAN_POINT('Ctrl Pts',(2.43063415586637,1.,-3.02313656036004));
#70329=CARTESIAN_POINT('Ctrl Pts',(2.43371241361488,-1.,-3.02995534946978));
#70330=CARTESIAN_POINT('Ctrl Pts',(2.43371241361488,1.,-3.02995534946978));
#70331=CARTESIAN_POINT('Ctrl Pts',(2.43671278042414,-1.,-3.03676949672822));
#70332=CARTESIAN_POINT('Ctrl Pts',(2.43671278042414,1.,-3.03676949672822));
#70333=CARTESIAN_POINT('Ctrl Pts',(2.43965194061857,-1.,-3.04359685040555));
#70334=CARTESIAN_POINT('Ctrl Pts',(2.43965194061857,1.,-3.04359685040555));
#70335=CARTESIAN_POINT('Ctrl Pts',(2.44254768923105,-1.,-3.05045678021504));
#70336=CARTESIAN_POINT('Ctrl Pts',(2.44254768923105,1.,-3.05045678021504));
#70337=CARTESIAN_POINT('Ctrl Pts',(2.44541251892556,-1.,-3.05736242671506));
#70338=CARTESIAN_POINT('Ctrl Pts',(2.44541251892556,1.,-3.05736242671506));
#70339=CARTESIAN_POINT('Ctrl Pts',(2.44824970516543,-1.,-3.06431596421405));
#70340=CARTESIAN_POINT('Ctrl Pts',(2.44824970516543,1.,-3.06431596421405));
#70341=CARTESIAN_POINT('Ctrl Pts',(2.45105688854422,-1.,-3.07131290521297));
#70342=CARTESIAN_POINT('Ctrl Pts',(2.45105688854422,1.,-3.07131290521297));
#70343=CARTESIAN_POINT('Ctrl Pts',(2.4538282678779,-1.,-3.07834472886139));
#70344=CARTESIAN_POINT('Ctrl Pts',(2.4538282678779,1.,-3.07834472886139));
#70345=CARTESIAN_POINT('Ctrl Pts',(2.45655725437039,-1.,-3.08540206545315));
#70346=CARTESIAN_POINT('Ctrl Pts',(2.45655725437039,1.,-3.08540206545315));
#70347=CARTESIAN_POINT('Ctrl Pts',(2.4592391256388,-1.,-3.09247787931887));
#70348=CARTESIAN_POINT('Ctrl Pts',(2.4592391256388,1.,-3.09247787931887));
#70349=CARTESIAN_POINT('Ctrl Pts',(2.46187308501884,-1.,-3.09956993697052));
#70350=CARTESIAN_POINT('Ctrl Pts',(2.46187308501884,1.,-3.09956993697052));
#70351=CARTESIAN_POINT('Ctrl Pts',(2.46446082979646,-1.,-3.1066790790198));
#70352=CARTESIAN_POINT('Ctrl Pts',(2.46446082979646,1.,-3.1066790790198));
#70353=CARTESIAN_POINT('Ctrl Pts',(2.46700558843506,-1.,-3.11380805536122));
#70354=CARTESIAN_POINT('Ctrl Pts',(2.46700558843506,1.,-3.11380805536122));
#70355=CARTESIAN_POINT('Ctrl Pts',(2.46951098947469,-1.,-3.12096015766983));
#70356=CARTESIAN_POINT('Ctrl Pts',(2.46951098947469,1.,-3.12096015766983));
#70357=CARTESIAN_POINT('Ctrl Pts',(2.47197997765871,-1.,-3.12813790805952));
#70358=CARTESIAN_POINT('Ctrl Pts',(2.47197997765871,1.,-3.12813790805952));
#70359=CARTESIAN_POINT('Ctrl Pts',(2.47441378371932,-1.,-3.13534181229295));
#70360=CARTESIAN_POINT('Ctrl Pts',(2.47441378371932,1.,-3.13534181229295));
#70361=CARTESIAN_POINT('Ctrl Pts',(2.47681245356109,-1.,-3.1425709954655));
#70362=CARTESIAN_POINT('Ctrl Pts',(2.47681245356109,1.,-3.1425709954655));
#70363=CARTESIAN_POINT('Ctrl Pts',(2.47917529057029,-1.,-3.14982373241352));
#70364=CARTESIAN_POINT('Ctrl Pts',(2.47917529057029,1.,-3.14982373241352));
#70365=CARTESIAN_POINT('Ctrl Pts',(2.48150133566571,-1.,-3.15709802322739));
#70366=CARTESIAN_POINT('Ctrl Pts',(2.48150133566571,1.,-3.15709802322739));
#70367=CARTESIAN_POINT('Ctrl Pts',(2.48378981792725,-1.,-3.16439213290161));
#70368=CARTESIAN_POINT('Ctrl Pts',(2.48378981792725,1.,-3.16439213290161));
#70369=CARTESIAN_POINT('Ctrl Pts',(2.48604065348587,-1.,-3.17170518863313));
#70370=CARTESIAN_POINT('Ctrl Pts',(2.48604065348587,1.,-3.17170518863313));
#70371=CARTESIAN_POINT('Ctrl Pts',(2.48825428288201,-1.,-3.17903698136622));
#70372=CARTESIAN_POINT('Ctrl Pts',(2.48825428288201,1.,-3.17903698136622));
#70373=CARTESIAN_POINT('Ctrl Pts',(2.49043146334059,-1.,-3.18638771282266));
#70374=CARTESIAN_POINT('Ctrl Pts',(2.49043146334059,1.,-3.18638771282266));
#70375=CARTESIAN_POINT('Ctrl Pts',(2.49257307239848,-1.,-3.19375775555798));
#70376=CARTESIAN_POINT('Ctrl Pts',(2.49257307239848,1.,-3.19375775555798));
#70377=CARTESIAN_POINT('Ctrl Pts',(2.49467992057755,-1.,-3.20114742397588));
#70378=CARTESIAN_POINT('Ctrl Pts',(2.49467992057755,1.,-3.20114742397588));
#70379=CARTESIAN_POINT('Ctrl Pts',(2.4967525264737,-1.,-3.20855669849836));
#70380=CARTESIAN_POINT('Ctrl Pts',(2.4967525264737,1.,-3.20855669849836));
#70381=CARTESIAN_POINT('Ctrl Pts',(2.4987911459939,-1.,-3.21598526261286));
#70382=CARTESIAN_POINT('Ctrl Pts',(2.4987911459939,1.,-3.21598526261286));
#70383=CARTESIAN_POINT('Ctrl Pts',(2.50079587201957,-1.,-3.22343262620503));
#70384=CARTESIAN_POINT('Ctrl Pts',(2.50079587201957,1.,-3.22343262620503));
#70385=CARTESIAN_POINT('Ctrl Pts',(2.50276671338111,-1.,-3.23089822320646));
#70386=CARTESIAN_POINT('Ctrl Pts',(2.50276671338111,1.,-3.23089822320646));
#70387=CARTESIAN_POINT('Ctrl Pts',(2.5047036758003,-1.,-3.23838151080319));
#70388=CARTESIAN_POINT('Ctrl Pts',(2.5047036758003,1.,-3.23838151080319));
#70389=CARTESIAN_POINT('Ctrl Pts',(2.506606859405,-1.,-3.24588208983849));
#70390=CARTESIAN_POINT('Ctrl Pts',(2.506606859405,1.,-3.24588208983849));
#70391=CARTESIAN_POINT('Ctrl Pts',(2.50847647070723,-1.,-3.25339971460982));
#70392=CARTESIAN_POINT('Ctrl Pts',(2.50847647070723,1.,-3.25339971460982));
#70393=CARTESIAN_POINT('Ctrl Pts',(2.51031277813486,-1.,-3.26093423001434));
#70394=CARTESIAN_POINT('Ctrl Pts',(2.51031277813486,1.,-3.26093423001434));
#70395=CARTESIAN_POINT('Ctrl Pts',(2.51211608411423,-1.,-3.26848552888116));
#70396=CARTESIAN_POINT('Ctrl Pts',(2.51211608411423,1.,-3.26848552888116));
#70397=CARTESIAN_POINT('Ctrl Pts',(2.513886692704,-1.,-3.27605350473142));
#70398=CARTESIAN_POINT('Ctrl Pts',(2.513886692704,1.,-3.27605350473142));
#70399=CARTESIAN_POINT('Ctrl Pts',(2.51562487464514,-1.,-3.28363799702982));
#70400=CARTESIAN_POINT('Ctrl Pts',(2.51562487464514,1.,-3.28363799702982));
#70401=CARTESIAN_POINT('Ctrl Pts',(2.51733085123797,-1.,-3.2912387729927));
#70402=CARTESIAN_POINT('Ctrl Pts',(2.51733085123797,1.,-3.2912387729927));
#70403=CARTESIAN_POINT('Ctrl Pts',(2.51900480701068,-1.,-3.29885556388353));
#70404=CARTESIAN_POINT('Ctrl Pts',(2.51900480701068,1.,-3.29885556388353));
#70405=CARTESIAN_POINT('Ctrl Pts',(2.52064689568511,-1.,-3.30648808815443));
#70406=CARTESIAN_POINT('Ctrl Pts',(2.52064689568511,1.,-3.30648808815443));
#70407=CARTESIAN_POINT('Ctrl Pts',(2.52225724871313,-1.,-3.31413607874645));
#70408=CARTESIAN_POINT('Ctrl Pts',(2.52225724871313,1.,-3.31413607874645));
#70409=CARTESIAN_POINT('Ctrl Pts',(2.5238359839626,-1.,-3.32179931078699));
#70410=CARTESIAN_POINT('Ctrl Pts',(2.5238359839626,1.,-3.32179931078699));
#70411=CARTESIAN_POINT('Ctrl Pts',(2.52538321164634,-1.,-3.32947762187533));
#70412=CARTESIAN_POINT('Ctrl Pts',(2.52538321164634,1.,-3.32947762187533));
#70413=CARTESIAN_POINT('Ctrl Pts',(2.52689902690158,-1.,-3.33717089999103));
#70414=CARTESIAN_POINT('Ctrl Pts',(2.52689902690158,1.,-3.33717089999103));
#70415=CARTESIAN_POINT('Ctrl Pts',(2.52808660915689,-1.,-3.34333744115511));
#70416=CARTESIAN_POINT('Ctrl Pts',(2.52808660915689,1.,-3.34333744115511));
#70417=CARTESIAN_POINT('Ctrl Pts',(2.52896321610703,-1.,-3.34796903576663));
#70418=CARTESIAN_POINT('Ctrl Pts',(2.52896321610703,1.,-3.34796903576663));
#70419=CARTESIAN_POINT('Ctrl Pts',(2.5295413654909,-1.,-3.35105973714072));
#70420=CARTESIAN_POINT('Ctrl Pts',(2.5295413654909,1.,-3.35105973714072));
#70421=CARTESIAN_POINT('Ctrl Pts',(2.52982887637028,-1.,-3.35260583073571));
#70422=CARTESIAN_POINT('Ctrl Pts',(2.52982887637028,1.,-3.35260583073571));
#70423=CARTESIAN_POINT('',(2.36531447826073,1.,-2.90994629141676));
#70424=CARTESIAN_POINT('Ctrl Pts',(2.36531447826073,-1.,-2.90994629141676));
#70425=CARTESIAN_POINT('Ctrl Pts',(2.36531447826073,-0.666666666666667,
-2.90994629141676));
#70426=CARTESIAN_POINT('Ctrl Pts',(2.36531447826073,-0.333333333333333,
-2.90994629141676));
#70427=CARTESIAN_POINT('Ctrl Pts',(2.36531447826073,0.333333333333333,-2.90994629141676));
#70428=CARTESIAN_POINT('Ctrl Pts',(2.36531447826074,0.666666666666667,-2.90994629141676));
#70429=CARTESIAN_POINT('Ctrl Pts',(2.36531447826074,1.,-2.90994629141676));
#70430=CARTESIAN_POINT('',(2.52982887637028,1.,-3.35260583073571));
#70431=CARTESIAN_POINT('',(2.52982887637028,0.,-3.35260583073571));
#70432=CARTESIAN_POINT('Ctrl Pts',(2.36531447826073,1.,-2.90994629141676));
#70433=CARTESIAN_POINT('Ctrl Pts',(2.36536211188453,1.,-2.90995756655606));
#70434=CARTESIAN_POINT('Ctrl Pts',(2.36553202948613,1.,-2.91005770527719));
#70435=CARTESIAN_POINT('Ctrl Pts',(2.36599991765749,1.,-2.91051690822156));
#70436=CARTESIAN_POINT('Ctrl Pts',(2.36707658451664,1.,-2.91181344022548));
#70437=CARTESIAN_POINT('Ctrl Pts',(2.36919161373173,1.,-2.9146124988314));
#70438=CARTESIAN_POINT('Ctrl Pts',(2.37229381109821,1.,-2.91891503791411));
#70439=CARTESIAN_POINT('Ctrl Pts',(2.3760651052403,1.,-2.92430340582608));
#70440=CARTESIAN_POINT('Ctrl Pts',(2.38028989582073,1.,-2.93049643640206));
#70441=CARTESIAN_POINT('Ctrl Pts',(2.38472771516311,1.,-2.93717903280391));
#70442=CARTESIAN_POINT('Ctrl Pts',(2.38914929090759,1.,-2.94404820669076));
#70443=CARTESIAN_POINT('Ctrl Pts',(2.39337207631667,1.,-2.95085857128439));
#70444=CARTESIAN_POINT('Ctrl Pts',(2.39730553974516,1.,-2.95748006482942));
#70445=CARTESIAN_POINT('Ctrl Pts',(2.4009556571164,1.,-2.96390432240312));
#70446=CARTESIAN_POINT('Ctrl Pts',(2.40438604734919,1.,-2.9701964131236));
#70447=CARTESIAN_POINT('Ctrl Pts',(2.40768975073713,1.,-2.97646002822422));
#70448=CARTESIAN_POINT('Ctrl Pts',(2.41095909342571,1.,-2.98280015815107));
#70449=CARTESIAN_POINT('Ctrl Pts',(2.41425064199586,1.,-2.98927983005796));
#70450=CARTESIAN_POINT('Ctrl Pts',(2.41757324500514,1.,-2.99590509293503));
#70451=CARTESIAN_POINT('Ctrl Pts',(2.42090763946779,1.,-3.00264868585996));
#70452=CARTESIAN_POINT('Ctrl Pts',(2.42421849439613,1.,-3.00946442616659));
#70453=CARTESIAN_POINT('Ctrl Pts',(2.42746856264168,1.,-3.01630420830504));
#70454=CARTESIAN_POINT('Ctrl Pts',(2.43063415586637,1.,-3.02313656036004));
#70455=CARTESIAN_POINT('Ctrl Pts',(2.43371241361488,1.,-3.02995534946978));
#70456=CARTESIAN_POINT('Ctrl Pts',(2.43671278042414,1.,-3.03676949672822));
#70457=CARTESIAN_POINT('Ctrl Pts',(2.43965194061857,1.,-3.04359685040555));
#70458=CARTESIAN_POINT('Ctrl Pts',(2.44254768923105,1.,-3.05045678021504));
#70459=CARTESIAN_POINT('Ctrl Pts',(2.44541251892556,1.,-3.05736242671506));
#70460=CARTESIAN_POINT('Ctrl Pts',(2.44824970516543,1.,-3.06431596421405));
#70461=CARTESIAN_POINT('Ctrl Pts',(2.45105688854422,1.,-3.07131290521297));
#70462=CARTESIAN_POINT('Ctrl Pts',(2.4538282678779,1.,-3.07834472886139));
#70463=CARTESIAN_POINT('Ctrl Pts',(2.45655725437039,1.,-3.08540206545315));
#70464=CARTESIAN_POINT('Ctrl Pts',(2.4592391256388,1.,-3.09247787931887));
#70465=CARTESIAN_POINT('Ctrl Pts',(2.46187308501884,1.,-3.09956993697052));
#70466=CARTESIAN_POINT('Ctrl Pts',(2.46446082979646,1.,-3.1066790790198));
#70467=CARTESIAN_POINT('Ctrl Pts',(2.46700558843506,1.,-3.11380805536122));
#70468=CARTESIAN_POINT('Ctrl Pts',(2.46951098947469,1.,-3.12096015766983));
#70469=CARTESIAN_POINT('Ctrl Pts',(2.47197997765871,1.,-3.12813790805952));
#70470=CARTESIAN_POINT('Ctrl Pts',(2.47441378371932,1.,-3.13534181229295));
#70471=CARTESIAN_POINT('Ctrl Pts',(2.47681245356109,1.,-3.1425709954655));
#70472=CARTESIAN_POINT('Ctrl Pts',(2.47917529057029,1.,-3.14982373241352));
#70473=CARTESIAN_POINT('Ctrl Pts',(2.48150133566571,1.,-3.15709802322739));
#70474=CARTESIAN_POINT('Ctrl Pts',(2.48378981792725,1.,-3.16439213290161));
#70475=CARTESIAN_POINT('Ctrl Pts',(2.48604065348587,1.,-3.17170518863313));
#70476=CARTESIAN_POINT('Ctrl Pts',(2.48825428288201,1.,-3.17903698136622));
#70477=CARTESIAN_POINT('Ctrl Pts',(2.49043146334059,1.,-3.18638771282266));
#70478=CARTESIAN_POINT('Ctrl Pts',(2.49257307239848,1.,-3.19375775555798));
#70479=CARTESIAN_POINT('Ctrl Pts',(2.49467992057755,1.,-3.20114742397588));
#70480=CARTESIAN_POINT('Ctrl Pts',(2.4967525264737,1.,-3.20855669849836));
#70481=CARTESIAN_POINT('Ctrl Pts',(2.4987911459939,1.,-3.21598526261286));
#70482=CARTESIAN_POINT('Ctrl Pts',(2.50079587201957,1.,-3.22343262620503));
#70483=CARTESIAN_POINT('Ctrl Pts',(2.50276671338111,1.,-3.23089822320646));
#70484=CARTESIAN_POINT('Ctrl Pts',(2.5047036758003,1.,-3.23838151080319));
#70485=CARTESIAN_POINT('Ctrl Pts',(2.506606859405,1.,-3.24588208983849));
#70486=CARTESIAN_POINT('Ctrl Pts',(2.50847647070723,1.,-3.25339971460982));
#70487=CARTESIAN_POINT('Ctrl Pts',(2.51031277813486,1.,-3.26093423001434));
#70488=CARTESIAN_POINT('Ctrl Pts',(2.51211608411423,1.,-3.26848552888116));
#70489=CARTESIAN_POINT('Ctrl Pts',(2.513886692704,1.,-3.27605350473142));
#70490=CARTESIAN_POINT('Ctrl Pts',(2.51562487464514,1.,-3.28363799702982));
#70491=CARTESIAN_POINT('Ctrl Pts',(2.51733085123797,1.,-3.2912387729927));
#70492=CARTESIAN_POINT('Ctrl Pts',(2.51900480701068,1.,-3.29885556388353));
#70493=CARTESIAN_POINT('Ctrl Pts',(2.52064689568511,1.,-3.30648808815443));
#70494=CARTESIAN_POINT('Ctrl Pts',(2.52225724871313,1.,-3.31413607874645));
#70495=CARTESIAN_POINT('Ctrl Pts',(2.5238359839626,1.,-3.32179931078699));
#70496=CARTESIAN_POINT('Ctrl Pts',(2.52538321164634,1.,-3.32947762187533));
#70497=CARTESIAN_POINT('Ctrl Pts',(2.52689902690158,1.,-3.33717089999103));
#70498=CARTESIAN_POINT('Ctrl Pts',(2.52808660915689,1.,-3.34333744115511));
#70499=CARTESIAN_POINT('Ctrl Pts',(2.52896321610703,1.,-3.34796903576663));
#70500=CARTESIAN_POINT('Ctrl Pts',(2.5295413654909,1.,-3.35105973714072));
#70501=CARTESIAN_POINT('Ctrl Pts',(2.52982887637028,1.,-3.35260583073571));
#70502=CARTESIAN_POINT('Origin',(2.52982887637028,0.,-3.35260583073571));
#70503=CARTESIAN_POINT('',(2.40675750623143,1.,-3.44202241512147));
#70504=CARTESIAN_POINT('Origin',(0.,0.,0.));
#70505=CARTESIAN_POINT('',(2.50410331873042,1.,-2.79140942341378));
#70506=CARTESIAN_POINT('Origin',(0.,1.,0.));
#70507=CARTESIAN_POINT('Ctrl Pts',(2.50410331873042,1.,-2.79140942341378));
#70508=CARTESIAN_POINT('Ctrl Pts',(2.50410331873042,0.666666666666667,-2.79140942341378));
#70509=CARTESIAN_POINT('Ctrl Pts',(2.50410331873042,0.333333333333333,-2.79140942341378));
#70510=CARTESIAN_POINT('Ctrl Pts',(2.50410331873042,-0.333333333333333,
-2.79140942341378));
#70511=CARTESIAN_POINT('Ctrl Pts',(2.50410331873042,-0.666666666666667,
-2.79140942341378));
#70512=CARTESIAN_POINT('Ctrl Pts',(2.50410331873042,-1.,-2.79140942341378));
#70513=CARTESIAN_POINT('Ctrl Pts',(2.91557726271063,-1.,-3.02314558451372));
#70514=CARTESIAN_POINT('Ctrl Pts',(2.91557726271063,1.,-3.02314558451372));
#70515=CARTESIAN_POINT('Ctrl Pts',(2.91409518070707,-1.,-3.02261975104912));
#70516=CARTESIAN_POINT('Ctrl Pts',(2.91409518070707,1.,-3.02261975104912));
#70517=CARTESIAN_POINT('Ctrl Pts',(2.91113297349052,-1.,-3.02156522743299));
#70518=CARTESIAN_POINT('Ctrl Pts',(2.91113297349052,1.,-3.02156522743299));
#70519=CARTESIAN_POINT('Ctrl Pts',(2.90669553303902,-1.,-3.01997487194926));
#70520=CARTESIAN_POINT('Ctrl Pts',(2.90669553303902,1.,-3.01997487194926));
#70521=CARTESIAN_POINT('Ctrl Pts',(2.90079069102661,-1.,-3.01783725123646));
#70522=CARTESIAN_POINT('Ctrl Pts',(2.90079069102661,1.,-3.01783725123646));
#70523=CARTESIAN_POINT('Ctrl Pts',(2.8934292556764,-1.,-3.01513660433291));
#70524=CARTESIAN_POINT('Ctrl Pts',(2.8934292556764,1.,-3.01513660433291));
#70525=CARTESIAN_POINT('Ctrl Pts',(2.88608751706796,-1.,-3.01240727309568));
#70526=CARTESIAN_POINT('Ctrl Pts',(2.88608751706796,1.,-3.01240727309568));
#70527=CARTESIAN_POINT('Ctrl Pts',(2.87876560072799,-1.,-3.0096491810855));
#70528=CARTESIAN_POINT('Ctrl Pts',(2.87876560072799,1.,-3.0096491810855));
#70529=CARTESIAN_POINT('Ctrl Pts',(2.87146368430104,-1.,-3.00686224485374));
#70530=CARTESIAN_POINT('Ctrl Pts',(2.87146368430104,1.,-3.00686224485374));
#70531=CARTESIAN_POINT('Ctrl Pts',(2.86418200833065,-1.,-3.00404638316245));
#70532=CARTESIAN_POINT('Ctrl Pts',(2.86418200833065,1.,-3.00404638316245));
#70533=CARTESIAN_POINT('Ctrl Pts',(2.85692085715129,-1.,-3.0012015079552));
#70534=CARTESIAN_POINT('Ctrl Pts',(2.85692085715129,1.,-3.0012015079552));
#70535=CARTESIAN_POINT('Ctrl Pts',(2.84968053289104,-1.,-2.99832751144566));
#70536=CARTESIAN_POINT('Ctrl Pts',(2.84968053289104,1.,-2.99832751144566));
#70537=CARTESIAN_POINT('Ctrl Pts',(2.84246132984334,-1.,-2.995424253416));
#70538=CARTESIAN_POINT('Ctrl Pts',(2.84246132984334,1.,-2.995424253416));
#70539=CARTESIAN_POINT('Ctrl Pts',(2.83526351254383,-1.,-2.99249155170479));
#70540=CARTESIAN_POINT('Ctrl Pts',(2.83526351254383,1.,-2.99249155170479));
#70541=CARTESIAN_POINT('Ctrl Pts',(2.82808728190402,-1.,-2.98952916401699));
#70542=CARTESIAN_POINT('Ctrl Pts',(2.82808728190402,1.,-2.98952916401699));
#70543=CARTESIAN_POINT('Ctrl Pts',(2.82093279065704,-1.,-2.98653680669434));
#70544=CARTESIAN_POINT('Ctrl Pts',(2.82093279065704,1.,-2.98653680669434));
#70545=CARTESIAN_POINT('Ctrl Pts',(2.81380019196454,-1.,-2.9835141977994));
#70546=CARTESIAN_POINT('Ctrl Pts',(2.81380019196454,1.,-2.9835141977994));
#70547=CARTESIAN_POINT('Ctrl Pts',(2.80668968101162,-1.,-2.98046109647299));
#70548=CARTESIAN_POINT('Ctrl Pts',(2.80668968101162,1.,-2.98046109647299));
#70549=CARTESIAN_POINT('Ctrl Pts',(2.79960153278186,-1.,-2.97737733718242));
#70550=CARTESIAN_POINT('Ctrl Pts',(2.79960153278186,1.,-2.97737733718242));
#70551=CARTESIAN_POINT('Ctrl Pts',(2.79253615718147,-1.,-2.97426288347475));
#70552=CARTESIAN_POINT('Ctrl Pts',(2.79253615718147,1.,-2.97426288347475));
#70553=CARTESIAN_POINT('Ctrl Pts',(2.78549409123657,-1.,-2.97111781461349));
#70554=CARTESIAN_POINT('Ctrl Pts',(2.78549409123657,1.,-2.97111781461349));
#70555=CARTESIAN_POINT('Ctrl Pts',(2.77847589542767,-1.,-2.9679422104295));
#70556=CARTESIAN_POINT('Ctrl Pts',(2.77847589542767,1.,-2.9679422104295));
#70557=CARTESIAN_POINT('Ctrl Pts',(2.77148206836464,-1.,-2.96473605585548));
#70558=CARTESIAN_POINT('Ctrl Pts',(2.77148206836464,1.,-2.96473605585548));
#70559=CARTESIAN_POINT('Ctrl Pts',(2.76451296269571,-1.,-2.96149914764832));
#70560=CARTESIAN_POINT('Ctrl Pts',(2.76451296269571,1.,-2.96149914764832));
#70561=CARTESIAN_POINT('Ctrl Pts',(2.75756867888393,-1.,-2.9582309766594));
#70562=CARTESIAN_POINT('Ctrl Pts',(2.75756867888393,1.,-2.9582309766594));
#70563=CARTESIAN_POINT('Ctrl Pts',(2.75064903318996,-1.,-2.95493069316211));
#70564=CARTESIAN_POINT('Ctrl Pts',(2.75064903318996,1.,-2.95493069316211));
#70565=CARTESIAN_POINT('Ctrl Pts',(2.7437537949221,-1.,-2.95159737214305));
#70566=CARTESIAN_POINT('Ctrl Pts',(2.7437537949221,1.,-2.95159737214305));
#70567=CARTESIAN_POINT('Ctrl Pts',(2.73688288329825,-1.,-2.94823023414381));
#70568=CARTESIAN_POINT('Ctrl Pts',(2.73688288329825,1.,-2.94823023414381));
#70569=CARTESIAN_POINT('Ctrl Pts',(2.73003657371613,-1.,-2.94482887675139));
#70570=CARTESIAN_POINT('Ctrl Pts',(2.73003657371613,1.,-2.94482887675139));
#70571=CARTESIAN_POINT('Ctrl Pts',(2.72321571511322,-1.,-2.94139351933882));
#70572=CARTESIAN_POINT('Ctrl Pts',(2.72321571511322,1.,-2.94139351933882));
#70573=CARTESIAN_POINT('Ctrl Pts',(2.71642190053575,-1.,-2.93792519474955));
#70574=CARTESIAN_POINT('Ctrl Pts',(2.71642190053575,1.,-2.93792519474955));
#70575=CARTESIAN_POINT('Ctrl Pts',(2.70965695523776,-1.,-2.93442516311168));
#70576=CARTESIAN_POINT('Ctrl Pts',(2.70965695523776,1.,-2.93442516311168));
#70577=CARTESIAN_POINT('Ctrl Pts',(2.70292247416881,-1.,-2.93089438233746));
#70578=CARTESIAN_POINT('Ctrl Pts',(2.70292247416881,1.,-2.93089438233746));
#70579=CARTESIAN_POINT('Ctrl Pts',(2.69621932864302,-1.,-2.92733294395268));
#70580=CARTESIAN_POINT('Ctrl Pts',(2.69621932864302,1.,-2.92733294395268));
#70581=CARTESIAN_POINT('Ctrl Pts',(2.68954721165342,-1.,-2.92373955325876));
#70582=CARTESIAN_POINT('Ctrl Pts',(2.68954721165342,1.,-2.92373955325876));
#70583=CARTESIAN_POINT('Ctrl Pts',(2.68290409279689,-1.,-2.92011090722152));
#70584=CARTESIAN_POINT('Ctrl Pts',(2.68290409279689,1.,-2.92011090722152));
#70585=CARTESIAN_POINT('Ctrl Pts',(2.67628728855309,-1.,-2.91644290704281));
#70586=CARTESIAN_POINT('Ctrl Pts',(2.67628728855309,1.,-2.91644290704281));
#70587=CARTESIAN_POINT('Ctrl Pts',(2.66969458792627,-1.,-2.91273193382876));
#70588=CARTESIAN_POINT('Ctrl Pts',(2.66969458792627,1.,-2.91273193382876));
#70589=CARTESIAN_POINT('Ctrl Pts',(2.66312542616808,-1.,-2.90897617968921));
#70590=CARTESIAN_POINT('Ctrl Pts',(2.66312542616808,1.,-2.90897617968921));
#70591=CARTESIAN_POINT('Ctrl Pts',(2.65658188464287,-1.,-2.90517678087467));
#70592=CARTESIAN_POINT('Ctrl Pts',(2.65658188464287,1.,-2.90517678087467));
#70593=CARTESIAN_POINT('Ctrl Pts',(2.65007017365576,-1.,-2.90133950224879));
#70594=CARTESIAN_POINT('Ctrl Pts',(2.65007017365576,1.,-2.90133950224879));
#70595=CARTESIAN_POINT('Ctrl Pts',(2.64359851684146,-1.,-2.89747231723361));
#70596=CARTESIAN_POINT('Ctrl Pts',(2.64359851684146,1.,-2.89747231723361));
#70597=CARTESIAN_POINT('Ctrl Pts',(2.63717442263944,-1.,-2.89358228854557));
#70598=CARTESIAN_POINT('Ctrl Pts',(2.63717442263944,1.,-2.89358228854557));
#70599=CARTESIAN_POINT('Ctrl Pts',(2.63080195420771,-1.,-2.88967244854243));
#70600=CARTESIAN_POINT('Ctrl Pts',(2.63080195420771,1.,-2.88967244854243));
#70601=CARTESIAN_POINT('Ctrl Pts',(2.62447947640253,-1.,-2.88573922195049));
#70602=CARTESIAN_POINT('Ctrl Pts',(2.62447947640253,1.,-2.88573922195049));
#70603=CARTESIAN_POINT('Ctrl Pts',(2.61819596473087,-1.,-2.88176821427502));
#70604=CARTESIAN_POINT('Ctrl Pts',(2.61819596473087,1.,-2.88176821427502));
#70605=CARTESIAN_POINT('Ctrl Pts',(2.61193507170928,-1.,-2.87773881947885));
#70606=CARTESIAN_POINT('Ctrl Pts',(2.61193507170928,1.,-2.87773881947885));
#70607=CARTESIAN_POINT('Ctrl Pts',(2.6056817788128,-1.,-2.87363176656475));
#70608=CARTESIAN_POINT('Ctrl Pts',(2.6056817788128,1.,-2.87363176656475));
#70609=CARTESIAN_POINT('Ctrl Pts',(2.59942875223202,-1.,-2.86943633170712));
#70610=CARTESIAN_POINT('Ctrl Pts',(2.59942875223202,1.,-2.86943633170712));
#70611=CARTESIAN_POINT('Ctrl Pts',(2.59318160184921,-1.,-2.86515629953528));
#70612=CARTESIAN_POINT('Ctrl Pts',(2.59318160184921,1.,-2.86515629953528));
#70613=CARTESIAN_POINT('Ctrl Pts',(2.5869677064356,-1.,-2.86081999003668));
#70614=CARTESIAN_POINT('Ctrl Pts',(2.5869677064356,1.,-2.86081999003668));
#70615=CARTESIAN_POINT('Ctrl Pts',(2.58082875254407,-1.,-2.85647171715147));
#70616=CARTESIAN_POINT('Ctrl Pts',(2.58082875254407,1.,-2.85647171715147));
#70617=CARTESIAN_POINT('Ctrl Pts',(2.57480482727128,-1.,-2.85215360144483));
#70618=CARTESIAN_POINT('Ctrl Pts',(2.57480482727128,1.,-2.85215360144483));
#70619=CARTESIAN_POINT('Ctrl Pts',(2.56891984251743,-1.,-2.84788893329091));
#70620=CARTESIAN_POINT('Ctrl Pts',(2.56891984251743,1.,-2.84788893329091));
#70621=CARTESIAN_POINT('Ctrl Pts',(2.56316920798489,-1.,-2.84366802680211));
#70622=CARTESIAN_POINT('Ctrl Pts',(2.56316920798489,1.,-2.84366802680211));
#70623=CARTESIAN_POINT('Ctrl Pts',(2.55749952145165,-1.,-2.83942515220699));
#70624=CARTESIAN_POINT('Ctrl Pts',(2.55749952145165,1.,-2.83942515220699));
#70625=CARTESIAN_POINT('Ctrl Pts',(2.55182152806964,-1.,-2.83505269592412));
#70626=CARTESIAN_POINT('Ctrl Pts',(2.55182152806964,1.,-2.83505269592412));
#70627=CARTESIAN_POINT('Ctrl Pts',(2.54604736792542,-1.,-2.83044254225794));
#70628=CARTESIAN_POINT('Ctrl Pts',(2.54604736792542,1.,-2.83044254225794));
#70629=CARTESIAN_POINT('Ctrl Pts',(2.54012272520141,-1.,-2.82552167649157));
#70630=CARTESIAN_POINT('Ctrl Pts',(2.54012272520141,1.,-2.82552167649157));
#70631=CARTESIAN_POINT('Ctrl Pts',(2.53405679667463,-1.,-2.82028550483744));
#70632=CARTESIAN_POINT('Ctrl Pts',(2.53405679667463,1.,-2.82028550483744));
#70633=CARTESIAN_POINT('Ctrl Pts',(2.52796388055457,-1.,-2.8148437904867));
#70634=CARTESIAN_POINT('Ctrl Pts',(2.52796388055457,1.,-2.8148437904867));
#70635=CARTESIAN_POINT('Ctrl Pts',(2.52205778589922,-1.,-2.80941521967234));
#70636=CARTESIAN_POINT('Ctrl Pts',(2.52205778589922,1.,-2.80941521967234));
#70637=CARTESIAN_POINT('Ctrl Pts',(2.51660190466067,-1.,-2.80427363984939));
#70638=CARTESIAN_POINT('Ctrl Pts',(2.51660190466067,1.,-2.80427363984939));
#70639=CARTESIAN_POINT('Ctrl Pts',(2.51186983687947,-1.,-2.79970585014308));
#70640=CARTESIAN_POINT('Ctrl Pts',(2.51186983687947,1.,-2.79970585014308));
#70641=CARTESIAN_POINT('Ctrl Pts',(2.50810555977564,-1.,-2.7959687805717));
#70642=CARTESIAN_POINT('Ctrl Pts',(2.50810555977564,1.,-2.7959687805717));
#70643=CARTESIAN_POINT('Ctrl Pts',(2.50547439929077,-1.,-2.79323694088143));
#70644=CARTESIAN_POINT('Ctrl Pts',(2.50547439929077,1.,-2.79323694088143));
#70645=CARTESIAN_POINT('Ctrl Pts',(2.50433799076945,-1.,-2.79192122906739));
#70646=CARTESIAN_POINT('Ctrl Pts',(2.50433799076945,1.,-2.79192122906739));
#70647=CARTESIAN_POINT('Ctrl Pts',(2.50404230339032,-1.,-2.79143626022225));
#70648=CARTESIAN_POINT('Ctrl Pts',(2.50404230339032,1.,-2.79143626022225));
#70649=CARTESIAN_POINT('Ctrl Pts',(2.50409239460011,-1.,-2.79133581100044));
#70650=CARTESIAN_POINT('Ctrl Pts',(2.50409239460011,1.,-2.79133581100044));
#70651=CARTESIAN_POINT('Ctrl Pts',(2.50417924854921,-1.,-2.79134130681569));
#70652=CARTESIAN_POINT('Ctrl Pts',(2.50417924854921,1.,-2.79134130681569));
#70653=CARTESIAN_POINT('',(2.91557726271063,1.,-3.02314558451372));
#70654=CARTESIAN_POINT('Ctrl Pts',(2.91557726271063,1.,-3.02314558451372));
#70655=CARTESIAN_POINT('Ctrl Pts',(2.91409518070707,1.,-3.02261975104912));
#70656=CARTESIAN_POINT('Ctrl Pts',(2.91113297349052,1.,-3.02156522743299));
#70657=CARTESIAN_POINT('Ctrl Pts',(2.90669553303902,1.,-3.01997487194926));
#70658=CARTESIAN_POINT('Ctrl Pts',(2.90079069102661,1.,-3.01783725123646));
#70659=CARTESIAN_POINT('Ctrl Pts',(2.8934292556764,1.,-3.01513660433291));
#70660=CARTESIAN_POINT('Ctrl Pts',(2.88608751706796,1.,-3.01240727309568));
#70661=CARTESIAN_POINT('Ctrl Pts',(2.87876560072799,1.,-3.0096491810855));
#70662=CARTESIAN_POINT('Ctrl Pts',(2.87146368430104,1.,-3.00686224485374));
#70663=CARTESIAN_POINT('Ctrl Pts',(2.86418200833065,1.,-3.00404638316245));
#70664=CARTESIAN_POINT('Ctrl Pts',(2.85692085715129,1.,-3.0012015079552));
#70665=CARTESIAN_POINT('Ctrl Pts',(2.84968053289104,1.,-2.99832751144566));
#70666=CARTESIAN_POINT('Ctrl Pts',(2.84246132984334,1.,-2.995424253416));
#70667=CARTESIAN_POINT('Ctrl Pts',(2.83526351254383,1.,-2.99249155170479));
#70668=CARTESIAN_POINT('Ctrl Pts',(2.82808728190402,1.,-2.98952916401699));
#70669=CARTESIAN_POINT('Ctrl Pts',(2.82093279065704,1.,-2.98653680669434));
#70670=CARTESIAN_POINT('Ctrl Pts',(2.81380019196454,1.,-2.9835141977994));
#70671=CARTESIAN_POINT('Ctrl Pts',(2.80668968101162,1.,-2.98046109647299));
#70672=CARTESIAN_POINT('Ctrl Pts',(2.79960153278186,1.,-2.97737733718242));
#70673=CARTESIAN_POINT('Ctrl Pts',(2.79253615718147,1.,-2.97426288347475));
#70674=CARTESIAN_POINT('Ctrl Pts',(2.78549409123657,1.,-2.97111781461349));
#70675=CARTESIAN_POINT('Ctrl Pts',(2.77847589542767,1.,-2.9679422104295));
#70676=CARTESIAN_POINT('Ctrl Pts',(2.77148206836464,1.,-2.96473605585548));
#70677=CARTESIAN_POINT('Ctrl Pts',(2.76451296269571,1.,-2.96149914764832));
#70678=CARTESIAN_POINT('Ctrl Pts',(2.75756867888393,1.,-2.9582309766594));
#70679=CARTESIAN_POINT('Ctrl Pts',(2.75064903318996,1.,-2.95493069316211));
#70680=CARTESIAN_POINT('Ctrl Pts',(2.7437537949221,1.,-2.95159737214305));
#70681=CARTESIAN_POINT('Ctrl Pts',(2.73688288329825,1.,-2.94823023414381));
#70682=CARTESIAN_POINT('Ctrl Pts',(2.73003657371613,1.,-2.94482887675139));
#70683=CARTESIAN_POINT('Ctrl Pts',(2.72321571511322,1.,-2.94139351933882));
#70684=CARTESIAN_POINT('Ctrl Pts',(2.71642190053575,1.,-2.93792519474955));
#70685=CARTESIAN_POINT('Ctrl Pts',(2.70965695523776,1.,-2.93442516311168));
#70686=CARTESIAN_POINT('Ctrl Pts',(2.70292247416881,1.,-2.93089438233746));
#70687=CARTESIAN_POINT('Ctrl Pts',(2.69621932864302,1.,-2.92733294395268));
#70688=CARTESIAN_POINT('Ctrl Pts',(2.68954721165342,1.,-2.92373955325876));
#70689=CARTESIAN_POINT('Ctrl Pts',(2.68290409279689,1.,-2.92011090722152));
#70690=CARTESIAN_POINT('Ctrl Pts',(2.67628728855309,1.,-2.91644290704281));
#70691=CARTESIAN_POINT('Ctrl Pts',(2.66969458792627,1.,-2.91273193382876));
#70692=CARTESIAN_POINT('Ctrl Pts',(2.66312542616808,1.,-2.90897617968921));
#70693=CARTESIAN_POINT('Ctrl Pts',(2.65658188464287,1.,-2.90517678087467));
#70694=CARTESIAN_POINT('Ctrl Pts',(2.65007017365576,1.,-2.90133950224879));
#70695=CARTESIAN_POINT('Ctrl Pts',(2.64359851684146,1.,-2.89747231723361));
#70696=CARTESIAN_POINT('Ctrl Pts',(2.63717442263944,1.,-2.89358228854557));
#70697=CARTESIAN_POINT('Ctrl Pts',(2.63080195420771,1.,-2.88967244854243));
#70698=CARTESIAN_POINT('Ctrl Pts',(2.62447947640253,1.,-2.88573922195049));
#70699=CARTESIAN_POINT('Ctrl Pts',(2.61819596473087,1.,-2.88176821427502));
#70700=CARTESIAN_POINT('Ctrl Pts',(2.61193507170928,1.,-2.87773881947885));
#70701=CARTESIAN_POINT('Ctrl Pts',(2.6056817788128,1.,-2.87363176656475));
#70702=CARTESIAN_POINT('Ctrl Pts',(2.59942875223202,1.,-2.86943633170712));
#70703=CARTESIAN_POINT('Ctrl Pts',(2.59318160184921,1.,-2.86515629953528));
#70704=CARTESIAN_POINT('Ctrl Pts',(2.5869677064356,1.,-2.86081999003668));
#70705=CARTESIAN_POINT('Ctrl Pts',(2.58082875254407,1.,-2.85647171715147));
#70706=CARTESIAN_POINT('Ctrl Pts',(2.57480482727128,1.,-2.85215360144483));
#70707=CARTESIAN_POINT('Ctrl Pts',(2.56891984251743,1.,-2.84788893329091));
#70708=CARTESIAN_POINT('Ctrl Pts',(2.56316920798489,1.,-2.84366802680211));
#70709=CARTESIAN_POINT('Ctrl Pts',(2.55749952145165,1.,-2.83942515220699));
#70710=CARTESIAN_POINT('Ctrl Pts',(2.55182152806964,1.,-2.83505269592412));
#70711=CARTESIAN_POINT('Ctrl Pts',(2.54604736792542,1.,-2.83044254225794));
#70712=CARTESIAN_POINT('Ctrl Pts',(2.54012272520141,1.,-2.82552167649157));
#70713=CARTESIAN_POINT('Ctrl Pts',(2.53405679667463,1.,-2.82028550483744));
#70714=CARTESIAN_POINT('Ctrl Pts',(2.52796388055457,1.,-2.8148437904867));
#70715=CARTESIAN_POINT('Ctrl Pts',(2.52205778589922,1.,-2.80941521967234));
#70716=CARTESIAN_POINT('Ctrl Pts',(2.51660190466067,1.,-2.80427363984939));
#70717=CARTESIAN_POINT('Ctrl Pts',(2.51186983687947,1.,-2.79970585014308));
#70718=CARTESIAN_POINT('Ctrl Pts',(2.50810555977564,1.,-2.7959687805717));
#70719=CARTESIAN_POINT('Ctrl Pts',(2.50567182569153,1.,-2.79344192164204));
#70720=CARTESIAN_POINT('Ctrl Pts',(2.50455968395235,1.,-2.79217568804874));
#70721=CARTESIAN_POINT('Ctrl Pts',(2.50417932839344,1.,-2.79164172519039));
#70722=CARTESIAN_POINT('Ctrl Pts',(2.50410700351427,1.,-2.79145823440899));
#70723=CARTESIAN_POINT('Ctrl Pts',(2.50410331873043,1.,-2.79140942341378));
#70724=CARTESIAN_POINT('',(2.91557726271063,0.,-3.02314558451372));
#70725=CARTESIAN_POINT('Ctrl Pts',(2.79134130681569,-1.,-2.50417924854921));
#70726=CARTESIAN_POINT('Ctrl Pts',(2.79134130681569,1.,-2.50417924854921));
#70727=CARTESIAN_POINT('Ctrl Pts',(2.7913358110015,-1.,-2.50409239460108));
#70728=CARTESIAN_POINT('Ctrl Pts',(2.7913358110015,1.,-2.50409239460108));
#70729=CARTESIAN_POINT('Ctrl Pts',(2.79143626022503,-1.,-2.50404230339286));
#70730=CARTESIAN_POINT('Ctrl Pts',(2.79143626022503,1.,-2.50404230339286));
#70731=CARTESIAN_POINT('Ctrl Pts',(2.79192122907148,-1.,-2.5043379907732));
#70732=CARTESIAN_POINT('Ctrl Pts',(2.79192122907148,1.,-2.5043379907732));
#70733=CARTESIAN_POINT('Ctrl Pts',(2.7932369408851,-1.,-2.50547439929414));
#70734=CARTESIAN_POINT('Ctrl Pts',(2.7932369408851,1.,-2.50547439929414));
#70735=CARTESIAN_POINT('Ctrl Pts',(2.79596878057287,-1.,-2.50810555977671));
#70736=CARTESIAN_POINT('Ctrl Pts',(2.79596878057287,1.,-2.50810555977671));
#70737=CARTESIAN_POINT('Ctrl Pts',(2.79970585014168,-1.,-2.51186983687818));
#70738=CARTESIAN_POINT('Ctrl Pts',(2.79970585014168,1.,-2.51186983687818));
#70739=CARTESIAN_POINT('Ctrl Pts',(2.80427363984653,-1.,-2.51660190465805));
#70740=CARTESIAN_POINT('Ctrl Pts',(2.80427363984653,1.,-2.51660190465805));
#70741=CARTESIAN_POINT('Ctrl Pts',(2.80941521966941,-1.,-2.52205778589653));
#70742=CARTESIAN_POINT('Ctrl Pts',(2.80941521966941,1.,-2.52205778589653));
#70743=CARTESIAN_POINT('Ctrl Pts',(2.81484379048475,-1.,-2.52796388055278));
#70744=CARTESIAN_POINT('Ctrl Pts',(2.81484379048475,1.,-2.52796388055278));
#70745=CARTESIAN_POINT('Ctrl Pts',(2.82028550483689,-1.,-2.53405679667412));
#70746=CARTESIAN_POINT('Ctrl Pts',(2.82028550483689,1.,-2.53405679667412));
#70747=CARTESIAN_POINT('Ctrl Pts',(2.8255216764922,-1.,-2.54012272520199));
#70748=CARTESIAN_POINT('Ctrl Pts',(2.8255216764922,1.,-2.54012272520199));
#70749=CARTESIAN_POINT('Ctrl Pts',(2.83044254225917,-1.,-2.54604736792655));
#70750=CARTESIAN_POINT('Ctrl Pts',(2.83044254225917,1.,-2.54604736792655));
#70751=CARTESIAN_POINT('Ctrl Pts',(2.83505269592536,-1.,-2.55182152807077));
#70752=CARTESIAN_POINT('Ctrl Pts',(2.83505269592536,1.,-2.55182152807077));
#70753=CARTESIAN_POINT('Ctrl Pts',(2.83942515220782,-1.,-2.55749952145241));
#70754=CARTESIAN_POINT('Ctrl Pts',(2.83942515220782,1.,-2.55749952145241));
#70755=CARTESIAN_POINT('Ctrl Pts',(2.84366802680237,-1.,-2.56316920798513));
#70756=CARTESIAN_POINT('Ctrl Pts',(2.84366802680237,1.,-2.56316920798513));
#70757=CARTESIAN_POINT('Ctrl Pts',(2.84788893329067,-1.,-2.56891984251721));
#70758=CARTESIAN_POINT('Ctrl Pts',(2.84788893329067,1.,-2.56891984251721));
#70759=CARTESIAN_POINT('Ctrl Pts',(2.85215360144431,-1.,-2.57480482727081));
#70760=CARTESIAN_POINT('Ctrl Pts',(2.85215360144431,1.,-2.57480482727081));
#70761=CARTESIAN_POINT('Ctrl Pts',(2.85647171715092,-1.,-2.58082875254357));
#70762=CARTESIAN_POINT('Ctrl Pts',(2.85647171715092,1.,-2.58082875254357));
#70763=CARTESIAN_POINT('Ctrl Pts',(2.86081999003629,-1.,-2.58696770643524));
#70764=CARTESIAN_POINT('Ctrl Pts',(2.86081999003629,1.,-2.58696770643524));
#70765=CARTESIAN_POINT('Ctrl Pts',(2.86515629953513,-1.,-2.59318160184908));
#70766=CARTESIAN_POINT('Ctrl Pts',(2.86515629953513,1.,-2.59318160184908));
#70767=CARTESIAN_POINT('Ctrl Pts',(2.86943633170722,-1.,-2.5994287522321));
#70768=CARTESIAN_POINT('Ctrl Pts',(2.86943633170722,1.,-2.5994287522321));
#70769=CARTESIAN_POINT('Ctrl Pts',(2.87363176656501,-1.,-2.60568177881303));
#70770=CARTESIAN_POINT('Ctrl Pts',(2.87363176656501,1.,-2.60568177881303));
#70771=CARTESIAN_POINT('Ctrl Pts',(2.87773881947915,-1.,-2.61193507170955));
#70772=CARTESIAN_POINT('Ctrl Pts',(2.87773881947915,1.,-2.61193507170955));
#70773=CARTESIAN_POINT('Ctrl Pts',(2.88176821427525,-1.,-2.61819596473108));
#70774=CARTESIAN_POINT('Ctrl Pts',(2.88176821427525,1.,-2.61819596473108));
#70775=CARTESIAN_POINT('Ctrl Pts',(2.88573922195059,-1.,-2.62447947640262));
#70776=CARTESIAN_POINT('Ctrl Pts',(2.88573922195059,1.,-2.62447947640262));
#70777=CARTESIAN_POINT('Ctrl Pts',(2.88967244854239,-1.,-2.63080195420767));
#70778=CARTESIAN_POINT('Ctrl Pts',(2.88967244854239,1.,-2.63080195420767));
#70779=CARTESIAN_POINT('Ctrl Pts',(2.89358228854544,-1.,-2.63717442263932));
#70780=CARTESIAN_POINT('Ctrl Pts',(2.89358228854544,1.,-2.63717442263932));
#70781=CARTESIAN_POINT('Ctrl Pts',(2.89747231723345,-1.,-2.64359851684131));
#70782=CARTESIAN_POINT('Ctrl Pts',(2.89747231723345,1.,-2.64359851684131));
#70783=CARTESIAN_POINT('Ctrl Pts',(2.90133950224867,-1.,-2.65007017365564));
#70784=CARTESIAN_POINT('Ctrl Pts',(2.90133950224867,1.,-2.65007017365564));
#70785=CARTESIAN_POINT('Ctrl Pts',(2.90517678087461,-1.,-2.65658188464282));
#70786=CARTESIAN_POINT('Ctrl Pts',(2.90517678087461,1.,-2.65658188464282));
#70787=CARTESIAN_POINT('Ctrl Pts',(2.90897617968923,-1.,-2.6631254261681));
#70788=CARTESIAN_POINT('Ctrl Pts',(2.90897617968923,1.,-2.6631254261681));
#70789=CARTESIAN_POINT('Ctrl Pts',(2.91273193382882,-1.,-2.66969458792631));
#70790=CARTESIAN_POINT('Ctrl Pts',(2.91273193382882,1.,-2.66969458792631));
#70791=CARTESIAN_POINT('Ctrl Pts',(2.91644290704285,-1.,-2.67628728855312));
#70792=CARTESIAN_POINT('Ctrl Pts',(2.91644290704285,1.,-2.67628728855312));
#70793=CARTESIAN_POINT('Ctrl Pts',(2.92011090722152,-1.,-2.68290409279688));
#70794=CARTESIAN_POINT('Ctrl Pts',(2.92011090722152,1.,-2.68290409279688));
#70795=CARTESIAN_POINT('Ctrl Pts',(2.92373955325875,-1.,-2.68954721165339));
#70796=CARTESIAN_POINT('Ctrl Pts',(2.92373955325875,1.,-2.68954721165339));
#70797=CARTESIAN_POINT('Ctrl Pts',(2.92733294395267,-1.,-2.69621932864301));
#70798=CARTESIAN_POINT('Ctrl Pts',(2.92733294395267,1.,-2.69621932864301));
#70799=CARTESIAN_POINT('Ctrl Pts',(2.93089438233749,-1.,-2.70292247416885));
#70800=CARTESIAN_POINT('Ctrl Pts',(2.93089438233749,1.,-2.70292247416885));
#70801=CARTESIAN_POINT('Ctrl Pts',(2.93442516311179,-1.,-2.70965695523787));
#70802=CARTESIAN_POINT('Ctrl Pts',(2.93442516311179,1.,-2.70965695523787));
#70803=CARTESIAN_POINT('Ctrl Pts',(2.93792519474972,-1.,-2.71642190053592));
#70804=CARTESIAN_POINT('Ctrl Pts',(2.93792519474972,1.,-2.71642190053592));
#70805=CARTESIAN_POINT('Ctrl Pts',(2.94139351933897,-1.,-2.72321571511337));
#70806=CARTESIAN_POINT('Ctrl Pts',(2.94139351933897,1.,-2.72321571511337));
#70807=CARTESIAN_POINT('Ctrl Pts',(2.94482887675143,-1.,-2.73003657371617));
#70808=CARTESIAN_POINT('Ctrl Pts',(2.94482887675143,1.,-2.73003657371617));
#70809=CARTESIAN_POINT('Ctrl Pts',(2.94823023414364,-1.,-2.73688288329808));
#70810=CARTESIAN_POINT('Ctrl Pts',(2.94823023414364,1.,-2.73688288329808));
#70811=CARTESIAN_POINT('Ctrl Pts',(2.95159737214266,-1.,-2.74375379492172));
#70812=CARTESIAN_POINT('Ctrl Pts',(2.95159737214266,1.,-2.74375379492172));
#70813=CARTESIAN_POINT('Ctrl Pts',(2.95493069316161,-1.,-2.75064903318947));
#70814=CARTESIAN_POINT('Ctrl Pts',(2.95493069316161,1.,-2.75064903318947));
#70815=CARTESIAN_POINT('Ctrl Pts',(2.95823097665896,-1.,-2.7575686788835));
#70816=CARTESIAN_POINT('Ctrl Pts',(2.95823097665896,1.,-2.7575686788835));
#70817=CARTESIAN_POINT('Ctrl Pts',(2.96149914764818,-1.,-2.76451296269557));
#70818=CARTESIAN_POINT('Ctrl Pts',(2.96149914764818,1.,-2.76451296269557));
#70819=CARTESIAN_POINT('Ctrl Pts',(2.96473605585583,-1.,-2.77148206836498));
#70820=CARTESIAN_POINT('Ctrl Pts',(2.96473605585583,1.,-2.77148206836498));
#70821=CARTESIAN_POINT('Ctrl Pts',(2.96794221043036,-1.,-2.7784758954285));
#70822=CARTESIAN_POINT('Ctrl Pts',(2.96794221043036,1.,-2.7784758954285));
#70823=CARTESIAN_POINT('Ctrl Pts',(2.97111781461465,-1.,-2.78549409123769));
#70824=CARTESIAN_POINT('Ctrl Pts',(2.97111781461465,1.,-2.78549409123769));
#70825=CARTESIAN_POINT('Ctrl Pts',(2.9742628834758,-1.,-2.79253615718248));
#70826=CARTESIAN_POINT('Ctrl Pts',(2.9742628834758,1.,-2.79253615718248));
#70827=CARTESIAN_POINT('Ctrl Pts',(2.97737733718287,-1.,-2.7996015327823));
#70828=CARTESIAN_POINT('Ctrl Pts',(2.97737733718287,1.,-2.7996015327823));
#70829=CARTESIAN_POINT('Ctrl Pts',(2.98046109647241,-1.,-2.80668968101106));
#70830=CARTESIAN_POINT('Ctrl Pts',(2.98046109647241,1.,-2.80668968101106));
#70831=CARTESIAN_POINT('Ctrl Pts',(2.98351419779767,-1.,-2.81380019196286));
#70832=CARTESIAN_POINT('Ctrl Pts',(2.98351419779767,1.,-2.81380019196286));
#70833=CARTESIAN_POINT('Ctrl Pts',(2.9865368066918,-1.,-2.82093279065457));
#70834=CARTESIAN_POINT('Ctrl Pts',(2.9865368066918,1.,-2.82093279065457));
#70835=CARTESIAN_POINT('Ctrl Pts',(2.98952916401446,-1.,-2.82808728190157));
#70836=CARTESIAN_POINT('Ctrl Pts',(2.98952916401446,1.,-2.82808728190157));
#70837=CARTESIAN_POINT('Ctrl Pts',(2.99249155170339,-1.,-2.83526351254248));
#70838=CARTESIAN_POINT('Ctrl Pts',(2.99249155170339,1.,-2.83526351254248));
#70839=CARTESIAN_POINT('Ctrl Pts',(2.99542425341685,-1.,-2.84246132984415));
#70840=CARTESIAN_POINT('Ctrl Pts',(2.99542425341685,1.,-2.84246132984415));
#70841=CARTESIAN_POINT('Ctrl Pts',(2.99832751144925,-1.,-2.84968053289451));
#70842=CARTESIAN_POINT('Ctrl Pts',(2.99832751144925,1.,-2.84968053289451));
#70843=CARTESIAN_POINT('Ctrl Pts',(3.00120150796095,-1.,-2.85692085715686));
#70844=CARTESIAN_POINT('Ctrl Pts',(3.00120150796095,1.,-2.85692085715686));
#70845=CARTESIAN_POINT('Ctrl Pts',(3.00404638316867,-1.,-2.86418200833667));
#70846=CARTESIAN_POINT('Ctrl Pts',(3.00404638316867,1.,-2.86418200833667));
#70847=CARTESIAN_POINT('Ctrl Pts',(3.00686224485784,-1.,-2.87146368430502));
#70848=CARTESIAN_POINT('Ctrl Pts',(3.00686224485784,1.,-2.87146368430502));
#70849=CARTESIAN_POINT('Ctrl Pts',(3.00964918108476,-1.,-2.87876560072727));
#70850=CARTESIAN_POINT('Ctrl Pts',(3.00964918108476,1.,-2.87876560072727));
#70851=CARTESIAN_POINT('Ctrl Pts',(3.01240727308829,-1.,-2.8860875170608));
#70852=CARTESIAN_POINT('Ctrl Pts',(3.01240727308829,1.,-2.8860875170608));
#70853=CARTESIAN_POINT('Ctrl Pts',(3.01513660431928,-1.,-2.89342925566321));
#70854=CARTESIAN_POINT('Ctrl Pts',(3.01513660431928,1.,-2.89342925566321));
#70855=CARTESIAN_POINT('Ctrl Pts',(3.01783725121981,-1.,-2.9007906910105));
#70856=CARTESIAN_POINT('Ctrl Pts',(3.01783725121981,1.,-2.9007906910105));
#70857=CARTESIAN_POINT('Ctrl Pts',(3.01997487193503,-1.,-2.90669553302526));
#70858=CARTESIAN_POINT('Ctrl Pts',(3.01997487193503,1.,-2.90669553302526));
#70859=CARTESIAN_POINT('Ctrl Pts',(3.02156522742431,-1.,-2.91113297348212));
#70860=CARTESIAN_POINT('Ctrl Pts',(3.02156522742431,1.,-2.91113297348212));
#70861=CARTESIAN_POINT('Ctrl Pts',(3.02261975104593,-1.,-2.91409518070399));
#70862=CARTESIAN_POINT('Ctrl Pts',(3.02261975104593,1.,-2.91409518070399));
#70863=CARTESIAN_POINT('Ctrl Pts',(3.02314558451372,-1.,-2.91557726271063));
#70864=CARTESIAN_POINT('Ctrl Pts',(3.02314558451372,1.,-2.91557726271063));
#70865=CARTESIAN_POINT('',(2.79140942341258,1.,-2.50410331873176));
#70866=CARTESIAN_POINT('Ctrl Pts',(2.79140942341258,-1.,-2.50410331873176));
#70867=CARTESIAN_POINT('Ctrl Pts',(2.79140942341258,-0.666666666666667,
-2.50410331873176));
#70868=CARTESIAN_POINT('Ctrl Pts',(2.79140942341258,-0.333333333333333,
-2.50410331873176));
#70869=CARTESIAN_POINT('Ctrl Pts',(2.79140942341258,0.333333333333333,-2.50410331873176));
#70870=CARTESIAN_POINT('Ctrl Pts',(2.79140942341258,0.666666666666667,-2.50410331873176));
#70871=CARTESIAN_POINT('Ctrl Pts',(2.79140942341258,1.,-2.50410331873176));
#70872=CARTESIAN_POINT('',(3.02314558451372,1.,-2.91557726271063));
#70873=CARTESIAN_POINT('',(3.02314558451372,0.,-2.91557726271063));
#70874=CARTESIAN_POINT('Ctrl Pts',(2.79140942341258,1.,-2.50410331873176));
#70875=CARTESIAN_POINT('Ctrl Pts',(2.79145823440781,1.,-2.50410700351493));
#70876=CARTESIAN_POINT('Ctrl Pts',(2.79164172518905,1.,-2.50417932839313));
#70877=CARTESIAN_POINT('Ctrl Pts',(2.79217568804755,1.,-2.50455968395146));
#70878=CARTESIAN_POINT('Ctrl Pts',(2.79344192164147,1.,-2.50567182569081));
#70879=CARTESIAN_POINT('Ctrl Pts',(2.79596878057287,1.,-2.50810555977671));
#70880=CARTESIAN_POINT('Ctrl Pts',(2.79970585014168,1.,-2.51186983687818));
#70881=CARTESIAN_POINT('Ctrl Pts',(2.80427363984653,1.,-2.51660190465805));
#70882=CARTESIAN_POINT('Ctrl Pts',(2.80941521966941,1.,-2.52205778589653));
#70883=CARTESIAN_POINT('Ctrl Pts',(2.81484379048475,1.,-2.52796388055278));
#70884=CARTESIAN_POINT('Ctrl Pts',(2.82028550483689,1.,-2.53405679667412));
#70885=CARTESIAN_POINT('Ctrl Pts',(2.8255216764922,1.,-2.54012272520199));
#70886=CARTESIAN_POINT('Ctrl Pts',(2.83044254225917,1.,-2.54604736792655));
#70887=CARTESIAN_POINT('Ctrl Pts',(2.83505269592536,1.,-2.55182152807077));
#70888=CARTESIAN_POINT('Ctrl Pts',(2.83942515220782,1.,-2.55749952145241));
#70889=CARTESIAN_POINT('Ctrl Pts',(2.84366802680237,1.,-2.56316920798513));
#70890=CARTESIAN_POINT('Ctrl Pts',(2.84788893329067,1.,-2.56891984251721));
#70891=CARTESIAN_POINT('Ctrl Pts',(2.85215360144431,1.,-2.57480482727081));
#70892=CARTESIAN_POINT('Ctrl Pts',(2.85647171715092,1.,-2.58082875254357));
#70893=CARTESIAN_POINT('Ctrl Pts',(2.86081999003629,1.,-2.58696770643524));
#70894=CARTESIAN_POINT('Ctrl Pts',(2.86515629953513,1.,-2.59318160184908));
#70895=CARTESIAN_POINT('Ctrl Pts',(2.86943633170722,1.,-2.5994287522321));
#70896=CARTESIAN_POINT('Ctrl Pts',(2.87363176656501,1.,-2.60568177881303));
#70897=CARTESIAN_POINT('Ctrl Pts',(2.87773881947915,1.,-2.61193507170955));
#70898=CARTESIAN_POINT('Ctrl Pts',(2.88176821427525,1.,-2.61819596473108));
#70899=CARTESIAN_POINT('Ctrl Pts',(2.88573922195059,1.,-2.62447947640262));
#70900=CARTESIAN_POINT('Ctrl Pts',(2.88967244854239,1.,-2.63080195420767));
#70901=CARTESIAN_POINT('Ctrl Pts',(2.89358228854544,1.,-2.63717442263932));
#70902=CARTESIAN_POINT('Ctrl Pts',(2.89747231723345,1.,-2.64359851684131));
#70903=CARTESIAN_POINT('Ctrl Pts',(2.90133950224867,1.,-2.65007017365564));
#70904=CARTESIAN_POINT('Ctrl Pts',(2.90517678087461,1.,-2.65658188464282));
#70905=CARTESIAN_POINT('Ctrl Pts',(2.90897617968923,1.,-2.6631254261681));
#70906=CARTESIAN_POINT('Ctrl Pts',(2.91273193382882,1.,-2.66969458792631));
#70907=CARTESIAN_POINT('Ctrl Pts',(2.91644290704285,1.,-2.67628728855312));
#70908=CARTESIAN_POINT('Ctrl Pts',(2.92011090722152,1.,-2.68290409279688));
#70909=CARTESIAN_POINT('Ctrl Pts',(2.92373955325875,1.,-2.68954721165339));
#70910=CARTESIAN_POINT('Ctrl Pts',(2.92733294395267,1.,-2.69621932864301));
#70911=CARTESIAN_POINT('Ctrl Pts',(2.93089438233749,1.,-2.70292247416885));
#70912=CARTESIAN_POINT('Ctrl Pts',(2.93442516311179,1.,-2.70965695523787));
#70913=CARTESIAN_POINT('Ctrl Pts',(2.93792519474972,1.,-2.71642190053592));
#70914=CARTESIAN_POINT('Ctrl Pts',(2.94139351933897,1.,-2.72321571511337));
#70915=CARTESIAN_POINT('Ctrl Pts',(2.94482887675143,1.,-2.73003657371617));
#70916=CARTESIAN_POINT('Ctrl Pts',(2.94823023414364,1.,-2.73688288329808));
#70917=CARTESIAN_POINT('Ctrl Pts',(2.95159737214266,1.,-2.74375379492172));
#70918=CARTESIAN_POINT('Ctrl Pts',(2.95493069316161,1.,-2.75064903318947));
#70919=CARTESIAN_POINT('Ctrl Pts',(2.95823097665896,1.,-2.7575686788835));
#70920=CARTESIAN_POINT('Ctrl Pts',(2.96149914764818,1.,-2.76451296269557));
#70921=CARTESIAN_POINT('Ctrl Pts',(2.96473605585583,1.,-2.77148206836498));
#70922=CARTESIAN_POINT('Ctrl Pts',(2.96794221043036,1.,-2.7784758954285));
#70923=CARTESIAN_POINT('Ctrl Pts',(2.97111781461465,1.,-2.78549409123769));
#70924=CARTESIAN_POINT('Ctrl Pts',(2.9742628834758,1.,-2.79253615718248));
#70925=CARTESIAN_POINT('Ctrl Pts',(2.97737733718287,1.,-2.7996015327823));
#70926=CARTESIAN_POINT('Ctrl Pts',(2.98046109647241,1.,-2.80668968101106));
#70927=CARTESIAN_POINT('Ctrl Pts',(2.98351419779767,1.,-2.81380019196286));
#70928=CARTESIAN_POINT('Ctrl Pts',(2.9865368066918,1.,-2.82093279065457));
#70929=CARTESIAN_POINT('Ctrl Pts',(2.98952916401446,1.,-2.82808728190157));
#70930=CARTESIAN_POINT('Ctrl Pts',(2.99249155170339,1.,-2.83526351254248));
#70931=CARTESIAN_POINT('Ctrl Pts',(2.99542425341685,1.,-2.84246132984415));
#70932=CARTESIAN_POINT('Ctrl Pts',(2.99832751144925,1.,-2.84968053289451));
#70933=CARTESIAN_POINT('Ctrl Pts',(3.00120150796095,1.,-2.85692085715686));
#70934=CARTESIAN_POINT('Ctrl Pts',(3.00404638316867,1.,-2.86418200833667));
#70935=CARTESIAN_POINT('Ctrl Pts',(3.00686224485784,1.,-2.87146368430502));
#70936=CARTESIAN_POINT('Ctrl Pts',(3.00964918108476,1.,-2.87876560072727));
#70937=CARTESIAN_POINT('Ctrl Pts',(3.01240727308829,1.,-2.8860875170608));
#70938=CARTESIAN_POINT('Ctrl Pts',(3.01513660431928,1.,-2.89342925566321));
#70939=CARTESIAN_POINT('Ctrl Pts',(3.01783725121981,1.,-2.9007906910105));
#70940=CARTESIAN_POINT('Ctrl Pts',(3.01997487193503,1.,-2.90669553302526));
#70941=CARTESIAN_POINT('Ctrl Pts',(3.02156522742431,1.,-2.91113297348212));
#70942=CARTESIAN_POINT('Ctrl Pts',(3.02261975104593,1.,-2.91409518070399));
#70943=CARTESIAN_POINT('Ctrl Pts',(3.02314558451372,1.,-2.91557726271063));
#70944=CARTESIAN_POINT('Origin',(3.02314558451372,0.,-2.91557726271063));
#70945=CARTESIAN_POINT('',(2.91557726271063,1.,-3.02314558451372));
#70946=CARTESIAN_POINT('Origin',(0.,0.,0.));
#70947=CARTESIAN_POINT('',(2.90994629141562,1.,-2.36531447826213));
#70948=CARTESIAN_POINT('Origin',(0.,1.,0.));
#70949=CARTESIAN_POINT('Ctrl Pts',(2.90994629141562,1.,-2.36531447826213));
#70950=CARTESIAN_POINT('Ctrl Pts',(2.90994629141562,0.666666666666667,-2.36531447826213));
#70951=CARTESIAN_POINT('Ctrl Pts',(2.90994629141562,0.333333333333333,-2.36531447826213));
#70952=CARTESIAN_POINT('Ctrl Pts',(2.90994629141562,-0.333333333333333,
-2.36531447826213));
#70953=CARTESIAN_POINT('Ctrl Pts',(2.90994629141562,-0.666666666666667,
-2.36531447826213));
#70954=CARTESIAN_POINT('Ctrl Pts',(2.90994629141562,-1.,-2.36531447826213));
#70955=CARTESIAN_POINT('Ctrl Pts',(3.35260583073571,-1.,-2.52982887637028));
#70956=CARTESIAN_POINT('Ctrl Pts',(3.35260583073571,1.,-2.52982887637028));
#70957=CARTESIAN_POINT('Ctrl Pts',(3.35105973714426,-1.,-2.52954136549357));
#70958=CARTESIAN_POINT('Ctrl Pts',(3.35105973714426,1.,-2.52954136549357));
#70959=CARTESIAN_POINT('Ctrl Pts',(3.34796903577628,-1.,-2.5289632161143));
#70960=CARTESIAN_POINT('Ctrl Pts',(3.34796903577628,1.,-2.5289632161143));
#70961=CARTESIAN_POINT('Ctrl Pts',(3.34333744117093,-1.,-2.52808660916879));
#70962=CARTESIAN_POINT('Ctrl Pts',(3.34333744117093,1.,-2.52808660916879));
#70963=CARTESIAN_POINT('Ctrl Pts',(3.33717090000955,-1.,-2.52689902691551));
#70964=CARTESIAN_POINT('Ctrl Pts',(3.33717090000955,1.,-2.52689902691551));
#70965=CARTESIAN_POINT('Ctrl Pts',(3.32947762189049,-1.,-2.52538321165774));
#70966=CARTESIAN_POINT('Ctrl Pts',(3.32947762189049,1.,-2.52538321165774));
#70967=CARTESIAN_POINT('Ctrl Pts',(3.32179931079521,-1.,-2.52383598396878));
#70968=CARTESIAN_POINT('Ctrl Pts',(3.32179931079521,1.,-2.52383598396878));
#70969=CARTESIAN_POINT('Ctrl Pts',(3.31413607874727,-1.,-2.52225724871375));
#70970=CARTESIAN_POINT('Ctrl Pts',(3.31413607874727,1.,-2.52225724871375));
#70971=CARTESIAN_POINT('Ctrl Pts',(3.30648808814986,-1.,-2.52064689568167));
#70972=CARTESIAN_POINT('Ctrl Pts',(3.30648808814986,1.,-2.52064689568167));
#70973=CARTESIAN_POINT('Ctrl Pts',(3.29885556387661,-1.,-2.51900480700548));
#70974=CARTESIAN_POINT('Ctrl Pts',(3.29885556387661,1.,-2.51900480700548));
#70975=CARTESIAN_POINT('Ctrl Pts',(3.2912387729863,-1.,-2.51733085123316));
#70976=CARTESIAN_POINT('Ctrl Pts',(3.2912387729863,1.,-2.51733085123316));
#70977=CARTESIAN_POINT('Ctrl Pts',(3.28363799702583,-1.,-2.51562487464215));
#70978=CARTESIAN_POINT('Ctrl Pts',(3.28363799702583,1.,-2.51562487464215));
#70979=CARTESIAN_POINT('Ctrl Pts',(3.27605350473048,-1.,-2.51388669270329));
#70980=CARTESIAN_POINT('Ctrl Pts',(3.27605350473048,1.,-2.51388669270329));
#70981=CARTESIAN_POINT('Ctrl Pts',(3.26848552888271,-1.,-2.51211608411539));
#70982=CARTESIAN_POINT('Ctrl Pts',(3.26848552888271,1.,-2.51211608411539));
#70983=CARTESIAN_POINT('Ctrl Pts',(3.26093423001716,-1.,-2.51031277813697));
#70984=CARTESIAN_POINT('Ctrl Pts',(3.26093423001716,1.,-2.51031277813697));
#70985=CARTESIAN_POINT('Ctrl Pts',(3.25339971461265,-1.,-2.50847647070936));
#70986=CARTESIAN_POINT('Ctrl Pts',(3.25339971461265,1.,-2.50847647070936));
#70987=CARTESIAN_POINT('Ctrl Pts',(3.24588208984042,-1.,-2.50660685940645));
#70988=CARTESIAN_POINT('Ctrl Pts',(3.24588208984042,1.,-2.50660685940645));
#70989=CARTESIAN_POINT('Ctrl Pts',(3.23838151080383,-1.,-2.50470367580078));
#70990=CARTESIAN_POINT('Ctrl Pts',(3.23838151080383,1.,-2.50470367580078));
#70991=CARTESIAN_POINT('Ctrl Pts',(3.23089822320596,-1.,-2.50276671338074));
#70992=CARTESIAN_POINT('Ctrl Pts',(3.23089822320596,1.,-2.50276671338074));
#70993=CARTESIAN_POINT('Ctrl Pts',(3.22343262620387,-1.,-2.5007958720187));
#70994=CARTESIAN_POINT('Ctrl Pts',(3.22343262620387,1.,-2.5007958720187));
#70995=CARTESIAN_POINT('Ctrl Pts',(3.21598526261157,-1.,-2.49879114599293));
#70996=CARTESIAN_POINT('Ctrl Pts',(3.21598526261157,1.,-2.49879114599293));
#70997=CARTESIAN_POINT('Ctrl Pts',(3.2085566984974,-1.,-2.49675252647298));
#70998=CARTESIAN_POINT('Ctrl Pts',(3.2085566984974,1.,-2.49675252647298));
#70999=CARTESIAN_POINT('Ctrl Pts',(3.20114742397549,-1.,-2.49467992057726));
#71000=CARTESIAN_POINT('Ctrl Pts',(3.20114742397549,1.,-2.49467992057726));
#71001=CARTESIAN_POINT('Ctrl Pts',(3.19375775555814,-1.,-2.4925730723986));
#71002=CARTESIAN_POINT('Ctrl Pts',(3.19375775555814,1.,-2.4925730723986));
#71003=CARTESIAN_POINT('Ctrl Pts',(3.18638771282315,-1.,-2.49043146334095));
#71004=CARTESIAN_POINT('Ctrl Pts',(3.18638771282315,1.,-2.49043146334095));
#71005=CARTESIAN_POINT('Ctrl Pts',(3.17903698136678,-1.,-2.48825428288243));
#71006=CARTESIAN_POINT('Ctrl Pts',(3.17903698136678,1.,-2.48825428288243));
#71007=CARTESIAN_POINT('Ctrl Pts',(3.17170518863357,-1.,-2.48604065348619));
#71008=CARTESIAN_POINT('Ctrl Pts',(3.17170518863357,1.,-2.48604065348619));
#71009=CARTESIAN_POINT('Ctrl Pts',(3.16439213290181,-1.,-2.48378981792739));
#71010=CARTESIAN_POINT('Ctrl Pts',(3.16439213290181,1.,-2.48378981792739));
#71011=CARTESIAN_POINT('Ctrl Pts',(3.15709802322735,-1.,-2.48150133566568));
#71012=CARTESIAN_POINT('Ctrl Pts',(3.15709802322735,1.,-2.48150133566568));
#71013=CARTESIAN_POINT('Ctrl Pts',(3.14982373241335,-1.,-2.47917529057016));
#71014=CARTESIAN_POINT('Ctrl Pts',(3.14982373241335,1.,-2.47917529057016));
#71015=CARTESIAN_POINT('Ctrl Pts',(3.14257099546531,-1.,-2.47681245356095));
#71016=CARTESIAN_POINT('Ctrl Pts',(3.14257099546531,1.,-2.47681245356095));
#71017=CARTESIAN_POINT('Ctrl Pts',(3.13534181229282,-1.,-2.47441378371923));
#71018=CARTESIAN_POINT('Ctrl Pts',(3.13534181229282,1.,-2.47441378371923));
#71019=CARTESIAN_POINT('Ctrl Pts',(3.12813790805948,-1.,-2.47197997765868));
#71020=CARTESIAN_POINT('Ctrl Pts',(3.12813790805948,1.,-2.47197997765868));
#71021=CARTESIAN_POINT('Ctrl Pts',(3.12096015766984,-1.,-2.4695109894747));
#71022=CARTESIAN_POINT('Ctrl Pts',(3.12096015766984,1.,-2.4695109894747));
#71023=CARTESIAN_POINT('Ctrl Pts',(3.11380805536124,-1.,-2.46700558843507));
#71024=CARTESIAN_POINT('Ctrl Pts',(3.11380805536124,1.,-2.46700558843507));
#71025=CARTESIAN_POINT('Ctrl Pts',(3.10667907901981,-1.,-2.46446082979645));
#71026=CARTESIAN_POINT('Ctrl Pts',(3.10667907901981,1.,-2.46446082979645));
#71027=CARTESIAN_POINT('Ctrl Pts',(3.09956993697048,-1.,-2.4618730850188));
#71028=CARTESIAN_POINT('Ctrl Pts',(3.09956993697048,1.,-2.4618730850188));
#71029=CARTESIAN_POINT('Ctrl Pts',(3.09247787931881,-1.,-2.45923912563875));
#71030=CARTESIAN_POINT('Ctrl Pts',(3.09247787931881,1.,-2.45923912563875));
#71031=CARTESIAN_POINT('Ctrl Pts',(3.08540206545313,-1.,-2.45655725437037));
#71032=CARTESIAN_POINT('Ctrl Pts',(3.08540206545313,1.,-2.45655725437037));
#71033=CARTESIAN_POINT('Ctrl Pts',(3.07834472886145,-1.,-2.45382826787795));
#71034=CARTESIAN_POINT('Ctrl Pts',(3.07834472886145,1.,-2.45382826787795));
#71035=CARTESIAN_POINT('Ctrl Pts',(3.0713129052131,-1.,-2.45105688854432));
#71036=CARTESIAN_POINT('Ctrl Pts',(3.0713129052131,1.,-2.45105688854432));
#71037=CARTESIAN_POINT('Ctrl Pts',(3.06431596421422,-1.,-2.44824970516558));
#71038=CARTESIAN_POINT('Ctrl Pts',(3.06431596421422,1.,-2.44824970516558));
#71039=CARTESIAN_POINT('Ctrl Pts',(3.05736242671521,-1.,-2.44541251892568));
#71040=CARTESIAN_POINT('Ctrl Pts',(3.05736242671521,1.,-2.44541251892568));
#71041=CARTESIAN_POINT('Ctrl Pts',(3.05045678021509,-1.,-2.44254768923109));
#71042=CARTESIAN_POINT('Ctrl Pts',(3.05045678021509,1.,-2.44254768923109));
#71043=CARTESIAN_POINT('Ctrl Pts',(3.04359685040545,-1.,-2.43965194061849));
#71044=CARTESIAN_POINT('Ctrl Pts',(3.04359685040545,1.,-2.43965194061849));
#71045=CARTESIAN_POINT('Ctrl Pts',(3.03676949672797,-1.,-2.43671278042394));
#71046=CARTESIAN_POINT('Ctrl Pts',(3.03676949672797,1.,-2.43671278042394));
#71047=CARTESIAN_POINT('Ctrl Pts',(3.02995534946946,-1.,-2.43371241361462));
#71048=CARTESIAN_POINT('Ctrl Pts',(3.02995534946946,1.,-2.43371241361462));
#71049=CARTESIAN_POINT('Ctrl Pts',(3.02313656035977,-1.,-2.43063415586615));
#71050=CARTESIAN_POINT('Ctrl Pts',(3.02313656035977,1.,-2.43063415586615));
#71051=CARTESIAN_POINT('Ctrl Pts',(3.01630420830493,-1.,-2.4274685626416));
#71052=CARTESIAN_POINT('Ctrl Pts',(3.01630420830493,1.,-2.4274685626416));
#71053=CARTESIAN_POINT('Ctrl Pts',(3.00946442616674,-1.,-2.42421849439625));
#71054=CARTESIAN_POINT('Ctrl Pts',(3.00946442616674,1.,-2.42421849439625));
#71055=CARTESIAN_POINT('Ctrl Pts',(3.00264868586038,-1.,-2.42090763946812));
#71056=CARTESIAN_POINT('Ctrl Pts',(3.00264868586038,1.,-2.42090763946812));
#71057=CARTESIAN_POINT('Ctrl Pts',(2.99590509293561,-1.,-2.4175732450056));
#71058=CARTESIAN_POINT('Ctrl Pts',(2.99590509293561,1.,-2.4175732450056));
#71059=CARTESIAN_POINT('Ctrl Pts',(2.98927983005851,-1.,-2.4142506419963));
#71060=CARTESIAN_POINT('Ctrl Pts',(2.98927983005851,1.,-2.4142506419963));
#71061=CARTESIAN_POINT('Ctrl Pts',(2.98280015815132,-1.,-2.41095909342591));
#71062=CARTESIAN_POINT('Ctrl Pts',(2.98280015815132,1.,-2.41095909342591));
#71063=CARTESIAN_POINT('Ctrl Pts',(2.97646002822395,-1.,-2.40768975073691));
#71064=CARTESIAN_POINT('Ctrl Pts',(2.97646002822395,1.,-2.40768975073691));
#71065=CARTESIAN_POINT('Ctrl Pts',(2.97019641312272,-1.,-2.40438604734848));
#71066=CARTESIAN_POINT('Ctrl Pts',(2.97019641312272,1.,-2.40438604734848));
#71067=CARTESIAN_POINT('Ctrl Pts',(2.9639043224018,-1.,-2.40095565711535));
#71068=CARTESIAN_POINT('Ctrl Pts',(2.9639043224018,1.,-2.40095565711535));
#71069=CARTESIAN_POINT('Ctrl Pts',(2.95748006482811,-1.,-2.39730553974412));
#71070=CARTESIAN_POINT('Ctrl Pts',(2.95748006482811,1.,-2.39730553974412));
#71071=CARTESIAN_POINT('Ctrl Pts',(2.95085857128372,-1.,-2.39337207631613));
#71072=CARTESIAN_POINT('Ctrl Pts',(2.95085857128372,1.,-2.39337207631613));
#71073=CARTESIAN_POINT('Ctrl Pts',(2.94404820669135,-1.,-2.38914929090806));
#71074=CARTESIAN_POINT('Ctrl Pts',(2.94404820669135,1.,-2.38914929090806));
#71075=CARTESIAN_POINT('Ctrl Pts',(2.93717903280599,-1.,-2.38472771516476));
#71076=CARTESIAN_POINT('Ctrl Pts',(2.93717903280599,1.,-2.38472771516476));
#71077=CARTESIAN_POINT('Ctrl Pts',(2.93049643640517,-1.,-2.3802898958232));
#71078=CARTESIAN_POINT('Ctrl Pts',(2.93049643640517,1.,-2.3802898958232));
#71079=CARTESIAN_POINT('Ctrl Pts',(2.92430340582912,-1.,-2.37606510524271));
#71080=CARTESIAN_POINT('Ctrl Pts',(2.92430340582912,1.,-2.37606510524271));
#71081=CARTESIAN_POINT('Ctrl Pts',(2.9189150379156,-1.,-2.37229381109939));
#71082=CARTESIAN_POINT('Ctrl Pts',(2.9189150379156,1.,-2.37229381109939));
#71083=CARTESIAN_POINT('Ctrl Pts',(2.91461249883016,-1.,-2.36919161373074));
#71084=CARTESIAN_POINT('Ctrl Pts',(2.91461249883016,1.,-2.36919161373074));
#71085=CARTESIAN_POINT('Ctrl Pts',(2.9115863784165,-1.,-2.36690501170317));
#71086=CARTESIAN_POINT('Ctrl Pts',(2.9115863784165,1.,-2.36690501170317));
#71087=CARTESIAN_POINT('Ctrl Pts',(2.91025813829606,-1.,-2.36578327194396));
#71088=CARTESIAN_POINT('Ctrl Pts',(2.91025813829606,1.,-2.36578327194396));
#71089=CARTESIAN_POINT('Ctrl Pts',(2.90989022547738,-1.,-2.36535052956704));
#71090=CARTESIAN_POINT('Ctrl Pts',(2.90989022547738,1.,-2.36535052956704));
#71091=CARTESIAN_POINT('Ctrl Pts',(2.90992398626098,-1.,-2.36524348105023));
#71092=CARTESIAN_POINT('Ctrl Pts',(2.90992398626098,1.,-2.36524348105023));
#71093=CARTESIAN_POINT('Ctrl Pts',(2.91001063062876,-1.,-2.36523532225181));
#71094=CARTESIAN_POINT('Ctrl Pts',(2.91001063062876,1.,-2.36523532225181));
#71095=CARTESIAN_POINT('',(3.35260583073571,1.,-2.52982887637028));
#71096=CARTESIAN_POINT('Ctrl Pts',(3.35260583073571,1.,-2.52982887637028));
#71097=CARTESIAN_POINT('Ctrl Pts',(3.35105973714426,1.,-2.52954136549357));
#71098=CARTESIAN_POINT('Ctrl Pts',(3.34796903577628,1.,-2.5289632161143));
#71099=CARTESIAN_POINT('Ctrl Pts',(3.34333744117093,1.,-2.52808660916879));
#71100=CARTESIAN_POINT('Ctrl Pts',(3.33717090000955,1.,-2.52689902691551));
#71101=CARTESIAN_POINT('Ctrl Pts',(3.32947762189049,1.,-2.52538321165774));
#71102=CARTESIAN_POINT('Ctrl Pts',(3.32179931079521,1.,-2.52383598396878));
#71103=CARTESIAN_POINT('Ctrl Pts',(3.31413607874727,1.,-2.52225724871375));
#71104=CARTESIAN_POINT('Ctrl Pts',(3.30648808814986,1.,-2.52064689568167));
#71105=CARTESIAN_POINT('Ctrl Pts',(3.29885556387661,1.,-2.51900480700548));
#71106=CARTESIAN_POINT('Ctrl Pts',(3.2912387729863,1.,-2.51733085123316));
#71107=CARTESIAN_POINT('Ctrl Pts',(3.28363799702583,1.,-2.51562487464215));
#71108=CARTESIAN_POINT('Ctrl Pts',(3.27605350473048,1.,-2.51388669270329));
#71109=CARTESIAN_POINT('Ctrl Pts',(3.26848552888271,1.,-2.51211608411539));
#71110=CARTESIAN_POINT('Ctrl Pts',(3.26093423001716,1.,-2.51031277813697));
#71111=CARTESIAN_POINT('Ctrl Pts',(3.25339971461265,1.,-2.50847647070936));
#71112=CARTESIAN_POINT('Ctrl Pts',(3.24588208984042,1.,-2.50660685940645));
#71113=CARTESIAN_POINT('Ctrl Pts',(3.23838151080383,1.,-2.50470367580078));
#71114=CARTESIAN_POINT('Ctrl Pts',(3.23089822320596,1.,-2.50276671338074));
#71115=CARTESIAN_POINT('Ctrl Pts',(3.22343262620387,1.,-2.5007958720187));
#71116=CARTESIAN_POINT('Ctrl Pts',(3.21598526261157,1.,-2.49879114599293));
#71117=CARTESIAN_POINT('Ctrl Pts',(3.2085566984974,1.,-2.49675252647298));
#71118=CARTESIAN_POINT('Ctrl Pts',(3.20114742397549,1.,-2.49467992057726));
#71119=CARTESIAN_POINT('Ctrl Pts',(3.19375775555814,1.,-2.4925730723986));
#71120=CARTESIAN_POINT('Ctrl Pts',(3.18638771282315,1.,-2.49043146334095));
#71121=CARTESIAN_POINT('Ctrl Pts',(3.17903698136678,1.,-2.48825428288243));
#71122=CARTESIAN_POINT('Ctrl Pts',(3.17170518863357,1.,-2.48604065348619));
#71123=CARTESIAN_POINT('Ctrl Pts',(3.16439213290181,1.,-2.48378981792739));
#71124=CARTESIAN_POINT('Ctrl Pts',(3.15709802322735,1.,-2.48150133566568));
#71125=CARTESIAN_POINT('Ctrl Pts',(3.14982373241335,1.,-2.47917529057016));
#71126=CARTESIAN_POINT('Ctrl Pts',(3.14257099546531,1.,-2.47681245356095));
#71127=CARTESIAN_POINT('Ctrl Pts',(3.13534181229282,1.,-2.47441378371923));
#71128=CARTESIAN_POINT('Ctrl Pts',(3.12813790805948,1.,-2.47197997765868));
#71129=CARTESIAN_POINT('Ctrl Pts',(3.12096015766984,1.,-2.4695109894747));
#71130=CARTESIAN_POINT('Ctrl Pts',(3.11380805536124,1.,-2.46700558843507));
#71131=CARTESIAN_POINT('Ctrl Pts',(3.10667907901981,1.,-2.46446082979645));
#71132=CARTESIAN_POINT('Ctrl Pts',(3.09956993697048,1.,-2.4618730850188));
#71133=CARTESIAN_POINT('Ctrl Pts',(3.09247787931881,1.,-2.45923912563875));
#71134=CARTESIAN_POINT('Ctrl Pts',(3.08540206545313,1.,-2.45655725437037));
#71135=CARTESIAN_POINT('Ctrl Pts',(3.07834472886145,1.,-2.45382826787795));
#71136=CARTESIAN_POINT('Ctrl Pts',(3.0713129052131,1.,-2.45105688854432));
#71137=CARTESIAN_POINT('Ctrl Pts',(3.06431596421422,1.,-2.44824970516558));
#71138=CARTESIAN_POINT('Ctrl Pts',(3.05736242671521,1.,-2.44541251892568));
#71139=CARTESIAN_POINT('Ctrl Pts',(3.05045678021509,1.,-2.44254768923109));
#71140=CARTESIAN_POINT('Ctrl Pts',(3.04359685040545,1.,-2.43965194061849));
#71141=CARTESIAN_POINT('Ctrl Pts',(3.03676949672797,1.,-2.43671278042394));
#71142=CARTESIAN_POINT('Ctrl Pts',(3.02995534946946,1.,-2.43371241361462));
#71143=CARTESIAN_POINT('Ctrl Pts',(3.02313656035977,1.,-2.43063415586615));
#71144=CARTESIAN_POINT('Ctrl Pts',(3.01630420830493,1.,-2.4274685626416));
#71145=CARTESIAN_POINT('Ctrl Pts',(3.00946442616674,1.,-2.42421849439625));
#71146=CARTESIAN_POINT('Ctrl Pts',(3.00264868586038,1.,-2.42090763946812));
#71147=CARTESIAN_POINT('Ctrl Pts',(2.99590509293561,1.,-2.4175732450056));
#71148=CARTESIAN_POINT('Ctrl Pts',(2.98927983005851,1.,-2.4142506419963));
#71149=CARTESIAN_POINT('Ctrl Pts',(2.98280015815132,1.,-2.41095909342591));
#71150=CARTESIAN_POINT('Ctrl Pts',(2.97646002822395,1.,-2.40768975073691));
#71151=CARTESIAN_POINT('Ctrl Pts',(2.97019641312272,1.,-2.40438604734848));
#71152=CARTESIAN_POINT('Ctrl Pts',(2.9639043224018,1.,-2.40095565711535));
#71153=CARTESIAN_POINT('Ctrl Pts',(2.95748006482811,1.,-2.39730553974412));
#71154=CARTESIAN_POINT('Ctrl Pts',(2.95085857128372,1.,-2.39337207631613));
#71155=CARTESIAN_POINT('Ctrl Pts',(2.94404820669135,1.,-2.38914929090806));
#71156=CARTESIAN_POINT('Ctrl Pts',(2.93717903280599,1.,-2.38472771516476));
#71157=CARTESIAN_POINT('Ctrl Pts',(2.93049643640517,1.,-2.3802898958232));
#71158=CARTESIAN_POINT('Ctrl Pts',(2.92430340582912,1.,-2.37606510524271));
#71159=CARTESIAN_POINT('Ctrl Pts',(2.9189150379156,1.,-2.37229381109939));
#71160=CARTESIAN_POINT('Ctrl Pts',(2.91461249883016,1.,-2.36919161373074));
#71161=CARTESIAN_POINT('Ctrl Pts',(2.91181344022628,1.,-2.36707658451709));
#71162=CARTESIAN_POINT('Ctrl Pts',(2.91051690822262,1.,-2.36599991765853));
#71163=CARTESIAN_POINT('Ctrl Pts',(2.9100577052777,1.,-2.36553202948741));
#71164=CARTESIAN_POINT('Ctrl Pts',(2.90995756655558,1.,-2.3653621118858));
#71165=CARTESIAN_POINT('Ctrl Pts',(2.90994629141562,1.,-2.36531447826213));
#71166=CARTESIAN_POINT('',(3.35260583073571,0.,-2.52982887637028));
#71167=CARTESIAN_POINT('Ctrl Pts',(3.1487152044751,-1.,-2.03668666247593));
#71168=CARTESIAN_POINT('Ctrl Pts',(3.1487152044751,1.,-2.03668666247593));
#71169=CARTESIAN_POINT('Ctrl Pts',(3.14869618937258,-1.,-2.03660173757879));
#71170=CARTESIAN_POINT('Ctrl Pts',(3.14869618937258,1.,-2.03660173757879));
#71171=CARTESIAN_POINT('Ctrl Pts',(3.14878756590812,-1.,-2.03653654935592));
#71172=CARTESIAN_POINT('Ctrl Pts',(3.14878756590812,1.,-2.03653654935592));
#71173=CARTESIAN_POINT('Ctrl Pts',(3.14931281968048,-1.,-2.03675273049189));
#71174=CARTESIAN_POINT('Ctrl Pts',(3.14931281968048,1.,-2.03675273049189));
#71175=CARTESIAN_POINT('Ctrl Pts',(3.15079010635742,-1.,-2.03766932526445));
#71176=CARTESIAN_POINT('Ctrl Pts',(3.15079010635742,1.,-2.03766932526445));
#71177=CARTESIAN_POINT('Ctrl Pts',(3.15389991674792,-1.,-2.03984073791519));
#71178=CARTESIAN_POINT('Ctrl Pts',(3.15389991674792,1.,-2.03984073791519));
#71179=CARTESIAN_POINT('Ctrl Pts',(3.15817983946367,-1.,-2.04297406404027));
#71180=CARTESIAN_POINT('Ctrl Pts',(3.15817983946367,1.,-2.04297406404027));
#71181=CARTESIAN_POINT('Ctrl Pts',(3.16343165058912,-1.,-2.04693331247446));
#71182=CARTESIAN_POINT('Ctrl Pts',(3.16343165058912,1.,-2.04693331247446));
#71183=CARTESIAN_POINT('Ctrl Pts',(3.16936341689527,-1.,-2.05151770247233));
#71184=CARTESIAN_POINT('Ctrl Pts',(3.16936341689527,1.,-2.05151770247233));
#71185=CARTESIAN_POINT('Ctrl Pts',(3.17564906975371,-1.,-2.05650186773132));
#71186=CARTESIAN_POINT('Ctrl Pts',(3.17564906975371,1.,-2.05650186773132));
#71187=CARTESIAN_POINT('Ctrl Pts',(3.18197692964614,-1.,-2.06166849827101));
#71188=CARTESIAN_POINT('Ctrl Pts',(3.18197692964614,1.,-2.06166849827101));
#71189=CARTESIAN_POINT('Ctrl Pts',(3.18809755562368,-1.,-2.06684062744112));
#71190=CARTESIAN_POINT('Ctrl Pts',(3.18809755562368,1.,-2.06684062744112));
#71191=CARTESIAN_POINT('Ctrl Pts',(3.19388465568252,-1.,-2.07192253497857));
#71192=CARTESIAN_POINT('Ctrl Pts',(3.19388465568252,1.,-2.07192253497857));
#71193=CARTESIAN_POINT('Ctrl Pts',(3.19934132836019,-1.,-2.07690441870722));
#71194=CARTESIAN_POINT('Ctrl Pts',(3.19934132836019,1.,-2.07690441870722));
#71195=CARTESIAN_POINT('Ctrl Pts',(3.2045481863073,-1.,-2.08182850370878));
#71196=CARTESIAN_POINT('Ctrl Pts',(3.2045481863073,1.,-2.08182850370878));
#71197=CARTESIAN_POINT('Ctrl Pts',(3.20962575845463,-1.,-2.08676465517455));
#71198=CARTESIAN_POINT('Ctrl Pts',(3.20962575845463,1.,-2.08676465517455));
#71199=CARTESIAN_POINT('Ctrl Pts',(3.21469429601654,-1.,-2.09178419460443));
#71200=CARTESIAN_POINT('Ctrl Pts',(3.21469429601654,1.,-2.09178419460443));
#71201=CARTESIAN_POINT('Ctrl Pts',(3.21982707347009,-1.,-2.09692958434895));
#71202=CARTESIAN_POINT('Ctrl Pts',(3.21982707347009,1.,-2.09692958434895));
#71203=CARTESIAN_POINT('Ctrl Pts',(3.22503437553434,-1.,-2.10220384298492));
#71204=CARTESIAN_POINT('Ctrl Pts',(3.22503437553434,1.,-2.10220384298492));
#71205=CARTESIAN_POINT('Ctrl Pts',(3.23028945793289,-1.,-2.10758699642451));
#71206=CARTESIAN_POINT('Ctrl Pts',(3.23028945793289,1.,-2.10758699642451));
#71207=CARTESIAN_POINT('Ctrl Pts',(3.23554444767099,-1.,-2.11304604021773));
#71208=CARTESIAN_POINT('Ctrl Pts',(3.23554444767099,1.,-2.11304604021773));
#71209=CARTESIAN_POINT('Ctrl Pts',(3.24074905517293,-1.,-2.11854673326979));
#71210=CARTESIAN_POINT('Ctrl Pts',(3.24074905517293,1.,-2.11854673326979));
#71211=CARTESIAN_POINT('Ctrl Pts',(3.24587102613376,-1.,-2.12406646410962));
#71212=CARTESIAN_POINT('Ctrl Pts',(3.24587102613376,1.,-2.12406646410962));
#71213=CARTESIAN_POINT('Ctrl Pts',(3.25090574494028,-1.,-2.12960028396832));
#71214=CARTESIAN_POINT('Ctrl Pts',(3.25090574494028,1.,-2.12960028396832));
#71215=CARTESIAN_POINT('Ctrl Pts',(3.25586495065054,-1.,-2.13515375878803));
#71216=CARTESIAN_POINT('Ctrl Pts',(3.25586495065054,1.,-2.13515375878803));
#71217=CARTESIAN_POINT('Ctrl Pts',(3.26077002641879,-1.,-2.14073870754264));
#71218=CARTESIAN_POINT('Ctrl Pts',(3.26077002641879,1.,-2.14073870754264));
#71219=CARTESIAN_POINT('Ctrl Pts',(3.26564388189759,-1.,-2.1463680529566));
#71220=CARTESIAN_POINT('Ctrl Pts',(3.26564388189759,1.,-2.1463680529566));
#71221=CARTESIAN_POINT('Ctrl Pts',(3.27050245897228,-1.,-2.15205043199808));
#71222=CARTESIAN_POINT('Ctrl Pts',(3.27050245897228,1.,-2.15205043199808));
#71223=CARTESIAN_POINT('Ctrl Pts',(3.27534954469187,-1.,-2.15778690038347));
#71224=CARTESIAN_POINT('Ctrl Pts',(3.27534954469187,1.,-2.15778690038347));
#71225=CARTESIAN_POINT('Ctrl Pts',(3.280181508414,-1.,-2.16357391934425));
#71226=CARTESIAN_POINT('Ctrl Pts',(3.280181508414,1.,-2.16357391934425));
#71227=CARTESIAN_POINT('Ctrl Pts',(3.28499019979724,-1.,-2.16940517773455));
#71228=CARTESIAN_POINT('Ctrl Pts',(3.28499019979724,1.,-2.16940517773455));
#71229=CARTESIAN_POINT('Ctrl Pts',(3.28976645712568,-1.,-2.17527380048423));
#71230=CARTESIAN_POINT('Ctrl Pts',(3.28976645712568,1.,-2.17527380048423));
#71231=CARTESIAN_POINT('Ctrl Pts',(3.2945036150049,-1.,-2.18117455557065));
#71232=CARTESIAN_POINT('Ctrl Pts',(3.2945036150049,1.,-2.18117455557065));
#71233=CARTESIAN_POINT('Ctrl Pts',(3.29920022557639,-1.,-2.18710556500327));
#71234=CARTESIAN_POINT('Ctrl Pts',(3.29920022557639,1.,-2.18710556500327));
#71235=CARTESIAN_POINT('Ctrl Pts',(3.30385816281831,-1.,-2.19306710376111));
#71236=CARTESIAN_POINT('Ctrl Pts',(3.30385816281831,1.,-2.19306710376111));
#71237=CARTESIAN_POINT('Ctrl Pts',(3.30848134694595,-1.,-2.19906078949923));
#71238=CARTESIAN_POINT('Ctrl Pts',(3.30848134694595,1.,-2.19906078949923));
#71239=CARTESIAN_POINT('Ctrl Pts',(3.31307424608949,-1.,-2.20508863150607));
#71240=CARTESIAN_POINT('Ctrl Pts',(3.31307424608949,1.,-2.20508863150607));
#71241=CARTESIAN_POINT('Ctrl Pts',(3.31764044024235,-1.,-2.21115211847875));
#71242=CARTESIAN_POINT('Ctrl Pts',(3.31764044024235,1.,-2.21115211847875));
#71243=CARTESIAN_POINT('Ctrl Pts',(3.32218125618968,-1.,-2.21725135110898));
#71244=CARTESIAN_POINT('Ctrl Pts',(3.32218125618968,1.,-2.21725135110898));
#71245=CARTESIAN_POINT('Ctrl Pts',(3.3266964672289,-1.,-2.22338548312772));
#71246=CARTESIAN_POINT('Ctrl Pts',(3.3266964672289,1.,-2.22338548312772));
#71247=CARTESIAN_POINT('Ctrl Pts',(3.33118487773611,-1.,-2.22955308907233));
#71248=CARTESIAN_POINT('Ctrl Pts',(3.33118487773611,1.,-2.22955308907233));
#71249=CARTESIAN_POINT('Ctrl Pts',(3.33564495756481,-1.,-2.23575256328812));
#71250=CARTESIAN_POINT('Ctrl Pts',(3.33564495756481,1.,-2.23575256328812));
#71251=CARTESIAN_POINT('Ctrl Pts',(3.34007543738025,-1.,-2.24198249391422));
#71252=CARTESIAN_POINT('Ctrl Pts',(3.34007543738025,1.,-2.24198249391422));
#71253=CARTESIAN_POINT('Ctrl Pts',(3.34447596770723,-1.,-2.24824207678256));
#71254=CARTESIAN_POINT('Ctrl Pts',(3.34447596770723,1.,-2.24824207678256));
#71255=CARTESIAN_POINT('Ctrl Pts',(3.34884690292285,-1.,-2.25453097693483));
#71256=CARTESIAN_POINT('Ctrl Pts',(3.34884690292285,1.,-2.25453097693483));
#71257=CARTESIAN_POINT('Ctrl Pts',(3.35318902552626,-1.,-2.26084915222449));
#71258=CARTESIAN_POINT('Ctrl Pts',(3.35318902552626,1.,-2.26084915222449));
#71259=CARTESIAN_POINT('Ctrl Pts',(3.35750328523061,-1.,-2.2671966857991));
#71260=CARTESIAN_POINT('Ctrl Pts',(3.35750328523061,1.,-2.2671966857991));
#71261=CARTESIAN_POINT('Ctrl Pts',(3.36179055004409,-1.,-2.2735736262093));
#71262=CARTESIAN_POINT('Ctrl Pts',(3.36179055004409,1.,-2.2735736262093));
#71263=CARTESIAN_POINT('Ctrl Pts',(3.36605130713076,-1.,-2.27997979458037));
#71264=CARTESIAN_POINT('Ctrl Pts',(3.36605130713076,1.,-2.27997979458037));
#71265=CARTESIAN_POINT('Ctrl Pts',(3.37028570206488,-1.,-2.28641481081137));
#71266=CARTESIAN_POINT('Ctrl Pts',(3.37028570206488,1.,-2.28641481081137));
#71267=CARTESIAN_POINT('Ctrl Pts',(3.37449367172826,-1.,-2.29287818007393));
#71268=CARTESIAN_POINT('Ctrl Pts',(3.37449367172826,1.,-2.29287818007393));
#71269=CARTESIAN_POINT('Ctrl Pts',(3.37867504959433,-1.,-2.29936936127624));
#71270=CARTESIAN_POINT('Ctrl Pts',(3.37867504959433,1.,-2.29936936127624));
#71271=CARTESIAN_POINT('Ctrl Pts',(3.3828296733661,-1.,-2.30588783640343));
#71272=CARTESIAN_POINT('Ctrl Pts',(3.3828296733661,1.,-2.30588783640343));
#71273=CARTESIAN_POINT('Ctrl Pts',(3.38695751492462,-1.,-2.31243319489367));
#71274=CARTESIAN_POINT('Ctrl Pts',(3.38695751492462,1.,-2.31243319489367));
#71275=CARTESIAN_POINT('Ctrl Pts',(3.39105869474822,-1.,-2.31900513925424));
#71276=CARTESIAN_POINT('Ctrl Pts',(3.39105869474822,1.,-2.31900513925424));
#71277=CARTESIAN_POINT('Ctrl Pts',(3.39513342019756,-1.,-2.3256034390248));
#71278=CARTESIAN_POINT('Ctrl Pts',(3.39513342019756,1.,-2.3256034390248));
#71279=CARTESIAN_POINT('Ctrl Pts',(3.39918194577956,-1.,-2.33222789882489));
#71280=CARTESIAN_POINT('Ctrl Pts',(3.39918194577956,1.,-2.33222789882489));
#71281=CARTESIAN_POINT('Ctrl Pts',(3.40320452776743,-1.,-2.33887832342782));
#71282=CARTESIAN_POINT('Ctrl Pts',(3.40320452776743,1.,-2.33887832342782));
#71283=CARTESIAN_POINT('Ctrl Pts',(3.40720137404297,-1.,-2.34555447649188));
#71284=CARTESIAN_POINT('Ctrl Pts',(3.40720137404297,1.,-2.34555447649188));
#71285=CARTESIAN_POINT('Ctrl Pts',(3.41117262314119,-1.,-2.35225606824109));
#71286=CARTESIAN_POINT('Ctrl Pts',(3.41117262314119,1.,-2.35225606824109));
#71287=CARTESIAN_POINT('Ctrl Pts',(3.41511836751469,-1.,-2.35898278606946));
#71288=CARTESIAN_POINT('Ctrl Pts',(3.41511836751469,1.,-2.35898278606946));
#71289=CARTESIAN_POINT('Ctrl Pts',(3.41903866635852,-1.,-2.36573431470642));
#71290=CARTESIAN_POINT('Ctrl Pts',(3.41903866635852,1.,-2.36573431470642));
#71291=CARTESIAN_POINT('Ctrl Pts',(3.42293356216511,-1.,-2.37251035954292));
#71292=CARTESIAN_POINT('Ctrl Pts',(3.42293356216511,1.,-2.37251035954292));
#71293=CARTESIAN_POINT('Ctrl Pts',(3.42680309754399,-1.,-2.37931067028926));
#71294=CARTESIAN_POINT('Ctrl Pts',(3.42680309754399,1.,-2.37931067028926));
#71295=CARTESIAN_POINT('Ctrl Pts',(3.43064732712919,-1.,-2.38613505843552));
#71296=CARTESIAN_POINT('Ctrl Pts',(3.43064732712919,1.,-2.38613505843552));
#71297=CARTESIAN_POINT('Ctrl Pts',(3.4344663067854,-1.,-2.39298338804493));
#71298=CARTESIAN_POINT('Ctrl Pts',(3.4344663067854,1.,-2.39298338804493));
#71299=CARTESIAN_POINT('Ctrl Pts',(3.43750133064416,-1.,-2.39848113410292));
#71300=CARTESIAN_POINT('Ctrl Pts',(3.43750133064416,1.,-2.39848113410292));
#71301=CARTESIAN_POINT('Ctrl Pts',(3.43976627484234,-1.,-2.40261515589405));
#71302=CARTESIAN_POINT('Ctrl Pts',(3.43976627484234,1.,-2.40261515589405));
#71303=CARTESIAN_POINT('Ctrl Pts',(3.44127120683039,-1.,-2.4053759295909));
#71304=CARTESIAN_POINT('Ctrl Pts',(3.44127120683039,1.,-2.4053759295909));
#71305=CARTESIAN_POINT('Ctrl Pts',(3.44202241512147,-1.,-2.40675750623143));
#71306=CARTESIAN_POINT('Ctrl Pts',(3.44202241512147,1.,-2.40675750623143));
#71307=CARTESIAN_POINT('',(3.14877060440327,1.,-2.03660101169715));
#71308=CARTESIAN_POINT('Ctrl Pts',(3.14877060440327,-1.,-2.03660101169715));
#71309=CARTESIAN_POINT('Ctrl Pts',(3.14877060440327,-0.666666666666667,
-2.03660101169715));
#71310=CARTESIAN_POINT('Ctrl Pts',(3.14877060440327,-0.333333333333333,
-2.03660101169715));
#71311=CARTESIAN_POINT('Ctrl Pts',(3.14877060440327,0.333333333333333,-2.03660101169715));
#71312=CARTESIAN_POINT('Ctrl Pts',(3.14877060440328,0.666666666666667,-2.03660101169714));
#71313=CARTESIAN_POINT('Ctrl Pts',(3.14877060440328,1.,-2.03660101169714));
#71314=CARTESIAN_POINT('',(3.44202241512147,1.,-2.40675750623143));
#71315=CARTESIAN_POINT('',(3.44202241512147,0.,-2.40675750623143));
#71316=CARTESIAN_POINT('Ctrl Pts',(3.14877060440327,1.,-2.03660101169715));
#71317=CARTESIAN_POINT('Ctrl Pts',(3.14881939088124,1.,-2.03659701539259));
#71318=CARTESIAN_POINT('Ctrl Pts',(3.1490119366901,1.,-2.03663974554932));
#71319=CARTESIAN_POINT('Ctrl Pts',(3.14959882629804,1.,-2.03693188810544));
#71320=CARTESIAN_POINT('Ctrl Pts',(3.15102344775328,1.,-2.03783225495961));
#71321=CARTESIAN_POINT('Ctrl Pts',(3.15389991674792,1.,-2.03984073791519));
#71322=CARTESIAN_POINT('Ctrl Pts',(3.15817983946367,1.,-2.04297406404027));
#71323=CARTESIAN_POINT('Ctrl Pts',(3.16343165058912,1.,-2.04693331247446));
#71324=CARTESIAN_POINT('Ctrl Pts',(3.16936341689527,1.,-2.05151770247233));
#71325=CARTESIAN_POINT('Ctrl Pts',(3.17564906975371,1.,-2.05650186773132));
#71326=CARTESIAN_POINT('Ctrl Pts',(3.18197692964614,1.,-2.06166849827101));
#71327=CARTESIAN_POINT('Ctrl Pts',(3.18809755562368,1.,-2.06684062744112));
#71328=CARTESIAN_POINT('Ctrl Pts',(3.19388465568252,1.,-2.07192253497857));
#71329=CARTESIAN_POINT('Ctrl Pts',(3.19934132836019,1.,-2.07690441870722));
#71330=CARTESIAN_POINT('Ctrl Pts',(3.2045481863073,1.,-2.08182850370878));
#71331=CARTESIAN_POINT('Ctrl Pts',(3.20962575845463,1.,-2.08676465517455));
#71332=CARTESIAN_POINT('Ctrl Pts',(3.21469429601654,1.,-2.09178419460443));
#71333=CARTESIAN_POINT('Ctrl Pts',(3.21982707347009,1.,-2.09692958434895));
#71334=CARTESIAN_POINT('Ctrl Pts',(3.22503437553434,1.,-2.10220384298492));
#71335=CARTESIAN_POINT('Ctrl Pts',(3.23028945793289,1.,-2.10758699642451));
#71336=CARTESIAN_POINT('Ctrl Pts',(3.23554444767099,1.,-2.11304604021773));
#71337=CARTESIAN_POINT('Ctrl Pts',(3.24074905517293,1.,-2.11854673326979));
#71338=CARTESIAN_POINT('Ctrl Pts',(3.24587102613376,1.,-2.12406646410962));
#71339=CARTESIAN_POINT('Ctrl Pts',(3.25090574494028,1.,-2.12960028396832));
#71340=CARTESIAN_POINT('Ctrl Pts',(3.25586495065054,1.,-2.13515375878803));
#71341=CARTESIAN_POINT('Ctrl Pts',(3.26077002641879,1.,-2.14073870754264));
#71342=CARTESIAN_POINT('Ctrl Pts',(3.26564388189759,1.,-2.1463680529566));
#71343=CARTESIAN_POINT('Ctrl Pts',(3.27050245897228,1.,-2.15205043199808));
#71344=CARTESIAN_POINT('Ctrl Pts',(3.27534954469187,1.,-2.15778690038347));
#71345=CARTESIAN_POINT('Ctrl Pts',(3.280181508414,1.,-2.16357391934425));
#71346=CARTESIAN_POINT('Ctrl Pts',(3.28499019979724,1.,-2.16940517773455));
#71347=CARTESIAN_POINT('Ctrl Pts',(3.28976645712568,1.,-2.17527380048423));
#71348=CARTESIAN_POINT('Ctrl Pts',(3.2945036150049,1.,-2.18117455557065));
#71349=CARTESIAN_POINT('Ctrl Pts',(3.29920022557639,1.,-2.18710556500327));
#71350=CARTESIAN_POINT('Ctrl Pts',(3.30385816281831,1.,-2.19306710376111));
#71351=CARTESIAN_POINT('Ctrl Pts',(3.30848134694595,1.,-2.19906078949923));
#71352=CARTESIAN_POINT('Ctrl Pts',(3.31307424608949,1.,-2.20508863150607));
#71353=CARTESIAN_POINT('Ctrl Pts',(3.31764044024235,1.,-2.21115211847875));
#71354=CARTESIAN_POINT('Ctrl Pts',(3.32218125618968,1.,-2.21725135110898));
#71355=CARTESIAN_POINT('Ctrl Pts',(3.3266964672289,1.,-2.22338548312772));
#71356=CARTESIAN_POINT('Ctrl Pts',(3.33118487773611,1.,-2.22955308907233));
#71357=CARTESIAN_POINT('Ctrl Pts',(3.33564495756481,1.,-2.23575256328812));
#71358=CARTESIAN_POINT('Ctrl Pts',(3.34007543738025,1.,-2.24198249391422));
#71359=CARTESIAN_POINT('Ctrl Pts',(3.34447596770723,1.,-2.24824207678256));
#71360=CARTESIAN_POINT('Ctrl Pts',(3.34884690292285,1.,-2.25453097693483));
#71361=CARTESIAN_POINT('Ctrl Pts',(3.35318902552626,1.,-2.26084915222449));
#71362=CARTESIAN_POINT('Ctrl Pts',(3.35750328523061,1.,-2.2671966857991));
#71363=CARTESIAN_POINT('Ctrl Pts',(3.36179055004409,1.,-2.2735736262093));
#71364=CARTESIAN_POINT('Ctrl Pts',(3.36605130713076,1.,-2.27997979458037));
#71365=CARTESIAN_POINT('Ctrl Pts',(3.37028570206488,1.,-2.28641481081137));
#71366=CARTESIAN_POINT('Ctrl Pts',(3.37449367172826,1.,-2.29287818007393));
#71367=CARTESIAN_POINT('Ctrl Pts',(3.37867504959433,1.,-2.29936936127624));
#71368=CARTESIAN_POINT('Ctrl Pts',(3.3828296733661,1.,-2.30588783640343));
#71369=CARTESIAN_POINT('Ctrl Pts',(3.38695751492462,1.,-2.31243319489367));
#71370=CARTESIAN_POINT('Ctrl Pts',(3.39105869474822,1.,-2.31900513925424));
#71371=CARTESIAN_POINT('Ctrl Pts',(3.39513342019756,1.,-2.3256034390248));
#71372=CARTESIAN_POINT('Ctrl Pts',(3.39918194577956,1.,-2.33222789882489));
#71373=CARTESIAN_POINT('Ctrl Pts',(3.40320452776743,1.,-2.33887832342782));
#71374=CARTESIAN_POINT('Ctrl Pts',(3.40720137404297,1.,-2.34555447649188));
#71375=CARTESIAN_POINT('Ctrl Pts',(3.41117262314119,1.,-2.35225606824109));
#71376=CARTESIAN_POINT('Ctrl Pts',(3.41511836751469,1.,-2.35898278606946));
#71377=CARTESIAN_POINT('Ctrl Pts',(3.41903866635852,1.,-2.36573431470642));
#71378=CARTESIAN_POINT('Ctrl Pts',(3.42293356216511,1.,-2.37251035954292));
#71379=CARTESIAN_POINT('Ctrl Pts',(3.42680309754399,1.,-2.37931067028926));
#71380=CARTESIAN_POINT('Ctrl Pts',(3.43064732712919,1.,-2.38613505843552));
#71381=CARTESIAN_POINT('Ctrl Pts',(3.4344663067854,1.,-2.39298338804493));
#71382=CARTESIAN_POINT('Ctrl Pts',(3.43750133064416,1.,-2.39848113410292));
#71383=CARTESIAN_POINT('Ctrl Pts',(3.43976627484234,1.,-2.40261515589405));
#71384=CARTESIAN_POINT('Ctrl Pts',(3.44127120683039,1.,-2.4053759295909));
#71385=CARTESIAN_POINT('Ctrl Pts',(3.44202241512147,1.,-2.40675750623143));
#71386=CARTESIAN_POINT('Origin',(3.44202241512147,0.,-2.40675750623143));
#71387=CARTESIAN_POINT('',(3.35260583073571,1.,-2.52982887637028));
#71388=CARTESIAN_POINT('Origin',(0.,0.,0.));
#71389=CARTESIAN_POINT('',(3.24413672884812,1.,-1.88097764062697));
#71390=CARTESIAN_POINT('Origin',(0.,1.,0.));
#71391=CARTESIAN_POINT('Ctrl Pts',(3.24413672884812,1.,-1.88097764062697));
#71392=CARTESIAN_POINT('Ctrl Pts',(3.24413672884812,0.666666666666667,-1.88097764062697));
#71393=CARTESIAN_POINT('Ctrl Pts',(3.24413672884812,0.333333333333333,-1.88097764062697));
#71394=CARTESIAN_POINT('Ctrl Pts',(3.24413672884812,-0.333333333333333,
-1.88097764062697));
#71395=CARTESIAN_POINT('Ctrl Pts',(3.24413672884812,-0.666666666666667,
-1.88097764062697));
#71396=CARTESIAN_POINT('Ctrl Pts',(3.24413672884812,-1.,-1.88097764062697));
#71397=CARTESIAN_POINT('Ctrl Pts',(3.70708211654725,-1.,-1.97421938526992));
#71398=CARTESIAN_POINT('Ctrl Pts',(3.70708211654725,1.,-1.97421938526992));
#71399=CARTESIAN_POINT('Ctrl Pts',(3.70551008132332,-1.,-1.97417727645308));
#71400=CARTESIAN_POINT('Ctrl Pts',(3.70551008132332,1.,-1.97417727645308));
#71401=CARTESIAN_POINT('Ctrl Pts',(3.70236698912904,-1.,-1.97408973726715));
#71402=CARTESIAN_POINT('Ctrl Pts',(3.70236698912904,1.,-1.97408973726715));
#71403=CARTESIAN_POINT('Ctrl Pts',(3.6976552856004,-1.,-1.97394846383216));
#71404=CARTESIAN_POINT('Ctrl Pts',(3.6976552856004,1.,-1.97394846383216));
#71405=CARTESIAN_POINT('Ctrl Pts',(3.69137888599902,-1.,-1.97374016225483));
#71406=CARTESIAN_POINT('Ctrl Pts',(3.69137888599902,1.,-1.97374016225483));
#71407=CARTESIAN_POINT('Ctrl Pts',(3.68354319915092,-1.,-1.97344650304519));
#71408=CARTESIAN_POINT('Ctrl Pts',(3.68354319915092,1.,-1.97344650304519));
#71409=CARTESIAN_POINT('Ctrl Pts',(3.67571738107084,-1.,-1.97311947678517));
#71410=CARTESIAN_POINT('Ctrl Pts',(3.67571738107084,1.,-1.97311947678517));
#71411=CARTESIAN_POINT('Ctrl Pts',(3.66790152752075,-1.,-1.97275897198678));
#71412=CARTESIAN_POINT('Ctrl Pts',(3.66790152752075,1.,-1.97275897198678));
#71413=CARTESIAN_POINT('Ctrl Pts',(3.6600957816636,-1.,-1.9723648543905));
#71414=CARTESIAN_POINT('Ctrl Pts',(3.6600957816636,1.,-1.9723648543905));
#71415=CARTESIAN_POINT('Ctrl Pts',(3.652300347166,-1.,-1.9719369724024));
#71416=CARTESIAN_POINT('Ctrl Pts',(3.652300347166,1.,-1.9719369724024));
#71417=CARTESIAN_POINT('Ctrl Pts',(3.64451546723514,-1.,-1.97147515441164));
#71418=CARTESIAN_POINT('Ctrl Pts',(3.64451546723514,1.,-1.97147515441164));
#71419=CARTESIAN_POINT('Ctrl Pts',(3.63674139590412,-1.,-1.97097920454464));
#71420=CARTESIAN_POINT('Ctrl Pts',(3.63674139590412,1.,-1.97097920454464));
#71421=CARTESIAN_POINT('Ctrl Pts',(3.62897836973293,-1.,-1.97044889850463));
#71422=CARTESIAN_POINT('Ctrl Pts',(3.62897836973293,1.,-1.97044889850463));
#71423=CARTESIAN_POINT('Ctrl Pts',(3.62122658401893,-1.,-1.96988398129978));
#71424=CARTESIAN_POINT('Ctrl Pts',(3.62122658401893,1.,-1.96988398129978));
#71425=CARTESIAN_POINT('Ctrl Pts',(3.61348615496704,-1.,-1.96928416040877));
#71426=CARTESIAN_POINT('Ctrl Pts',(3.61348615496704,1.,-1.96928416040877));
#71427=CARTESIAN_POINT('Ctrl Pts',(3.60575714017989,-1.,-1.9686491188594));
#71428=CARTESIAN_POINT('Ctrl Pts',(3.60575714017989,1.,-1.9686491188594));
#71429=CARTESIAN_POINT('Ctrl Pts',(3.59803959819938,-1.,-1.96797854118369));
#71430=CARTESIAN_POINT('Ctrl Pts',(3.59803959819938,1.,-1.96797854118369));
#71431=CARTESIAN_POINT('Ctrl Pts',(3.59033364022801,-1.,-1.96727213799544));
#71432=CARTESIAN_POINT('Ctrl Pts',(3.59033364022801,1.,-1.96727213799544));
#71433=CARTESIAN_POINT('Ctrl Pts',(3.58263947663829,-1.,-1.96652966688911));
#71434=CARTESIAN_POINT('Ctrl Pts',(3.58263947663829,1.,-1.96652966688911));
#71435=CARTESIAN_POINT('Ctrl Pts',(3.57495748600959,-1.,-1.96575096652789));
#71436=CARTESIAN_POINT('Ctrl Pts',(3.57495748600959,1.,-1.96575096652789));
#71437=CARTESIAN_POINT('Ctrl Pts',(3.56728820357791,-1.,-1.96493594634567));
#71438=CARTESIAN_POINT('Ctrl Pts',(3.56728820357791,1.,-1.96493594634567));
#71439=CARTESIAN_POINT('Ctrl Pts',(3.55963218706096,-1.,-1.96408450906812));
#71440=CARTESIAN_POINT('Ctrl Pts',(3.55963218706096,1.,-1.96408450906812));
#71441=CARTESIAN_POINT('Ctrl Pts',(3.55198990600886,-1.,-1.96319648628644));
#71442=CARTESIAN_POINT('Ctrl Pts',(3.55198990600886,1.,-1.96319648628644));
#71443=CARTESIAN_POINT('Ctrl Pts',(3.54436163300443,-1.,-1.96227157573067));
#71444=CARTESIAN_POINT('Ctrl Pts',(3.54436163300443,1.,-1.96227157573067));
#71445=CARTESIAN_POINT('Ctrl Pts',(3.53674730625813,-1.,-1.96130926212689));
#71446=CARTESIAN_POINT('Ctrl Pts',(3.53674730625813,1.,-1.96130926212689));
#71447=CARTESIAN_POINT('Ctrl Pts',(3.52914648844351,-1.,-1.96030879411566));
#71448=CARTESIAN_POINT('Ctrl Pts',(3.52914648844351,1.,-1.96030879411566));
#71449=CARTESIAN_POINT('Ctrl Pts',(3.52155867431486,-1.,-1.95926936324461));
#71450=CARTESIAN_POINT('Ctrl Pts',(3.52155867431486,1.,-1.95926936324461));
#71451=CARTESIAN_POINT('Ctrl Pts',(3.51398354617794,-1.,-1.95819025316779));
#71452=CARTESIAN_POINT('Ctrl Pts',(3.51398354617794,1.,-1.95819025316779));
#71453=CARTESIAN_POINT('Ctrl Pts',(3.50642124159909,-1.,-1.95707099606511));
#71454=CARTESIAN_POINT('Ctrl Pts',(3.50642124159909,1.,-1.95707099606511));
#71455=CARTESIAN_POINT('Ctrl Pts',(3.49887263575583,-1.,-1.95591153823661));
#71456=CARTESIAN_POINT('Ctrl Pts',(3.49887263575583,1.,-1.95591153823661));
#71457=CARTESIAN_POINT('Ctrl Pts',(3.49133956289133,-1.,-1.95471236969643));
#71458=CARTESIAN_POINT('Ctrl Pts',(3.49133956289133,1.,-1.95471236969643));
#71459=CARTESIAN_POINT('Ctrl Pts',(3.48382414832634,-1.,-1.95347412486309));
#71460=CARTESIAN_POINT('Ctrl Pts',(3.48382414832634,1.,-1.95347412486309));
#71461=CARTESIAN_POINT('Ctrl Pts',(3.47632820495921,-1.,-1.95219722189876));
#71462=CARTESIAN_POINT('Ctrl Pts',(3.47632820495921,1.,-1.95219722189876));
#71463=CARTESIAN_POINT('Ctrl Pts',(3.46885258974191,-1.,-1.95088147859877));
#71464=CARTESIAN_POINT('Ctrl Pts',(3.46885258974191,1.,-1.95088147859877));
#71465=CARTESIAN_POINT('Ctrl Pts',(3.46139661060962,-1.,-1.94952575850197));
#71466=CARTESIAN_POINT('Ctrl Pts',(3.46139661060962,1.,-1.94952575850197));
#71467=CARTESIAN_POINT('Ctrl Pts',(3.45395731584051,-1.,-1.94812754766524));
#71468=CARTESIAN_POINT('Ctrl Pts',(3.45395731584051,1.,-1.94812754766524));
#71469=CARTESIAN_POINT('Ctrl Pts',(3.44653088665681,-1.,-1.94668377715329));
#71470=CARTESIAN_POINT('Ctrl Pts',(3.44653088665681,1.,-1.94668377715329));
#71471=CARTESIAN_POINT('Ctrl Pts',(3.43911410197687,-1.,-1.94519168842879));
#71472=CARTESIAN_POINT('Ctrl Pts',(3.43911410197687,1.,-1.94519168842879));
#71473=CARTESIAN_POINT('Ctrl Pts',(3.43170586602434,-1.,-1.94364973660284));
#71474=CARTESIAN_POINT('Ctrl Pts',(3.43170586602434,1.,-1.94364973660284));
#71475=CARTESIAN_POINT('Ctrl Pts',(3.42430850941503,-1.,-1.94205835913696));
#71476=CARTESIAN_POINT('Ctrl Pts',(3.42430850941503,1.,-1.94205835913696));
#71477=CARTESIAN_POINT('Ctrl Pts',(3.41692971994096,-1.,-1.94042111965246));
#71478=CARTESIAN_POINT('Ctrl Pts',(3.41692971994096,1.,-1.94042111965246));
#71479=CARTESIAN_POINT('Ctrl Pts',(3.40957978266642,-1.,-1.93874306008143));
#71480=CARTESIAN_POINT('Ctrl Pts',(3.40957978266642,1.,-1.93874306008143));
#71481=CARTESIAN_POINT('Ctrl Pts',(3.40226802104109,-1.,-1.93702857723098));
#71482=CARTESIAN_POINT('Ctrl Pts',(3.40226802104109,1.,-1.93702857723098));
#71483=CARTESIAN_POINT('Ctrl Pts',(3.39499923640795,-1.,-1.93527929945985));
#71484=CARTESIAN_POINT('Ctrl Pts',(3.39499923640795,1.,-1.93527929945985));
#71485=CARTESIAN_POINT('Ctrl Pts',(3.38777076883256,-1.,-1.93349233176788));
#71486=CARTESIAN_POINT('Ctrl Pts',(3.38777076883256,1.,-1.93349233176788));
#71487=CARTESIAN_POINT('Ctrl Pts',(3.3805676852555,-1.,-1.93165739093276));
#71488=CARTESIAN_POINT('Ctrl Pts',(3.3805676852555,1.,-1.93165739093276));
#71489=CARTESIAN_POINT('Ctrl Pts',(3.37336807068043,-1.,-1.92975993109877));
#71490=CARTESIAN_POINT('Ctrl Pts',(3.37336807068043,1.,-1.92975993109877));
#71491=CARTESIAN_POINT('Ctrl Pts',(3.36615168657567,-1.,-1.92778626543786));
#71492=CARTESIAN_POINT('Ctrl Pts',(3.36615168657567,1.,-1.92778626543786));
#71493=CARTESIAN_POINT('Ctrl Pts',(3.35890824422965,-1.,-1.92572846125756));
#71494=CARTESIAN_POINT('Ctrl Pts',(3.35890824422965,1.,-1.92572846125756));
#71495=CARTESIAN_POINT('Ctrl Pts',(3.35164424847223,-1.,-1.92358838440528));
#71496=CARTESIAN_POINT('Ctrl Pts',(3.35164424847223,1.,-1.92358838440528));
#71497=CARTESIAN_POINT('Ctrl Pts',(3.34439448941961,-1.,-1.92138450828404));
#71498=CARTESIAN_POINT('Ctrl Pts',(3.34439448941961,1.,-1.92138450828404));
#71499=CARTESIAN_POINT('Ctrl Pts',(3.33721230710012,-1.,-1.9191460961021));
#71500=CARTESIAN_POINT('Ctrl Pts',(3.33721230710012,1.,-1.9191460961021));
#71501=CARTESIAN_POINT('Ctrl Pts',(3.33014884257873,-1.,-1.91690081930332));
#71502=CARTESIAN_POINT('Ctrl Pts',(3.33014884257873,1.,-1.91690081930332));
#71503=CARTESIAN_POINT('Ctrl Pts',(3.32323403454535,-1.,-1.91466343916628));
#71504=CARTESIAN_POINT('Ctrl Pts',(3.32323403454535,1.,-1.91466343916628));
#71505=CARTESIAN_POINT('Ctrl Pts',(3.31646052426364,-1.,-1.91242616234442));
#71506=CARTESIAN_POINT('Ctrl Pts',(3.31646052426364,1.,-1.91242616234442));
#71507=CARTESIAN_POINT('Ctrl Pts',(3.30975721158596,-1.,-1.91014297830446));
#71508=CARTESIAN_POINT('Ctrl Pts',(3.30975721158596,1.,-1.91014297830446));
#71509=CARTESIAN_POINT('Ctrl Pts',(3.30300595568195,-1.,-1.90773912171341));
#71510=CARTESIAN_POINT('Ctrl Pts',(3.30300595568195,1.,-1.90773912171341));
#71511=CARTESIAN_POINT('Ctrl Pts',(3.29608978722113,-1.,-1.90513891864087));
#71512=CARTESIAN_POINT('Ctrl Pts',(3.29608978722113,1.,-1.90513891864087));
#71513=CARTESIAN_POINT('Ctrl Pts',(3.2889344860029,-1.,-1.90228971247527));
#71514=CARTESIAN_POINT('Ctrl Pts',(3.2889344860029,1.,-1.90228971247527));
#71515=CARTESIAN_POINT('Ctrl Pts',(3.28154737912352,-1.,-1.89918429230462));
#71516=CARTESIAN_POINT('Ctrl Pts',(3.28154737912352,1.,-1.89918429230462));
#71517=CARTESIAN_POINT('Ctrl Pts',(3.27407108933139,-1.,-1.89589172903793));
#71518=CARTESIAN_POINT('Ctrl Pts',(3.27407108933139,1.,-1.89589172903793));
#71519=CARTESIAN_POINT('Ctrl Pts',(3.26677653888676,-1.,-1.89255393500965));
#71520=CARTESIAN_POINT('Ctrl Pts',(3.26677653888676,1.,-1.89255393500965));
#71521=CARTESIAN_POINT('Ctrl Pts',(3.25999885193947,-1.,-1.88934996203698));
#71522=CARTESIAN_POINT('Ctrl Pts',(3.25999885193947,1.,-1.88934996203698));
#71523=CARTESIAN_POINT('Ctrl Pts',(3.25408686339463,-1.,-1.88646802523466));
#71524=CARTESIAN_POINT('Ctrl Pts',(3.25408686339463,1.,-1.88646802523466));
#71525=CARTESIAN_POINT('Ctrl Pts',(3.24935200511918,-1.,-1.88407708646357));
#71526=CARTESIAN_POINT('Ctrl Pts',(3.24935200511918,1.,-1.88407708646357));
#71527=CARTESIAN_POINT('Ctrl Pts',(3.24600543790443,-1.,-1.88229202582941));
#71528=CARTESIAN_POINT('Ctrl Pts',(3.24600543790443,1.,-1.88229202582941));
#71529=CARTESIAN_POINT('Ctrl Pts',(3.24451807186481,-1.,-1.88139187908074));
#71530=CARTESIAN_POINT('Ctrl Pts',(3.24451807186481,1.,-1.88139187908074));
#71531=CARTESIAN_POINT('Ctrl Pts',(3.24408699284121,-1.,-1.88102201872555));
#71532=CARTESIAN_POINT('Ctrl Pts',(3.24408699284121,1.,-1.88102201872555));
#71533=CARTESIAN_POINT('Ctrl Pts',(3.24410359189609,-1.,-1.88091100680349));
#71534=CARTESIAN_POINT('Ctrl Pts',(3.24410359189609,1.,-1.88091100680349));
#71535=CARTESIAN_POINT('Ctrl Pts',(3.24418789321065,-1.,-1.8808893942881));
#71536=CARTESIAN_POINT('Ctrl Pts',(3.24418789321065,1.,-1.8808893942881));
#71537=CARTESIAN_POINT('',(3.70708211654725,1.,-1.97421938526992));
#71538=CARTESIAN_POINT('Ctrl Pts',(3.70708211654725,1.,-1.97421938526992));
#71539=CARTESIAN_POINT('Ctrl Pts',(3.70551008132332,1.,-1.97417727645308));
#71540=CARTESIAN_POINT('Ctrl Pts',(3.70236698912904,1.,-1.97408973726715));
#71541=CARTESIAN_POINT('Ctrl Pts',(3.6976552856004,1.,-1.97394846383216));
#71542=CARTESIAN_POINT('Ctrl Pts',(3.69137888599902,1.,-1.97374016225483));
#71543=CARTESIAN_POINT('Ctrl Pts',(3.68354319915092,1.,-1.97344650304519));
#71544=CARTESIAN_POINT('Ctrl Pts',(3.67571738107084,1.,-1.97311947678517));
#71545=CARTESIAN_POINT('Ctrl Pts',(3.66790152752075,1.,-1.97275897198678));
#71546=CARTESIAN_POINT('Ctrl Pts',(3.6600957816636,1.,-1.9723648543905));
#71547=CARTESIAN_POINT('Ctrl Pts',(3.652300347166,1.,-1.9719369724024));
#71548=CARTESIAN_POINT('Ctrl Pts',(3.64451546723514,1.,-1.97147515441164));
#71549=CARTESIAN_POINT('Ctrl Pts',(3.63674139590412,1.,-1.97097920454464));
#71550=CARTESIAN_POINT('Ctrl Pts',(3.62897836973293,1.,-1.97044889850463));
#71551=CARTESIAN_POINT('Ctrl Pts',(3.62122658401893,1.,-1.96988398129978));
#71552=CARTESIAN_POINT('Ctrl Pts',(3.61348615496704,1.,-1.96928416040877));
#71553=CARTESIAN_POINT('Ctrl Pts',(3.60575714017989,1.,-1.9686491188594));
#71554=CARTESIAN_POINT('Ctrl Pts',(3.59803959819938,1.,-1.96797854118369));
#71555=CARTESIAN_POINT('Ctrl Pts',(3.59033364022801,1.,-1.96727213799544));
#71556=CARTESIAN_POINT('Ctrl Pts',(3.58263947663829,1.,-1.96652966688911));
#71557=CARTESIAN_POINT('Ctrl Pts',(3.57495748600959,1.,-1.96575096652789));
#71558=CARTESIAN_POINT('Ctrl Pts',(3.56728820357791,1.,-1.96493594634567));
#71559=CARTESIAN_POINT('Ctrl Pts',(3.55963218706096,1.,-1.96408450906812));
#71560=CARTESIAN_POINT('Ctrl Pts',(3.55198990600886,1.,-1.96319648628644));
#71561=CARTESIAN_POINT('Ctrl Pts',(3.54436163300443,1.,-1.96227157573067));
#71562=CARTESIAN_POINT('Ctrl Pts',(3.53674730625813,1.,-1.96130926212689));
#71563=CARTESIAN_POINT('Ctrl Pts',(3.52914648844351,1.,-1.96030879411566));
#71564=CARTESIAN_POINT('Ctrl Pts',(3.52155867431486,1.,-1.95926936324461));
#71565=CARTESIAN_POINT('Ctrl Pts',(3.51398354617794,1.,-1.95819025316779));
#71566=CARTESIAN_POINT('Ctrl Pts',(3.50642124159909,1.,-1.95707099606511));
#71567=CARTESIAN_POINT('Ctrl Pts',(3.49887263575583,1.,-1.95591153823661));
#71568=CARTESIAN_POINT('Ctrl Pts',(3.49133956289133,1.,-1.95471236969643));
#71569=CARTESIAN_POINT('Ctrl Pts',(3.48382414832634,1.,-1.95347412486309));
#71570=CARTESIAN_POINT('Ctrl Pts',(3.47632820495921,1.,-1.95219722189876));
#71571=CARTESIAN_POINT('Ctrl Pts',(3.46885258974191,1.,-1.95088147859877));
#71572=CARTESIAN_POINT('Ctrl Pts',(3.46139661060962,1.,-1.94952575850197));
#71573=CARTESIAN_POINT('Ctrl Pts',(3.45395731584051,1.,-1.94812754766524));
#71574=CARTESIAN_POINT('Ctrl Pts',(3.44653088665681,1.,-1.94668377715329));
#71575=CARTESIAN_POINT('Ctrl Pts',(3.43911410197687,1.,-1.94519168842879));
#71576=CARTESIAN_POINT('Ctrl Pts',(3.43170586602434,1.,-1.94364973660284));
#71577=CARTESIAN_POINT('Ctrl Pts',(3.42430850941503,1.,-1.94205835913696));
#71578=CARTESIAN_POINT('Ctrl Pts',(3.41692971994096,1.,-1.94042111965246));
#71579=CARTESIAN_POINT('Ctrl Pts',(3.40957978266642,1.,-1.93874306008143));
#71580=CARTESIAN_POINT('Ctrl Pts',(3.40226802104109,1.,-1.93702857723098));
#71581=CARTESIAN_POINT('Ctrl Pts',(3.39499923640795,1.,-1.93527929945985));
#71582=CARTESIAN_POINT('Ctrl Pts',(3.38777076883256,1.,-1.93349233176788));
#71583=CARTESIAN_POINT('Ctrl Pts',(3.3805676852555,1.,-1.93165739093276));
#71584=CARTESIAN_POINT('Ctrl Pts',(3.37336807068043,1.,-1.92975993109877));
#71585=CARTESIAN_POINT('Ctrl Pts',(3.36615168657567,1.,-1.92778626543786));
#71586=CARTESIAN_POINT('Ctrl Pts',(3.35890824422965,1.,-1.92572846125756));
#71587=CARTESIAN_POINT('Ctrl Pts',(3.35164424847223,1.,-1.92358838440528));
#71588=CARTESIAN_POINT('Ctrl Pts',(3.34439448941961,1.,-1.92138450828404));
#71589=CARTESIAN_POINT('Ctrl Pts',(3.33721230710012,1.,-1.9191460961021));
#71590=CARTESIAN_POINT('Ctrl Pts',(3.33014884257873,1.,-1.91690081930332));
#71591=CARTESIAN_POINT('Ctrl Pts',(3.32323403454535,1.,-1.91466343916628));
#71592=CARTESIAN_POINT('Ctrl Pts',(3.31646052426364,1.,-1.91242616234442));
#71593=CARTESIAN_POINT('Ctrl Pts',(3.30975721158596,1.,-1.91014297830446));
#71594=CARTESIAN_POINT('Ctrl Pts',(3.30300595568195,1.,-1.90773912171341));
#71595=CARTESIAN_POINT('Ctrl Pts',(3.29608978722113,1.,-1.90513891864087));
#71596=CARTESIAN_POINT('Ctrl Pts',(3.2889344860029,1.,-1.90228971247527));
#71597=CARTESIAN_POINT('Ctrl Pts',(3.28154737912352,1.,-1.89918429230462));
#71598=CARTESIAN_POINT('Ctrl Pts',(3.27407108933139,1.,-1.89589172903793));
#71599=CARTESIAN_POINT('Ctrl Pts',(3.26677653888676,1.,-1.89255393500965));
#71600=CARTESIAN_POINT('Ctrl Pts',(3.25999885193947,1.,-1.88934996203698));
#71601=CARTESIAN_POINT('Ctrl Pts',(3.25408686339463,1.,-1.88646802523466));
#71602=CARTESIAN_POINT('Ctrl Pts',(3.24935200511918,1.,-1.88407708646357));
#71603=CARTESIAN_POINT('Ctrl Pts',(3.2462565441079,1.,-1.88242596600454));
#71604=CARTESIAN_POINT('Ctrl Pts',(3.24480754676064,1.,-1.88156537699203));
#71605=CARTESIAN_POINT('Ctrl Pts',(3.24428080353022,1.,-1.88117508446775));
#71606=CARTESIAN_POINT('Ctrl Pts',(3.24415531671284,1.,-1.8810229239812));
#71607=CARTESIAN_POINT('Ctrl Pts',(3.24413672884812,1.,-1.88097764062697));
#71608=CARTESIAN_POINT('',(3.70708211654725,0.,-1.97421938526992));
#71609=CARTESIAN_POINT('Ctrl Pts',(3.42855728381368,-1.,-1.519044091397));
#71610=CARTESIAN_POINT('Ctrl Pts',(3.42855728381368,1.,-1.519044091397));
#71611=CARTESIAN_POINT('Ctrl Pts',(3.42852521763778,-1.,-1.51896318668366));
#71612=CARTESIAN_POINT('Ctrl Pts',(3.42852521763778,1.,-1.51896318668366));
#71613=CARTESIAN_POINT('Ctrl Pts',(3.42860527149177,-1.,-1.51888450659652));
#71614=CARTESIAN_POINT('Ctrl Pts',(3.42860527149177,1.,-1.51888450659652));
#71615=CARTESIAN_POINT('Ctrl Pts',(3.42915787669893,-1.,-1.51901585839109));
#71616=CARTESIAN_POINT('Ctrl Pts',(3.42915787669893,1.,-1.51901585839109));
#71617=CARTESIAN_POINT('Ctrl Pts',(3.43076036253837,-1.,-1.51969006980999));
#71618=CARTESIAN_POINT('Ctrl Pts',(3.43076036253837,1.,-1.51969006980999));
#71619=CARTESIAN_POINT('Ctrl Pts',(3.43417156977893,-1.,-1.52134826724293));
#71620=CARTESIAN_POINT('Ctrl Pts',(3.43417156977893,1.,-1.52134826724293));
#71621=CARTESIAN_POINT('Ctrl Pts',(3.4388889597401,-1.,-1.5237734895035));
#71622=CARTESIAN_POINT('Ctrl Pts',(3.4388889597401,1.,-1.5237734895035));
#71623=CARTESIAN_POINT('Ctrl Pts',(3.44469547526647,-1.,-1.52686242875556));
#71624=CARTESIAN_POINT('Ctrl Pts',(3.44469547526647,1.,-1.52686242875556));
#71625=CARTESIAN_POINT('Ctrl Pts',(3.45127136828305,-1.,-1.53046244461635));
#71626=CARTESIAN_POINT('Ctrl Pts',(3.45127136828305,1.,-1.53046244461635));
#71627=CARTESIAN_POINT('Ctrl Pts',(3.45825932955032,-1.,-1.53440195378792));
#71628=CARTESIAN_POINT('Ctrl Pts',(3.45825932955032,1.,-1.53440195378792));
#71629=CARTESIAN_POINT('Ctrl Pts',(3.46531752207153,-1.,-1.53851507915502));
#71630=CARTESIAN_POINT('Ctrl Pts',(3.46531752207153,1.,-1.53851507915502));
#71631=CARTESIAN_POINT('Ctrl Pts',(3.47217189224653,-1.,-1.54266605398188));
#71632=CARTESIAN_POINT('Ctrl Pts',(3.47217189224653,1.,-1.54266605398188));
#71633=CARTESIAN_POINT('Ctrl Pts',(3.47868272898751,-1.,-1.54678009290276));
#71634=CARTESIAN_POINT('Ctrl Pts',(3.47868272898751,1.,-1.54678009290276));
#71635=CARTESIAN_POINT('Ctrl Pts',(3.48485155928567,-1.,-1.55084702970452));
#71636=CARTESIAN_POINT('Ctrl Pts',(3.48485155928567,1.,-1.55084702970452));
#71637=CARTESIAN_POINT('Ctrl Pts',(3.4907646087742,-1.,-1.55489595901116));
#71638=CARTESIAN_POINT('Ctrl Pts',(3.4907646087742,1.,-1.55489595901116));
#71639=CARTESIAN_POINT('Ctrl Pts',(3.49655185179655,-1.,-1.55897703097874));
#71640=CARTESIAN_POINT('Ctrl Pts',(3.49655185179655,1.,-1.55897703097874));
#71641=CARTESIAN_POINT('Ctrl Pts',(3.50234321621578,-1.,-1.56314187758675));
#71642=CARTESIAN_POINT('Ctrl Pts',(3.50234321621578,1.,-1.56314187758675));
#71643=CARTESIAN_POINT('Ctrl Pts',(3.50821771695363,-1.,-1.56742097575012));
#71644=CARTESIAN_POINT('Ctrl Pts',(3.50821771695363,1.,-1.56742097575012));
#71645=CARTESIAN_POINT('Ctrl Pts',(3.51418598431665,-1.,-1.57181569799743));
#71646=CARTESIAN_POINT('Ctrl Pts',(3.51418598431665,1.,-1.57181569799743));
#71647=CARTESIAN_POINT('Ctrl Pts',(3.52021847865912,-1.,-1.57631049988158));
#71648=CARTESIAN_POINT('Ctrl Pts',(3.52021847865912,1.,-1.57631049988158));
#71649=CARTESIAN_POINT('Ctrl Pts',(3.52626275334881,-1.,-1.58088027227848));
#71650=CARTESIAN_POINT('Ctrl Pts',(3.52626275334881,1.,-1.58088027227848));
#71651=CARTESIAN_POINT('Ctrl Pts',(3.5322637814708,-1.,-1.58549906268088));
#71652=CARTESIAN_POINT('Ctrl Pts',(3.5322637814708,1.,-1.58549906268088));
#71653=CARTESIAN_POINT('Ctrl Pts',(3.53818616861077,-1.,-1.59014958368739));
#71654=CARTESIAN_POINT('Ctrl Pts',(3.53818616861077,1.,-1.59014958368739));
#71655=CARTESIAN_POINT('Ctrl Pts',(3.54402458182337,-1.,-1.59482766949766));
#71656=CARTESIAN_POINT('Ctrl Pts',(3.54402458182337,1.,-1.59482766949766));
#71657=CARTESIAN_POINT('Ctrl Pts',(3.54979148634454,-1.,-1.59953698113457));
#71658=CARTESIAN_POINT('Ctrl Pts',(3.54979148634454,1.,-1.59953698113457));
#71659=CARTESIAN_POINT('Ctrl Pts',(3.55550985096129,-1.,-1.60428584699853));
#71660=CARTESIAN_POINT('Ctrl Pts',(3.55550985096129,1.,-1.60428584699853));
#71661=CARTESIAN_POINT('Ctrl Pts',(3.5612043248298,-1.,-1.60908344685457));
#71662=CARTESIAN_POINT('Ctrl Pts',(3.5612043248298,1.,-1.60908344685457));
#71663=CARTESIAN_POINT('Ctrl Pts',(3.56689200468387,-1.,-1.61393581747514));
#71664=CARTESIAN_POINT('Ctrl Pts',(3.56689200468387,1.,-1.61393581747514));
#71665=CARTESIAN_POINT('Ctrl Pts',(3.57257679609806,-1.,-1.61884340915404));
#71666=CARTESIAN_POINT('Ctrl Pts',(3.57257679609806,1.,-1.61884340915404));
#71667=CARTESIAN_POINT('Ctrl Pts',(3.5782545595439,-1.,-1.62380329464844));
#71668=CARTESIAN_POINT('Ctrl Pts',(3.5782545595439,1.,-1.62380329464844));
#71669=CARTESIAN_POINT('Ctrl Pts',(3.58391625774343,-1.,-1.62881051550745));
#71670=CARTESIAN_POINT('Ctrl Pts',(3.58391625774343,1.,-1.62881051550745));
#71671=CARTESIAN_POINT('Ctrl Pts',(3.58955176627879,-1.,-1.6338597145126));
#71672=CARTESIAN_POINT('Ctrl Pts',(3.58955176627879,1.,-1.6338597145126));
#71673=CARTESIAN_POINT('Ctrl Pts',(3.59515368334893,-1.,-1.63894676675352));
#71674=CARTESIAN_POINT('Ctrl Pts',(3.59515368334893,1.,-1.63894676675352));
#71675=CARTESIAN_POINT('Ctrl Pts',(3.60072028513845,-1.,-1.64407004385582));
#71676=CARTESIAN_POINT('Ctrl Pts',(3.60072028513845,1.,-1.64407004385582));
#71677=CARTESIAN_POINT('Ctrl Pts',(3.60625346556992,-1.,-1.64922952425832));
#71678=CARTESIAN_POINT('Ctrl Pts',(3.60625346556992,1.,-1.64922952425832));
#71679=CARTESIAN_POINT('Ctrl Pts',(3.61175734965127,-1.,-1.65442619244325));
#71680=CARTESIAN_POINT('Ctrl Pts',(3.61175734965127,1.,-1.65442619244325));
#71681=CARTESIAN_POINT('Ctrl Pts',(3.61723666482456,-1.,-1.65966133399186));
#71682=CARTESIAN_POINT('Ctrl Pts',(3.61723666482456,1.,-1.65966133399186));
#71683=CARTESIAN_POINT('Ctrl Pts',(3.62269517989109,-1.,-1.66493585923855));
#71684=CARTESIAN_POINT('Ctrl Pts',(3.62269517989109,1.,-1.66493585923855));
#71685=CARTESIAN_POINT('Ctrl Pts',(3.62813422105271,-1.,-1.67024966008045));
#71686=CARTESIAN_POINT('Ctrl Pts',(3.62813422105271,1.,-1.67024966008045));
#71687=CARTESIAN_POINT('Ctrl Pts',(3.63355343201232,-1.,-1.67560193613156));
#71688=CARTESIAN_POINT('Ctrl Pts',(3.63355343201232,1.,-1.67560193613156));
#71689=CARTESIAN_POINT('Ctrl Pts',(3.63895140887462,-1.,-1.68099146651586));
#71690=CARTESIAN_POINT('Ctrl Pts',(3.63895140887462,1.,-1.68099146651586));
#71691=CARTESIAN_POINT('Ctrl Pts',(3.64432638915203,-1.,-1.68641690471457));
#71692=CARTESIAN_POINT('Ctrl Pts',(3.64432638915203,1.,-1.68641690471457));
#71693=CARTESIAN_POINT('Ctrl Pts',(3.64967689827371,-1.,-1.69187705481689));
#71694=CARTESIAN_POINT('Ctrl Pts',(3.64967689827371,1.,-1.69187705481689));
#71695=CARTESIAN_POINT('Ctrl Pts',(3.65500246526749,-1.,-1.69737117722534));
#71696=CARTESIAN_POINT('Ctrl Pts',(3.65500246526749,1.,-1.69737117722534));
#71697=CARTESIAN_POINT('Ctrl Pts',(3.66030338774847,-1.,-1.70289888566873));
#71698=CARTESIAN_POINT('Ctrl Pts',(3.66030338774847,1.,-1.70289888566873));
#71699=CARTESIAN_POINT('Ctrl Pts',(3.66558043198876,-1.,-1.70846001610956));
#71700=CARTESIAN_POINT('Ctrl Pts',(3.66558043198876,1.,-1.70846001610956));
#71701=CARTESIAN_POINT('Ctrl Pts',(3.67083454901611,-1.,-1.71405450210384));
#71702=CARTESIAN_POINT('Ctrl Pts',(3.67083454901611,1.,-1.71405450210384));
#71703=CARTESIAN_POINT('Ctrl Pts',(3.67606660374709,-1.,-1.71968225581808));
#71704=CARTESIAN_POINT('Ctrl Pts',(3.67606660374709,1.,-1.71968225581808));
#71705=CARTESIAN_POINT('Ctrl Pts',(3.68127704936579,-1.,-1.72534302437056));
#71706=CARTESIAN_POINT('Ctrl Pts',(3.68127704936579,1.,-1.72534302437056));
#71707=CARTESIAN_POINT('Ctrl Pts',(3.68646597019332,-1.,-1.73103640956717));
#71708=CARTESIAN_POINT('Ctrl Pts',(3.68646597019332,1.,-1.73103640956717));
#71709=CARTESIAN_POINT('Ctrl Pts',(3.69163322648036,-1.,-1.73676193254557));
#71710=CARTESIAN_POINT('Ctrl Pts',(3.69163322648036,1.,-1.73676193254557));
#71711=CARTESIAN_POINT('Ctrl Pts',(3.69677856910517,-1.,-1.74251908492617));
#71712=CARTESIAN_POINT('Ctrl Pts',(3.69677856910517,1.,-1.74251908492617));
#71713=CARTESIAN_POINT('Ctrl Pts',(3.7019017567335,-1.,-1.74830738046057));
#71714=CARTESIAN_POINT('Ctrl Pts',(3.7019017567335,1.,-1.74830738046057));
#71715=CARTESIAN_POINT('Ctrl Pts',(3.70700269736659,-1.,-1.75412641804042));
#71716=CARTESIAN_POINT('Ctrl Pts',(3.70700269736659,1.,-1.75412641804042));
#71717=CARTESIAN_POINT('Ctrl Pts',(3.71208146346136,-1.,-1.75997588498865));
#71718=CARTESIAN_POINT('Ctrl Pts',(3.71208146346136,1.,-1.75997588498865));
#71719=CARTESIAN_POINT('Ctrl Pts',(3.71713822377359,-1.,-1.76585552124394));
#71720=CARTESIAN_POINT('Ctrl Pts',(3.71713822377359,1.,-1.76585552124394));
#71721=CARTESIAN_POINT('Ctrl Pts',(3.72217319911254,-1.,-1.77176509401761));
#71722=CARTESIAN_POINT('Ctrl Pts',(3.72217319911254,1.,-1.77176509401761));
#71723=CARTESIAN_POINT('Ctrl Pts',(3.72718661205609,-1.,-1.77770437039658));
#71724=CARTESIAN_POINT('Ctrl Pts',(3.72718661205609,1.,-1.77770437039658));
#71725=CARTESIAN_POINT('Ctrl Pts',(3.7321786309547,-1.,-1.78367308442901));
#71726=CARTESIAN_POINT('Ctrl Pts',(3.7321786309547,1.,-1.78367308442901));
#71727=CARTESIAN_POINT('Ctrl Pts',(3.73714934730681,-1.,-1.78967092823491));
#71728=CARTESIAN_POINT('Ctrl Pts',(3.73714934730681,1.,-1.78967092823491));
#71729=CARTESIAN_POINT('Ctrl Pts',(3.74209880352445,-1.,-1.79569757859422));
#71730=CARTESIAN_POINT('Ctrl Pts',(3.74209880352445,1.,-1.79569757859422));
#71731=CARTESIAN_POINT('Ctrl Pts',(3.74702700875467,-1.,-1.8017527148577));
#71732=CARTESIAN_POINT('Ctrl Pts',(3.74702700875467,1.,-1.8017527148577));
#71733=CARTESIAN_POINT('Ctrl Pts',(3.75193395887977,-1.,-1.80783603939617));
#71734=CARTESIAN_POINT('Ctrl Pts',(3.75193395887977,1.,-1.80783603939617));
#71735=CARTESIAN_POINT('Ctrl Pts',(3.75681965683071,-1.,-1.8139472983358));
#71736=CARTESIAN_POINT('Ctrl Pts',(3.75681965683071,1.,-1.8139472983358));
#71737=CARTESIAN_POINT('Ctrl Pts',(3.76168412707948,-1.,-1.82008629694091));
#71738=CARTESIAN_POINT('Ctrl Pts',(3.76168412707948,1.,-1.82008629694091));
#71739=CARTESIAN_POINT('Ctrl Pts',(3.76652740353775,-1.,-1.82625289220915));
#71740=CARTESIAN_POINT('Ctrl Pts',(3.76652740353775,1.,-1.82625289220915));
#71741=CARTESIAN_POINT('Ctrl Pts',(3.77038509817999,-1.,-1.83120816955646));
#71742=CARTESIAN_POINT('Ctrl Pts',(3.77038509817999,1.,-1.83120816955646));
#71743=CARTESIAN_POINT('Ctrl Pts',(3.77326886064398,-1.,-1.83493697934534));
#71744=CARTESIAN_POINT('Ctrl Pts',(3.77326886064398,1.,-1.83493697934534));
#71745=CARTESIAN_POINT('Ctrl Pts',(3.77518714457833,-1.,-1.83742834010626));
#71746=CARTESIAN_POINT('Ctrl Pts',(3.77518714457833,1.,-1.83742834010626));
#71747=CARTESIAN_POINT('Ctrl Pts',(3.77614523045147,-1.,-1.83867539237861));
#71748=CARTESIAN_POINT('Ctrl Pts',(3.77614523045147,1.,-1.83867539237861));
#71749=CARTESIAN_POINT('',(3.42859860294306,1.,-1.5189508286633));
#71750=CARTESIAN_POINT('Ctrl Pts',(3.42859860294306,-1.,-1.5189508286633));
#71751=CARTESIAN_POINT('Ctrl Pts',(3.42859860294306,-0.666666666666667,
-1.5189508286633));
#71752=CARTESIAN_POINT('Ctrl Pts',(3.42859860294306,-0.333333333333333,
-1.5189508286633));
#71753=CARTESIAN_POINT('Ctrl Pts',(3.42859860294306,0.333333333333333,-1.5189508286633));
#71754=CARTESIAN_POINT('Ctrl Pts',(3.42859860294306,0.666666666666667,-1.5189508286633));
#71755=CARTESIAN_POINT('Ctrl Pts',(3.42859860294306,1.,-1.5189508286633));
#71756=CARTESIAN_POINT('',(3.77614523045147,1.,-1.83867539237861));
#71757=CARTESIAN_POINT('',(3.77614523045147,0.,-1.83867539237861));
#71758=CARTESIAN_POINT('Ctrl Pts',(3.42859860294306,1.,-1.5189508286633));
#71759=CARTESIAN_POINT('Ctrl Pts',(3.42864616361875,1.,-1.51893924967331));
#71760=CARTESIAN_POINT('Ctrl Pts',(3.42884302333841,1.,-1.5189513329503));
#71761=CARTESIAN_POINT('Ctrl Pts',(3.42946838852588,1.,-1.51914806898491));
#71762=CARTESIAN_POINT('Ctrl Pts',(3.43101631893414,1.,-1.5198144909338));
#71763=CARTESIAN_POINT('Ctrl Pts',(3.43417156977893,1.,-1.52134826724293));
#71764=CARTESIAN_POINT('Ctrl Pts',(3.4388889597401,1.,-1.5237734895035));
#71765=CARTESIAN_POINT('Ctrl Pts',(3.44469547526647,1.,-1.52686242875556));
#71766=CARTESIAN_POINT('Ctrl Pts',(3.45127136828305,1.,-1.53046244461635));
#71767=CARTESIAN_POINT('Ctrl Pts',(3.45825932955032,1.,-1.53440195378792));
#71768=CARTESIAN_POINT('Ctrl Pts',(3.46531752207153,1.,-1.53851507915502));
#71769=CARTESIAN_POINT('Ctrl Pts',(3.47217189224653,1.,-1.54266605398188));
#71770=CARTESIAN_POINT('Ctrl Pts',(3.47868272898751,1.,-1.54678009290276));
#71771=CARTESIAN_POINT('Ctrl Pts',(3.48485155928567,1.,-1.55084702970452));
#71772=CARTESIAN_POINT('Ctrl Pts',(3.4907646087742,1.,-1.55489595901116));
#71773=CARTESIAN_POINT('Ctrl Pts',(3.49655185179655,1.,-1.55897703097874));
#71774=CARTESIAN_POINT('Ctrl Pts',(3.50234321621578,1.,-1.56314187758675));
#71775=CARTESIAN_POINT('Ctrl Pts',(3.50821771695363,1.,-1.56742097575012));
#71776=CARTESIAN_POINT('Ctrl Pts',(3.51418598431665,1.,-1.57181569799743));
#71777=CARTESIAN_POINT('Ctrl Pts',(3.52021847865912,1.,-1.57631049988158));
#71778=CARTESIAN_POINT('Ctrl Pts',(3.52626275334881,1.,-1.58088027227848));
#71779=CARTESIAN_POINT('Ctrl Pts',(3.5322637814708,1.,-1.58549906268088));
#71780=CARTESIAN_POINT('Ctrl Pts',(3.53818616861077,1.,-1.59014958368739));
#71781=CARTESIAN_POINT('Ctrl Pts',(3.54402458182337,1.,-1.59482766949766));
#71782=CARTESIAN_POINT('Ctrl Pts',(3.54979148634454,1.,-1.59953698113457));
#71783=CARTESIAN_POINT('Ctrl Pts',(3.55550985096129,1.,-1.60428584699853));
#71784=CARTESIAN_POINT('Ctrl Pts',(3.5612043248298,1.,-1.60908344685457));
#71785=CARTESIAN_POINT('Ctrl Pts',(3.56689200468387,1.,-1.61393581747514));
#71786=CARTESIAN_POINT('Ctrl Pts',(3.57257679609806,1.,-1.61884340915404));
#71787=CARTESIAN_POINT('Ctrl Pts',(3.5782545595439,1.,-1.62380329464844));
#71788=CARTESIAN_POINT('Ctrl Pts',(3.58391625774343,1.,-1.62881051550745));
#71789=CARTESIAN_POINT('Ctrl Pts',(3.58955176627879,1.,-1.6338597145126));
#71790=CARTESIAN_POINT('Ctrl Pts',(3.59515368334893,1.,-1.63894676675352));
#71791=CARTESIAN_POINT('Ctrl Pts',(3.60072028513845,1.,-1.64407004385582));
#71792=CARTESIAN_POINT('Ctrl Pts',(3.60625346556992,1.,-1.64922952425832));
#71793=CARTESIAN_POINT('Ctrl Pts',(3.61175734965127,1.,-1.65442619244325));
#71794=CARTESIAN_POINT('Ctrl Pts',(3.61723666482456,1.,-1.65966133399186));
#71795=CARTESIAN_POINT('Ctrl Pts',(3.62269517989109,1.,-1.66493585923855));
#71796=CARTESIAN_POINT('Ctrl Pts',(3.62813422105271,1.,-1.67024966008045));
#71797=CARTESIAN_POINT('Ctrl Pts',(3.63355343201232,1.,-1.67560193613156));
#71798=CARTESIAN_POINT('Ctrl Pts',(3.63895140887462,1.,-1.68099146651586));
#71799=CARTESIAN_POINT('Ctrl Pts',(3.64432638915203,1.,-1.68641690471457));
#71800=CARTESIAN_POINT('Ctrl Pts',(3.64967689827371,1.,-1.69187705481689));
#71801=CARTESIAN_POINT('Ctrl Pts',(3.65500246526749,1.,-1.69737117722534));
#71802=CARTESIAN_POINT('Ctrl Pts',(3.66030338774847,1.,-1.70289888566873));
#71803=CARTESIAN_POINT('Ctrl Pts',(3.66558043198876,1.,-1.70846001610956));
#71804=CARTESIAN_POINT('Ctrl Pts',(3.67083454901611,1.,-1.71405450210384));
#71805=CARTESIAN_POINT('Ctrl Pts',(3.67606660374709,1.,-1.71968225581808));
#71806=CARTESIAN_POINT('Ctrl Pts',(3.68127704936579,1.,-1.72534302437056));
#71807=CARTESIAN_POINT('Ctrl Pts',(3.68646597019332,1.,-1.73103640956717));
#71808=CARTESIAN_POINT('Ctrl Pts',(3.69163322648036,1.,-1.73676193254557));
#71809=CARTESIAN_POINT('Ctrl Pts',(3.69677856910517,1.,-1.74251908492617));
#71810=CARTESIAN_POINT('Ctrl Pts',(3.7019017567335,1.,-1.74830738046057));
#71811=CARTESIAN_POINT('Ctrl Pts',(3.70700269736659,1.,-1.75412641804042));
#71812=CARTESIAN_POINT('Ctrl Pts',(3.71208146346136,1.,-1.75997588498865));
#71813=CARTESIAN_POINT('Ctrl Pts',(3.71713822377359,1.,-1.76585552124394));
#71814=CARTESIAN_POINT('Ctrl Pts',(3.72217319911254,1.,-1.77176509401761));
#71815=CARTESIAN_POINT('Ctrl Pts',(3.72718661205609,1.,-1.77770437039658));
#71816=CARTESIAN_POINT('Ctrl Pts',(3.7321786309547,1.,-1.78367308442901));
#71817=CARTESIAN_POINT('Ctrl Pts',(3.73714934730681,1.,-1.78967092823491));
#71818=CARTESIAN_POINT('Ctrl Pts',(3.74209880352445,1.,-1.79569757859422));
#71819=CARTESIAN_POINT('Ctrl Pts',(3.74702700875467,1.,-1.8017527148577));
#71820=CARTESIAN_POINT('Ctrl Pts',(3.75193395887977,1.,-1.80783603939617));
#71821=CARTESIAN_POINT('Ctrl Pts',(3.75681965683071,1.,-1.8139472983358));
#71822=CARTESIAN_POINT('Ctrl Pts',(3.76168412707948,1.,-1.82008629694091));
#71823=CARTESIAN_POINT('Ctrl Pts',(3.76652740353775,1.,-1.82625289220915));
#71824=CARTESIAN_POINT('Ctrl Pts',(3.77038509817999,1.,-1.83120816955646));
#71825=CARTESIAN_POINT('Ctrl Pts',(3.77326886064398,1.,-1.83493697934534));
#71826=CARTESIAN_POINT('Ctrl Pts',(3.77518714457833,1.,-1.83742834010626));
#71827=CARTESIAN_POINT('Ctrl Pts',(3.77614523045147,1.,-1.83867539237861));
#71828=CARTESIAN_POINT('Origin',(3.77614523045147,0.,-1.83867539237861));
#71829=CARTESIAN_POINT('',(3.70708211654725,1.,-1.97421938526992));
#71830=CARTESIAN_POINT('Origin',(0.,0.,0.));
#71831=CARTESIAN_POINT('',(3.49844575334386,1.,-1.35032489087269));
#71832=CARTESIAN_POINT('Origin',(0.,1.,0.));
#71833=CARTESIAN_POINT('Ctrl Pts',(3.49844575334386,1.,-1.35032489087269));
#71834=CARTESIAN_POINT('Ctrl Pts',(3.49844575334386,0.666666666666667,-1.35032489087269));
#71835=CARTESIAN_POINT('Ctrl Pts',(3.49844575334386,0.333333333333333,-1.35032489087269));
#71836=CARTESIAN_POINT('Ctrl Pts',(3.49844575334386,-0.333333333333333,
-1.35032489087269));
#71837=CARTESIAN_POINT('Ctrl Pts',(3.49844575334386,-0.666666666666667,
-1.35032489087269));
#71838=CARTESIAN_POINT('Ctrl Pts',(3.49844575334386,-1.,-1.35032489087269));
#71839=CARTESIAN_POINT('Ctrl Pts',(3.97027773754922,-1.,-1.36999806084572));
#71840=CARTESIAN_POINT('Ctrl Pts',(3.97027773754922,1.,-1.36999806084572));
#71841=CARTESIAN_POINT('Ctrl Pts',(3.9687184694173,-1.,-1.37020239094758));
#71842=CARTESIAN_POINT('Ctrl Pts',(3.9687184694173,1.,-1.37020239094758));
#71843=CARTESIAN_POINT('Ctrl Pts',(3.96560037975788,-1.,-1.37060761746027));
#71844=CARTESIAN_POINT('Ctrl Pts',(3.96560037975788,1.,-1.37060761746027));
#71845=CARTESIAN_POINT('Ctrl Pts',(3.96092458508407,-1.,-1.37120515615663));
#71846=CARTESIAN_POINT('Ctrl Pts',(3.96092458508407,1.,-1.37120515615663));
#71847=CARTESIAN_POINT('Ctrl Pts',(3.95469287283105,-1.,-1.37198126433139));
#71848=CARTESIAN_POINT('Ctrl Pts',(3.95469287283105,1.,-1.37198126433139));
#71849=CARTESIAN_POINT('Ctrl Pts',(3.94690771786926,-1.,-1.37291699203423));
#71850=CARTESIAN_POINT('Ctrl Pts',(3.94690771786926,1.,-1.37291699203423));
#71851=CARTESIAN_POINT('Ctrl Pts',(3.93912709041791,-1.,-1.37381821967499));
#71852=CARTESIAN_POINT('Ctrl Pts',(3.93912709041791,1.,-1.37381821967499));
#71853=CARTESIAN_POINT('Ctrl Pts',(3.93135106761941,-1.,-1.37468482215784));
#71854=CARTESIAN_POINT('Ctrl Pts',(3.93135106761941,1.,-1.37468482215784));
#71855=CARTESIAN_POINT('Ctrl Pts',(3.92357976987132,-1.,-1.37551664448057));
#71856=CARTESIAN_POINT('Ctrl Pts',(3.92357976987132,1.,-1.37551664448057));
#71857=CARTESIAN_POINT('Ctrl Pts',(3.91581337461825,-1.,-1.37631350505516));
#71858=CARTESIAN_POINT('Ctrl Pts',(3.91581337461825,1.,-1.37631350505516));
#71859=CARTESIAN_POINT('Ctrl Pts',(3.90805209522729,-1.,-1.3770751963376));
#71860=CARTESIAN_POINT('Ctrl Pts',(3.90805209522729,1.,-1.3770751963376));
#71861=CARTESIAN_POINT('Ctrl Pts',(3.90029615196255,-1.,-1.3778014851263));
#71862=CARTESIAN_POINT('Ctrl Pts',(3.90029615196255,1.,-1.3778014851263));
#71863=CARTESIAN_POINT('Ctrl Pts',(3.89254574338385,-1.,-1.37849211287981));
#71864=CARTESIAN_POINT('Ctrl Pts',(3.89254574338385,1.,-1.37849211287981));
#71865=CARTESIAN_POINT('Ctrl Pts',(3.88480102249461,-1.,-1.37914679719446));
#71866=CARTESIAN_POINT('Ctrl Pts',(3.88480102249461,1.,-1.37914679719446));
#71867=CARTESIAN_POINT('Ctrl Pts',(3.87706205830865,-1.,-1.37976523097187));
#71868=CARTESIAN_POINT('Ctrl Pts',(3.87706205830865,1.,-1.37976523097187));
#71869=CARTESIAN_POINT('Ctrl Pts',(3.86932885813403,-1.,-1.38034709213129));
#71870=CARTESIAN_POINT('Ctrl Pts',(3.86932885813403,1.,-1.38034709213129));
#71871=CARTESIAN_POINT('Ctrl Pts',(3.86160143044187,-1.,-1.38089205993068));
#71872=CARTESIAN_POINT('Ctrl Pts',(3.86160143044187,1.,-1.38089205993068));
#71873=CARTESIAN_POINT('Ctrl Pts',(3.85387983979557,-1.,-1.38139983115075));
#71874=CARTESIAN_POINT('Ctrl Pts',(3.85387983979557,1.,-1.38139983115075));
#71875=CARTESIAN_POINT('Ctrl Pts',(3.84616425605705,-1.,-1.38187013346089));
#71876=CARTESIAN_POINT('Ctrl Pts',(3.84616425605705,1.,-1.38187013346089));
#71877=CARTESIAN_POINT('Ctrl Pts',(3.83845502790609,-1.,-1.38230274828774));
#71878=CARTESIAN_POINT('Ctrl Pts',(3.83845502790609,1.,-1.38230274828774));
#71879=CARTESIAN_POINT('Ctrl Pts',(3.83075266982138,-1.,-1.38269750245086));
#71880=CARTESIAN_POINT('Ctrl Pts',(3.83075266982138,1.,-1.38269750245086));
#71881=CARTESIAN_POINT('Ctrl Pts',(3.82305771743715,-1.,-1.38305421262724));
#71882=CARTESIAN_POINT('Ctrl Pts',(3.82305771743715,1.,-1.38305421262724));
#71883=CARTESIAN_POINT('Ctrl Pts',(3.81537060817765,-1.,-1.38337263902766));
#71884=CARTESIAN_POINT('Ctrl Pts',(3.81537060817765,1.,-1.38337263902766));
#71885=CARTESIAN_POINT('Ctrl Pts',(3.80769156398429,-1.,-1.38365244046226));
#71886=CARTESIAN_POINT('Ctrl Pts',(3.80769156398429,1.,-1.38365244046226));
#71887=CARTESIAN_POINT('Ctrl Pts',(3.80002044322169,-1.,-1.38389311766701));
#71888=CARTESIAN_POINT('Ctrl Pts',(3.80002044322169,1.,-1.38389311766701));
#71889=CARTESIAN_POINT('Ctrl Pts',(3.79235669640907,-1.,-1.38409399694589));
#71890=CARTESIAN_POINT('Ctrl Pts',(3.79235669640907,1.,-1.38409399694589));
#71891=CARTESIAN_POINT('Ctrl Pts',(3.78469969805134,-1.,-1.38425435883773));
#71892=CARTESIAN_POINT('Ctrl Pts',(3.78469969805134,1.,-1.38425435883773));
#71893=CARTESIAN_POINT('Ctrl Pts',(3.77704902230441,-1.,-1.38437354551435));
#71894=CARTESIAN_POINT('Ctrl Pts',(3.77704902230441,1.,-1.38437354551435));
#71895=CARTESIAN_POINT('Ctrl Pts',(3.76940473185775,-1.,-1.38445107339517));
#71896=CARTESIAN_POINT('Ctrl Pts',(3.76940473185775,1.,-1.38445107339517));
#71897=CARTESIAN_POINT('Ctrl Pts',(3.76176768271347,-1.,-1.38448675253343));
#71898=CARTESIAN_POINT('Ctrl Pts',(3.76176768271347,1.,-1.38448675253343));
#71899=CARTESIAN_POINT('Ctrl Pts',(3.75413976318727,-1.,-1.38448077997155));
#71900=CARTESIAN_POINT('Ctrl Pts',(3.75413976318727,1.,-1.38448077997155));
#71901=CARTESIAN_POINT('Ctrl Pts',(3.7465231716786,-1.,-1.38443344984389));
#71902=CARTESIAN_POINT('Ctrl Pts',(3.7465231716786,1.,-1.38443344984389));
#71903=CARTESIAN_POINT('Ctrl Pts',(3.73891976418099,-1.,-1.38434489156456));
#71904=CARTESIAN_POINT('Ctrl Pts',(3.73891976418099,1.,-1.38434489156456));
#71905=CARTESIAN_POINT('Ctrl Pts',(3.73133035859283,-1.,-1.38421479111531));
#71906=CARTESIAN_POINT('Ctrl Pts',(3.73133035859283,1.,-1.38421479111531));
#71907=CARTESIAN_POINT('Ctrl Pts',(3.72375409358805,-1.,-1.3840421342895));
#71908=CARTESIAN_POINT('Ctrl Pts',(3.72375409358805,1.,-1.3840421342895));
#71909=CARTESIAN_POINT('Ctrl Pts',(3.7161876605181,-1.,-1.38382489984585));
#71910=CARTESIAN_POINT('Ctrl Pts',(3.7161876605181,1.,-1.38382489984585));
#71911=CARTESIAN_POINT('Ctrl Pts',(3.70862680753343,-1.,-1.38356065402122));
#71912=CARTESIAN_POINT('Ctrl Pts',(3.70862680753343,1.,-1.38356065402122));
#71913=CARTESIAN_POINT('Ctrl Pts',(3.70106792167894,-1.,-1.38324717612862));
#71914=CARTESIAN_POINT('Ctrl Pts',(3.70106792167894,1.,-1.38324717612862));
#71915=CARTESIAN_POINT('Ctrl Pts',(3.69350967899523,-1.,-1.38288311171649));
#71916=CARTESIAN_POINT('Ctrl Pts',(3.69350967899523,1.,-1.38288311171649));
#71917=CARTESIAN_POINT('Ctrl Pts',(3.68595444983844,-1.,-1.38246852827185));
#71918=CARTESIAN_POINT('Ctrl Pts',(3.68595444983844,1.,-1.38246852827185));
#71919=CARTESIAN_POINT('Ctrl Pts',(3.6784103848243,-1.,-1.38200574290626));
#71920=CARTESIAN_POINT('Ctrl Pts',(3.6784103848243,1.,-1.38200574290626));
#71921=CARTESIAN_POINT('Ctrl Pts',(3.67088843112282,-1.,-1.38149812653876));
#71922=CARTESIAN_POINT('Ctrl Pts',(3.67088843112282,1.,-1.38149812653876));
#71923=CARTESIAN_POINT('Ctrl Pts',(3.66339848520874,-1.,-1.38094856333558));
#71924=CARTESIAN_POINT('Ctrl Pts',(3.66339848520874,1.,-1.38094856333558));
#71925=CARTESIAN_POINT('Ctrl Pts',(3.65594554404396,-1.,-1.38035791051215));
#71926=CARTESIAN_POINT('Ctrl Pts',(3.65594554404396,1.,-1.38035791051215));
#71927=CARTESIAN_POINT('Ctrl Pts',(3.64852652756444,-1.,-1.37972372481598));
#71928=CARTESIAN_POINT('Ctrl Pts',(3.64852652756444,1.,-1.37972372481598));
#71929=CARTESIAN_POINT('Ctrl Pts',(3.64112507791112,-1.,-1.37903818567347));
#71930=CARTESIAN_POINT('Ctrl Pts',(3.64112507791112,1.,-1.37903818567347));
#71931=CARTESIAN_POINT('Ctrl Pts',(3.63371727442448,-1.,-1.37829035457325));
#71932=CARTESIAN_POINT('Ctrl Pts',(3.63371727442448,1.,-1.37829035457325));
#71933=CARTESIAN_POINT('Ctrl Pts',(3.62628098665112,-1.,-1.37746987919868));
#71934=CARTESIAN_POINT('Ctrl Pts',(3.62628098665112,1.,-1.37746987919868));
#71935=CARTESIAN_POINT('Ctrl Pts',(3.61880481160408,-1.,-1.37657053403102));
#71936=CARTESIAN_POINT('Ctrl Pts',(3.61880481160408,1.,-1.37657053403102));
#71937=CARTESIAN_POINT('Ctrl Pts',(3.61129546591082,-1.,-1.37559314436641));
#71938=CARTESIAN_POINT('Ctrl Pts',(3.61129546591082,1.,-1.37559314436641));
#71939=CARTESIAN_POINT('Ctrl Pts',(3.60379020124038,-1.,-1.37455051379642));
#71940=CARTESIAN_POINT('Ctrl Pts',(3.60379020124038,1.,-1.37455051379642));
#71941=CARTESIAN_POINT('Ctrl Pts',(3.59634627869117,-1.,-1.37346320103184));
#71942=CARTESIAN_POINT('Ctrl Pts',(3.59634627869117,1.,-1.37346320103184));
#71943=CARTESIAN_POINT('Ctrl Pts',(3.5890185384643,-1.,-1.37235053661));
#71944=CARTESIAN_POINT('Ctrl Pts',(3.5890185384643,1.,-1.37235053661));
#71945=CARTESIAN_POINT('Ctrl Pts',(3.58183885982745,-1.,-1.37122241663073));
#71946=CARTESIAN_POINT('Ctrl Pts',(3.58183885982745,1.,-1.37122241663073));
#71947=CARTESIAN_POINT('Ctrl Pts',(3.57479875549453,-1.,-1.37007229485646));
#71948=CARTESIAN_POINT('Ctrl Pts',(3.57479875549453,1.,-1.37007229485646));
#71949=CARTESIAN_POINT('Ctrl Pts',(3.56782080304554,-1.,-1.36886584973349));
#71950=CARTESIAN_POINT('Ctrl Pts',(3.56782080304554,1.,-1.36886584973349));
#71951=CARTESIAN_POINT('Ctrl Pts',(3.56077662028492,-1.,-1.36754771771174));
#71952=CARTESIAN_POINT('Ctrl Pts',(3.56077662028492,1.,-1.36754771771174));
#71953=CARTESIAN_POINT('Ctrl Pts',(3.55353883995793,-1.,-1.36606145456711));
#71954=CARTESIAN_POINT('Ctrl Pts',(3.55353883995793,1.,-1.36606145456711));
#71955=CARTESIAN_POINT('Ctrl Pts',(3.54602591832893,-1.,-1.36436666257568));
#71956=CARTESIAN_POINT('Ctrl Pts',(3.54602591832893,1.,-1.36436666257568));
#71957=CARTESIAN_POINT('Ctrl Pts',(3.53824396425032,-1.,-1.36245507339334));
#71958=CARTESIAN_POINT('Ctrl Pts',(3.53824396425032,1.,-1.36245507339334));
#71959=CARTESIAN_POINT('Ctrl Pts',(3.53034464961849,-1.,-1.36037259643827));
#71960=CARTESIAN_POINT('Ctrl Pts',(3.53034464961849,1.,-1.36037259643827));
#71961=CARTESIAN_POINT('Ctrl Pts',(3.52261776117121,-1.,-1.35821701528975));
#71962=CARTESIAN_POINT('Ctrl Pts',(3.52261776117121,1.,-1.35821701528975));
#71963=CARTESIAN_POINT('Ctrl Pts',(3.51542230699919,-1.,-1.35611275237288));
#71964=CARTESIAN_POINT('Ctrl Pts',(3.51542230699919,1.,-1.35611275237288));
#71965=CARTESIAN_POINT('Ctrl Pts',(3.50913227060177,-1.,-1.35419113576022));
#71966=CARTESIAN_POINT('Ctrl Pts',(3.50913227060177,1.,-1.35419113576022));
#71967=CARTESIAN_POINT('Ctrl Pts',(3.50408168106113,-1.,-1.3525703284343));
#71968=CARTESIAN_POINT('Ctrl Pts',(3.50408168106113,1.,-1.3525703284343));
#71969=CARTESIAN_POINT('Ctrl Pts',(3.50049707063673,-1.,-1.35133076331065));
#71970=CARTESIAN_POINT('Ctrl Pts',(3.50049707063673,1.,-1.35133076331065));
#71971=CARTESIAN_POINT('Ctrl Pts',(3.49888720256612,-1.,-1.35067437417289));
#71972=CARTESIAN_POINT('Ctrl Pts',(3.49888720256612,1.,-1.35067437417289));
#71973=CARTESIAN_POINT('Ctrl Pts',(3.49840357193384,-1.,-1.35037650302887));
#71974=CARTESIAN_POINT('Ctrl Pts',(3.49840357193384,1.,-1.35037650302887));
#71975=CARTESIAN_POINT('Ctrl Pts',(3.49840260053616,-1.,-1.35026426118352));
#71976=CARTESIAN_POINT('Ctrl Pts',(3.49840260053616,1.,-1.35026426118352));
#71977=CARTESIAN_POINT('Ctrl Pts',(3.49848248301936,-1.,-1.35022972712301));
#71978=CARTESIAN_POINT('Ctrl Pts',(3.49848248301936,1.,-1.35022972712301));
#71979=CARTESIAN_POINT('',(3.97027773754922,1.,-1.36999806084572));
#71980=CARTESIAN_POINT('Ctrl Pts',(3.97027773754922,1.,-1.36999806084572));
#71981=CARTESIAN_POINT('Ctrl Pts',(3.9687184694173,1.,-1.37020239094758));
#71982=CARTESIAN_POINT('Ctrl Pts',(3.96560037975788,1.,-1.37060761746027));
#71983=CARTESIAN_POINT('Ctrl Pts',(3.96092458508407,1.,-1.37120515615663));
#71984=CARTESIAN_POINT('Ctrl Pts',(3.95469287283105,1.,-1.37198126433139));
#71985=CARTESIAN_POINT('Ctrl Pts',(3.94690771786926,1.,-1.37291699203423));
#71986=CARTESIAN_POINT('Ctrl Pts',(3.93912709041791,1.,-1.37381821967499));
#71987=CARTESIAN_POINT('Ctrl Pts',(3.93135106761941,1.,-1.37468482215784));
#71988=CARTESIAN_POINT('Ctrl Pts',(3.92357976987132,1.,-1.37551664448057));
#71989=CARTESIAN_POINT('Ctrl Pts',(3.91581337461825,1.,-1.37631350505516));
#71990=CARTESIAN_POINT('Ctrl Pts',(3.90805209522729,1.,-1.3770751963376));
#71991=CARTESIAN_POINT('Ctrl Pts',(3.90029615196255,1.,-1.3778014851263));
#71992=CARTESIAN_POINT('Ctrl Pts',(3.89254574338385,1.,-1.37849211287981));
#71993=CARTESIAN_POINT('Ctrl Pts',(3.88480102249461,1.,-1.37914679719446));
#71994=CARTESIAN_POINT('Ctrl Pts',(3.87706205830865,1.,-1.37976523097187));
#71995=CARTESIAN_POINT('Ctrl Pts',(3.86932885813403,1.,-1.38034709213129));
#71996=CARTESIAN_POINT('Ctrl Pts',(3.86160143044187,1.,-1.38089205993068));
#71997=CARTESIAN_POINT('Ctrl Pts',(3.85387983979557,1.,-1.38139983115075));
#71998=CARTESIAN_POINT('Ctrl Pts',(3.84616425605705,1.,-1.38187013346089));
#71999=CARTESIAN_POINT('Ctrl Pts',(3.83845502790609,1.,-1.38230274828774));
#72000=CARTESIAN_POINT('Ctrl Pts',(3.83075266982138,1.,-1.38269750245086));
#72001=CARTESIAN_POINT('Ctrl Pts',(3.82305771743715,1.,-1.38305421262724));
#72002=CARTESIAN_POINT('Ctrl Pts',(3.81537060817765,1.,-1.38337263902766));
#72003=CARTESIAN_POINT('Ctrl Pts',(3.80769156398429,1.,-1.38365244046226));
#72004=CARTESIAN_POINT('Ctrl Pts',(3.80002044322169,1.,-1.38389311766701));
#72005=CARTESIAN_POINT('Ctrl Pts',(3.79235669640907,1.,-1.38409399694589));
#72006=CARTESIAN_POINT('Ctrl Pts',(3.78469969805134,1.,-1.38425435883773));
#72007=CARTESIAN_POINT('Ctrl Pts',(3.77704902230441,1.,-1.38437354551435));
#72008=CARTESIAN_POINT('Ctrl Pts',(3.76940473185775,1.,-1.38445107339517));
#72009=CARTESIAN_POINT('Ctrl Pts',(3.76176768271347,1.,-1.38448675253343));
#72010=CARTESIAN_POINT('Ctrl Pts',(3.75413976318727,1.,-1.38448077997155));
#72011=CARTESIAN_POINT('Ctrl Pts',(3.7465231716786,1.,-1.38443344984389));
#72012=CARTESIAN_POINT('Ctrl Pts',(3.73891976418099,1.,-1.38434489156456));
#72013=CARTESIAN_POINT('Ctrl Pts',(3.73133035859283,1.,-1.38421479111531));
#72014=CARTESIAN_POINT('Ctrl Pts',(3.72375409358805,1.,-1.3840421342895));
#72015=CARTESIAN_POINT('Ctrl Pts',(3.7161876605181,1.,-1.38382489984585));
#72016=CARTESIAN_POINT('Ctrl Pts',(3.70862680753343,1.,-1.38356065402122));
#72017=CARTESIAN_POINT('Ctrl Pts',(3.70106792167894,1.,-1.38324717612862));
#72018=CARTESIAN_POINT('Ctrl Pts',(3.69350967899523,1.,-1.38288311171649));
#72019=CARTESIAN_POINT('Ctrl Pts',(3.68595444983844,1.,-1.38246852827185));
#72020=CARTESIAN_POINT('Ctrl Pts',(3.6784103848243,1.,-1.38200574290626));
#72021=CARTESIAN_POINT('Ctrl Pts',(3.67088843112282,1.,-1.38149812653876));
#72022=CARTESIAN_POINT('Ctrl Pts',(3.66339848520874,1.,-1.38094856333558));
#72023=CARTESIAN_POINT('Ctrl Pts',(3.65594554404396,1.,-1.38035791051215));
#72024=CARTESIAN_POINT('Ctrl Pts',(3.64852652756444,1.,-1.37972372481598));
#72025=CARTESIAN_POINT('Ctrl Pts',(3.64112507791112,1.,-1.37903818567347));
#72026=CARTESIAN_POINT('Ctrl Pts',(3.63371727442448,1.,-1.37829035457325));
#72027=CARTESIAN_POINT('Ctrl Pts',(3.62628098665112,1.,-1.37746987919868));
#72028=CARTESIAN_POINT('Ctrl Pts',(3.61880481160408,1.,-1.37657053403102));
#72029=CARTESIAN_POINT('Ctrl Pts',(3.61129546591082,1.,-1.37559314436641));
#72030=CARTESIAN_POINT('Ctrl Pts',(3.60379020124038,1.,-1.37455051379642));
#72031=CARTESIAN_POINT('Ctrl Pts',(3.59634627869117,1.,-1.37346320103184));
#72032=CARTESIAN_POINT('Ctrl Pts',(3.5890185384643,1.,-1.37235053661));
#72033=CARTESIAN_POINT('Ctrl Pts',(3.58183885982745,1.,-1.37122241663073));
#72034=CARTESIAN_POINT('Ctrl Pts',(3.57479875549453,1.,-1.37007229485646));
#72035=CARTESIAN_POINT('Ctrl Pts',(3.56782080304554,1.,-1.36886584973349));
#72036=CARTESIAN_POINT('Ctrl Pts',(3.56077662028492,1.,-1.36754771771174));
#72037=CARTESIAN_POINT('Ctrl Pts',(3.55353883995793,1.,-1.36606145456711));
#72038=CARTESIAN_POINT('Ctrl Pts',(3.54602591832893,1.,-1.36436666257568));
#72039=CARTESIAN_POINT('Ctrl Pts',(3.53824396425032,1.,-1.36245507339334));
#72040=CARTESIAN_POINT('Ctrl Pts',(3.53034464961849,1.,-1.36037259643827));
#72041=CARTESIAN_POINT('Ctrl Pts',(3.52261776117121,1.,-1.35821701528975));
#72042=CARTESIAN_POINT('Ctrl Pts',(3.51542230699919,1.,-1.35611275237288));
#72043=CARTESIAN_POINT('Ctrl Pts',(3.50913227060177,1.,-1.35419113576022));
#72044=CARTESIAN_POINT('Ctrl Pts',(3.50408168106113,1.,-1.3525703284343));
#72045=CARTESIAN_POINT('Ctrl Pts',(3.5007660381658,1.,-1.35142377279535));
#72046=CARTESIAN_POINT('Ctrl Pts',(3.49920025459856,1.,-1.35080045218652));
#72047=CARTESIAN_POINT('Ctrl Pts',(3.49861894124915,1.,-1.35049736560633));
#72048=CARTESIAN_POINT('Ctrl Pts',(3.49847119623841,1.,-1.35036670893102));
#72049=CARTESIAN_POINT('Ctrl Pts',(3.49844575334386,1.,-1.35032489087269));
#72050=CARTESIAN_POINT('',(3.97027773754922,0.,-1.36999806084572));
#72051=CARTESIAN_POINT('Ctrl Pts',(3.62397690409552,-1.,-0.963997613369571));
#72052=CARTESIAN_POINT('Ctrl Pts',(3.62397690409552,1.,-0.963997613369571));
#72053=CARTESIAN_POINT('Ctrl Pts',(3.62393257642191,-1.,-0.963922720982576));
#72054=CARTESIAN_POINT('Ctrl Pts',(3.62393257642191,1.,-0.963922720982576));
#72055=CARTESIAN_POINT('Ctrl Pts',(3.62399933640277,-1.,-0.963832486396056));
#72056=CARTESIAN_POINT('Ctrl Pts',(3.62399933640277,1.,-0.963832486396056));
#72057=CARTESIAN_POINT('Ctrl Pts',(3.62456568607055,-1.,-0.963875774532103));
#72058=CARTESIAN_POINT('Ctrl Pts',(3.62456568607055,1.,-0.963875774532103));
#72059=CARTESIAN_POINT('Ctrl Pts',(3.62625391255277,-1.,-0.964291001274619));
#72060=CARTESIAN_POINT('Ctrl Pts',(3.62625391255277,1.,-0.964291001274619));
#72061=CARTESIAN_POINT('Ctrl Pts',(3.62988252139998,-1.,-0.965395153165716));
#72062=CARTESIAN_POINT('Ctrl Pts',(3.62988252139998,1.,-0.965395153165716));
#72063=CARTESIAN_POINT('Ctrl Pts',(3.6349212208096,-1.,-0.967052554540878));
#72064=CARTESIAN_POINT('Ctrl Pts',(3.6349212208096,1.,-0.967052554540878));
#72065=CARTESIAN_POINT('Ctrl Pts',(3.64113946505393,-1.,-0.969195124674829));
#72066=CARTESIAN_POINT('Ctrl Pts',(3.64113946505393,1.,-0.969195124674829));
#72067=CARTESIAN_POINT('Ctrl Pts',(3.64819756447072,-1.,-0.971722122060278));
#72068=CARTESIAN_POINT('Ctrl Pts',(3.64819756447072,1.,-0.971722122060278));
#72069=CARTESIAN_POINT('Ctrl Pts',(3.6557157673487,-1.,-0.974519971354139));
#72070=CARTESIAN_POINT('Ctrl Pts',(3.6557157673487,1.,-0.974519971354139));
#72071=CARTESIAN_POINT('Ctrl Pts',(3.66333049637403,-1.,-0.977478312751416));
#72072=CARTESIAN_POINT('Ctrl Pts',(3.66333049637403,1.,-0.977478312751416));
#72073=CARTESIAN_POINT('Ctrl Pts',(3.67074983340444,-1.,-0.980505922458495));
#72074=CARTESIAN_POINT('Ctrl Pts',(3.67074983340444,1.,-0.980505922458495));
#72075=CARTESIAN_POINT('Ctrl Pts',(3.67782408841876,-1.,-0.983550791470865));
#72076=CARTESIAN_POINT('Ctrl Pts',(3.67782408841876,1.,-0.983550791470865));
#72077=CARTESIAN_POINT('Ctrl Pts',(3.6845531792623,-1.,-0.986602639864286));
#72078=CARTESIAN_POINT('Ctrl Pts',(3.6845531792623,1.,-0.986602639864286));
#72079=CARTESIAN_POINT('Ctrl Pts',(3.69102682138955,-1.,-0.989676715398859));
#72080=CARTESIAN_POINT('Ctrl Pts',(3.69102682138955,1.,-0.989676715398859));
#72081=CARTESIAN_POINT('Ctrl Pts',(3.69738123415696,-1.,-0.992802218332104));
#72082=CARTESIAN_POINT('Ctrl Pts',(3.69738123415696,1.,-0.992802218332104));
#72083=CARTESIAN_POINT('Ctrl Pts',(3.70375282282107,-1.,-0.996009819772432));
#72084=CARTESIAN_POINT('Ctrl Pts',(3.70375282282107,1.,-0.996009819772432));
#72085=CARTESIAN_POINT('Ctrl Pts',(3.7102243971387,-1.,-0.999317260756345));
#72086=CARTESIAN_POINT('Ctrl Pts',(3.7102243971387,1.,-0.999317260756345));
#72087=CARTESIAN_POINT('Ctrl Pts',(3.71680667125047,-1.,-1.00272423396802));
#72088=CARTESIAN_POINT('Ctrl Pts',(3.71680667125047,1.,-1.00272423396802));
#72089=CARTESIAN_POINT('Ctrl Pts',(3.72346803750544,-1.,-1.00622000735696));
#72090=CARTESIAN_POINT('Ctrl Pts',(3.72346803750544,1.,-1.00622000735696));
#72091=CARTESIAN_POINT('Ctrl Pts',(3.73015276704407,-1.,-1.00978798539491));
#72092=CARTESIAN_POINT('Ctrl Pts',(3.73015276704407,1.,-1.00978798539491));
#72093=CARTESIAN_POINT('Ctrl Pts',(3.73680245055747,-1.,-1.01341114319906));
#72094=CARTESIAN_POINT('Ctrl Pts',(3.73680245055747,1.,-1.01341114319906));
#72095=CARTESIAN_POINT('Ctrl Pts',(3.74337942504993,-1.,-1.01707794311088));
#72096=CARTESIAN_POINT('Ctrl Pts',(3.74337942504993,1.,-1.01707794311088));
#72097=CARTESIAN_POINT('Ctrl Pts',(3.74987777155873,-1.,-1.02078510487439));
#72098=CARTESIAN_POINT('Ctrl Pts',(3.74987777155873,1.,-1.02078510487439));
#72099=CARTESIAN_POINT('Ctrl Pts',(3.75631037456224,-1.,-1.02453429444668));
#72100=CARTESIAN_POINT('Ctrl Pts',(3.75631037456224,1.,-1.02453429444668));
#72101=CARTESIAN_POINT('Ctrl Pts',(3.76270122291245,-1.,-1.02833014458184));
#72102=CARTESIAN_POINT('Ctrl Pts',(3.76270122291245,1.,-1.02833014458184));
#72103=CARTESIAN_POINT('Ctrl Pts',(3.76907609832516,-1.,-1.03217786604919));
#72104=CARTESIAN_POINT('Ctrl Pts',(3.76907609832516,1.,-1.03217786604919));
#72105=CARTESIAN_POINT('Ctrl Pts',(3.77545283140427,-1.,-1.03608074678008));
#72106=CARTESIAN_POINT('Ctrl Pts',(3.77545283140427,1.,-1.03608074678008));
#72107=CARTESIAN_POINT('Ctrl Pts',(3.7818353500817,-1.,-1.04003862055798));
#72108=CARTESIAN_POINT('Ctrl Pts',(3.7818353500817,1.,-1.04003862055798));
#72109=CARTESIAN_POINT('Ctrl Pts',(3.78821910787179,-1.,-1.04404924374422));
#72110=CARTESIAN_POINT('Ctrl Pts',(3.78821910787179,1.,-1.04404924374422));
#72111=CARTESIAN_POINT('Ctrl Pts',(3.79459440308786,-1.,-1.04810913267639));
#72112=CARTESIAN_POINT('Ctrl Pts',(3.79459440308786,1.,-1.04810913267639));
#72113=CARTESIAN_POINT('Ctrl Pts',(3.80095039790681,-1.,-1.05221457990016));
#72114=CARTESIAN_POINT('Ctrl Pts',(3.80095039790681,1.,-1.05221457990016));
#72115=CARTESIAN_POINT('Ctrl Pts',(3.80727913637791,-1.,-1.05636266918644));
#72116=CARTESIAN_POINT('Ctrl Pts',(3.80727913637791,1.,-1.05636266918644));
#72117=CARTESIAN_POINT('Ctrl Pts',(3.8135786611749,-1.,-1.06055206187299));
#72118=CARTESIAN_POINT('Ctrl Pts',(3.8135786611749,1.,-1.06055206187299));
#72119=CARTESIAN_POINT('Ctrl Pts',(3.81985083953012,-1.,-1.0647824403893));
#72120=CARTESIAN_POINT('Ctrl Pts',(3.81985083953012,1.,-1.0647824403893));
#72121=CARTESIAN_POINT('Ctrl Pts',(3.82609989967276,-1.,-1.06905413180359));
#72122=CARTESIAN_POINT('Ctrl Pts',(3.82609989967276,1.,-1.06905413180359));
#72123=CARTESIAN_POINT('Ctrl Pts',(3.83233071195144,-1.,-1.07336766633459));
#72124=CARTESIAN_POINT('Ctrl Pts',(3.83233071195144,1.,-1.07336766633459));
#72125=CARTESIAN_POINT('Ctrl Pts',(3.83854714117491,-1.,-1.07772335353858));
#72126=CARTESIAN_POINT('Ctrl Pts',(3.83854714117491,1.,-1.07772335353858));
#72127=CARTESIAN_POINT('Ctrl Pts',(3.8447504803063,-1.,-1.08212087917991));
#72128=CARTESIAN_POINT('Ctrl Pts',(3.8447504803063,1.,-1.08212087917991));
#72129=CARTESIAN_POINT('Ctrl Pts',(3.85094025222713,-1.,-1.08655950846384));
#72130=CARTESIAN_POINT('Ctrl Pts',(3.85094025222713,1.,-1.08655950846384));
#72131=CARTESIAN_POINT('Ctrl Pts',(3.85711487933931,-1.,-1.09103825516294));
#72132=CARTESIAN_POINT('Ctrl Pts',(3.85711487933931,1.,-1.09103825516294));
#72133=CARTESIAN_POINT('Ctrl Pts',(3.86327241021247,-1.,-1.09555606505013));
#72134=CARTESIAN_POINT('Ctrl Pts',(3.86327241021247,1.,-1.09555606505013));
#72135=CARTESIAN_POINT('Ctrl Pts',(3.86941120134849,-1.,-1.10011198761195));
#72136=CARTESIAN_POINT('Ctrl Pts',(3.86941120134849,1.,-1.10011198761195));
#72137=CARTESIAN_POINT('Ctrl Pts',(3.87553067187514,-1.,-1.10470536603287));
#72138=CARTESIAN_POINT('Ctrl Pts',(3.87553067187514,1.,-1.10470536603287));
#72139=CARTESIAN_POINT('Ctrl Pts',(3.88163105531724,-1.,-1.10933577224008));
#72140=CARTESIAN_POINT('Ctrl Pts',(3.88163105531724,1.,-1.10933577224008));
#72141=CARTESIAN_POINT('Ctrl Pts',(3.88771308285171,-1.,-1.11400292434429));
#72142=CARTESIAN_POINT('Ctrl Pts',(3.88771308285171,1.,-1.11400292434429));
#72143=CARTESIAN_POINT('Ctrl Pts',(3.89377768340344,-1.,-1.11870660794603));
#72144=CARTESIAN_POINT('Ctrl Pts',(3.89377768340344,1.,-1.11870660794603));
#72145=CARTESIAN_POINT('Ctrl Pts',(3.89982569750025,-1.,-1.12344660099043));
#72146=CARTESIAN_POINT('Ctrl Pts',(3.89982569750025,1.,-1.12344660099043));
#72147=CARTESIAN_POINT('Ctrl Pts',(3.90585753318737,-1.,-1.12822258281553));
#72148=CARTESIAN_POINT('Ctrl Pts',(3.90585753318737,1.,-1.12822258281553));
#72149=CARTESIAN_POINT('Ctrl Pts',(3.91187321145649,-1.,-1.13303414693896));
#72150=CARTESIAN_POINT('Ctrl Pts',(3.91187321145649,1.,-1.13303414693896));
#72151=CARTESIAN_POINT('Ctrl Pts',(3.91787251936827,-1.,-1.13788084225554));
#72152=CARTESIAN_POINT('Ctrl Pts',(3.91787251936827,1.,-1.13788084225554));
#72153=CARTESIAN_POINT('Ctrl Pts',(3.92385513133997,-1.,-1.14276220561593));
#72154=CARTESIAN_POINT('Ctrl Pts',(3.92385513133997,1.,-1.14276220561593));
#72155=CARTESIAN_POINT('Ctrl Pts',(3.92982073294257,-1.,-1.14767779451124));
#72156=CARTESIAN_POINT('Ctrl Pts',(3.92982073294257,1.,-1.14767779451124));
#72157=CARTESIAN_POINT('Ctrl Pts',(3.9357691705628,-1.,-1.1526272271632));
#72158=CARTESIAN_POINT('Ctrl Pts',(3.9357691705628,1.,-1.1526272271632));
#72159=CARTESIAN_POINT('Ctrl Pts',(3.94170046685203,-1.,-1.15761018340956));
#72160=CARTESIAN_POINT('Ctrl Pts',(3.94170046685203,1.,-1.15761018340956));
#72161=CARTESIAN_POINT('Ctrl Pts',(3.94761474780583,-1.,-1.16262637999157));
#72162=CARTESIAN_POINT('Ctrl Pts',(3.94761474780583,1.,-1.16262637999157));
#72163=CARTESIAN_POINT('Ctrl Pts',(3.95351219509876,-1.,-1.16767555244438));
#72164=CARTESIAN_POINT('Ctrl Pts',(3.95351219509876,1.,-1.16767555244438));
#72165=CARTESIAN_POINT('Ctrl Pts',(3.95939299213276,-1.,-1.17275743590361));
#72166=CARTESIAN_POINT('Ctrl Pts',(3.95939299213276,1.,-1.17275743590361));
#72167=CARTESIAN_POINT('Ctrl Pts',(3.96525726358159,-1.,-1.17787174135592));
#72168=CARTESIAN_POINT('Ctrl Pts',(3.96525726358159,1.,-1.17787174135592));
#72169=CARTESIAN_POINT('Ctrl Pts',(3.97110505165415,-1.,-1.18301815039831));
#72170=CARTESIAN_POINT('Ctrl Pts',(3.97110505165415,1.,-1.18301815039831));
#72171=CARTESIAN_POINT('Ctrl Pts',(3.97693634767754,-1.,-1.18819633715539));
#72172=CARTESIAN_POINT('Ctrl Pts',(3.97693634767754,1.,-1.18819633715539));
#72173=CARTESIAN_POINT('Ctrl Pts',(3.98275111052561,-1.,-1.19340598349475));
#72174=CARTESIAN_POINT('Ctrl Pts',(3.98275111052561,1.,-1.19340598349475));
#72175=CARTESIAN_POINT('Ctrl Pts',(3.98854928957189,-1.,-1.19864679609566));
#72176=CARTESIAN_POINT('Ctrl Pts',(3.98854928957189,1.,-1.19864679609566));
#72177=CARTESIAN_POINT('Ctrl Pts',(3.99433084799666,-1.,-1.20391852375139));
#72178=CARTESIAN_POINT('Ctrl Pts',(3.99433084799666,1.,-1.20391852375139));
#72179=CARTESIAN_POINT('Ctrl Pts',(4.00009577950721,-1.,-1.20922097029551));
#72180=CARTESIAN_POINT('Ctrl Pts',(4.00009577950721,1.,-1.20922097029551));
#72181=CARTESIAN_POINT('Ctrl Pts',(4.00584409522722,-1.,-1.21455398918133));
#72182=CARTESIAN_POINT('Ctrl Pts',(4.00584409522722,1.,-1.21455398918133));
#72183=CARTESIAN_POINT('Ctrl Pts',(4.01042947140789,-1.,-1.21884478244403));
#72184=CARTESIAN_POINT('Ctrl Pts',(4.01042947140789,1.,-1.21884478244403));
#72185=CARTESIAN_POINT('Ctrl Pts',(4.01386104433519,-1.,-1.22207656455845));
#72186=CARTESIAN_POINT('Ctrl Pts',(4.01386104433519,1.,-1.22207656455845));
#72187=CARTESIAN_POINT('Ctrl Pts',(4.01614544569895,-1.,-1.22423716681317));
#72188=CARTESIAN_POINT('Ctrl Pts',(4.01614544569895,1.,-1.22423716681317));
#72189=CARTESIAN_POINT('Ctrl Pts',(4.01728681790024,-1.,-1.22531898815164));
#72190=CARTESIAN_POINT('Ctrl Pts',(4.01728681790024,1.,-1.22531898815164));
#72191=CARTESIAN_POINT('',(3.62400312501199,1.,-0.963899035118984));
#72192=CARTESIAN_POINT('Ctrl Pts',(3.62400312501199,-1.,-0.963899035118986));
#72193=CARTESIAN_POINT('Ctrl Pts',(3.62400312501199,-0.666666666666667,
-0.963899035118986));
#72194=CARTESIAN_POINT('Ctrl Pts',(3.62400312501199,-0.333333333333333,
-0.963899035118986));
#72195=CARTESIAN_POINT('Ctrl Pts',(3.62400312501199,0.333333333333333,-0.963899035118986));
#72196=CARTESIAN_POINT('Ctrl Pts',(3.62400312501199,0.666666666666667,-0.963899035118986));
#72197=CARTESIAN_POINT('Ctrl Pts',(3.62400312501199,1.,-0.963899035118986));
#72198=CARTESIAN_POINT('',(4.01728681790024,1.,-1.22531898815164));
#72199=CARTESIAN_POINT('',(4.01728681790024,0.,-1.22531898815164));
#72200=CARTESIAN_POINT('Ctrl Pts',(3.62400312501199,1.,-0.963899035118985));
#72201=CARTESIAN_POINT('Ctrl Pts',(3.62404828878374,1.,-0.963880158556713));
#72202=CARTESIAN_POINT('Ctrl Pts',(3.62424461507455,1.,-0.963861297423579));
#72203=CARTESIAN_POINT('Ctrl Pts',(3.62489305727516,1.,-0.96395778264259));
#72204=CARTESIAN_POINT('Ctrl Pts',(3.62652618145252,1.,-0.964373850166082));
#72205=CARTESIAN_POINT('Ctrl Pts',(3.62988252139998,1.,-0.965395153165716));
#72206=CARTESIAN_POINT('Ctrl Pts',(3.6349212208096,1.,-0.967052554540878));
#72207=CARTESIAN_POINT('Ctrl Pts',(3.64113946505393,1.,-0.969195124674829));
#72208=CARTESIAN_POINT('Ctrl Pts',(3.64819756447072,1.,-0.971722122060278));
#72209=CARTESIAN_POINT('Ctrl Pts',(3.6557157673487,1.,-0.974519971354139));
#72210=CARTESIAN_POINT('Ctrl Pts',(3.66333049637403,1.,-0.977478312751416));
#72211=CARTESIAN_POINT('Ctrl Pts',(3.67074983340444,1.,-0.980505922458495));
#72212=CARTESIAN_POINT('Ctrl Pts',(3.67782408841876,1.,-0.983550791470865));
#72213=CARTESIAN_POINT('Ctrl Pts',(3.6845531792623,1.,-0.986602639864286));
#72214=CARTESIAN_POINT('Ctrl Pts',(3.69102682138955,1.,-0.989676715398859));
#72215=CARTESIAN_POINT('Ctrl Pts',(3.69738123415696,1.,-0.992802218332104));
#72216=CARTESIAN_POINT('Ctrl Pts',(3.70375282282107,1.,-0.996009819772432));
#72217=CARTESIAN_POINT('Ctrl Pts',(3.7102243971387,1.,-0.999317260756345));
#72218=CARTESIAN_POINT('Ctrl Pts',(3.71680667125047,1.,-1.00272423396802));
#72219=CARTESIAN_POINT('Ctrl Pts',(3.72346803750544,1.,-1.00622000735696));
#72220=CARTESIAN_POINT('Ctrl Pts',(3.73015276704407,1.,-1.00978798539491));
#72221=CARTESIAN_POINT('Ctrl Pts',(3.73680245055747,1.,-1.01341114319906));
#72222=CARTESIAN_POINT('Ctrl Pts',(3.74337942504993,1.,-1.01707794311088));
#72223=CARTESIAN_POINT('Ctrl Pts',(3.74987777155873,1.,-1.02078510487439));
#72224=CARTESIAN_POINT('Ctrl Pts',(3.75631037456224,1.,-1.02453429444668));
#72225=CARTESIAN_POINT('Ctrl Pts',(3.76270122291245,1.,-1.02833014458184));
#72226=CARTESIAN_POINT('Ctrl Pts',(3.76907609832516,1.,-1.03217786604919));
#72227=CARTESIAN_POINT('Ctrl Pts',(3.77545283140427,1.,-1.03608074678008));
#72228=CARTESIAN_POINT('Ctrl Pts',(3.7818353500817,1.,-1.04003862055798));
#72229=CARTESIAN_POINT('Ctrl Pts',(3.78821910787179,1.,-1.04404924374422));
#72230=CARTESIAN_POINT('Ctrl Pts',(3.79459440308786,1.,-1.04810913267639));
#72231=CARTESIAN_POINT('Ctrl Pts',(3.80095039790681,1.,-1.05221457990016));
#72232=CARTESIAN_POINT('Ctrl Pts',(3.80727913637791,1.,-1.05636266918644));
#72233=CARTESIAN_POINT('Ctrl Pts',(3.8135786611749,1.,-1.06055206187299));
#72234=CARTESIAN_POINT('Ctrl Pts',(3.81985083953012,1.,-1.0647824403893));
#72235=CARTESIAN_POINT('Ctrl Pts',(3.82609989967276,1.,-1.06905413180359));
#72236=CARTESIAN_POINT('Ctrl Pts',(3.83233071195144,1.,-1.07336766633459));
#72237=CARTESIAN_POINT('Ctrl Pts',(3.83854714117491,1.,-1.07772335353858));
#72238=CARTESIAN_POINT('Ctrl Pts',(3.8447504803063,1.,-1.08212087917991));
#72239=CARTESIAN_POINT('Ctrl Pts',(3.85094025222713,1.,-1.08655950846384));
#72240=CARTESIAN_POINT('Ctrl Pts',(3.85711487933931,1.,-1.09103825516294));
#72241=CARTESIAN_POINT('Ctrl Pts',(3.86327241021247,1.,-1.09555606505013));
#72242=CARTESIAN_POINT('Ctrl Pts',(3.86941120134849,1.,-1.10011198761195));
#72243=CARTESIAN_POINT('Ctrl Pts',(3.87553067187514,1.,-1.10470536603287));
#72244=CARTESIAN_POINT('Ctrl Pts',(3.88163105531724,1.,-1.10933577224008));
#72245=CARTESIAN_POINT('Ctrl Pts',(3.88771308285171,1.,-1.11400292434429));
#72246=CARTESIAN_POINT('Ctrl Pts',(3.89377768340344,1.,-1.11870660794603));
#72247=CARTESIAN_POINT('Ctrl Pts',(3.89982569750025,1.,-1.12344660099043));
#72248=CARTESIAN_POINT('Ctrl Pts',(3.90585753318737,1.,-1.12822258281553));
#72249=CARTESIAN_POINT('Ctrl Pts',(3.91187321145649,1.,-1.13303414693896));
#72250=CARTESIAN_POINT('Ctrl Pts',(3.91787251936827,1.,-1.13788084225554));
#72251=CARTESIAN_POINT('Ctrl Pts',(3.92385513133997,1.,-1.14276220561593));
#72252=CARTESIAN_POINT('Ctrl Pts',(3.92982073294257,1.,-1.14767779451124));
#72253=CARTESIAN_POINT('Ctrl Pts',(3.9357691705628,1.,-1.1526272271632));
#72254=CARTESIAN_POINT('Ctrl Pts',(3.94170046685203,1.,-1.15761018340956));
#72255=CARTESIAN_POINT('Ctrl Pts',(3.94761474780583,1.,-1.16262637999157));
#72256=CARTESIAN_POINT('Ctrl Pts',(3.95351219509876,1.,-1.16767555244438));
#72257=CARTESIAN_POINT('Ctrl Pts',(3.95939299213276,1.,-1.17275743590361));
#72258=CARTESIAN_POINT('Ctrl Pts',(3.96525726358159,1.,-1.17787174135592));
#72259=CARTESIAN_POINT('Ctrl Pts',(3.97110505165415,1.,-1.18301815039831));
#72260=CARTESIAN_POINT('Ctrl Pts',(3.97693634767754,1.,-1.18819633715539));
#72261=CARTESIAN_POINT('Ctrl Pts',(3.98275111052561,1.,-1.19340598349475));
#72262=CARTESIAN_POINT('Ctrl Pts',(3.98854928957189,1.,-1.19864679609566));
#72263=CARTESIAN_POINT('Ctrl Pts',(3.99433084799666,1.,-1.20391852375139));
#72264=CARTESIAN_POINT('Ctrl Pts',(4.00009577950721,1.,-1.20922097029551));
#72265=CARTESIAN_POINT('Ctrl Pts',(4.00584409522722,1.,-1.21455398918133));
#72266=CARTESIAN_POINT('Ctrl Pts',(4.01042947140789,1.,-1.21884478244403));
#72267=CARTESIAN_POINT('Ctrl Pts',(4.01386104433519,1.,-1.22207656455845));
#72268=CARTESIAN_POINT('Ctrl Pts',(4.01614544569895,1.,-1.22423716681317));
#72269=CARTESIAN_POINT('Ctrl Pts',(4.01728681790024,1.,-1.22531898815164));
#72270=CARTESIAN_POINT('Origin',(4.01728681790024,0.,-1.22531898815164));
#72271=CARTESIAN_POINT('',(3.97027773754922,1.,-1.36999806084572));
#72272=CARTESIAN_POINT('Origin',(0.,0.,0.));
#72273=CARTESIAN_POINT('',(3.66661143271648,1.,-0.786422660833743));
#72274=CARTESIAN_POINT('Origin',(0.,1.,0.));
#72275=CARTESIAN_POINT('Ctrl Pts',(3.66661143271648,1.,-0.786422660833743));
#72276=CARTESIAN_POINT('Ctrl Pts',(3.66661143271648,0.666666666666667,-0.786422660833743));
#72277=CARTESIAN_POINT('Ctrl Pts',(3.66661143271648,0.333333333333333,-0.786422660833743));
#72278=CARTESIAN_POINT('Ctrl Pts',(3.66661143271648,-0.333333333333333,
-0.786422660833743));
#72279=CARTESIAN_POINT('Ctrl Pts',(3.66661143271648,-0.666666666666667,
-0.786422660833742));
#72280=CARTESIAN_POINT('Ctrl Pts',(3.66661143271648,-1.,-0.786422660833742));
#72281=CARTESIAN_POINT('Ctrl Pts',(4.13571194405636,-1.,-0.73204283740062));
#72282=CARTESIAN_POINT('Ctrl Pts',(4.13571194405636,1.,-0.73204283740062));
#72283=CARTESIAN_POINT('Ctrl Pts',(4.13420383737278,-1.,-0.732488575135926));
#72284=CARTESIAN_POINT('Ctrl Pts',(4.13420383737278,1.,-0.732488575135926));
#72285=CARTESIAN_POINT('Ctrl Pts',(4.13118752796397,-1.,-0.733376589325634));
#72286=CARTESIAN_POINT('Ctrl Pts',(4.13118752796397,1.,-0.733376589325634));
#72287=CARTESIAN_POINT('Ctrl Pts',(4.12666277572794,-1.,-0.734698226767513));
#72288=CARTESIAN_POINT('Ctrl Pts',(4.12666277572794,1.,-0.734698226767513));
#72289=CARTESIAN_POINT('Ctrl Pts',(4.12062919626082,-1.,-0.736439634335347));
#72290=CARTESIAN_POINT('Ctrl Pts',(4.12062919626082,1.,-0.736439634335347));
#72291=CARTESIAN_POINT('Ctrl Pts',(4.11308626953795,-1.,-0.738581708229119));
#72292=CARTESIAN_POINT('Ctrl Pts',(4.11308626953795,1.,-0.738581708229119));
#72293=CARTESIAN_POINT('Ctrl Pts',(4.1055424175856,-1.,-0.740688998555152));
#72294=CARTESIAN_POINT('Ctrl Pts',(4.1055424175856,1.,-0.740688998555152));
#72295=CARTESIAN_POINT('Ctrl Pts',(4.09799769702712,-1.,-0.742761369690018));
#72296=CARTESIAN_POINT('Ctrl Pts',(4.09799769702712,1.,-0.742761369690018));
#72297=CARTESIAN_POINT('Ctrl Pts',(4.09045220253011,-1.,-0.744798649705514));
#72298=CARTESIAN_POINT('Ctrl Pts',(4.09045220253011,1.,-0.744798649705514));
#72299=CARTESIAN_POINT('Ctrl Pts',(4.08290608094789,-1.,-0.746800631490822));
#72300=CARTESIAN_POINT('Ctrl Pts',(4.08290608094789,1.,-0.746800631490822));
#72301=CARTESIAN_POINT('Ctrl Pts',(4.07535951055363,-1.,-0.748767076679177));
#72302=CARTESIAN_POINT('Ctrl Pts',(4.07535951055363,1.,-0.748767076679177));
#72303=CARTESIAN_POINT('Ctrl Pts',(4.06781267241886,-1.,-0.750697720483176));
#72304=CARTESIAN_POINT('Ctrl Pts',(4.06781267241886,1.,-0.750697720483176));
#72305=CARTESIAN_POINT('Ctrl Pts',(4.06026572221399,-1.,-0.752592276482869));
#72306=CARTESIAN_POINT('Ctrl Pts',(4.06026572221399,1.,-0.752592276482869));
#72307=CARTESIAN_POINT('Ctrl Pts',(4.05271876688106,-1.,-0.754450441816412));
#72308=CARTESIAN_POINT('Ctrl Pts',(4.05271876688106,1.,-0.754450441816412));
#72309=CARTESIAN_POINT('Ctrl Pts',(4.04517182654344,-1.,-0.756271902370187));
#72310=CARTESIAN_POINT('Ctrl Pts',(4.04517182654344,1.,-0.756271902370187));
#72311=CARTESIAN_POINT('Ctrl Pts',(4.03762485803468,-1.,-0.758056338885554));
#72312=CARTESIAN_POINT('Ctrl Pts',(4.03762485803468,1.,-0.758056338885554));
#72313=CARTESIAN_POINT('Ctrl Pts',(4.0300778195465,-1.,-0.759803433244166));
#72314=CARTESIAN_POINT('Ctrl Pts',(4.0300778195465,1.,-0.759803433244166));
#72315=CARTESIAN_POINT('Ctrl Pts',(4.02253072741347,-1.,-0.761512875859942));
#72316=CARTESIAN_POINT('Ctrl Pts',(4.02253072741347,1.,-0.761512875859942));
#72317=CARTESIAN_POINT('Ctrl Pts',(4.01498370680434,-1.,-0.763184371182827));
#72318=CARTESIAN_POINT('Ctrl Pts',(4.01498370680434,1.,-0.763184371182827));
#72319=CARTESIAN_POINT('Ctrl Pts',(4.00743706791366,-1.,-0.764817648784947));
#72320=CARTESIAN_POINT('Ctrl Pts',(4.00743706791366,1.,-0.764817648784947));
#72321=CARTESIAN_POINT('Ctrl Pts',(3.99989129179464,-1.,-0.766412457135786));
#72322=CARTESIAN_POINT('Ctrl Pts',(3.99989129179464,1.,-0.766412457135786));
#72323=CARTESIAN_POINT('Ctrl Pts',(3.99234687880892,-1.,-0.767968531377708));
#72324=CARTESIAN_POINT('Ctrl Pts',(3.99234687880892,1.,-0.767968531377708));
#72325=CARTESIAN_POINT('Ctrl Pts',(3.98480422348403,-1.,-0.76948556624546));
#72326=CARTESIAN_POINT('Ctrl Pts',(3.98480422348403,1.,-0.76948556624546));
#72327=CARTESIAN_POINT('Ctrl Pts',(3.97726349165507,-1.,-0.770963190030504));
#72328=CARTESIAN_POINT('Ctrl Pts',(3.97726349165507,1.,-0.770963190030504));
#72329=CARTESIAN_POINT('Ctrl Pts',(3.96972446532832,-1.,-0.772400931772239));
#72330=CARTESIAN_POINT('Ctrl Pts',(3.96972446532832,1.,-0.772400931772239));
#72331=CARTESIAN_POINT('Ctrl Pts',(3.96218649639876,-1.,-0.773798212026683));
#72332=CARTESIAN_POINT('Ctrl Pts',(3.96218649639876,1.,-0.773798212026683));
#72333=CARTESIAN_POINT('Ctrl Pts',(3.95464885452364,-1.,-0.775154418039442));
#72334=CARTESIAN_POINT('Ctrl Pts',(3.95464885452364,1.,-0.775154418039442));
#72335=CARTESIAN_POINT('Ctrl Pts',(3.94711101619471,-1.,-0.77646896669796));
#72336=CARTESIAN_POINT('Ctrl Pts',(3.94711101619471,1.,-0.77646896669796));
#72337=CARTESIAN_POINT('Ctrl Pts',(3.93957296768098,-1.,-0.77774137056855));
#72338=CARTESIAN_POINT('Ctrl Pts',(3.93957296768098,1.,-0.77774137056855));
#72339=CARTESIAN_POINT('Ctrl Pts',(3.93203552473153,-1.,-0.778971308134786));
#72340=CARTESIAN_POINT('Ctrl Pts',(3.93203552473153,1.,-0.778971308134786));
#72341=CARTESIAN_POINT('Ctrl Pts',(3.92450058323799,-1.,-0.780158678615507));
#72342=CARTESIAN_POINT('Ctrl Pts',(3.92450058323799,1.,-0.780158678615507));
#72343=CARTESIAN_POINT('Ctrl Pts',(3.9169703605466,-1.,-0.781303428618344));
#72344=CARTESIAN_POINT('Ctrl Pts',(3.9169703605466,1.,-0.781303428618344));
#72345=CARTESIAN_POINT('Ctrl Pts',(3.90944671004536,-1.,-0.782405395622759));
#72346=CARTESIAN_POINT('Ctrl Pts',(3.90944671004536,1.,-0.782405395622759));
#72347=CARTESIAN_POINT('Ctrl Pts',(3.90193039043971,-1.,-0.783464141529083));
#72348=CARTESIAN_POINT('Ctrl Pts',(3.90193039043971,1.,-0.783464141529083));
#72349=CARTESIAN_POINT('Ctrl Pts',(3.89442039235105,-1.,-0.784478799358336));
#72350=CARTESIAN_POINT('Ctrl Pts',(3.89442039235105,1.,-0.784478799358336));
#72351=CARTESIAN_POINT('Ctrl Pts',(3.88691313167399,-1.,-0.785447890340723));
#72352=CARTESIAN_POINT('Ctrl Pts',(3.88691313167399,1.,-0.785447890340723));
#72353=CARTESIAN_POINT('Ctrl Pts',(3.87940402818186,-1.,-0.786369675812592));
#72354=CARTESIAN_POINT('Ctrl Pts',(3.87940402818186,1.,-0.786369675812592));
#72355=CARTESIAN_POINT('Ctrl Pts',(3.87188916600905,-1.,-0.787242527617981));
#72356=CARTESIAN_POINT('Ctrl Pts',(3.87188916600905,1.,-0.787242527617981));
#72357=CARTESIAN_POINT('Ctrl Pts',(3.86436702561342,-1.,-0.788065315093771));
#72358=CARTESIAN_POINT('Ctrl Pts',(3.86436702561342,1.,-0.788065315093771));
#72359=CARTESIAN_POINT('Ctrl Pts',(3.85683995872536,-1.,-0.788837734090688));
#72360=CARTESIAN_POINT('Ctrl Pts',(3.85683995872536,1.,-0.788837734090688));
#72361=CARTESIAN_POINT('Ctrl Pts',(3.8493163780891,-1.,-0.789560798155619));
#72362=CARTESIAN_POINT('Ctrl Pts',(3.8493163780891,1.,-0.789560798155619));
#72363=CARTESIAN_POINT('Ctrl Pts',(3.84180762342476,-1.,-0.790236124191289));
#72364=CARTESIAN_POINT('Ctrl Pts',(3.84180762342476,1.,-0.790236124191289));
#72365=CARTESIAN_POINT('Ctrl Pts',(3.83432392054804,-1.,-0.79086501270534));
#72366=CARTESIAN_POINT('Ctrl Pts',(3.83432392054804,1.,-0.79086501270534));
#72367=CARTESIAN_POINT('Ctrl Pts',(3.82687033899799,-1.,-0.791447528662381));
#72368=CARTESIAN_POINT('Ctrl Pts',(3.82687033899799,1.,-0.791447528662381));
#72369=CARTESIAN_POINT('Ctrl Pts',(3.81944345442237,-1.,-0.791981740718607));
#72370=CARTESIAN_POINT('Ctrl Pts',(3.81944345442237,1.,-0.791981740718607));
#72371=CARTESIAN_POINT('Ctrl Pts',(3.81202588694726,-1.,-0.792462483517568));
#72372=CARTESIAN_POINT('Ctrl Pts',(3.81202588694726,1.,-0.792462483517568));
#72373=CARTESIAN_POINT('Ctrl Pts',(3.80459229925598,-1.,-0.792882695234693));
#72374=CARTESIAN_POINT('Ctrl Pts',(3.80459229925598,1.,-0.792882695234693));
#72375=CARTESIAN_POINT('Ctrl Pts',(3.79711921389862,-1.,-0.793235612973201));
#72376=CARTESIAN_POINT('Ctrl Pts',(3.79711921389862,1.,-0.793235612973201));
#72377=CARTESIAN_POINT('Ctrl Pts',(3.78959439439222,-1.,-0.793516871680966));
#72378=CARTESIAN_POINT('Ctrl Pts',(3.78959439439222,1.,-0.793516871680966));
#72379=CARTESIAN_POINT('Ctrl Pts',(3.78202460377617,-1.,-0.79372623578134));
#72380=CARTESIAN_POINT('Ctrl Pts',(3.78202460377617,1.,-0.79372623578134));
#72381=CARTESIAN_POINT('Ctrl Pts',(3.77444863801264,-1.,-0.793870523787515));
#72382=CARTESIAN_POINT('Ctrl Pts',(3.77444863801264,1.,-0.793870523787515));
#72383=CARTESIAN_POINT('Ctrl Pts',(3.76692626931184,-1.,-0.793961083689141));
#72384=CARTESIAN_POINT('Ctrl Pts',(3.76692626931184,1.,-0.793961083689141));
#72385=CARTESIAN_POINT('Ctrl Pts',(3.75951468666325,-1.,-0.794008429135047));
#72386=CARTESIAN_POINT('Ctrl Pts',(3.75951468666325,1.,-0.794008429135047));
#72387=CARTESIAN_POINT('Ctrl Pts',(3.75224692493895,-1.,-0.794017347371441));
#72388=CARTESIAN_POINT('Ctrl Pts',(3.75224692493895,1.,-0.794017347371441));
#72389=CARTESIAN_POINT('Ctrl Pts',(3.74511357728827,-1.,-0.79398270045988));
#72390=CARTESIAN_POINT('Ctrl Pts',(3.74511357728827,1.,-0.79398270045988));
#72391=CARTESIAN_POINT('Ctrl Pts',(3.73803280541576,-1.,-0.793882700936791));
#72392=CARTESIAN_POINT('Ctrl Pts',(3.73803280541576,1.,-0.793882700936791));
#72393=CARTESIAN_POINT('Ctrl Pts',(3.7308691469564,-1.,-0.793682750269348));
#72394=CARTESIAN_POINT('Ctrl Pts',(3.7308691469564,1.,-0.793682750269348));
#72395=CARTESIAN_POINT('Ctrl Pts',(3.7234879729357,-1.,-0.793347023783871));
#72396=CARTESIAN_POINT('Ctrl Pts',(3.7234879729357,1.,-0.793347023783871));
#72397=CARTESIAN_POINT('Ctrl Pts',(3.7158024239604,-1.,-0.792848377370116));
#72398=CARTESIAN_POINT('Ctrl Pts',(3.7158024239604,1.,-0.792848377370116));
#72399=CARTESIAN_POINT('Ctrl Pts',(3.70781724021879,-1.,-0.792177688845968));
#72400=CARTESIAN_POINT('Ctrl Pts',(3.70781724021879,1.,-0.792177688845968));
#72401=CARTESIAN_POINT('Ctrl Pts',(3.69968940808982,-1.,-0.791356575696509));
#72402=CARTESIAN_POINT('Ctrl Pts',(3.69968940808982,1.,-0.791356575696509));
#72403=CARTESIAN_POINT('Ctrl Pts',(3.69172044327754,-1.,-0.79043628498958));
#72404=CARTESIAN_POINT('Ctrl Pts',(3.69172044327754,1.,-0.79043628498958));
#72405=CARTESIAN_POINT('Ctrl Pts',(3.68428439784285,-1.,-0.789483546065159));
#72406=CARTESIAN_POINT('Ctrl Pts',(3.68428439784285,1.,-0.789483546065159));
#72407=CARTESIAN_POINT('Ctrl Pts',(3.67777119516438,-1.,-0.788569566220663));
#72408=CARTESIAN_POINT('Ctrl Pts',(3.67777119516438,1.,-0.788569566220663));
#72409=CARTESIAN_POINT('Ctrl Pts',(3.672529236635,-1.,-0.787758799995427));
#72410=CARTESIAN_POINT('Ctrl Pts',(3.672529236635,1.,-0.787758799995427));
#72411=CARTESIAN_POINT('Ctrl Pts',(3.66879484800625,-1.,-0.787095252589508));
#72412=CARTESIAN_POINT('Ctrl Pts',(3.66879484800625,1.,-0.787095252589508));
#72413=CARTESIAN_POINT('Ctrl Pts',(3.66710211819938,-1.,-0.786698783541658));
#72414=CARTESIAN_POINT('Ctrl Pts',(3.66710211819938,1.,-0.786698783541658));
#72415=CARTESIAN_POINT('Ctrl Pts',(3.66657784454965,-1.,-0.786480236184947));
#72416=CARTESIAN_POINT('Ctrl Pts',(3.66657784454965,1.,-0.786480236184947));
#72417=CARTESIAN_POINT('Ctrl Pts',(3.66655932661846,-1.,-0.78636952818304));
#72418=CARTESIAN_POINT('Ctrl Pts',(3.66655932661846,1.,-0.78636952818304));
#72419=CARTESIAN_POINT('Ctrl Pts',(3.66663282329846,-1.,-0.786322922920599));
#72420=CARTESIAN_POINT('Ctrl Pts',(3.66663282329846,1.,-0.786322922920599));
#72421=CARTESIAN_POINT('',(4.13571194405636,1.,-0.73204283740062));
#72422=CARTESIAN_POINT('Ctrl Pts',(4.13571194405636,1.,-0.73204283740062));
#72423=CARTESIAN_POINT('Ctrl Pts',(4.13420383737278,1.,-0.732488575135926));
#72424=CARTESIAN_POINT('Ctrl Pts',(4.13118752796397,1.,-0.733376589325634));
#72425=CARTESIAN_POINT('Ctrl Pts',(4.12666277572794,1.,-0.734698226767513));
#72426=CARTESIAN_POINT('Ctrl Pts',(4.12062919626082,1.,-0.736439634335347));
#72427=CARTESIAN_POINT('Ctrl Pts',(4.11308626953795,1.,-0.738581708229119));
#72428=CARTESIAN_POINT('Ctrl Pts',(4.1055424175856,1.,-0.740688998555152));
#72429=CARTESIAN_POINT('Ctrl Pts',(4.09799769702712,1.,-0.742761369690018));
#72430=CARTESIAN_POINT('Ctrl Pts',(4.09045220253011,1.,-0.744798649705514));
#72431=CARTESIAN_POINT('Ctrl Pts',(4.08290608094789,1.,-0.746800631490822));
#72432=CARTESIAN_POINT('Ctrl Pts',(4.07535951055363,1.,-0.748767076679177));
#72433=CARTESIAN_POINT('Ctrl Pts',(4.06781267241886,1.,-0.750697720483176));
#72434=CARTESIAN_POINT('Ctrl Pts',(4.06026572221399,1.,-0.752592276482869));
#72435=CARTESIAN_POINT('Ctrl Pts',(4.05271876688106,1.,-0.754450441816412));
#72436=CARTESIAN_POINT('Ctrl Pts',(4.04517182654344,1.,-0.756271902370187));
#72437=CARTESIAN_POINT('Ctrl Pts',(4.03762485803468,1.,-0.758056338885554));
#72438=CARTESIAN_POINT('Ctrl Pts',(4.0300778195465,1.,-0.759803433244166));
#72439=CARTESIAN_POINT('Ctrl Pts',(4.02253072741347,1.,-0.761512875859942));
#72440=CARTESIAN_POINT('Ctrl Pts',(4.01498370680434,1.,-0.763184371182827));
#72441=CARTESIAN_POINT('Ctrl Pts',(4.00743706791366,1.,-0.764817648784947));
#72442=CARTESIAN_POINT('Ctrl Pts',(3.99989129179464,1.,-0.766412457135786));
#72443=CARTESIAN_POINT('Ctrl Pts',(3.99234687880892,1.,-0.767968531377708));
#72444=CARTESIAN_POINT('Ctrl Pts',(3.98480422348403,1.,-0.76948556624546));
#72445=CARTESIAN_POINT('Ctrl Pts',(3.97726349165507,1.,-0.770963190030504));
#72446=CARTESIAN_POINT('Ctrl Pts',(3.96972446532832,1.,-0.772400931772239));
#72447=CARTESIAN_POINT('Ctrl Pts',(3.96218649639876,1.,-0.773798212026683));
#72448=CARTESIAN_POINT('Ctrl Pts',(3.95464885452364,1.,-0.775154418039442));
#72449=CARTESIAN_POINT('Ctrl Pts',(3.94711101619471,1.,-0.77646896669796));
#72450=CARTESIAN_POINT('Ctrl Pts',(3.93957296768098,1.,-0.77774137056855));
#72451=CARTESIAN_POINT('Ctrl Pts',(3.93203552473153,1.,-0.778971308134786));
#72452=CARTESIAN_POINT('Ctrl Pts',(3.92450058323799,1.,-0.780158678615507));
#72453=CARTESIAN_POINT('Ctrl Pts',(3.9169703605466,1.,-0.781303428618344));
#72454=CARTESIAN_POINT('Ctrl Pts',(3.90944671004536,1.,-0.782405395622759));
#72455=CARTESIAN_POINT('Ctrl Pts',(3.90193039043971,1.,-0.783464141529083));
#72456=CARTESIAN_POINT('Ctrl Pts',(3.89442039235105,1.,-0.784478799358336));
#72457=CARTESIAN_POINT('Ctrl Pts',(3.88691313167399,1.,-0.785447890340723));
#72458=CARTESIAN_POINT('Ctrl Pts',(3.87940402818186,1.,-0.786369675812592));
#72459=CARTESIAN_POINT('Ctrl Pts',(3.87188916600905,1.,-0.787242527617981));
#72460=CARTESIAN_POINT('Ctrl Pts',(3.86436702561342,1.,-0.788065315093771));
#72461=CARTESIAN_POINT('Ctrl Pts',(3.85683995872536,1.,-0.788837734090688));
#72462=CARTESIAN_POINT('Ctrl Pts',(3.8493163780891,1.,-0.789560798155619));
#72463=CARTESIAN_POINT('Ctrl Pts',(3.84180762342476,1.,-0.790236124191289));
#72464=CARTESIAN_POINT('Ctrl Pts',(3.83432392054804,1.,-0.79086501270534));
#72465=CARTESIAN_POINT('Ctrl Pts',(3.82687033899799,1.,-0.791447528662381));
#72466=CARTESIAN_POINT('Ctrl Pts',(3.81944345442237,1.,-0.791981740718607));
#72467=CARTESIAN_POINT('Ctrl Pts',(3.81202588694726,1.,-0.792462483517568));
#72468=CARTESIAN_POINT('Ctrl Pts',(3.80459229925598,1.,-0.792882695234693));
#72469=CARTESIAN_POINT('Ctrl Pts',(3.79711921389862,1.,-0.793235612973201));
#72470=CARTESIAN_POINT('Ctrl Pts',(3.78959439439222,1.,-0.793516871680966));
#72471=CARTESIAN_POINT('Ctrl Pts',(3.78202460377617,1.,-0.79372623578134));
#72472=CARTESIAN_POINT('Ctrl Pts',(3.77444863801264,1.,-0.793870523787515));
#72473=CARTESIAN_POINT('Ctrl Pts',(3.76692626931184,1.,-0.793961083689141));
#72474=CARTESIAN_POINT('Ctrl Pts',(3.75951468666325,1.,-0.794008429135047));
#72475=CARTESIAN_POINT('Ctrl Pts',(3.75224692493895,1.,-0.794017347371441));
#72476=CARTESIAN_POINT('Ctrl Pts',(3.74511357728827,1.,-0.79398270045988));
#72477=CARTESIAN_POINT('Ctrl Pts',(3.73803280541576,1.,-0.793882700936791));
#72478=CARTESIAN_POINT('Ctrl Pts',(3.7308691469564,1.,-0.793682750269348));
#72479=CARTESIAN_POINT('Ctrl Pts',(3.7234879729357,1.,-0.793347023783871));
#72480=CARTESIAN_POINT('Ctrl Pts',(3.7158024239604,1.,-0.792848377370116));
#72481=CARTESIAN_POINT('Ctrl Pts',(3.70781724021879,1.,-0.792177688845968));
#72482=CARTESIAN_POINT('Ctrl Pts',(3.69968940808982,1.,-0.791356575696509));
#72483=CARTESIAN_POINT('Ctrl Pts',(3.69172044327754,1.,-0.79043628498958));
#72484=CARTESIAN_POINT('Ctrl Pts',(3.68428439784285,1.,-0.789483546065159));
#72485=CARTESIAN_POINT('Ctrl Pts',(3.67777119516438,1.,-0.788569566220663));
#72486=CARTESIAN_POINT('Ctrl Pts',(3.672529236635,1.,-0.787758799995427));
#72487=CARTESIAN_POINT('Ctrl Pts',(3.66907505398769,1.,-0.787145041181589));
#72488=CARTESIAN_POINT('Ctrl Pts',(3.66743103898844,1.,-0.7867743371985));
#72489=CARTESIAN_POINT('Ctrl Pts',(3.66680946938396,1.,-0.78656591955989));
#72490=CARTESIAN_POINT('Ctrl Pts',(3.66664310415236,1.,-0.786459983896781));
#72491=CARTESIAN_POINT('Ctrl Pts',(3.66661143271648,1.,-0.786422660833743));
#72492=CARTESIAN_POINT('',(4.13571194405636,0.,-0.73204283740062));
#72493=CARTESIAN_POINT('Origin',(4.15950947128175,0.,-0.581791163835815));
#72494=CARTESIAN_POINT('',(4.15950947128175,1.,-0.581791163835815));
#72495=CARTESIAN_POINT('',(4.13571194405636,1.,-0.73204283740062));
#72496=CARTESIAN_POINT('',(4.15950947128175,0.,-0.581791163835815));
#72497=CARTESIAN_POINT('Ctrl Pts',(3.73016218570874,-1.,-0.385214314776329));
#72498=CARTESIAN_POINT('Ctrl Pts',(3.73016218570874,1.,-0.385214314776329));
#72499=CARTESIAN_POINT('Ctrl Pts',(3.73010668803185,-1.,-0.385147278814804));
#72500=CARTESIAN_POINT('Ctrl Pts',(3.73010668803185,1.,-0.385147278814804));
#72501=CARTESIAN_POINT('Ctrl Pts',(3.73015851028729,-1.,-0.385047711603887));
#72502=CARTESIAN_POINT('Ctrl Pts',(3.73015851028729,1.,-0.385047711603887));
#72503=CARTESIAN_POINT('Ctrl Pts',(3.73072465900727,-1.,-0.385001870183842));
#72504=CARTESIAN_POINT('Ctrl Pts',(3.73072465900727,1.,-0.385001870183842));
#72505=CARTESIAN_POINT('Ctrl Pts',(3.73245705639337,-1.,-0.385147887989515));
#72506=CARTESIAN_POINT('Ctrl Pts',(3.73245705639337,1.,-0.385147887989515));
#72507=CARTESIAN_POINT('Ctrl Pts',(3.73621371845475,-1.,-0.385670806454744));
#72508=CARTESIAN_POINT('Ctrl Pts',(3.73621371845475,1.,-0.385670806454744));
#72509=CARTESIAN_POINT('Ctrl Pts',(3.74144965781088,-1.,-0.386519576222036));
#72510=CARTESIAN_POINT('Ctrl Pts',(3.74144965781088,1.,-0.386519576222036));
#72511=CARTESIAN_POINT('Ctrl Pts',(3.74792651696269,-1.,-0.387663020050396));
#72512=CARTESIAN_POINT('Ctrl Pts',(3.74792651696269,1.,-0.387663020050396));
#72513=CARTESIAN_POINT('Ctrl Pts',(3.75529302894757,-1.,-0.389054775898251));
#72514=CARTESIAN_POINT('Ctrl Pts',(3.75529302894757,1.,-0.389054775898251));
#72515=CARTESIAN_POINT('Ctrl Pts',(3.76315635032993,-1.,-0.390642072979259));
#72516=CARTESIAN_POINT('Ctrl Pts',(3.76315635032993,1.,-0.390642072979259));
#72517=CARTESIAN_POINT('Ctrl Pts',(3.77114011595892,-1.,-0.392372786223347));
#72518=CARTESIAN_POINT('Ctrl Pts',(3.77114011595892,1.,-0.392372786223347));
#72519=CARTESIAN_POINT('Ctrl Pts',(3.77894173114368,-1.,-0.394202481011595));
#72520=CARTESIAN_POINT('Ctrl Pts',(3.77894173114368,1.,-0.394202481011595));
#72521=CARTESIAN_POINT('Ctrl Pts',(3.78640521279479,-1.,-0.396103205335029));
#72522=CARTESIAN_POINT('Ctrl Pts',(3.78640521279479,1.,-0.396103205335029));
#72523=CARTESIAN_POINT('Ctrl Pts',(3.79352887163457,-1.,-0.398064818684159));
#72524=CARTESIAN_POINT('Ctrl Pts',(3.79352887163457,1.,-0.398064818684159));
#72525=CARTESIAN_POINT('Ctrl Pts',(3.80040370384659,-1.,-0.400088346504727));
#72526=CARTESIAN_POINT('Ctrl Pts',(3.80040370384659,1.,-0.400088346504727));
#72527=CARTESIAN_POINT('Ctrl Pts',(3.80716881962763,-1.,-0.402181320148475));
#72528=CARTESIAN_POINT('Ctrl Pts',(3.80716881962763,1.,-0.402181320148475));
#72529=CARTESIAN_POINT('Ctrl Pts',(3.81396374287762,-1.,-0.404352694628237));
#72530=CARTESIAN_POINT('Ctrl Pts',(3.81396374287762,1.,-0.404352694628237));
#72531=CARTESIAN_POINT('Ctrl Pts',(3.82087303913741,-1.,-0.406607038258907));
#72532=CARTESIAN_POINT('Ctrl Pts',(3.82087303913741,1.,-0.406607038258907));
#72533=CARTESIAN_POINT('Ctrl Pts',(3.82790724256397,-1.,-0.408942371447377));
#72534=CARTESIAN_POINT('Ctrl Pts',(3.82790724256397,1.,-0.408942371447377));
#72535=CARTESIAN_POINT('Ctrl Pts',(3.83503345578645,-1.,-0.41135303879846));
#72536=CARTESIAN_POINT('Ctrl Pts',(3.83503345578645,1.,-0.41135303879846));
#72537=CARTESIAN_POINT('Ctrl Pts',(3.84219403994742,-1.,-0.413831367016727));
#72538=CARTESIAN_POINT('Ctrl Pts',(3.84219403994742,1.,-0.413831367016727));
#72539=CARTESIAN_POINT('Ctrl Pts',(3.8493286415751,-1.,-0.41636967805292));
#72540=CARTESIAN_POINT('Ctrl Pts',(3.8493286415751,1.,-0.41636967805292));
#72541=CARTESIAN_POINT('Ctrl Pts',(3.85639825648031,-1.,-0.41896246808681));
#72542=CARTESIAN_POINT('Ctrl Pts',(3.85639825648031,1.,-0.41896246808681));
#72543=CARTESIAN_POINT('Ctrl Pts',(3.86339652542749,-1.,-0.421607423177576));
#72544=CARTESIAN_POINT('Ctrl Pts',(3.86339652542749,1.,-0.421607423177576));
#72545=CARTESIAN_POINT('Ctrl Pts',(3.87033643487882,-1.,-0.424304173195143));
#72546=CARTESIAN_POINT('Ctrl Pts',(3.87033643487882,1.,-0.424304173195143));
#72547=CARTESIAN_POINT('Ctrl Pts',(3.87724240306609,-1.,-0.427053541173469));
#72548=CARTESIAN_POINT('Ctrl Pts',(3.87724240306609,1.,-0.427053541173469));
#72549=CARTESIAN_POINT('Ctrl Pts',(3.88414070943334,-1.,-0.429856640579734));
#72550=CARTESIAN_POINT('Ctrl Pts',(3.88414070943334,1.,-0.429856640579734));
#72551=CARTESIAN_POINT('Ctrl Pts',(3.89104947940592,-1.,-0.43271392954444));
#72552=CARTESIAN_POINT('Ctrl Pts',(3.89104947940592,1.,-0.43271392954444));
#72553=CARTESIAN_POINT('Ctrl Pts',(3.8979725665544,-1.,-0.435624629433506));
#72554=CARTESIAN_POINT('Ctrl Pts',(3.8979725665544,1.,-0.435624629433506));
#72555=CARTESIAN_POINT('Ctrl Pts',(3.90490512938546,-1.,-0.438587235458234));
#72556=CARTESIAN_POINT('Ctrl Pts',(3.90490512938546,1.,-0.438587235458234));
#72557=CARTESIAN_POINT('Ctrl Pts',(3.91183704069146,-1.,-0.441599824524048));
#72558=CARTESIAN_POINT('Ctrl Pts',(3.91183704069146,1.,-0.441599824524048));
#72559=CARTESIAN_POINT('Ctrl Pts',(3.91875701610721,-1.,-0.444660430230593));
#72560=CARTESIAN_POINT('Ctrl Pts',(3.91875701610721,1.,-0.444660430230593));
#72561=CARTESIAN_POINT('Ctrl Pts',(3.92565674143424,-1.,-0.447767416837297));
#72562=CARTESIAN_POINT('Ctrl Pts',(3.92565674143424,1.,-0.447767416837297));
#72563=CARTESIAN_POINT('Ctrl Pts',(3.93253407403128,-1.,-0.450919768356347));
#72564=CARTESIAN_POINT('Ctrl Pts',(3.93253407403128,1.,-0.450919768356347));
#72565=CARTESIAN_POINT('Ctrl Pts',(3.93939080846298,-1.,-0.454116879027576));
#72566=CARTESIAN_POINT('Ctrl Pts',(3.93939080846298,1.,-0.454116879027576));
#72567=CARTESIAN_POINT('Ctrl Pts',(3.94623117206675,-1.,-0.457358410451674));
#72568=CARTESIAN_POINT('Ctrl Pts',(3.94623117206675,1.,-0.457358410451674));
#72569=CARTESIAN_POINT('Ctrl Pts',(3.95306005817363,-1.,-0.460644124429119));
#72570=CARTESIAN_POINT('Ctrl Pts',(3.95306005817363,1.,-0.460644124429119));
#72571=CARTESIAN_POINT('Ctrl Pts',(3.95988133243543,-1.,-0.463973722115745));
#72572=CARTESIAN_POINT('Ctrl Pts',(3.95988133243543,1.,-0.463973722115745));
#72573=CARTESIAN_POINT('Ctrl Pts',(3.96669622273946,-1.,-0.467346690880672));
#72574=CARTESIAN_POINT('Ctrl Pts',(3.96669622273946,1.,-0.467346690880672));
#72575=CARTESIAN_POINT('Ctrl Pts',(3.97350414289415,-1.,-0.470762379613478));
#72576=CARTESIAN_POINT('Ctrl Pts',(3.97350414289415,1.,-0.470762379613478));
#72577=CARTESIAN_POINT('Ctrl Pts',(3.9803033804443,-1.,-0.474220061019542));
#72578=CARTESIAN_POINT('Ctrl Pts',(3.9803033804443,1.,-0.474220061019542));
#72579=CARTESIAN_POINT('Ctrl Pts',(3.98709184306743,-1.,-0.477718999122033));
#72580=CARTESIAN_POINT('Ctrl Pts',(3.98709184306743,1.,-0.477718999122033));
#72581=CARTESIAN_POINT('Ctrl Pts',(3.99386775880655,-1.,-0.481258512209638));
#72582=CARTESIAN_POINT('Ctrl Pts',(3.99386775880655,1.,-0.481258512209638));
#72583=CARTESIAN_POINT('Ctrl Pts',(4.00063045119234,-1.,-0.484838042421754));
#72584=CARTESIAN_POINT('Ctrl Pts',(4.00063045119234,1.,-0.484838042421754));
#72585=CARTESIAN_POINT('Ctrl Pts',(4.0073800839092,-1.,-0.488457130424531));
#72586=CARTESIAN_POINT('Ctrl Pts',(4.0073800839092,1.,-0.488457130424531));
#72587=CARTESIAN_POINT('Ctrl Pts',(4.01411733503486,-1.,-0.492115383417931));
#72588=CARTESIAN_POINT('Ctrl Pts',(4.01411733503486,1.,-0.492115383417931));
#72589=CARTESIAN_POINT('Ctrl Pts',(4.02084308851813,-1.,-0.495812444326223));
#72590=CARTESIAN_POINT('Ctrl Pts',(4.02084308851813,1.,-0.495812444326223));
#72591=CARTESIAN_POINT('Ctrl Pts',(4.0275581398015,-1.,-0.49954796234089));
#72592=CARTESIAN_POINT('Ctrl Pts',(4.0275581398015,1.,-0.49954796234089));
#72593=CARTESIAN_POINT('Ctrl Pts',(4.0342628417439,-1.,-0.503321556915514));
#72594=CARTESIAN_POINT('Ctrl Pts',(4.0342628417439,1.,-0.503321556915514));
#72595=CARTESIAN_POINT('Ctrl Pts',(4.04095715149074,-1.,-0.507132823288362));
#72596=CARTESIAN_POINT('Ctrl Pts',(4.04095715149074,1.,-0.507132823288362));
#72597=CARTESIAN_POINT('Ctrl Pts',(4.04764078815591,-1.,-0.510981349219174));
#72598=CARTESIAN_POINT('Ctrl Pts',(4.04764078815591,1.,-0.510981349219174));
#72599=CARTESIAN_POINT('Ctrl Pts',(4.05431335771261,-1.,-0.514866728193104));
#72600=CARTESIAN_POINT('Ctrl Pts',(4.05431335771261,1.,-0.514866728193104));
#72601=CARTESIAN_POINT('Ctrl Pts',(4.06097448037934,-1.,-0.51878857233681));
#72602=CARTESIAN_POINT('Ctrl Pts',(4.06097448037934,1.,-0.51878857233681));
#72603=CARTESIAN_POINT('Ctrl Pts',(4.06762394471075,-1.,-0.522746528602768));
#72604=CARTESIAN_POINT('Ctrl Pts',(4.06762394471075,1.,-0.522746528602768));
#72605=CARTESIAN_POINT('Ctrl Pts',(4.07426172299496,-1.,-0.526740277227));
#72606=CARTESIAN_POINT('Ctrl Pts',(4.07426172299496,1.,-0.526740277227));
#72607=CARTESIAN_POINT('Ctrl Pts',(4.08088789536488,-1.,-0.530769518728076));
#72608=CARTESIAN_POINT('Ctrl Pts',(4.08088789536488,1.,-0.530769518728076));
#72609=CARTESIAN_POINT('Ctrl Pts',(4.08750259988693,-1.,-0.534833963477));
#72610=CARTESIAN_POINT('Ctrl Pts',(4.08750259988693,1.,-0.534833963477));
#72611=CARTESIAN_POINT('Ctrl Pts',(4.09410597627116,-1.,-0.538933321179921));
#72612=CARTESIAN_POINT('Ctrl Pts',(4.09410597627116,1.,-0.538933321179921));
#72613=CARTESIAN_POINT('Ctrl Pts',(4.10069810244473,-1.,-0.543067286878457));
#72614=CARTESIAN_POINT('Ctrl Pts',(4.10069810244473,1.,-0.543067286878457));
#72615=CARTESIAN_POINT('Ctrl Pts',(4.1072789702877,-1.,-0.54723553948676));
#72616=CARTESIAN_POINT('Ctrl Pts',(4.1072789702877,1.,-0.54723553948676));
#72617=CARTESIAN_POINT('Ctrl Pts',(4.11384852025578,-1.,-0.551437758498247));
#72618=CARTESIAN_POINT('Ctrl Pts',(4.11384852025578,1.,-0.551437758498247));
#72619=CARTESIAN_POINT('Ctrl Pts',(4.1204066619623,-1.,-0.555673636130778));
#72620=CARTESIAN_POINT('Ctrl Pts',(4.1204066619623,1.,-0.555673636130778));
#72621=CARTESIAN_POINT('Ctrl Pts',(4.12695329951859,-1.,-0.559942890594628));
#72622=CARTESIAN_POINT('Ctrl Pts',(4.12695329951859,1.,-0.559942890594628));
#72623=CARTESIAN_POINT('Ctrl Pts',(4.13348835726086,-1.,-0.564245279535706));
#72624=CARTESIAN_POINT('Ctrl Pts',(4.13348835726086,1.,-0.564245279535706));
#72625=CARTESIAN_POINT('Ctrl Pts',(4.14001179828669,-1.,-0.568580610187116));
#72626=CARTESIAN_POINT('Ctrl Pts',(4.14001179828669,1.,-0.568580610187116));
#72627=CARTESIAN_POINT('Ctrl Pts',(4.14652361065787,-1.,-0.572948736066277));
#72628=CARTESIAN_POINT('Ctrl Pts',(4.14652361065787,1.,-0.572948736066277));
#72629=CARTESIAN_POINT('Ctrl Pts',(4.1517237611974,-1.,-0.576469391673917));
#72630=CARTESIAN_POINT('Ctrl Pts',(4.1517237611974,1.,-0.576469391673917));
#72631=CARTESIAN_POINT('Ctrl Pts',(4.15561864787379,-1.,-0.579124568912544));
#72632=CARTESIAN_POINT('Ctrl Pts',(4.15561864787379,1.,-0.579124568912544));
#72633=CARTESIAN_POINT('Ctrl Pts',(4.15821291712391,-1.,-0.580901211462913));
#72634=CARTESIAN_POINT('Ctrl Pts',(4.15821291712391,1.,-0.580901211462913));
#72635=CARTESIAN_POINT('Ctrl Pts',(4.15950947128175,-1.,-0.581791163835815));
#72636=CARTESIAN_POINT('Ctrl Pts',(4.15950947128175,1.,-0.581791163835815));
#72637=CARTESIAN_POINT('',(3.73017266276632,1.,-0.385112848332548));
#72638=CARTESIAN_POINT('Ctrl Pts',(3.73017266276632,-1.,-0.385112848332549));
#72639=CARTESIAN_POINT('Ctrl Pts',(3.73017266276632,-0.666666666666667,
-0.385112848332549));
#72640=CARTESIAN_POINT('Ctrl Pts',(3.73017266276632,-0.333333333333333,
-0.385112848332549));
#72641=CARTESIAN_POINT('Ctrl Pts',(3.73017266276632,0.333333333333333,-0.385112848332549));
#72642=CARTESIAN_POINT('Ctrl Pts',(3.73017266276632,0.666666666666667,-0.38511284833255));
#72643=CARTESIAN_POINT('Ctrl Pts',(3.73017266276632,1.,-0.38511284833255));
#72644=CARTESIAN_POINT('Ctrl Pts',(3.73017266276632,1.,-0.385112848332549));
#72645=CARTESIAN_POINT('Ctrl Pts',(3.73021431755218,1.,-0.385087139001609));
#72646=CARTESIAN_POINT('Ctrl Pts',(3.73040527620929,1.,-0.385037797882046));
#72647=CARTESIAN_POINT('Ctrl Pts',(3.731060828624,1.,-0.385031656499142));
#72648=CARTESIAN_POINT('Ctrl Pts',(3.73273893363318,1.,-0.385187124633965));
#72649=CARTESIAN_POINT('Ctrl Pts',(3.73621371845475,1.,-0.385670806454744));
#72650=CARTESIAN_POINT('Ctrl Pts',(3.74144965781088,1.,-0.386519576222036));
#72651=CARTESIAN_POINT('Ctrl Pts',(3.74792651696269,1.,-0.387663020050396));
#72652=CARTESIAN_POINT('Ctrl Pts',(3.75529302894757,1.,-0.389054775898251));
#72653=CARTESIAN_POINT('Ctrl Pts',(3.76315635032993,1.,-0.390642072979259));
#72654=CARTESIAN_POINT('Ctrl Pts',(3.77114011595892,1.,-0.392372786223347));
#72655=CARTESIAN_POINT('Ctrl Pts',(3.77894173114368,1.,-0.394202481011595));
#72656=CARTESIAN_POINT('Ctrl Pts',(3.78640521279479,1.,-0.396103205335029));
#72657=CARTESIAN_POINT('Ctrl Pts',(3.79352887163457,1.,-0.398064818684159));
#72658=CARTESIAN_POINT('Ctrl Pts',(3.80040370384659,1.,-0.400088346504727));
#72659=CARTESIAN_POINT('Ctrl Pts',(3.80716881962763,1.,-0.402181320148475));
#72660=CARTESIAN_POINT('Ctrl Pts',(3.81396374287762,1.,-0.404352694628237));
#72661=CARTESIAN_POINT('Ctrl Pts',(3.82087303913741,1.,-0.406607038258907));
#72662=CARTESIAN_POINT('Ctrl Pts',(3.82790724256397,1.,-0.408942371447377));
#72663=CARTESIAN_POINT('Ctrl Pts',(3.83503345578645,1.,-0.41135303879846));
#72664=CARTESIAN_POINT('Ctrl Pts',(3.84219403994742,1.,-0.413831367016727));
#72665=CARTESIAN_POINT('Ctrl Pts',(3.8493286415751,1.,-0.41636967805292));
#72666=CARTESIAN_POINT('Ctrl Pts',(3.85639825648031,1.,-0.41896246808681));
#72667=CARTESIAN_POINT('Ctrl Pts',(3.86339652542749,1.,-0.421607423177576));
#72668=CARTESIAN_POINT('Ctrl Pts',(3.87033643487882,1.,-0.424304173195143));
#72669=CARTESIAN_POINT('Ctrl Pts',(3.87724240306609,1.,-0.427053541173469));
#72670=CARTESIAN_POINT('Ctrl Pts',(3.88414070943334,1.,-0.429856640579734));
#72671=CARTESIAN_POINT('Ctrl Pts',(3.89104947940592,1.,-0.43271392954444));
#72672=CARTESIAN_POINT('Ctrl Pts',(3.8979725665544,1.,-0.435624629433506));
#72673=CARTESIAN_POINT('Ctrl Pts',(3.90490512938546,1.,-0.438587235458234));
#72674=CARTESIAN_POINT('Ctrl Pts',(3.91183704069146,1.,-0.441599824524048));
#72675=CARTESIAN_POINT('Ctrl Pts',(3.91875701610721,1.,-0.444660430230593));
#72676=CARTESIAN_POINT('Ctrl Pts',(3.92565674143424,1.,-0.447767416837297));
#72677=CARTESIAN_POINT('Ctrl Pts',(3.93253407403128,1.,-0.450919768356347));
#72678=CARTESIAN_POINT('Ctrl Pts',(3.93939080846298,1.,-0.454116879027576));
#72679=CARTESIAN_POINT('Ctrl Pts',(3.94623117206675,1.,-0.457358410451674));
#72680=CARTESIAN_POINT('Ctrl Pts',(3.95306005817363,1.,-0.460644124429119));
#72681=CARTESIAN_POINT('Ctrl Pts',(3.95988133243543,1.,-0.463973722115745));
#72682=CARTESIAN_POINT('Ctrl Pts',(3.96669622273946,1.,-0.467346690880672));
#72683=CARTESIAN_POINT('Ctrl Pts',(3.97350414289415,1.,-0.470762379613478));
#72684=CARTESIAN_POINT('Ctrl Pts',(3.9803033804443,1.,-0.474220061019542));
#72685=CARTESIAN_POINT('Ctrl Pts',(3.98709184306743,1.,-0.477718999122033));
#72686=CARTESIAN_POINT('Ctrl Pts',(3.99386775880655,1.,-0.481258512209638));
#72687=CARTESIAN_POINT('Ctrl Pts',(4.00063045119234,1.,-0.484838042421754));
#72688=CARTESIAN_POINT('Ctrl Pts',(4.0073800839092,1.,-0.488457130424531));
#72689=CARTESIAN_POINT('Ctrl Pts',(4.01411733503486,1.,-0.492115383417931));
#72690=CARTESIAN_POINT('Ctrl Pts',(4.02084308851813,1.,-0.495812444326223));
#72691=CARTESIAN_POINT('Ctrl Pts',(4.0275581398015,1.,-0.49954796234089));
#72692=CARTESIAN_POINT('Ctrl Pts',(4.0342628417439,1.,-0.503321556915514));
#72693=CARTESIAN_POINT('Ctrl Pts',(4.04095715149074,1.,-0.507132823288362));
#72694=CARTESIAN_POINT('Ctrl Pts',(4.04764078815591,1.,-0.510981349219174));
#72695=CARTESIAN_POINT('Ctrl Pts',(4.05431335771261,1.,-0.514866728193104));
#72696=CARTESIAN_POINT('Ctrl Pts',(4.06097448037934,1.,-0.51878857233681));
#72697=CARTESIAN_POINT('Ctrl Pts',(4.06762394471075,1.,-0.522746528602768));
#72698=CARTESIAN_POINT('Ctrl Pts',(4.07426172299496,1.,-0.526740277227));
#72699=CARTESIAN_POINT('Ctrl Pts',(4.08088789536488,1.,-0.530769518728076));
#72700=CARTESIAN_POINT('Ctrl Pts',(4.08750259988693,1.,-0.534833963477));
#72701=CARTESIAN_POINT('Ctrl Pts',(4.09410597627116,1.,-0.538933321179921));
#72702=CARTESIAN_POINT('Ctrl Pts',(4.10069810244473,1.,-0.543067286878457));
#72703=CARTESIAN_POINT('Ctrl Pts',(4.1072789702877,1.,-0.54723553948676));
#72704=CARTESIAN_POINT('Ctrl Pts',(4.11384852025578,1.,-0.551437758498247));
#72705=CARTESIAN_POINT('Ctrl Pts',(4.1204066619623,1.,-0.555673636130778));
#72706=CARTESIAN_POINT('Ctrl Pts',(4.12695329951859,1.,-0.559942890594628));
#72707=CARTESIAN_POINT('Ctrl Pts',(4.13348835726086,1.,-0.564245279535706));
#72708=CARTESIAN_POINT('Ctrl Pts',(4.14001179828669,1.,-0.568580610187116));
#72709=CARTESIAN_POINT('Ctrl Pts',(4.14652361065787,1.,-0.572948736066277));
#72710=CARTESIAN_POINT('Ctrl Pts',(4.1517237611974,1.,-0.576469391673917));
#72711=CARTESIAN_POINT('Ctrl Pts',(4.15561864787379,1.,-0.579124568912544));
#72712=CARTESIAN_POINT('Ctrl Pts',(4.15821291712391,1.,-0.580901211462913));
#72713=CARTESIAN_POINT('Ctrl Pts',(4.15950947128175,1.,-0.581791163835815));
#72714=CARTESIAN_POINT('Origin',(0.,0.,0.));
#72715=CARTESIAN_POINT('',(3.74449296982994,1.,-0.203156094897896));
#72716=CARTESIAN_POINT('Origin',(0.,1.,0.));
#72717=CARTESIAN_POINT('Ctrl Pts',(3.74449296982994,1.,-0.203156094897896));
#72718=CARTESIAN_POINT('Ctrl Pts',(3.74449296982994,0.666666666666667,-0.203156094897896));
#72719=CARTESIAN_POINT('Ctrl Pts',(3.74449296982994,0.333333333333333,-0.203156094897896));
#72720=CARTESIAN_POINT('Ctrl Pts',(3.74449296982994,-0.333333333333333,
-0.203156094897896));
#72721=CARTESIAN_POINT('Ctrl Pts',(3.74449296982994,-0.666666666666667,
-0.203156094897895));
#72722=CARTESIAN_POINT('Ctrl Pts',(3.74449296982994,-1.,-0.203156094897895));
#72723=CARTESIAN_POINT('Ctrl Pts',(3.74449849461127,-1.,0.20305423869972));
#72724=CARTESIAN_POINT('Ctrl Pts',(3.74449849461127,1.,0.20305423869972));
#72725=CARTESIAN_POINT('Ctrl Pts',(3.7444331934681,-1.,0.203111767587923));
#72726=CARTESIAN_POINT('Ctrl Pts',(3.7444331934681,1.,0.203111767587923));
#72727=CARTESIAN_POINT('Ctrl Pts',(3.7444688019622,-1.,0.203218215748058));
#72728=CARTESIAN_POINT('Ctrl Pts',(3.7444688019622,1.,0.203218215748058));
#72729=CARTESIAN_POINT('Ctrl Pts',(3.74502080927395,-1.,0.203352057956297));
#72730=CARTESIAN_POINT('Ctrl Pts',(3.74502080927395,1.,0.203352057956297));
#72731=CARTESIAN_POINT('Ctrl Pts',(3.7467547201908,-1.,0.203478844530446));
#72732=CARTESIAN_POINT('Ctrl Pts',(3.7467547201908,1.,0.203478844530446));
#72733=CARTESIAN_POINT('Ctrl Pts',(3.75054693397875,-1.,0.203550035479166));
#72734=CARTESIAN_POINT('Ctrl Pts',(3.75054693397875,1.,0.203550035479166));
#72735=CARTESIAN_POINT('Ctrl Pts',(3.75585118707734,-1.,0.203530796848321));
#72736=CARTESIAN_POINT('Ctrl Pts',(3.75585118707734,1.,0.203530796848321));
#72737=CARTESIAN_POINT('Ctrl Pts',(3.76242717936885,-1.,0.203414634707478));
#72738=CARTESIAN_POINT('Ctrl Pts',(3.76242717936885,1.,0.203414634707478));
#72739=CARTESIAN_POINT('Ctrl Pts',(3.7699207159487,-1.,0.203192390045164));
#72740=CARTESIAN_POINT('Ctrl Pts',(3.7699207159487,1.,0.203192390045164));
#72741=CARTESIAN_POINT('Ctrl Pts',(3.77793553476614,-1.,0.20285472969908));
#72742=CARTESIAN_POINT('Ctrl Pts',(3.77793553476614,1.,0.20285472969908));
#72743=CARTESIAN_POINT('Ctrl Pts',(3.78609175019242,-1.,0.20239426051216));
#72744=CARTESIAN_POINT('Ctrl Pts',(3.78609175019242,1.,0.20239426051216));
#72745=CARTESIAN_POINT('Ctrl Pts',(3.7940835418736,-1.,0.201807533800837));
#72746=CARTESIAN_POINT('Ctrl Pts',(3.7940835418736,1.,0.201807533800837));
#72747=CARTESIAN_POINT('Ctrl Pts',(3.80175247447337,-1.,0.201097756307325));
#72748=CARTESIAN_POINT('Ctrl Pts',(3.80175247447337,1.,0.201097756307325));
#72749=CARTESIAN_POINT('Ctrl Pts',(3.80909529318669,-1.,0.200274679433364));
#72750=CARTESIAN_POINT('Ctrl Pts',(3.80909529318669,1.,0.200274679433364));
#72751=CARTESIAN_POINT('Ctrl Pts',(3.81620203429815,-1.,0.199351525297447));
#72752=CARTESIAN_POINT('Ctrl Pts',(3.81620203429815,1.,0.199351525297447));
#72753=CARTESIAN_POINT('Ctrl Pts',(3.82321127349016,-1.,0.198342616900486));
#72754=CARTESIAN_POINT('Ctrl Pts',(3.82321127349016,1.,0.198342616900486));
#72755=CARTESIAN_POINT('Ctrl Pts',(3.83026221776456,-1.,0.197260935827361));
#72756=CARTESIAN_POINT('Ctrl Pts',(3.83026221776456,1.,0.197260935827361));
#72757=CARTESIAN_POINT('Ctrl Pts',(3.83743910616195,-1.,0.196115198971858));
#72758=CARTESIAN_POINT('Ctrl Pts',(3.83743910616195,1.,0.196115198971858));
#72759=CARTESIAN_POINT('Ctrl Pts',(3.84475203346977,-1.,0.19490900946022));
#72760=CARTESIAN_POINT('Ctrl Pts',(3.84475203346977,1.,0.19490900946022));
#72761=CARTESIAN_POINT('Ctrl Pts',(3.85216762263966,-1.,0.193642806777722));
#72762=CARTESIAN_POINT('Ctrl Pts',(3.85216762263966,1.,0.193642806777722));
#72763=CARTESIAN_POINT('Ctrl Pts',(3.85962774407633,-1.,0.19231515304497));
#72764=CARTESIAN_POINT('Ctrl Pts',(3.85962774407633,1.,0.19231515304497));
#72765=CARTESIAN_POINT('Ctrl Pts',(3.86707158624783,-1.,0.190924190418619));
#72766=CARTESIAN_POINT('Ctrl Pts',(3.86707158624783,1.,0.190924190418619));
#72767=CARTESIAN_POINT('Ctrl Pts',(3.87445976418412,-1.,0.189469253358272));
#72768=CARTESIAN_POINT('Ctrl Pts',(3.87445976418412,1.,0.189469253358272));
#72769=CARTESIAN_POINT('Ctrl Pts',(3.88178563496228,-1.,0.187951632512684));
#72770=CARTESIAN_POINT('Ctrl Pts',(3.88178563496228,1.,0.187951632512684));
#72771=CARTESIAN_POINT('Ctrl Pts',(3.88906196725848,-1.,0.18637372498528));
#72772=CARTESIAN_POINT('Ctrl Pts',(3.88906196725848,1.,0.18637372498528));
#72773=CARTESIAN_POINT('Ctrl Pts',(3.89631300742646,-1.,0.184738537728042));
#72774=CARTESIAN_POINT('Ctrl Pts',(3.89631300742646,1.,0.184738537728042));
#72775=CARTESIAN_POINT('Ctrl Pts',(3.90356488555132,-1.,0.18304908199319));
#72776=CARTESIAN_POINT('Ctrl Pts',(3.90356488555132,1.,0.18304908199319));
#72777=CARTESIAN_POINT('Ctrl Pts',(3.91083557557175,-1.,0.181307740731785));
#72778=CARTESIAN_POINT('Ctrl Pts',(3.91083557557175,1.,0.181307740731785));
#72779=CARTESIAN_POINT('Ctrl Pts',(3.91812876180926,-1.,0.179515885822881));
#72780=CARTESIAN_POINT('Ctrl Pts',(3.91812876180926,1.,0.179515885822881));
#72781=CARTESIAN_POINT('Ctrl Pts',(3.92543942697655,-1.,0.177674246152317));
#72782=CARTESIAN_POINT('Ctrl Pts',(3.92543942697655,1.,0.177674246152317));
#72783=CARTESIAN_POINT('Ctrl Pts',(3.93275726771042,-1.,0.175783136893867));
#72784=CARTESIAN_POINT('Ctrl Pts',(3.93275726771042,1.,0.175783136893867));
#72785=CARTESIAN_POINT('Ctrl Pts',(3.94007083096217,-1.,0.173842734974609));
#72786=CARTESIAN_POINT('Ctrl Pts',(3.94007083096217,1.,0.173842734974609));
#72787=CARTESIAN_POINT('Ctrl Pts',(3.94737164900868,-1.,0.17185335536924));
#72788=CARTESIAN_POINT('Ctrl Pts',(3.94737164900868,1.,0.17185335536924));
#72789=CARTESIAN_POINT('Ctrl Pts',(3.95465744665268,-1.,0.169815666374138));
#72790=CARTESIAN_POINT('Ctrl Pts',(3.95465744665268,1.,0.169815666374138));
#72791=CARTESIAN_POINT('Ctrl Pts',(3.96192990160296,-1.,0.167730547023319));
#72792=CARTESIAN_POINT('Ctrl Pts',(3.96192990160296,1.,0.167730547023319));
#72793=CARTESIAN_POINT('Ctrl Pts',(3.96919313621407,-1.,0.165598992851102));
#72794=CARTESIAN_POINT('Ctrl Pts',(3.96919313621407,1.,0.165598992851102));
#72795=CARTESIAN_POINT('Ctrl Pts',(3.97645194630943,-1.,0.163422004609999));
#72796=CARTESIAN_POINT('Ctrl Pts',(3.97645194630943,1.,0.163422004609999));
#72797=CARTESIAN_POINT('Ctrl Pts',(3.98371010319872,-1.,0.161200482186084));
#72798=CARTESIAN_POINT('Ctrl Pts',(3.98371010319872,1.,0.161200482186084));
#72799=CARTESIAN_POINT('Ctrl Pts',(3.99096873945878,-1.,0.158935123982793));
#72800=CARTESIAN_POINT('Ctrl Pts',(3.99096873945878,1.,0.158935123982793));
#72801=CARTESIAN_POINT('Ctrl Pts',(3.99822717425893,-1.,0.156626481393734));
#72802=CARTESIAN_POINT('Ctrl Pts',(3.99822717425893,1.,0.156626481393734));
#72803=CARTESIAN_POINT('Ctrl Pts',(4.00548360245319,-1.,0.15427500487231));
#72804=CARTESIAN_POINT('Ctrl Pts',(4.00548360245319,1.,0.15427500487231));
#72805=CARTESIAN_POINT('Ctrl Pts',(4.01273584234689,-1.,0.15188109402291));
#72806=CARTESIAN_POINT('Ctrl Pts',(4.01273584234689,1.,0.15188109402291));
#72807=CARTESIAN_POINT('Ctrl Pts',(4.01998203715564,-1.,0.149445144968706));
#72808=CARTESIAN_POINT('Ctrl Pts',(4.01998203715564,1.,0.149445144968706));
#72809=CARTESIAN_POINT('Ctrl Pts',(4.02722143146994,-1.,0.146967602878994));
#72810=CARTESIAN_POINT('Ctrl Pts',(4.02722143146994,1.,0.146967602878994));
#72811=CARTESIAN_POINT('Ctrl Pts',(4.03445411510333,-1.,0.144448947038344));
#72812=CARTESIAN_POINT('Ctrl Pts',(4.03445411510333,1.,0.144448947038344));
#72813=CARTESIAN_POINT('Ctrl Pts',(4.04168069633781,-1.,0.1418896714855));
#72814=CARTESIAN_POINT('Ctrl Pts',(4.04168069633781,1.,0.1418896714855));
#72815=CARTESIAN_POINT('Ctrl Pts',(4.04890199238036,-1.,0.139290267180057));
#72816=CARTESIAN_POINT('Ctrl Pts',(4.04890199238036,1.,0.139290267180057));
#72817=CARTESIAN_POINT('Ctrl Pts',(4.05611873400172,-1.,0.136651205046119));
#72818=CARTESIAN_POINT('Ctrl Pts',(4.05611873400172,1.,0.136651205046119));
#72819=CARTESIAN_POINT('Ctrl Pts',(4.06333121018596,-1.,0.133972916144244));
#72820=CARTESIAN_POINT('Ctrl Pts',(4.06333121018596,1.,0.133972916144244));
#72821=CARTESIAN_POINT('Ctrl Pts',(4.0705393152874,-1.,0.13125579354894));
#72822=CARTESIAN_POINT('Ctrl Pts',(4.0705393152874,1.,0.13125579354894));
#72823=CARTESIAN_POINT('Ctrl Pts',(4.07774270738954,-1.,0.128500200484837));
#72824=CARTESIAN_POINT('Ctrl Pts',(4.07774270738954,1.,0.128500200484837));
#72825=CARTESIAN_POINT('Ctrl Pts',(4.08494093372377,-1.,0.125706476822539));
#72826=CARTESIAN_POINT('Ctrl Pts',(4.08494093372377,1.,0.125706476822539));
#72827=CARTESIAN_POINT('Ctrl Pts',(4.09213355850756,-1.,0.122874946249106));
#72828=CARTESIAN_POINT('Ctrl Pts',(4.09213355850756,1.,0.122874946249106));
#72829=CARTESIAN_POINT('Ctrl Pts',(4.09932031767002,-1.,0.120005924388124));
#72830=CARTESIAN_POINT('Ctrl Pts',(4.09932031767002,1.,0.120005924388124));
#72831=CARTESIAN_POINT('Ctrl Pts',(4.10650113381833,-1.,0.117099722731648));
#72832=CARTESIAN_POINT('Ctrl Pts',(4.10650113381833,1.,0.117099722731648));
#72833=CARTESIAN_POINT('Ctrl Pts',(4.11367603924961,-1.,0.114156649609545));
#72834=CARTESIAN_POINT('Ctrl Pts',(4.11367603924961,1.,0.114156649609545));
#72835=CARTESIAN_POINT('Ctrl Pts',(4.1208451250225,-1.,0.111177012683346));
#72836=CARTESIAN_POINT('Ctrl Pts',(4.1208451250225,1.,0.111177012683346));
#72837=CARTESIAN_POINT('Ctrl Pts',(4.12800848371504,-1.,0.108161120528369));
#72838=CARTESIAN_POINT('Ctrl Pts',(4.12800848371504,1.,0.108161120528369));
#72839=CARTESIAN_POINT('Ctrl Pts',(4.13516614458895,-1.,0.105109286538945));
#72840=CARTESIAN_POINT('Ctrl Pts',(4.13516614458895,1.,0.105109286538945));
#72841=CARTESIAN_POINT('Ctrl Pts',(4.14231804939538,-1.,0.102021826577583));
#72842=CARTESIAN_POINT('Ctrl Pts',(4.14231804939538,1.,0.102021826577583));
#72843=CARTESIAN_POINT('Ctrl Pts',(4.14946408918485,-1.,0.0988990478901221));
#72844=CARTESIAN_POINT('Ctrl Pts',(4.14946408918485,1.,0.0988990478901221));
#72845=CARTESIAN_POINT('Ctrl Pts',(4.15660412653577,-1.,0.0957412403298002));
#72846=CARTESIAN_POINT('Ctrl Pts',(4.15660412653577,1.,0.0957412403298002));
#72847=CARTESIAN_POINT('Ctrl Pts',(4.16373802265839,-1.,0.0925486672167526));
#72848=CARTESIAN_POINT('Ctrl Pts',(4.16373802265839,1.,0.0925486672167526));
#72849=CARTESIAN_POINT('Ctrl Pts',(4.17086566490794,-1.,0.0893215560848644));
#72850=CARTESIAN_POINT('Ctrl Pts',(4.17086566490794,1.,0.0893215560848644));
#72851=CARTESIAN_POINT('Ctrl Pts',(4.17798698668094,-1.,0.0860600915549391));
#72852=CARTESIAN_POINT('Ctrl Pts',(4.17798698668094,1.,0.0860600915549391));
#72853=CARTESIAN_POINT('Ctrl Pts',(4.18510195327123,-1.,0.0827644164385674));
#72854=CARTESIAN_POINT('Ctrl Pts',(4.18510195327123,1.,0.0827644164385674));
#72855=CARTESIAN_POINT('Ctrl Pts',(4.19078883320504,-1.,0.0801005887114315));
#72856=CARTESIAN_POINT('Ctrl Pts',(4.19078883320504,1.,0.0801005887114315));
#72857=CARTESIAN_POINT('Ctrl Pts',(4.19505112859416,-1.,0.0780873956242392));
#72858=CARTESIAN_POINT('Ctrl Pts',(4.19505112859416,1.,0.0780873956242392));
#72859=CARTESIAN_POINT('Ctrl Pts',(4.1978913862118,-1.,0.0767384596141459));
#72860=CARTESIAN_POINT('Ctrl Pts',(4.1978913862118,1.,0.0767384596141459));
#72861=CARTESIAN_POINT('Ctrl Pts',(4.19931119685982,-1.,0.0760622897878241));
#72862=CARTESIAN_POINT('Ctrl Pts',(4.19931119685982,1.,0.0760622897878241));
#72863=CARTESIAN_POINT('',(3.74449296983004,1.,0.2031560948961));
#72864=CARTESIAN_POINT('Ctrl Pts',(3.74449296983004,-1.,0.2031560948961));
#72865=CARTESIAN_POINT('Ctrl Pts',(3.74449296983004,-0.666666666666667,
0.2031560948961));
#72866=CARTESIAN_POINT('Ctrl Pts',(3.74449296983004,-0.333333333333333,
0.2031560948961));
#72867=CARTESIAN_POINT('Ctrl Pts',(3.74449296983004,0.333333333333333,0.2031560948961));
#72868=CARTESIAN_POINT('Ctrl Pts',(3.74449296983004,0.666666666666667,0.2031560948961));
#72869=CARTESIAN_POINT('Ctrl Pts',(3.74449296983004,1.,0.2031560948961));
#72870=CARTESIAN_POINT('',(4.19931119685982,1.,0.0760622897878241));
#72871=CARTESIAN_POINT('',(4.19931119685982,0.,0.0760622897878241));
#72872=CARTESIAN_POINT('Ctrl Pts',(3.74449296983004,1.,0.2031560948961));
#72873=CARTESIAN_POINT('Ctrl Pts',(3.74453008995092,1.,0.203188003946656));
#72874=CARTESIAN_POINT('Ctrl Pts',(3.74471097893845,1.,0.20326661011053));
#72875=CARTESIAN_POINT('Ctrl Pts',(3.74535749969115,1.,0.203375226874121));
#72876=CARTESIAN_POINT('Ctrl Pts',(3.74703926501752,1.,0.203484186269415));
#72877=CARTESIAN_POINT('Ctrl Pts',(3.75054693397875,1.,0.203550035479166));
#72878=CARTESIAN_POINT('Ctrl Pts',(3.75585118707734,1.,0.203530796848321));
#72879=CARTESIAN_POINT('Ctrl Pts',(3.76242717936885,1.,0.203414634707478));
#72880=CARTESIAN_POINT('Ctrl Pts',(3.7699207159487,1.,0.203192390045164));
#72881=CARTESIAN_POINT('Ctrl Pts',(3.77793553476614,1.,0.20285472969908));
#72882=CARTESIAN_POINT('Ctrl Pts',(3.78609175019242,1.,0.20239426051216));
#72883=CARTESIAN_POINT('Ctrl Pts',(3.7940835418736,1.,0.201807533800837));
#72884=CARTESIAN_POINT('Ctrl Pts',(3.80175247447337,1.,0.201097756307325));
#72885=CARTESIAN_POINT('Ctrl Pts',(3.80909529318669,1.,0.200274679433364));
#72886=CARTESIAN_POINT('Ctrl Pts',(3.81620203429815,1.,0.199351525297447));
#72887=CARTESIAN_POINT('Ctrl Pts',(3.82321127349016,1.,0.198342616900486));
#72888=CARTESIAN_POINT('Ctrl Pts',(3.83026221776456,1.,0.197260935827361));
#72889=CARTESIAN_POINT('Ctrl Pts',(3.83743910616195,1.,0.196115198971858));
#72890=CARTESIAN_POINT('Ctrl Pts',(3.84475203346977,1.,0.19490900946022));
#72891=CARTESIAN_POINT('Ctrl Pts',(3.85216762263966,1.,0.193642806777722));
#72892=CARTESIAN_POINT('Ctrl Pts',(3.85962774407633,1.,0.19231515304497));
#72893=CARTESIAN_POINT('Ctrl Pts',(3.86707158624783,1.,0.190924190418619));
#72894=CARTESIAN_POINT('Ctrl Pts',(3.87445976418412,1.,0.189469253358272));
#72895=CARTESIAN_POINT('Ctrl Pts',(3.88178563496228,1.,0.187951632512684));
#72896=CARTESIAN_POINT('Ctrl Pts',(3.88906196725848,1.,0.18637372498528));
#72897=CARTESIAN_POINT('Ctrl Pts',(3.89631300742646,1.,0.184738537728042));
#72898=CARTESIAN_POINT('Ctrl Pts',(3.90356488555132,1.,0.18304908199319));
#72899=CARTESIAN_POINT('Ctrl Pts',(3.91083557557175,1.,0.181307740731785));
#72900=CARTESIAN_POINT('Ctrl Pts',(3.91812876180926,1.,0.179515885822881));
#72901=CARTESIAN_POINT('Ctrl Pts',(3.92543942697655,1.,0.177674246152317));
#72902=CARTESIAN_POINT('Ctrl Pts',(3.93275726771042,1.,0.175783136893867));
#72903=CARTESIAN_POINT('Ctrl Pts',(3.94007083096217,1.,0.173842734974609));
#72904=CARTESIAN_POINT('Ctrl Pts',(3.94737164900868,1.,0.17185335536924));
#72905=CARTESIAN_POINT('Ctrl Pts',(3.95465744665268,1.,0.169815666374138));
#72906=CARTESIAN_POINT('Ctrl Pts',(3.96192990160296,1.,0.167730547023319));
#72907=CARTESIAN_POINT('Ctrl Pts',(3.96919313621407,1.,0.165598992851102));
#72908=CARTESIAN_POINT('Ctrl Pts',(3.97645194630943,1.,0.163422004609999));
#72909=CARTESIAN_POINT('Ctrl Pts',(3.98371010319872,1.,0.161200482186084));
#72910=CARTESIAN_POINT('Ctrl Pts',(3.99096873945878,1.,0.158935123982793));
#72911=CARTESIAN_POINT('Ctrl Pts',(3.99822717425893,1.,0.156626481393734));
#72912=CARTESIAN_POINT('Ctrl Pts',(4.00548360245319,1.,0.15427500487231));
#72913=CARTESIAN_POINT('Ctrl Pts',(4.01273584234689,1.,0.15188109402291));
#72914=CARTESIAN_POINT('Ctrl Pts',(4.01998203715564,1.,0.149445144968706));
#72915=CARTESIAN_POINT('Ctrl Pts',(4.02722143146994,1.,0.146967602878994));
#72916=CARTESIAN_POINT('Ctrl Pts',(4.03445411510333,1.,0.144448947038344));
#72917=CARTESIAN_POINT('Ctrl Pts',(4.04168069633781,1.,0.1418896714855));
#72918=CARTESIAN_POINT('Ctrl Pts',(4.04890199238036,1.,0.139290267180057));
#72919=CARTESIAN_POINT('Ctrl Pts',(4.05611873400172,1.,0.136651205046119));
#72920=CARTESIAN_POINT('Ctrl Pts',(4.06333121018596,1.,0.133972916144244));
#72921=CARTESIAN_POINT('Ctrl Pts',(4.0705393152874,1.,0.13125579354894));
#72922=CARTESIAN_POINT('Ctrl Pts',(4.07774270738954,1.,0.128500200484837));
#72923=CARTESIAN_POINT('Ctrl Pts',(4.08494093372377,1.,0.125706476822539));
#72924=CARTESIAN_POINT('Ctrl Pts',(4.09213355850756,1.,0.122874946249106));
#72925=CARTESIAN_POINT('Ctrl Pts',(4.09932031767002,1.,0.120005924388124));
#72926=CARTESIAN_POINT('Ctrl Pts',(4.10650113381833,1.,0.117099722731648));
#72927=CARTESIAN_POINT('Ctrl Pts',(4.11367603924961,1.,0.114156649609545));
#72928=CARTESIAN_POINT('Ctrl Pts',(4.1208451250225,1.,0.111177012683346));
#72929=CARTESIAN_POINT('Ctrl Pts',(4.12800848371504,1.,0.108161120528369));
#72930=CARTESIAN_POINT('Ctrl Pts',(4.13516614458895,1.,0.105109286538945));
#72931=CARTESIAN_POINT('Ctrl Pts',(4.14231804939538,1.,0.102021826577583));
#72932=CARTESIAN_POINT('Ctrl Pts',(4.14946408918485,1.,0.0988990478901221));
#72933=CARTESIAN_POINT('Ctrl Pts',(4.15660412653577,1.,0.0957412403298002));
#72934=CARTESIAN_POINT('Ctrl Pts',(4.16373802265839,1.,0.0925486672167526));
#72935=CARTESIAN_POINT('Ctrl Pts',(4.17086566490794,1.,0.0893215560848644));
#72936=CARTESIAN_POINT('Ctrl Pts',(4.17798698668094,1.,0.0860600915549391));
#72937=CARTESIAN_POINT('Ctrl Pts',(4.18510195327123,1.,0.0827644164385674));
#72938=CARTESIAN_POINT('Ctrl Pts',(4.19078883320504,1.,0.0801005887114315));
#72939=CARTESIAN_POINT('Ctrl Pts',(4.19505112859416,1.,0.0780873956242392));
#72940=CARTESIAN_POINT('Ctrl Pts',(4.1978913862118,1.,0.0767384596141459));
#72941=CARTESIAN_POINT('Ctrl Pts',(4.19931119685982,1.,0.0760622897878241));
#72942=CARTESIAN_POINT('Ctrl Pts',(4.19931119685982,-1.,-0.0760622897878241));
#72943=CARTESIAN_POINT('Ctrl Pts',(4.19931119685982,1.,-0.0760622897878241));
#72944=CARTESIAN_POINT('Ctrl Pts',(4.19789138621624,-1.,-0.07673845961422));
#72945=CARTESIAN_POINT('Ctrl Pts',(4.19789138621624,1.,-0.07673845961422));
#72946=CARTESIAN_POINT('Ctrl Pts',(4.19505112860624,-1.,-0.0780873956244407));
#72947=CARTESIAN_POINT('Ctrl Pts',(4.19505112860624,1.,-0.0780873956244407));
#72948=CARTESIAN_POINT('Ctrl Pts',(4.19078883322483,-1.,-0.0801005887117608));
#72949=CARTESIAN_POINT('Ctrl Pts',(4.19078883322483,1.,-0.0801005887117608));
#72950=CARTESIAN_POINT('Ctrl Pts',(4.1851019532944,-1.,-0.0827644164389515));
#72951=CARTESIAN_POINT('Ctrl Pts',(4.1851019532944,1.,-0.0827644164389515));
#72952=CARTESIAN_POINT('Ctrl Pts',(4.17798698669991,-1.,-0.086060091555252));
#72953=CARTESIAN_POINT('Ctrl Pts',(4.17798698669991,1.,-0.086060091555252));
#72954=CARTESIAN_POINT('Ctrl Pts',(4.17086566491823,-1.,-0.0893215560850332));
#72955=CARTESIAN_POINT('Ctrl Pts',(4.17086566491823,1.,-0.0893215560850332));
#72956=CARTESIAN_POINT('Ctrl Pts',(4.16373802265942,-1.,-0.0925486672167695));
#72957=CARTESIAN_POINT('Ctrl Pts',(4.16373802265942,1.,-0.0925486672167695));
#72958=CARTESIAN_POINT('Ctrl Pts',(4.15660412653006,-1.,-0.0957412403297072));
#72959=CARTESIAN_POINT('Ctrl Pts',(4.15660412653006,1.,-0.0957412403297072));
#72960=CARTESIAN_POINT('Ctrl Pts',(4.1494640891762,-1.,-0.0988990478899816));
#72961=CARTESIAN_POINT('Ctrl Pts',(4.1494640891762,1.,-0.0988990478899816));
#72962=CARTESIAN_POINT('Ctrl Pts',(4.14231804938737,-1.,-0.102021826577454));
#72963=CARTESIAN_POINT('Ctrl Pts',(4.14231804938737,1.,-0.102021826577454));
#72964=CARTESIAN_POINT('Ctrl Pts',(4.13516614458396,-1.,-0.105109286538864));
#72965=CARTESIAN_POINT('Ctrl Pts',(4.13516614458396,1.,-0.105109286538864));
#72966=CARTESIAN_POINT('Ctrl Pts',(4.12800848371386,-1.,-0.10816112052835));
#72967=CARTESIAN_POINT('Ctrl Pts',(4.12800848371386,1.,-0.10816112052835));
#72968=CARTESIAN_POINT('Ctrl Pts',(4.12084512502444,-1.,-0.111177012683378));
#72969=CARTESIAN_POINT('Ctrl Pts',(4.12084512502444,1.,-0.111177012683378));
#72970=CARTESIAN_POINT('Ctrl Pts',(4.11367603925313,-1.,-0.114156649609602));
#72971=CARTESIAN_POINT('Ctrl Pts',(4.11367603925313,1.,-0.114156649609602));
#72972=CARTESIAN_POINT('Ctrl Pts',(4.10650113382187,-1.,-0.117099722731705));
#72973=CARTESIAN_POINT('Ctrl Pts',(4.10650113382187,1.,-0.117099722731705));
#72974=CARTESIAN_POINT('Ctrl Pts',(4.09932031767243,-1.,-0.120005924388162));
#72975=CARTESIAN_POINT('Ctrl Pts',(4.09932031767243,1.,-0.120005924388162));
#72976=CARTESIAN_POINT('Ctrl Pts',(4.09213355850836,-1.,-0.122874946249119));
#72977=CARTESIAN_POINT('Ctrl Pts',(4.09213355850836,1.,-0.122874946249119));
#72978=CARTESIAN_POINT('Ctrl Pts',(4.08494093372315,-1.,-0.12570647682253));
#72979=CARTESIAN_POINT('Ctrl Pts',(4.08494093372315,1.,-0.12570647682253));
#72980=CARTESIAN_POINT('Ctrl Pts',(4.07774270738809,-1.,-0.128500200484814));
#72981=CARTESIAN_POINT('Ctrl Pts',(4.07774270738809,1.,-0.128500200484814));
#72982=CARTESIAN_POINT('Ctrl Pts',(4.07053931528579,-1.,-0.131255793548914));
#72983=CARTESIAN_POINT('Ctrl Pts',(4.07053931528579,1.,-0.131255793548914));
#72984=CARTESIAN_POINT('Ctrl Pts',(4.06333121018476,-1.,-0.133972916144225));
#72985=CARTESIAN_POINT('Ctrl Pts',(4.06333121018476,1.,-0.133972916144225));
#72986=CARTESIAN_POINT('Ctrl Pts',(4.05611873400122,-1.,-0.136651205046111));
#72987=CARTESIAN_POINT('Ctrl Pts',(4.05611873400122,1.,-0.136651205046111));
#72988=CARTESIAN_POINT('Ctrl Pts',(4.04890199238056,-1.,-0.13929026718006));
#72989=CARTESIAN_POINT('Ctrl Pts',(4.04890199238056,1.,-0.13929026718006));
#72990=CARTESIAN_POINT('Ctrl Pts',(4.04168069633842,-1.,-0.141889671485508));
#72991=CARTESIAN_POINT('Ctrl Pts',(4.04168069633842,1.,-0.141889671485508));
#72992=CARTESIAN_POINT('Ctrl Pts',(4.03445411510403,-1.,-0.144448947038352));
#72993=CARTESIAN_POINT('Ctrl Pts',(4.03445411510403,1.,-0.144448947038352));
#72994=CARTESIAN_POINT('Ctrl Pts',(4.02722143147048,-1.,-0.146967602878999));
#72995=CARTESIAN_POINT('Ctrl Pts',(4.02722143147048,1.,-0.146967602878999));
#72996=CARTESIAN_POINT('Ctrl Pts',(4.01998203715588,-1.,-0.149445144968708));
#72997=CARTESIAN_POINT('Ctrl Pts',(4.01998203715588,1.,-0.149445144968708));
#72998=CARTESIAN_POINT('Ctrl Pts',(4.01273584234684,-1.,-0.151881094022909));
#72999=CARTESIAN_POINT('Ctrl Pts',(4.01273584234684,1.,-0.151881094022909));
#73000=CARTESIAN_POINT('Ctrl Pts',(4.00548360245297,-1.,-0.15427500487231));
#73001=CARTESIAN_POINT('Ctrl Pts',(4.00548360245297,1.,-0.15427500487231));
#73002=CARTESIAN_POINT('Ctrl Pts',(3.99822717425869,-1.,-0.156626481393736));
#73003=CARTESIAN_POINT('Ctrl Pts',(3.99822717425869,1.,-0.156626481393736));
#73004=CARTESIAN_POINT('Ctrl Pts',(3.99096873945862,-1.,-0.158935123982796));
#73005=CARTESIAN_POINT('Ctrl Pts',(3.99096873945862,1.,-0.158935123982796));
#73006=CARTESIAN_POINT('Ctrl Pts',(3.98371010319866,-1.,-0.161200482186088));
#73007=CARTESIAN_POINT('Ctrl Pts',(3.98371010319866,1.,-0.161200482186088));
#73008=CARTESIAN_POINT('Ctrl Pts',(3.97645194630944,-1.,-0.163422004609999));
#73009=CARTESIAN_POINT('Ctrl Pts',(3.97645194630944,1.,-0.163422004609999));
#73010=CARTESIAN_POINT('Ctrl Pts',(3.9691931362141,-1.,-0.165598992851098));
#73011=CARTESIAN_POINT('Ctrl Pts',(3.9691931362141,1.,-0.165598992851098));
#73012=CARTESIAN_POINT('Ctrl Pts',(3.96192990160296,-1.,-0.167730547023312));
#73013=CARTESIAN_POINT('Ctrl Pts',(3.96192990160296,1.,-0.167730547023312));
#73014=CARTESIAN_POINT('Ctrl Pts',(3.95465744665263,-1.,-0.16981566637413));
#73015=CARTESIAN_POINT('Ctrl Pts',(3.95465744665263,1.,-0.16981566637413));
#73016=CARTESIAN_POINT('Ctrl Pts',(3.94737164900861,-1.,-0.171853355369233));
#73017=CARTESIAN_POINT('Ctrl Pts',(3.94737164900861,1.,-0.171853355369233));
#73018=CARTESIAN_POINT('Ctrl Pts',(3.94007083096214,-1.,-0.173842734974608));
#73019=CARTESIAN_POINT('Ctrl Pts',(3.94007083096214,1.,-0.173842734974608));
#73020=CARTESIAN_POINT('Ctrl Pts',(3.93275726771049,-1.,-0.175783136893873));
#73021=CARTESIAN_POINT('Ctrl Pts',(3.93275726771049,1.,-0.175783136893873));
#73022=CARTESIAN_POINT('Ctrl Pts',(3.92543942697672,-1.,-0.177674246152328));
#73023=CARTESIAN_POINT('Ctrl Pts',(3.92543942697672,1.,-0.177674246152328));
#73024=CARTESIAN_POINT('Ctrl Pts',(3.91812876180948,-1.,-0.179515885822895));
#73025=CARTESIAN_POINT('Ctrl Pts',(3.91812876180948,1.,-0.179515885822895));
#73026=CARTESIAN_POINT('Ctrl Pts',(3.91083557557193,-1.,-0.181307740731796));
#73027=CARTESIAN_POINT('Ctrl Pts',(3.91083557557193,1.,-0.181307740731796));
#73028=CARTESIAN_POINT('Ctrl Pts',(3.90356488555138,-1.,-0.183049081993193));
#73029=CARTESIAN_POINT('Ctrl Pts',(3.90356488555138,1.,-0.183049081993193));
#73030=CARTESIAN_POINT('Ctrl Pts',(3.89631300742633,-1.,-0.184738537728035));
#73031=CARTESIAN_POINT('Ctrl Pts',(3.89631300742633,1.,-0.184738537728035));
#73032=CARTESIAN_POINT('Ctrl Pts',(3.88906196725817,-1.,-0.186373724985263));
#73033=CARTESIAN_POINT('Ctrl Pts',(3.88906196725817,1.,-0.186373724985263));
#73034=CARTESIAN_POINT('Ctrl Pts',(3.88178563496187,-1.,-0.187951632512664));
#73035=CARTESIAN_POINT('Ctrl Pts',(3.88178563496187,1.,-0.187951632512664));
#73036=CARTESIAN_POINT('Ctrl Pts',(3.87445976418377,-1.,-0.189469253358255));
#73037=CARTESIAN_POINT('Ctrl Pts',(3.87445976418377,1.,-0.189469253358255));
#73038=CARTESIAN_POINT('Ctrl Pts',(3.8670715862477,-1.,-0.190924190418613));
#73039=CARTESIAN_POINT('Ctrl Pts',(3.8670715862477,1.,-0.190924190418613));
#73040=CARTESIAN_POINT('Ctrl Pts',(3.85962774407652,-1.,-0.19231515304498));
#73041=CARTESIAN_POINT('Ctrl Pts',(3.85962774407652,1.,-0.19231515304498));
#73042=CARTESIAN_POINT('Ctrl Pts',(3.85216762264019,-1.,-0.193642806777748));
#73043=CARTESIAN_POINT('Ctrl Pts',(3.85216762264019,1.,-0.193642806777748));
#73044=CARTESIAN_POINT('Ctrl Pts',(3.84475203347052,-1.,-0.194909009460255));
#73045=CARTESIAN_POINT('Ctrl Pts',(3.84475203347052,1.,-0.194909009460255));
#73046=CARTESIAN_POINT('Ctrl Pts',(3.83743910616265,-1.,-0.19611519897189));
#73047=CARTESIAN_POINT('Ctrl Pts',(3.83743910616265,1.,-0.19611519897189));
#73048=CARTESIAN_POINT('Ctrl Pts',(3.83026221776488,-1.,-0.197260935827375));
#73049=CARTESIAN_POINT('Ctrl Pts',(3.83026221776488,1.,-0.197260935827375));
#73050=CARTESIAN_POINT('Ctrl Pts',(3.82321127348981,-1.,-0.19834261690047));
#73051=CARTESIAN_POINT('Ctrl Pts',(3.82321127348981,1.,-0.19834261690047));
#73052=CARTESIAN_POINT('Ctrl Pts',(3.81620203429702,-1.,-0.199351525297397));
#73053=CARTESIAN_POINT('Ctrl Pts',(3.81620203429702,1.,-0.199351525297397));
#73054=CARTESIAN_POINT('Ctrl Pts',(3.80909529318501,-1.,-0.20027467943329));
#73055=CARTESIAN_POINT('Ctrl Pts',(3.80909529318501,1.,-0.20027467943329));
#73056=CARTESIAN_POINT('Ctrl Pts',(3.80175247447171,-1.,-0.201097756307252));
#73057=CARTESIAN_POINT('Ctrl Pts',(3.80175247447171,1.,-0.201097756307252));
#73058=CARTESIAN_POINT('Ctrl Pts',(3.79408354187274,-1.,-0.201807533800799));
#73059=CARTESIAN_POINT('Ctrl Pts',(3.79408354187274,1.,-0.201807533800799));
#73060=CARTESIAN_POINT('Ctrl Pts',(3.78609175019317,-1.,-0.202394260512193));
#73061=CARTESIAN_POINT('Ctrl Pts',(3.78609175019317,1.,-0.202394260512193));
#73062=CARTESIAN_POINT('Ctrl Pts',(3.77793553476879,-1.,-0.202854729699197));
#73063=CARTESIAN_POINT('Ctrl Pts',(3.77793553476879,1.,-0.202854729699197));
#73064=CARTESIAN_POINT('Ctrl Pts',(3.76992071595267,-1.,-0.203192390045338));
#73065=CARTESIAN_POINT('Ctrl Pts',(3.76992071595267,1.,-0.203192390045338));
#73066=CARTESIAN_POINT('Ctrl Pts',(3.76242717937273,-1.,-0.203414634707647));
#73067=CARTESIAN_POINT('Ctrl Pts',(3.76242717937273,1.,-0.203414634707647));
#73068=CARTESIAN_POINT('Ctrl Pts',(3.75585118707924,-1.,-0.203530796848404));
#73069=CARTESIAN_POINT('Ctrl Pts',(3.75585118707924,1.,-0.203530796848404));
#73070=CARTESIAN_POINT('Ctrl Pts',(3.75054693397716,-1.,-0.203550035479097));
#73071=CARTESIAN_POINT('Ctrl Pts',(3.75054693397716,1.,-0.203550035479097));
#73072=CARTESIAN_POINT('Ctrl Pts',(3.74675472018582,-1.,-0.20347884453023));
#73073=CARTESIAN_POINT('Ctrl Pts',(3.74675472018582,1.,-0.20347884453023));
#73074=CARTESIAN_POINT('Ctrl Pts',(3.7450208092684,-1.,-0.203352057956056));
#73075=CARTESIAN_POINT('Ctrl Pts',(3.7450208092684,1.,-0.203352057956056));
#73076=CARTESIAN_POINT('Ctrl Pts',(3.74446880195845,-1.,-0.203218215747895));
#73077=CARTESIAN_POINT('Ctrl Pts',(3.74446880195845,1.,-0.203218215747895));
#73078=CARTESIAN_POINT('Ctrl Pts',(3.74443319346666,-1.,-0.20311176758786));
#73079=CARTESIAN_POINT('Ctrl Pts',(3.74443319346666,1.,-0.20311176758786));
#73080=CARTESIAN_POINT('Ctrl Pts',(3.74449849461127,-1.,-0.20305423869972));
#73081=CARTESIAN_POINT('Ctrl Pts',(3.74449849461127,1.,-0.20305423869972));
#73082=CARTESIAN_POINT('',(4.19931119685982,1.,-0.0760622897878241));
#73083=CARTESIAN_POINT('Ctrl Pts',(4.19931119685982,1.,-0.0760622897878241));
#73084=CARTESIAN_POINT('Ctrl Pts',(4.19789138621624,1.,-0.07673845961422));
#73085=CARTESIAN_POINT('Ctrl Pts',(4.19505112860624,1.,-0.0780873956244407));
#73086=CARTESIAN_POINT('Ctrl Pts',(4.19078883322483,1.,-0.0801005887117608));
#73087=CARTESIAN_POINT('Ctrl Pts',(4.1851019532944,1.,-0.0827644164389515));
#73088=CARTESIAN_POINT('Ctrl Pts',(4.17798698669991,1.,-0.086060091555252));
#73089=CARTESIAN_POINT('Ctrl Pts',(4.17086566491823,1.,-0.0893215560850332));
#73090=CARTESIAN_POINT('Ctrl Pts',(4.16373802265942,1.,-0.0925486672167695));
#73091=CARTESIAN_POINT('Ctrl Pts',(4.15660412653006,1.,-0.0957412403297072));
#73092=CARTESIAN_POINT('Ctrl Pts',(4.1494640891762,1.,-0.0988990478899816));
#73093=CARTESIAN_POINT('Ctrl Pts',(4.14231804938737,1.,-0.102021826577454));
#73094=CARTESIAN_POINT('Ctrl Pts',(4.13516614458396,1.,-0.105109286538864));
#73095=CARTESIAN_POINT('Ctrl Pts',(4.12800848371386,1.,-0.10816112052835));
#73096=CARTESIAN_POINT('Ctrl Pts',(4.12084512502444,1.,-0.111177012683378));
#73097=CARTESIAN_POINT('Ctrl Pts',(4.11367603925313,1.,-0.114156649609602));
#73098=CARTESIAN_POINT('Ctrl Pts',(4.10650113382187,1.,-0.117099722731705));
#73099=CARTESIAN_POINT('Ctrl Pts',(4.09932031767243,1.,-0.120005924388162));
#73100=CARTESIAN_POINT('Ctrl Pts',(4.09213355850836,1.,-0.122874946249119));
#73101=CARTESIAN_POINT('Ctrl Pts',(4.08494093372315,1.,-0.12570647682253));
#73102=CARTESIAN_POINT('Ctrl Pts',(4.07774270738809,1.,-0.128500200484814));
#73103=CARTESIAN_POINT('Ctrl Pts',(4.07053931528579,1.,-0.131255793548914));
#73104=CARTESIAN_POINT('Ctrl Pts',(4.06333121018476,1.,-0.133972916144225));
#73105=CARTESIAN_POINT('Ctrl Pts',(4.05611873400122,1.,-0.136651205046111));
#73106=CARTESIAN_POINT('Ctrl Pts',(4.04890199238056,1.,-0.13929026718006));
#73107=CARTESIAN_POINT('Ctrl Pts',(4.04168069633842,1.,-0.141889671485508));
#73108=CARTESIAN_POINT('Ctrl Pts',(4.03445411510403,1.,-0.144448947038352));
#73109=CARTESIAN_POINT('Ctrl Pts',(4.02722143147048,1.,-0.146967602878999));
#73110=CARTESIAN_POINT('Ctrl Pts',(4.01998203715588,1.,-0.149445144968708));
#73111=CARTESIAN_POINT('Ctrl Pts',(4.01273584234684,1.,-0.151881094022909));
#73112=CARTESIAN_POINT('Ctrl Pts',(4.00548360245297,1.,-0.15427500487231));
#73113=CARTESIAN_POINT('Ctrl Pts',(3.99822717425869,1.,-0.156626481393736));
#73114=CARTESIAN_POINT('Ctrl Pts',(3.99096873945862,1.,-0.158935123982796));
#73115=CARTESIAN_POINT('Ctrl Pts',(3.98371010319866,1.,-0.161200482186088));
#73116=CARTESIAN_POINT('Ctrl Pts',(3.97645194630944,1.,-0.163422004609999));
#73117=CARTESIAN_POINT('Ctrl Pts',(3.9691931362141,1.,-0.165598992851098));
#73118=CARTESIAN_POINT('Ctrl Pts',(3.96192990160296,1.,-0.167730547023312));
#73119=CARTESIAN_POINT('Ctrl Pts',(3.95465744665263,1.,-0.16981566637413));
#73120=CARTESIAN_POINT('Ctrl Pts',(3.94737164900861,1.,-0.171853355369233));
#73121=CARTESIAN_POINT('Ctrl Pts',(3.94007083096214,1.,-0.173842734974608));
#73122=CARTESIAN_POINT('Ctrl Pts',(3.93275726771049,1.,-0.175783136893873));
#73123=CARTESIAN_POINT('Ctrl Pts',(3.92543942697672,1.,-0.177674246152328));
#73124=CARTESIAN_POINT('Ctrl Pts',(3.91812876180948,1.,-0.179515885822895));
#73125=CARTESIAN_POINT('Ctrl Pts',(3.91083557557193,1.,-0.181307740731796));
#73126=CARTESIAN_POINT('Ctrl Pts',(3.90356488555138,1.,-0.183049081993193));
#73127=CARTESIAN_POINT('Ctrl Pts',(3.89631300742633,1.,-0.184738537728035));
#73128=CARTESIAN_POINT('Ctrl Pts',(3.88906196725817,1.,-0.186373724985263));
#73129=CARTESIAN_POINT('Ctrl Pts',(3.88178563496187,1.,-0.187951632512664));
#73130=CARTESIAN_POINT('Ctrl Pts',(3.87445976418377,1.,-0.189469253358255));
#73131=CARTESIAN_POINT('Ctrl Pts',(3.8670715862477,1.,-0.190924190418613));
#73132=CARTESIAN_POINT('Ctrl Pts',(3.85962774407652,1.,-0.19231515304498));
#73133=CARTESIAN_POINT('Ctrl Pts',(3.85216762264019,1.,-0.193642806777748));
#73134=CARTESIAN_POINT('Ctrl Pts',(3.84475203347052,1.,-0.194909009460255));
#73135=CARTESIAN_POINT('Ctrl Pts',(3.83743910616265,1.,-0.19611519897189));
#73136=CARTESIAN_POINT('Ctrl Pts',(3.83026221776488,1.,-0.197260935827375));
#73137=CARTESIAN_POINT('Ctrl Pts',(3.82321127348981,1.,-0.19834261690047));
#73138=CARTESIAN_POINT('Ctrl Pts',(3.81620203429702,1.,-0.199351525297397));
#73139=CARTESIAN_POINT('Ctrl Pts',(3.80909529318501,1.,-0.20027467943329));
#73140=CARTESIAN_POINT('Ctrl Pts',(3.80175247447171,1.,-0.201097756307252));
#73141=CARTESIAN_POINT('Ctrl Pts',(3.79408354187274,1.,-0.201807533800799));
#73142=CARTESIAN_POINT('Ctrl Pts',(3.78609175019317,1.,-0.202394260512193));
#73143=CARTESIAN_POINT('Ctrl Pts',(3.77793553476879,1.,-0.202854729699197));
#73144=CARTESIAN_POINT('Ctrl Pts',(3.76992071595267,1.,-0.203192390045338));
#73145=CARTESIAN_POINT('Ctrl Pts',(3.76242717937273,1.,-0.203414634707647));
#73146=CARTESIAN_POINT('Ctrl Pts',(3.75585118707924,1.,-0.203530796848404));
#73147=CARTESIAN_POINT('Ctrl Pts',(3.75054693397716,1.,-0.203550035479097));
#73148=CARTESIAN_POINT('Ctrl Pts',(3.74703926501843,1.,-0.203484186269315));
#73149=CARTESIAN_POINT('Ctrl Pts',(3.74535749969262,1.,-0.203375226874332));
#73150=CARTESIAN_POINT('Ctrl Pts',(3.74471097893961,1.,-0.203266610111264));
#73151=CARTESIAN_POINT('Ctrl Pts',(3.74453008995129,1.,-0.203188003947965));
#73152=CARTESIAN_POINT('Ctrl Pts',(3.74449296982994,1.,-0.203156094897896));
#73153=CARTESIAN_POINT('',(4.19931119685982,0.,-0.0760622897878241));
#73154=CARTESIAN_POINT('Origin',(4.19931119685982,0.,0.0760622897878241));
#73155=CARTESIAN_POINT('',(4.19931119685982,1.,-0.0760622897878241));
#73156=CARTESIAN_POINT('Origin',(0.,1.,0.));
#73157=CARTESIAN_POINT('Origin',(0.,1.,0.));
#73158=CARTESIAN_POINT('Origin',(0.,0.,0.));
#73159=CARTESIAN_POINT('',(0.,0.,0.));
#73160=CARTESIAN_POINT('Origin',(-1.,0.,0.35));
#73161=CARTESIAN_POINT('',(-1.,-0.26,0.6));
#73162=CARTESIAN_POINT('',(-1.,-0.3,0.56));
#73163=CARTESIAN_POINT('',(-1.,-0.2675,0.5925));
#73164=CARTESIAN_POINT('',(-1.,0.26,0.6));
#73165=CARTESIAN_POINT('',(-1.,0.,0.6));
#73166=CARTESIAN_POINT('',(-1.,0.3,0.56));
#73167=CARTESIAN_POINT('',(-1.,0.2675,0.5925));
#73168=CARTESIAN_POINT('',(-1.,0.3,0.04));
#73169=CARTESIAN_POINT('',(-1.,0.3,0.175));
#73170=CARTESIAN_POINT('',(-1.,0.26,0.));
#73171=CARTESIAN_POINT('',(-1.,0.2925,0.0325));
#73172=CARTESIAN_POINT('',(-1.,-0.26,0.));
#73173=CARTESIAN_POINT('',(-1.,0.,0.));
#73174=CARTESIAN_POINT('',(-1.,-0.3,0.04));
#73175=CARTESIAN_POINT('',(-1.,-0.2925,0.0325));
#73176=CARTESIAN_POINT('',(-1.,-0.3,0.175));
#73177=CARTESIAN_POINT('Origin',(0.75,0.28,0.02));
#73178=CARTESIAN_POINT('',(1.,0.3,0.04));
#73179=CARTESIAN_POINT('',(0.75,0.3,0.04));
#73180=CARTESIAN_POINT('',(1.,0.26,0.));
#73181=CARTESIAN_POINT('',(1.,0.2925,0.0325));
#73182=CARTESIAN_POINT('',(0.75,0.26,0.));
#73183=CARTESIAN_POINT('Origin',(1.5,0.3,0.));
#73184=CARTESIAN_POINT('',(1.,0.3,0.56));
#73185=CARTESIAN_POINT('',(0.75,0.3,0.56));
#73186=CARTESIAN_POINT('',(1.,0.3,0.175));
#73187=CARTESIAN_POINT('Origin',(0.75,0.28,0.58));
#73188=CARTESIAN_POINT('',(1.,0.26,0.6));
#73189=CARTESIAN_POINT('',(0.75,0.26,0.6));
#73190=CARTESIAN_POINT('',(1.,0.2675,0.5925));
#73191=CARTESIAN_POINT('Origin',(0.,0.,0.6));
#73192=CARTESIAN_POINT('',(1.,-0.26,0.6));
#73193=CARTESIAN_POINT('',(-0.75,-0.26,0.6));
#73194=CARTESIAN_POINT('',(1.,0.,0.6));
#73195=CARTESIAN_POINT('Origin',(1.,0.,0.35));
#73196=CARTESIAN_POINT('',(1.,-0.26,0.));
#73197=CARTESIAN_POINT('',(1.,-0.3,0.04));
#73198=CARTESIAN_POINT('',(1.,-0.2925,0.0325));
#73199=CARTESIAN_POINT('',(1.,0.,0.));
#73200=CARTESIAN_POINT('',(1.,-0.3,0.56));
#73201=CARTESIAN_POINT('',(1.,-0.2675,0.5925));
#73202=CARTESIAN_POINT('',(1.,-0.3,0.175));
#73203=CARTESIAN_POINT('Origin',(0.,0.,0.));
#73204=CARTESIAN_POINT('',(-0.75,-0.26,0.));
#73205=CARTESIAN_POINT('Origin',(-0.75,-0.28,0.58));
#73206=CARTESIAN_POINT('',(-0.75,-0.3,0.56));
#73207=CARTESIAN_POINT('Origin',(-0.75,-0.28,0.02));
#73208=CARTESIAN_POINT('',(-0.75,-0.3,0.04));
#73209=CARTESIAN_POINT('Origin',(-1.5,-0.3,0.));
#73210=CARTESIAN_POINT('',(0.,0.,0.));
#73211=CARTESIAN_POINT('',(0.,0.,0.));
#73212=CARTESIAN_POINT('',(0.,0.,0.));
#73213=CARTESIAN_POINT('',(0.,0.,0.));
#73214=CARTESIAN_POINT('',(0.,0.,0.));
#73215=CARTESIAN_POINT('',(0.,0.,0.));
#73216=CARTESIAN_POINT('',(0.,0.,0.));
#73217=CARTESIAN_POINT('',(0.,0.,0.));
#73218=CARTESIAN_POINT('',(6.,-8.2,11.8));
#73219=CARTESIAN_POINT('',(6.,8.2,11.8));
#73220=CARTESIAN_POINT('',(6.,-2.,10.));
#73221=CARTESIAN_POINT('',(5.9490015877769,-1.4,9.35200373307347));
#73222=CARTESIAN_POINT('',(6.,2.,10.));
#73223=CARTESIAN_POINT('',(6.,2.6,9.35));
#73224=CARTESIAN_POINT('',(0.,0.,0.));
#73225=CARTESIAN_POINT('',(0.,0.,0.));
#73226=CARTESIAN_POINT('',(0.,0.,0.));
#73227=CARTESIAN_POINT('',(0.,0.,0.));
#73228=CARTESIAN_POINT('',(0.,0.,0.));
#73229=CARTESIAN_POINT('',(0.,0.,0.));
#73230=CARTESIAN_POINT('',(0.,0.,0.));
#73231=CARTESIAN_POINT('',(12.,-8.2,11.8));
#73232=CARTESIAN_POINT('',(12.,8.2,11.8));
#73233=CARTESIAN_POINT('',(12.,2.,10.));
#73234=CARTESIAN_POINT('',(11.9490015877769,2.6,9.35200373307347));
#73235=CARTESIAN_POINT('',(0.,0.,0.));
#73236=CARTESIAN_POINT('',(0.,0.,0.));
#73237=CARTESIAN_POINT('',(0.,0.,0.));
#73238=CARTESIAN_POINT('',(0.,0.,0.));
#73239=UNCERTAINTY_MEASURE_WITH_UNIT(LENGTH_MEASURE(0.001),#73367,
'DISTANCE_ACCURACY_VALUE',
'Maximum model space distance between geometric entities at asserted c
onnectivities');
#73240=UNCERTAINTY_MEASURE_WITH_UNIT(LENGTH_MEASURE(0.001),#73367,
'DISTANCE_ACCURACY_VALUE',
'Maximum model space distance between geometric entities at asserted c
onnectivities');
#73241=UNCERTAINTY_MEASURE_WITH_UNIT(LENGTH_MEASURE(0.001),#73367,
'DISTANCE_ACCURACY_VALUE',
'Maximum model space distance between geometric entities at asserted c
onnectivities');
#73242=UNCERTAINTY_MEASURE_WITH_UNIT(LENGTH_MEASURE(0.001),#73367,
'DISTANCE_ACCURACY_VALUE',
'Maximum model space distance between geometric entities at asserted c
onnectivities');
#73243=UNCERTAINTY_MEASURE_WITH_UNIT(LENGTH_MEASURE(0.001),#73367,
'DISTANCE_ACCURACY_VALUE',
'Maximum model space distance between geometric entities at asserted c
onnectivities');
#73244=UNCERTAINTY_MEASURE_WITH_UNIT(LENGTH_MEASURE(0.001),#73367,
'DISTANCE_ACCURACY_VALUE',
'Maximum model space distance between geometric entities at asserted c
onnectivities');
#73245=UNCERTAINTY_MEASURE_WITH_UNIT(LENGTH_MEASURE(0.001),#73367,
'DISTANCE_ACCURACY_VALUE',
'Maximum model space distance between geometric entities at asserted c
onnectivities');
#73246=UNCERTAINTY_MEASURE_WITH_UNIT(LENGTH_MEASURE(0.001),#73367,
'DISTANCE_ACCURACY_VALUE',
'Maximum model space distance between geometric entities at asserted c
onnectivities');
#73247=UNCERTAINTY_MEASURE_WITH_UNIT(LENGTH_MEASURE(0.001),#73367,
'DISTANCE_ACCURACY_VALUE',
'Maximum model space distance between geometric entities at asserted c
onnectivities');
#73248=UNCERTAINTY_MEASURE_WITH_UNIT(LENGTH_MEASURE(0.001),#73367,
'DISTANCE_ACCURACY_VALUE',
'Maximum model space distance between geometric entities at asserted c
onnectivities');
#73249=UNCERTAINTY_MEASURE_WITH_UNIT(LENGTH_MEASURE(0.001),#73367,
'DISTANCE_ACCURACY_VALUE',
'Maximum model space distance between geometric entities at asserted c
onnectivities');
#73250=UNCERTAINTY_MEASURE_WITH_UNIT(LENGTH_MEASURE(0.001),#73367,
'DISTANCE_ACCURACY_VALUE',
'Maximum model space distance between geometric entities at asserted c
onnectivities');
#73251=UNCERTAINTY_MEASURE_WITH_UNIT(LENGTH_MEASURE(0.001),#73367,
'DISTANCE_ACCURACY_VALUE',
'Maximum model space distance between geometric entities at asserted c
onnectivities');
#73252=UNCERTAINTY_MEASURE_WITH_UNIT(LENGTH_MEASURE(0.001),#73367,
'DISTANCE_ACCURACY_VALUE',
'Maximum model space distance between geometric entities at asserted c
onnectivities');
#73253=UNCERTAINTY_MEASURE_WITH_UNIT(LENGTH_MEASURE(0.001),#73367,
'DISTANCE_ACCURACY_VALUE',
'Maximum model space distance between geometric entities at asserted c
onnectivities');
#73254=UNCERTAINTY_MEASURE_WITH_UNIT(LENGTH_MEASURE(0.001),#73367,
'DISTANCE_ACCURACY_VALUE',
'Maximum model space distance between geometric entities at asserted c
onnectivities');
#73255=UNCERTAINTY_MEASURE_WITH_UNIT(LENGTH_MEASURE(0.001),#73367,
'DISTANCE_ACCURACY_VALUE',
'Maximum model space distance between geometric entities at asserted c
onnectivities');
#73256=UNCERTAINTY_MEASURE_WITH_UNIT(LENGTH_MEASURE(0.001),#73367,
'DISTANCE_ACCURACY_VALUE',
'Maximum model space distance between geometric entities at asserted c
onnectivities');
#73257=UNCERTAINTY_MEASURE_WITH_UNIT(LENGTH_MEASURE(0.001),#73367,
'DISTANCE_ACCURACY_VALUE',
'Maximum model space distance between geometric entities at asserted c
onnectivities');
#73258=UNCERTAINTY_MEASURE_WITH_UNIT(LENGTH_MEASURE(0.001),#73367,
'DISTANCE_ACCURACY_VALUE',
'Maximum model space distance between geometric entities at asserted c
onnectivities');
#73259=UNCERTAINTY_MEASURE_WITH_UNIT(LENGTH_MEASURE(0.001),#73367,
'DISTANCE_ACCURACY_VALUE',
'Maximum model space distance between geometric entities at asserted c
onnectivities');
#73260=UNCERTAINTY_MEASURE_WITH_UNIT(LENGTH_MEASURE(0.001),#73367,
'DISTANCE_ACCURACY_VALUE',
'Maximum model space distance between geometric entities at asserted c
onnectivities');
#73261=UNCERTAINTY_MEASURE_WITH_UNIT(LENGTH_MEASURE(0.001),#73367,
'DISTANCE_ACCURACY_VALUE',
'Maximum model space distance between geometric entities at asserted c
onnectivities');
#73262=UNCERTAINTY_MEASURE_WITH_UNIT(LENGTH_MEASURE(0.001),#73367,
'DISTANCE_ACCURACY_VALUE',
'Maximum model space distance between geometric entities at asserted c
onnectivities');
#73263=UNCERTAINTY_MEASURE_WITH_UNIT(LENGTH_MEASURE(0.001),#73367,
'DISTANCE_ACCURACY_VALUE',
'Maximum model space distance between geometric entities at asserted c
onnectivities');
#73264=UNCERTAINTY_MEASURE_WITH_UNIT(LENGTH_MEASURE(0.001),#73367,
'DISTANCE_ACCURACY_VALUE',
'Maximum model space distance between geometric entities at asserted c
onnectivities');
#73265=UNCERTAINTY_MEASURE_WITH_UNIT(LENGTH_MEASURE(0.001),#73367,
'DISTANCE_ACCURACY_VALUE',
'Maximum model space distance between geometric entities at asserted c
onnectivities');
#73266=UNCERTAINTY_MEASURE_WITH_UNIT(LENGTH_MEASURE(0.001),#73367,
'DISTANCE_ACCURACY_VALUE',
'Maximum model space distance between geometric entities at asserted c
onnectivities');
#73267=UNCERTAINTY_MEASURE_WITH_UNIT(LENGTH_MEASURE(0.001),#73367,
'DISTANCE_ACCURACY_VALUE',
'Maximum model space distance between geometric entities at asserted c
onnectivities');
#73268=UNCERTAINTY_MEASURE_WITH_UNIT(LENGTH_MEASURE(0.001),#73367,
'DISTANCE_ACCURACY_VALUE',
'Maximum model space distance between geometric entities at asserted c
onnectivities');
#73269=UNCERTAINTY_MEASURE_WITH_UNIT(LENGTH_MEASURE(0.001),#73367,
'DISTANCE_ACCURACY_VALUE',
'Maximum model space distance between geometric entities at asserted c
onnectivities');
#73270=UNCERTAINTY_MEASURE_WITH_UNIT(LENGTH_MEASURE(0.001),#73367,
'DISTANCE_ACCURACY_VALUE',
'Maximum model space distance between geometric entities at asserted c
onnectivities');
#73271=UNCERTAINTY_MEASURE_WITH_UNIT(LENGTH_MEASURE(0.001),#73367,
'DISTANCE_ACCURACY_VALUE',
'Maximum model space distance between geometric entities at asserted c
onnectivities');
#73272=UNCERTAINTY_MEASURE_WITH_UNIT(LENGTH_MEASURE(0.001),#73367,
'DISTANCE_ACCURACY_VALUE',
'Maximum model space distance between geometric entities at asserted c
onnectivities');
#73273=UNCERTAINTY_MEASURE_WITH_UNIT(LENGTH_MEASURE(0.001),#73367,
'DISTANCE_ACCURACY_VALUE',
'Maximum model space distance between geometric entities at asserted c
onnectivities');
#73274=UNCERTAINTY_MEASURE_WITH_UNIT(LENGTH_MEASURE(0.001),#73367,
'DISTANCE_ACCURACY_VALUE',
'Maximum model space distance between geometric entities at asserted c
onnectivities');
#73275=UNCERTAINTY_MEASURE_WITH_UNIT(LENGTH_MEASURE(0.001),#73367,
'DISTANCE_ACCURACY_VALUE',
'Maximum model space distance between geometric entities at asserted c
onnectivities');
#73276=UNCERTAINTY_MEASURE_WITH_UNIT(LENGTH_MEASURE(0.001),#73367,
'DISTANCE_ACCURACY_VALUE',
'Maximum model space distance between geometric entities at asserted c
onnectivities');
#73277=UNCERTAINTY_MEASURE_WITH_UNIT(LENGTH_MEASURE(0.001),#73367,
'DISTANCE_ACCURACY_VALUE',
'Maximum model space distance between geometric entities at asserted c
onnectivities');
#73278=UNCERTAINTY_MEASURE_WITH_UNIT(LENGTH_MEASURE(0.001),#73367,
'DISTANCE_ACCURACY_VALUE',
'Maximum model space distance between geometric entities at asserted c
onnectivities');
#73279=UNCERTAINTY_MEASURE_WITH_UNIT(LENGTH_MEASURE(0.001),#73367,
'DISTANCE_ACCURACY_VALUE',
'Maximum model space distance between geometric entities at asserted c
onnectivities');
#73280=UNCERTAINTY_MEASURE_WITH_UNIT(LENGTH_MEASURE(0.001),#73367,
'DISTANCE_ACCURACY_VALUE',
'Maximum model space distance between geometric entities at asserted c
onnectivities');
#73281=UNCERTAINTY_MEASURE_WITH_UNIT(LENGTH_MEASURE(0.001),#73367,
'DISTANCE_ACCURACY_VALUE',
'Maximum model space distance between geometric entities at asserted c
onnectivities');
#73282=UNCERTAINTY_MEASURE_WITH_UNIT(LENGTH_MEASURE(0.001),#73367,
'DISTANCE_ACCURACY_VALUE',
'Maximum model space distance between geometric entities at asserted c
onnectivities');
#73283=UNCERTAINTY_MEASURE_WITH_UNIT(LENGTH_MEASURE(0.001),#73367,
'DISTANCE_ACCURACY_VALUE',
'Maximum model space distance between geometric entities at asserted c
onnectivities');
#73284=UNCERTAINTY_MEASURE_WITH_UNIT(LENGTH_MEASURE(0.001),#73367,
'DISTANCE_ACCURACY_VALUE',
'Maximum model space distance between geometric entities at asserted c
onnectivities');
#73285=UNCERTAINTY_MEASURE_WITH_UNIT(LENGTH_MEASURE(0.001),#73367,
'DISTANCE_ACCURACY_VALUE',
'Maximum model space distance between geometric entities at asserted c
onnectivities');
#73286=UNCERTAINTY_MEASURE_WITH_UNIT(LENGTH_MEASURE(0.001),#73367,
'DISTANCE_ACCURACY_VALUE',
'Maximum model space distance between geometric entities at asserted c
onnectivities');
#73287=UNCERTAINTY_MEASURE_WITH_UNIT(LENGTH_MEASURE(0.001),#73367,
'DISTANCE_ACCURACY_VALUE',
'Maximum model space distance between geometric entities at asserted c
onnectivities');
#73288=UNCERTAINTY_MEASURE_WITH_UNIT(LENGTH_MEASURE(0.001),#73367,
'DISTANCE_ACCURACY_VALUE',
'Maximum model space distance between geometric entities at asserted c
onnectivities');
#73289=UNCERTAINTY_MEASURE_WITH_UNIT(LENGTH_MEASURE(0.001),#73367,
'DISTANCE_ACCURACY_VALUE',
'Maximum model space distance between geometric entities at asserted c
onnectivities');
#73290=UNCERTAINTY_MEASURE_WITH_UNIT(LENGTH_MEASURE(0.001),#73367,
'DISTANCE_ACCURACY_VALUE',
'Maximum model space distance between geometric entities at asserted c
onnectivities');
#73291=UNCERTAINTY_MEASURE_WITH_UNIT(LENGTH_MEASURE(0.001),#73367,
'DISTANCE_ACCURACY_VALUE',
'Maximum model space distance between geometric entities at asserted c
onnectivities');
#73292=UNCERTAINTY_MEASURE_WITH_UNIT(LENGTH_MEASURE(0.001),#73367,
'DISTANCE_ACCURACY_VALUE',
'Maximum model space distance between geometric entities at asserted c
onnectivities');
#73293=UNCERTAINTY_MEASURE_WITH_UNIT(LENGTH_MEASURE(0.001),#73367,
'DISTANCE_ACCURACY_VALUE',
'Maximum model space distance between geometric entities at asserted c
onnectivities');
#73294=UNCERTAINTY_MEASURE_WITH_UNIT(LENGTH_MEASURE(0.001),#73367,
'DISTANCE_ACCURACY_VALUE',
'Maximum model space distance between geometric entities at asserted c
onnectivities');
#73295=UNCERTAINTY_MEASURE_WITH_UNIT(LENGTH_MEASURE(0.001),#73367,
'DISTANCE_ACCURACY_VALUE',
'Maximum model space distance between geometric entities at asserted c
onnectivities');
#73296=UNCERTAINTY_MEASURE_WITH_UNIT(LENGTH_MEASURE(0.001),#73367,
'DISTANCE_ACCURACY_VALUE',
'Maximum model space distance between geometric entities at asserted c
onnectivities');
#73297=UNCERTAINTY_MEASURE_WITH_UNIT(LENGTH_MEASURE(0.001),#73367,
'DISTANCE_ACCURACY_VALUE',
'Maximum model space distance between geometric entities at asserted c
onnectivities');
#73298=UNCERTAINTY_MEASURE_WITH_UNIT(LENGTH_MEASURE(0.001),#73367,
'DISTANCE_ACCURACY_VALUE',
'Maximum model space distance between geometric entities at asserted c
onnectivities');
#73299=UNCERTAINTY_MEASURE_WITH_UNIT(LENGTH_MEASURE(0.001),#73367,
'DISTANCE_ACCURACY_VALUE',
'Maximum model space distance between geometric entities at asserted c
onnectivities');
#73300=UNCERTAINTY_MEASURE_WITH_UNIT(LENGTH_MEASURE(0.001),#73367,
'DISTANCE_ACCURACY_VALUE',
'Maximum model space distance between geometric entities at asserted c
onnectivities');
#73301=UNCERTAINTY_MEASURE_WITH_UNIT(LENGTH_MEASURE(0.001),#73367,
'DISTANCE_ACCURACY_VALUE',
'Maximum model space distance between geometric entities at asserted c
onnectivities');
#73302=UNCERTAINTY_MEASURE_WITH_UNIT(LENGTH_MEASURE(0.001),#73367,
'DISTANCE_ACCURACY_VALUE',
'Maximum model space distance between geometric entities at asserted c
onnectivities');
#73303=(
GEOMETRIC_REPRESENTATION_CONTEXT(3)
GLOBAL_UNCERTAINTY_ASSIGNED_CONTEXT((#73239))
GLOBAL_UNIT_ASSIGNED_CONTEXT((#73367,#73369,#73370))
REPRESENTATION_CONTEXT('','3D')
);
#73304=(
GEOMETRIC_REPRESENTATION_CONTEXT(3)
GLOBAL_UNCERTAINTY_ASSIGNED_CONTEXT((#73240))
GLOBAL_UNIT_ASSIGNED_CONTEXT((#73367,#73369,#73370))
REPRESENTATION_CONTEXT('','3D')
);
#73305=(
GEOMETRIC_REPRESENTATION_CONTEXT(3)
GLOBAL_UNCERTAINTY_ASSIGNED_CONTEXT((#73241))
GLOBAL_UNIT_ASSIGNED_CONTEXT((#73367,#73369,#73370))
REPRESENTATION_CONTEXT('','3D')
);
#73306=(
GEOMETRIC_REPRESENTATION_CONTEXT(3)
GLOBAL_UNCERTAINTY_ASSIGNED_CONTEXT((#73242))
GLOBAL_UNIT_ASSIGNED_CONTEXT((#73367,#73369,#73370))
REPRESENTATION_CONTEXT('','3D')
);
#73307=(
GEOMETRIC_REPRESENTATION_CONTEXT(3)
GLOBAL_UNCERTAINTY_ASSIGNED_CONTEXT((#73243))
GLOBAL_UNIT_ASSIGNED_CONTEXT((#73367,#73369,#73370))
REPRESENTATION_CONTEXT('','3D')
);
#73308=(
GEOMETRIC_REPRESENTATION_CONTEXT(3)
GLOBAL_UNCERTAINTY_ASSIGNED_CONTEXT((#73244))
GLOBAL_UNIT_ASSIGNED_CONTEXT((#73367,#73369,#73370))
REPRESENTATION_CONTEXT('','3D')
);
#73309=(
GEOMETRIC_REPRESENTATION_CONTEXT(3)
GLOBAL_UNCERTAINTY_ASSIGNED_CONTEXT((#73245))
GLOBAL_UNIT_ASSIGNED_CONTEXT((#73367,#73369,#73370))
REPRESENTATION_CONTEXT('','3D')
);
#73310=(
GEOMETRIC_REPRESENTATION_CONTEXT(3)
GLOBAL_UNCERTAINTY_ASSIGNED_CONTEXT((#73246))
GLOBAL_UNIT_ASSIGNED_CONTEXT((#73367,#73369,#73370))
REPRESENTATION_CONTEXT('','3D')
);
#73311=(
GEOMETRIC_REPRESENTATION_CONTEXT(3)
GLOBAL_UNCERTAINTY_ASSIGNED_CONTEXT((#73247))
GLOBAL_UNIT_ASSIGNED_CONTEXT((#73367,#73369,#73370))
REPRESENTATION_CONTEXT('','3D')
);
#73312=(
GEOMETRIC_REPRESENTATION_CONTEXT(3)
GLOBAL_UNCERTAINTY_ASSIGNED_CONTEXT((#73248))
GLOBAL_UNIT_ASSIGNED_CONTEXT((#73367,#73369,#73370))
REPRESENTATION_CONTEXT('','3D')
);
#73313=(
GEOMETRIC_REPRESENTATION_CONTEXT(3)
GLOBAL_UNCERTAINTY_ASSIGNED_CONTEXT((#73249))
GLOBAL_UNIT_ASSIGNED_CONTEXT((#73367,#73369,#73370))
REPRESENTATION_CONTEXT('','3D')
);
#73314=(
GEOMETRIC_REPRESENTATION_CONTEXT(3)
GLOBAL_UNCERTAINTY_ASSIGNED_CONTEXT((#73250))
GLOBAL_UNIT_ASSIGNED_CONTEXT((#73367,#73369,#73370))
REPRESENTATION_CONTEXT('','3D')
);
#73315=(
GEOMETRIC_REPRESENTATION_CONTEXT(3)
GLOBAL_UNCERTAINTY_ASSIGNED_CONTEXT((#73251))
GLOBAL_UNIT_ASSIGNED_CONTEXT((#73367,#73369,#73370))
REPRESENTATION_CONTEXT('','3D')
);
#73316=(
GEOMETRIC_REPRESENTATION_CONTEXT(3)
GLOBAL_UNCERTAINTY_ASSIGNED_CONTEXT((#73252))
GLOBAL_UNIT_ASSIGNED_CONTEXT((#73367,#73369,#73370))
REPRESENTATION_CONTEXT('','3D')
);
#73317=(
GEOMETRIC_REPRESENTATION_CONTEXT(3)
GLOBAL_UNCERTAINTY_ASSIGNED_CONTEXT((#73253))
GLOBAL_UNIT_ASSIGNED_CONTEXT((#73367,#73369,#73370))
REPRESENTATION_CONTEXT('','3D')
);
#73318=(
GEOMETRIC_REPRESENTATION_CONTEXT(3)
GLOBAL_UNCERTAINTY_ASSIGNED_CONTEXT((#73254))
GLOBAL_UNIT_ASSIGNED_CONTEXT((#73367,#73369,#73370))
REPRESENTATION_CONTEXT('','3D')
);
#73319=(
GEOMETRIC_REPRESENTATION_CONTEXT(3)
GLOBAL_UNCERTAINTY_ASSIGNED_CONTEXT((#73255))
GLOBAL_UNIT_ASSIGNED_CONTEXT((#73367,#73369,#73370))
REPRESENTATION_CONTEXT('','3D')
);
#73320=(
GEOMETRIC_REPRESENTATION_CONTEXT(3)
GLOBAL_UNCERTAINTY_ASSIGNED_CONTEXT((#73256))
GLOBAL_UNIT_ASSIGNED_CONTEXT((#73367,#73369,#73370))
REPRESENTATION_CONTEXT('','3D')
);
#73321=(
GEOMETRIC_REPRESENTATION_CONTEXT(3)
GLOBAL_UNCERTAINTY_ASSIGNED_CONTEXT((#73257))
GLOBAL_UNIT_ASSIGNED_CONTEXT((#73367,#73369,#73370))
REPRESENTATION_CONTEXT('','3D')
);
#73322=(
GEOMETRIC_REPRESENTATION_CONTEXT(3)
GLOBAL_UNCERTAINTY_ASSIGNED_CONTEXT((#73258))
GLOBAL_UNIT_ASSIGNED_CONTEXT((#73367,#73369,#73370))
REPRESENTATION_CONTEXT('','3D')
);
#73323=(
GEOMETRIC_REPRESENTATION_CONTEXT(3)
GLOBAL_UNCERTAINTY_ASSIGNED_CONTEXT((#73259))
GLOBAL_UNIT_ASSIGNED_CONTEXT((#73367,#73369,#73370))
REPRESENTATION_CONTEXT('','3D')
);
#73324=(
GEOMETRIC_REPRESENTATION_CONTEXT(3)
GLOBAL_UNCERTAINTY_ASSIGNED_CONTEXT((#73260))
GLOBAL_UNIT_ASSIGNED_CONTEXT((#73367,#73369,#73370))
REPRESENTATION_CONTEXT('','3D')
);
#73325=(
GEOMETRIC_REPRESENTATION_CONTEXT(3)
GLOBAL_UNCERTAINTY_ASSIGNED_CONTEXT((#73261))
GLOBAL_UNIT_ASSIGNED_CONTEXT((#73367,#73369,#73370))
REPRESENTATION_CONTEXT('','3D')
);
#73326=(
GEOMETRIC_REPRESENTATION_CONTEXT(3)
GLOBAL_UNCERTAINTY_ASSIGNED_CONTEXT((#73262))
GLOBAL_UNIT_ASSIGNED_CONTEXT((#73367,#73369,#73370))
REPRESENTATION_CONTEXT('','3D')
);
#73327=(
GEOMETRIC_REPRESENTATION_CONTEXT(3)
GLOBAL_UNCERTAINTY_ASSIGNED_CONTEXT((#73263))
GLOBAL_UNIT_ASSIGNED_CONTEXT((#73367,#73369,#73370))
REPRESENTATION_CONTEXT('','3D')
);
#73328=(
GEOMETRIC_REPRESENTATION_CONTEXT(3)
GLOBAL_UNCERTAINTY_ASSIGNED_CONTEXT((#73264))
GLOBAL_UNIT_ASSIGNED_CONTEXT((#73367,#73369,#73370))
REPRESENTATION_CONTEXT('','3D')
);
#73329=(
GEOMETRIC_REPRESENTATION_CONTEXT(3)
GLOBAL_UNCERTAINTY_ASSIGNED_CONTEXT((#73265))
GLOBAL_UNIT_ASSIGNED_CONTEXT((#73367,#73369,#73370))
REPRESENTATION_CONTEXT('','3D')
);
#73330=(
GEOMETRIC_REPRESENTATION_CONTEXT(3)
GLOBAL_UNCERTAINTY_ASSIGNED_CONTEXT((#73266))
GLOBAL_UNIT_ASSIGNED_CONTEXT((#73367,#73369,#73370))
REPRESENTATION_CONTEXT('','3D')
);
#73331=(
GEOMETRIC_REPRESENTATION_CONTEXT(3)
GLOBAL_UNCERTAINTY_ASSIGNED_CONTEXT((#73267))
GLOBAL_UNIT_ASSIGNED_CONTEXT((#73367,#73369,#73370))
REPRESENTATION_CONTEXT('','3D')
);
#73332=(
GEOMETRIC_REPRESENTATION_CONTEXT(3)
GLOBAL_UNCERTAINTY_ASSIGNED_CONTEXT((#73268))
GLOBAL_UNIT_ASSIGNED_CONTEXT((#73367,#73369,#73370))
REPRESENTATION_CONTEXT('','3D')
);
#73333=(
GEOMETRIC_REPRESENTATION_CONTEXT(3)
GLOBAL_UNCERTAINTY_ASSIGNED_CONTEXT((#73269))
GLOBAL_UNIT_ASSIGNED_CONTEXT((#73367,#73369,#73370))
REPRESENTATION_CONTEXT('','3D')
);
#73334=(
GEOMETRIC_REPRESENTATION_CONTEXT(3)
GLOBAL_UNCERTAINTY_ASSIGNED_CONTEXT((#73270))
GLOBAL_UNIT_ASSIGNED_CONTEXT((#73367,#73369,#73370))
REPRESENTATION_CONTEXT('','3D')
);
#73335=(
GEOMETRIC_REPRESENTATION_CONTEXT(3)
GLOBAL_UNCERTAINTY_ASSIGNED_CONTEXT((#73271))
GLOBAL_UNIT_ASSIGNED_CONTEXT((#73367,#73369,#73370))
REPRESENTATION_CONTEXT('','3D')
);
#73336=(
GEOMETRIC_REPRESENTATION_CONTEXT(3)
GLOBAL_UNCERTAINTY_ASSIGNED_CONTEXT((#73272))
GLOBAL_UNIT_ASSIGNED_CONTEXT((#73367,#73369,#73370))
REPRESENTATION_CONTEXT('','3D')
);
#73337=(
GEOMETRIC_REPRESENTATION_CONTEXT(3)
GLOBAL_UNCERTAINTY_ASSIGNED_CONTEXT((#73273))
GLOBAL_UNIT_ASSIGNED_CONTEXT((#73367,#73369,#73370))
REPRESENTATION_CONTEXT('','3D')
);
#73338=(
GEOMETRIC_REPRESENTATION_CONTEXT(3)
GLOBAL_UNCERTAINTY_ASSIGNED_CONTEXT((#73274))
GLOBAL_UNIT_ASSIGNED_CONTEXT((#73367,#73369,#73370))
REPRESENTATION_CONTEXT('','3D')
);
#73339=(
GEOMETRIC_REPRESENTATION_CONTEXT(3)
GLOBAL_UNCERTAINTY_ASSIGNED_CONTEXT((#73275))
GLOBAL_UNIT_ASSIGNED_CONTEXT((#73367,#73369,#73370))
REPRESENTATION_CONTEXT('','3D')
);
#73340=(
GEOMETRIC_REPRESENTATION_CONTEXT(3)
GLOBAL_UNCERTAINTY_ASSIGNED_CONTEXT((#73276))
GLOBAL_UNIT_ASSIGNED_CONTEXT((#73367,#73369,#73370))
REPRESENTATION_CONTEXT('','3D')
);
#73341=(
GEOMETRIC_REPRESENTATION_CONTEXT(3)
GLOBAL_UNCERTAINTY_ASSIGNED_CONTEXT((#73277))
GLOBAL_UNIT_ASSIGNED_CONTEXT((#73367,#73369,#73370))
REPRESENTATION_CONTEXT('','3D')
);
#73342=(
GEOMETRIC_REPRESENTATION_CONTEXT(3)
GLOBAL_UNCERTAINTY_ASSIGNED_CONTEXT((#73278))
GLOBAL_UNIT_ASSIGNED_CONTEXT((#73367,#73369,#73370))
REPRESENTATION_CONTEXT('','3D')
);
#73343=(
GEOMETRIC_REPRESENTATION_CONTEXT(3)
GLOBAL_UNCERTAINTY_ASSIGNED_CONTEXT((#73279))
GLOBAL_UNIT_ASSIGNED_CONTEXT((#73367,#73369,#73370))
REPRESENTATION_CONTEXT('','3D')
);
#73344=(
GEOMETRIC_REPRESENTATION_CONTEXT(3)
GLOBAL_UNCERTAINTY_ASSIGNED_CONTEXT((#73280))
GLOBAL_UNIT_ASSIGNED_CONTEXT((#73367,#73369,#73370))
REPRESENTATION_CONTEXT('','3D')
);
#73345=(
GEOMETRIC_REPRESENTATION_CONTEXT(3)
GLOBAL_UNCERTAINTY_ASSIGNED_CONTEXT((#73281))
GLOBAL_UNIT_ASSIGNED_CONTEXT((#73367,#73369,#73370))
REPRESENTATION_CONTEXT('','3D')
);
#73346=(
GEOMETRIC_REPRESENTATION_CONTEXT(3)
GLOBAL_UNCERTAINTY_ASSIGNED_CONTEXT((#73282))
GLOBAL_UNIT_ASSIGNED_CONTEXT((#73367,#73369,#73370))
REPRESENTATION_CONTEXT('','3D')
);
#73347=(
GEOMETRIC_REPRESENTATION_CONTEXT(3)
GLOBAL_UNCERTAINTY_ASSIGNED_CONTEXT((#73283))
GLOBAL_UNIT_ASSIGNED_CONTEXT((#73367,#73369,#73370))
REPRESENTATION_CONTEXT('','3D')
);
#73348=(
GEOMETRIC_REPRESENTATION_CONTEXT(3)
GLOBAL_UNCERTAINTY_ASSIGNED_CONTEXT((#73284))
GLOBAL_UNIT_ASSIGNED_CONTEXT((#73367,#73369,#73370))
REPRESENTATION_CONTEXT('','3D')
);
#73349=(
GEOMETRIC_REPRESENTATION_CONTEXT(3)
GLOBAL_UNCERTAINTY_ASSIGNED_CONTEXT((#73285))
GLOBAL_UNIT_ASSIGNED_CONTEXT((#73367,#73369,#73370))
REPRESENTATION_CONTEXT('','3D')
);
#73350=(
GEOMETRIC_REPRESENTATION_CONTEXT(3)
GLOBAL_UNCERTAINTY_ASSIGNED_CONTEXT((#73286))
GLOBAL_UNIT_ASSIGNED_CONTEXT((#73367,#73369,#73370))
REPRESENTATION_CONTEXT('','3D')
);
#73351=(
GEOMETRIC_REPRESENTATION_CONTEXT(3)
GLOBAL_UNCERTAINTY_ASSIGNED_CONTEXT((#73287))
GLOBAL_UNIT_ASSIGNED_CONTEXT((#73367,#73369,#73370))
REPRESENTATION_CONTEXT('','3D')
);
#73352=(
GEOMETRIC_REPRESENTATION_CONTEXT(3)
GLOBAL_UNCERTAINTY_ASSIGNED_CONTEXT((#73288))
GLOBAL_UNIT_ASSIGNED_CONTEXT((#73367,#73369,#73370))
REPRESENTATION_CONTEXT('','3D')
);
#73353=(
GEOMETRIC_REPRESENTATION_CONTEXT(3)
GLOBAL_UNCERTAINTY_ASSIGNED_CONTEXT((#73289))
GLOBAL_UNIT_ASSIGNED_CONTEXT((#73367,#73369,#73370))
REPRESENTATION_CONTEXT('','3D')
);
#73354=(
GEOMETRIC_REPRESENTATION_CONTEXT(3)
GLOBAL_UNCERTAINTY_ASSIGNED_CONTEXT((#73290))
GLOBAL_UNIT_ASSIGNED_CONTEXT((#73367,#73369,#73370))
REPRESENTATION_CONTEXT('','3D')
);
#73355=(
GEOMETRIC_REPRESENTATION_CONTEXT(3)
GLOBAL_UNCERTAINTY_ASSIGNED_CONTEXT((#73291))
GLOBAL_UNIT_ASSIGNED_CONTEXT((#73367,#73369,#73370))
REPRESENTATION_CONTEXT('','3D')
);
#73356=(
GEOMETRIC_REPRESENTATION_CONTEXT(3)
GLOBAL_UNCERTAINTY_ASSIGNED_CONTEXT((#73292))
GLOBAL_UNIT_ASSIGNED_CONTEXT((#73367,#73369,#73370))
REPRESENTATION_CONTEXT('','3D')
);
#73357=(
GEOMETRIC_REPRESENTATION_CONTEXT(3)
GLOBAL_UNCERTAINTY_ASSIGNED_CONTEXT((#73293))
GLOBAL_UNIT_ASSIGNED_CONTEXT((#73367,#73369,#73370))
REPRESENTATION_CONTEXT('','3D')
);
#73358=(
GEOMETRIC_REPRESENTATION_CONTEXT(3)
GLOBAL_UNCERTAINTY_ASSIGNED_CONTEXT((#73294))
GLOBAL_UNIT_ASSIGNED_CONTEXT((#73367,#73369,#73370))
REPRESENTATION_CONTEXT('','3D')
);
#73359=(
GEOMETRIC_REPRESENTATION_CONTEXT(3)
GLOBAL_UNCERTAINTY_ASSIGNED_CONTEXT((#73295))
GLOBAL_UNIT_ASSIGNED_CONTEXT((#73367,#73369,#73370))
REPRESENTATION_CONTEXT('','3D')
);
#73360=(
GEOMETRIC_REPRESENTATION_CONTEXT(3)
GLOBAL_UNCERTAINTY_ASSIGNED_CONTEXT((#73296))
GLOBAL_UNIT_ASSIGNED_CONTEXT((#73367,#73369,#73370))
REPRESENTATION_CONTEXT('','3D')
);
#73361=(
GEOMETRIC_REPRESENTATION_CONTEXT(3)
GLOBAL_UNCERTAINTY_ASSIGNED_CONTEXT((#73297))
GLOBAL_UNIT_ASSIGNED_CONTEXT((#73367,#73369,#73370))
REPRESENTATION_CONTEXT('','3D')
);
#73362=(
GEOMETRIC_REPRESENTATION_CONTEXT(3)
GLOBAL_UNCERTAINTY_ASSIGNED_CONTEXT((#73298))
GLOBAL_UNIT_ASSIGNED_CONTEXT((#73367,#73369,#73370))
REPRESENTATION_CONTEXT('','3D')
);
#73363=(
GEOMETRIC_REPRESENTATION_CONTEXT(3)
GLOBAL_UNCERTAINTY_ASSIGNED_CONTEXT((#73299))
GLOBAL_UNIT_ASSIGNED_CONTEXT((#73367,#73369,#73370))
REPRESENTATION_CONTEXT('','3D')
);
#73364=(
GEOMETRIC_REPRESENTATION_CONTEXT(3)
GLOBAL_UNCERTAINTY_ASSIGNED_CONTEXT((#73300))
GLOBAL_UNIT_ASSIGNED_CONTEXT((#73367,#73369,#73370))
REPRESENTATION_CONTEXT('','3D')
);
#73365=(
GEOMETRIC_REPRESENTATION_CONTEXT(3)
GLOBAL_UNCERTAINTY_ASSIGNED_CONTEXT((#73301))
GLOBAL_UNIT_ASSIGNED_CONTEXT((#73367,#73369,#73370))
REPRESENTATION_CONTEXT('','3D')
);
#73366=(
GEOMETRIC_REPRESENTATION_CONTEXT(3)
GLOBAL_UNCERTAINTY_ASSIGNED_CONTEXT((#73302))
GLOBAL_UNIT_ASSIGNED_CONTEXT((#73367,#73369,#73370))
REPRESENTATION_CONTEXT('','3D')
);
#73367=(
LENGTH_UNIT()
NAMED_UNIT(*)
SI_UNIT(.CENTI.,.METRE.)
);
#73368=(
LENGTH_UNIT()
NAMED_UNIT(*)
SI_UNIT($,.METRE.)
);
#73369=(
NAMED_UNIT(*)
PLANE_ANGLE_UNIT()
SI_UNIT($,.RADIAN.)
);
#73370=(
NAMED_UNIT(*)
SI_UNIT($,.STERADIAN.)
SOLID_ANGLE_UNIT()
);
#73371=SHAPE_DEFINITION_REPRESENTATION(#73434,#73607);
#73372=SHAPE_DEFINITION_REPRESENTATION(#73435,#73608);
#73373=SHAPE_DEFINITION_REPRESENTATION(#73436,#73609);
#73374=SHAPE_DEFINITION_REPRESENTATION(#73437,#73610);
#73375=SHAPE_DEFINITION_REPRESENTATION(#73438,#73611);
#73376=SHAPE_DEFINITION_REPRESENTATION(#73439,#73612);
#73377=SHAPE_DEFINITION_REPRESENTATION(#73440,#73613);
#73378=SHAPE_DEFINITION_REPRESENTATION(#73441,#73614);
#73379=SHAPE_DEFINITION_REPRESENTATION(#73442,#73615);
#73380=SHAPE_DEFINITION_REPRESENTATION(#73443,#73616);
#73381=SHAPE_DEFINITION_REPRESENTATION(#73444,#73617);
#73382=SHAPE_DEFINITION_REPRESENTATION(#73445,#73618);
#73383=SHAPE_DEFINITION_REPRESENTATION(#73446,#73619);
#73384=SHAPE_DEFINITION_REPRESENTATION(#73447,#73620);
#73385=SHAPE_DEFINITION_REPRESENTATION(#73448,#73621);
#73386=SHAPE_DEFINITION_REPRESENTATION(#73449,#73622);
#73387=SHAPE_DEFINITION_REPRESENTATION(#73450,#73623);
#73388=SHAPE_DEFINITION_REPRESENTATION(#73451,#73624);
#73389=SHAPE_DEFINITION_REPRESENTATION(#73452,#73625);
#73390=SHAPE_DEFINITION_REPRESENTATION(#73453,#73626);
#73391=SHAPE_DEFINITION_REPRESENTATION(#73454,#73627);
#73392=SHAPE_DEFINITION_REPRESENTATION(#73455,#73628);
#73393=SHAPE_DEFINITION_REPRESENTATION(#73456,#73629);
#73394=SHAPE_DEFINITION_REPRESENTATION(#73457,#73630);
#73395=SHAPE_DEFINITION_REPRESENTATION(#73458,#73631);
#73396=SHAPE_DEFINITION_REPRESENTATION(#73464,#73632);
#73397=SHAPE_DEFINITION_REPRESENTATION(#73465,#73633);
#73398=SHAPE_DEFINITION_REPRESENTATION(#73466,#73634);
#73399=SHAPE_DEFINITION_REPRESENTATION(#73467,#73635);
#73400=SHAPE_DEFINITION_REPRESENTATION(#73468,#73636);
#73401=SHAPE_DEFINITION_REPRESENTATION(#73469,#73637);
#73402=SHAPE_DEFINITION_REPRESENTATION(#73475,#73638);
#73403=SHAPE_DEFINITION_REPRESENTATION(#73536,#73639);
#73404=SHAPE_DEFINITION_REPRESENTATION(#73537,#73640);
#73405=SHAPE_DEFINITION_REPRESENTATION(#73538,#73641);
#73406=SHAPE_DEFINITION_REPRESENTATION(#73539,#73642);
#73407=SHAPE_DEFINITION_REPRESENTATION(#73540,#73643);
#73408=SHAPE_DEFINITION_REPRESENTATION(#73541,#73644);
#73409=SHAPE_DEFINITION_REPRESENTATION(#73542,#73645);
#73410=SHAPE_DEFINITION_REPRESENTATION(#73543,#73646);
#73411=SHAPE_DEFINITION_REPRESENTATION(#73544,#73647);
#73412=SHAPE_DEFINITION_REPRESENTATION(#73545,#73648);
#73413=SHAPE_DEFINITION_REPRESENTATION(#73546,#73649);
#73414=SHAPE_DEFINITION_REPRESENTATION(#73547,#73650);
#73415=SHAPE_DEFINITION_REPRESENTATION(#73548,#73651);
#73416=SHAPE_DEFINITION_REPRESENTATION(#73549,#73652);
#73417=SHAPE_DEFINITION_REPRESENTATION(#73550,#73653);
#73418=SHAPE_DEFINITION_REPRESENTATION(#73551,#73654);
#73419=SHAPE_DEFINITION_REPRESENTATION(#73552,#73655);
#73420=SHAPE_DEFINITION_REPRESENTATION(#73553,#73656);
#73421=SHAPE_DEFINITION_REPRESENTATION(#73554,#73657);
#73422=SHAPE_DEFINITION_REPRESENTATION(#73555,#73658);
#73423=SHAPE_DEFINITION_REPRESENTATION(#73556,#73659);
#73424=SHAPE_DEFINITION_REPRESENTATION(#73557,#73660);
#73425=SHAPE_DEFINITION_REPRESENTATION(#73558,#73661);
#73426=SHAPE_DEFINITION_REPRESENTATION(#73559,#73662);
#73427=SHAPE_DEFINITION_REPRESENTATION(#73560,#73663);
#73428=SHAPE_DEFINITION_REPRESENTATION(#73561,#73664);
#73429=SHAPE_DEFINITION_REPRESENTATION(#73562,#73665);
#73430=SHAPE_DEFINITION_REPRESENTATION(#73563,#73666);
#73431=SHAPE_DEFINITION_REPRESENTATION(#73564,#73667);
#73432=SHAPE_DEFINITION_REPRESENTATION(#73576,#73668);
#73433=SHAPE_DEFINITION_REPRESENTATION(#73577,#73669);
#73434=PRODUCT_DEFINITION_SHAPE('',$,#73671);
#73435=PRODUCT_DEFINITION_SHAPE('',$,#73672);
#73436=PRODUCT_DEFINITION_SHAPE('',$,#73673);
#73437=PRODUCT_DEFINITION_SHAPE('',$,#73674);
#73438=PRODUCT_DEFINITION_SHAPE('',$,#73675);
#73439=PRODUCT_DEFINITION_SHAPE('',$,#73676);
#73440=PRODUCT_DEFINITION_SHAPE('',$,#73677);
#73441=PRODUCT_DEFINITION_SHAPE('',$,#73678);
#73442=PRODUCT_DEFINITION_SHAPE('',$,#73679);
#73443=PRODUCT_DEFINITION_SHAPE('',$,#73680);
#73444=PRODUCT_DEFINITION_SHAPE('',$,#73681);
#73445=PRODUCT_DEFINITION_SHAPE('',$,#73682);
#73446=PRODUCT_DEFINITION_SHAPE('',$,#73683);
#73447=PRODUCT_DEFINITION_SHAPE('',$,#73684);
#73448=PRODUCT_DEFINITION_SHAPE('',$,#73685);
#73449=PRODUCT_DEFINITION_SHAPE('',$,#73686);
#73450=PRODUCT_DEFINITION_SHAPE('',$,#73687);
#73451=PRODUCT_DEFINITION_SHAPE('',$,#73688);
#73452=PRODUCT_DEFINITION_SHAPE('',$,#73689);
#73453=PRODUCT_DEFINITION_SHAPE('',$,#73690);
#73454=PRODUCT_DEFINITION_SHAPE('',$,#73691);
#73455=PRODUCT_DEFINITION_SHAPE('',$,#73692);
#73456=PRODUCT_DEFINITION_SHAPE('',$,#73693);
#73457=PRODUCT_DEFINITION_SHAPE('',$,#73694);
#73458=PRODUCT_DEFINITION_SHAPE('',$,#73695);
#73459=PRODUCT_DEFINITION_SHAPE($,$,#821);
#73460=PRODUCT_DEFINITION_SHAPE($,$,#822);
#73461=PRODUCT_DEFINITION_SHAPE($,$,#823);
#73462=PRODUCT_DEFINITION_SHAPE($,$,#824);
#73463=PRODUCT_DEFINITION_SHAPE($,$,#825);
#73464=PRODUCT_DEFINITION_SHAPE('',$,#73696);
#73465=PRODUCT_DEFINITION_SHAPE('',$,#73697);
#73466=PRODUCT_DEFINITION_SHAPE('',$,#73698);
#73467=PRODUCT_DEFINITION_SHAPE('',$,#73699);
#73468=PRODUCT_DEFINITION_SHAPE('',$,#73700);
#73469=PRODUCT_DEFINITION_SHAPE('',$,#73701);
#73470=PRODUCT_DEFINITION_SHAPE($,$,#826);
#73471=PRODUCT_DEFINITION_SHAPE($,$,#827);
#73472=PRODUCT_DEFINITION_SHAPE($,$,#828);
#73473=PRODUCT_DEFINITION_SHAPE($,$,#829);
#73474=PRODUCT_DEFINITION_SHAPE($,$,#830);
#73475=PRODUCT_DEFINITION_SHAPE('',$,#73702);
#73476=PRODUCT_DEFINITION_SHAPE($,$,#831);
#73477=PRODUCT_DEFINITION_SHAPE($,$,#832);
#73478=PRODUCT_DEFINITION_SHAPE($,$,#833);
#73479=PRODUCT_DEFINITION_SHAPE($,$,#834);
#73480=PRODUCT_DEFINITION_SHAPE($,$,#835);
#73481=PRODUCT_DEFINITION_SHAPE($,$,#836);
#73482=PRODUCT_DEFINITION_SHAPE($,$,#837);
#73483=PRODUCT_DEFINITION_SHAPE($,$,#838);
#73484=PRODUCT_DEFINITION_SHAPE($,$,#839);
#73485=PRODUCT_DEFINITION_SHAPE($,$,#840);
#73486=PRODUCT_DEFINITION_SHAPE($,$,#841);
#73487=PRODUCT_DEFINITION_SHAPE($,$,#842);
#73488=PRODUCT_DEFINITION_SHAPE($,$,#843);
#73489=PRODUCT_DEFINITION_SHAPE($,$,#844);
#73490=PRODUCT_DEFINITION_SHAPE($,$,#845);
#73491=PRODUCT_DEFINITION_SHAPE($,$,#846);
#73492=PRODUCT_DEFINITION_SHAPE($,$,#847);
#73493=PRODUCT_DEFINITION_SHAPE($,$,#848);
#73494=PRODUCT_DEFINITION_SHAPE($,$,#849);
#73495=PRODUCT_DEFINITION_SHAPE($,$,#850);
#73496=PRODUCT_DEFINITION_SHAPE($,$,#851);
#73497=PRODUCT_DEFINITION_SHAPE($,$,#852);
#73498=PRODUCT_DEFINITION_SHAPE($,$,#853);
#73499=PRODUCT_DEFINITION_SHAPE($,$,#854);
#73500=PRODUCT_DEFINITION_SHAPE($,$,#855);
#73501=PRODUCT_DEFINITION_SHAPE($,$,#856);
#73502=PRODUCT_DEFINITION_SHAPE($,$,#857);
#73503=PRODUCT_DEFINITION_SHAPE($,$,#858);
#73504=PRODUCT_DEFINITION_SHAPE($,$,#859);
#73505=PRODUCT_DEFINITION_SHAPE($,$,#860);
#73506=PRODUCT_DEFINITION_SHAPE($,$,#861);
#73507=PRODUCT_DEFINITION_SHAPE($,$,#862);
#73508=PRODUCT_DEFINITION_SHAPE($,$,#863);
#73509=PRODUCT_DEFINITION_SHAPE($,$,#864);
#73510=PRODUCT_DEFINITION_SHAPE($,$,#865);
#73511=PRODUCT_DEFINITION_SHAPE($,$,#866);
#73512=PRODUCT_DEFINITION_SHAPE($,$,#867);
#73513=PRODUCT_DEFINITION_SHAPE($,$,#868);
#73514=PRODUCT_DEFINITION_SHAPE($,$,#869);
#73515=PRODUCT_DEFINITION_SHAPE($,$,#870);
#73516=PRODUCT_DEFINITION_SHAPE($,$,#871);
#73517=PRODUCT_DEFINITION_SHAPE($,$,#872);
#73518=PRODUCT_DEFINITION_SHAPE($,$,#873);
#73519=PRODUCT_DEFINITION_SHAPE($,$,#874);
#73520=PRODUCT_DEFINITION_SHAPE($,$,#875);
#73521=PRODUCT_DEFINITION_SHAPE($,$,#876);
#73522=PRODUCT_DEFINITION_SHAPE($,$,#877);
#73523=PRODUCT_DEFINITION_SHAPE($,$,#878);
#73524=PRODUCT_DEFINITION_SHAPE($,$,#879);
#73525=PRODUCT_DEFINITION_SHAPE($,$,#880);
#73526=PRODUCT_DEFINITION_SHAPE($,$,#881);
#73527=PRODUCT_DEFINITION_SHAPE($,$,#882);
#73528=PRODUCT_DEFINITION_SHAPE($,$,#883);
#73529=PRODUCT_DEFINITION_SHAPE($,$,#884);
#73530=PRODUCT_DEFINITION_SHAPE($,$,#885);
#73531=PRODUCT_DEFINITION_SHAPE($,$,#886);
#73532=PRODUCT_DEFINITION_SHAPE($,$,#887);
#73533=PRODUCT_DEFINITION_SHAPE($,$,#888);
#73534=PRODUCT_DEFINITION_SHAPE($,$,#889);
#73535=PRODUCT_DEFINITION_SHAPE($,$,#890);
#73536=PRODUCT_DEFINITION_SHAPE('',$,#73703);
#73537=PRODUCT_DEFINITION_SHAPE('',$,#73704);
#73538=PRODUCT_DEFINITION_SHAPE('',$,#73705);
#73539=PRODUCT_DEFINITION_SHAPE('',$,#73706);
#73540=PRODUCT_DEFINITION_SHAPE('',$,#73707);
#73541=PRODUCT_DEFINITION_SHAPE('',$,#73708);
#73542=PRODUCT_DEFINITION_SHAPE('',$,#73709);
#73543=PRODUCT_DEFINITION_SHAPE('',$,#73710);
#73544=PRODUCT_DEFINITION_SHAPE('',$,#73711);
#73545=PRODUCT_DEFINITION_SHAPE('',$,#73712);
#73546=PRODUCT_DEFINITION_SHAPE('',$,#73713);
#73547=PRODUCT_DEFINITION_SHAPE('',$,#73714);
#73548=PRODUCT_DEFINITION_SHAPE('',$,#73715);
#73549=PRODUCT_DEFINITION_SHAPE('',$,#73716);
#73550=PRODUCT_DEFINITION_SHAPE('',$,#73717);
#73551=PRODUCT_DEFINITION_SHAPE('',$,#73718);
#73552=PRODUCT_DEFINITION_SHAPE('',$,#73719);
#73553=PRODUCT_DEFINITION_SHAPE('',$,#73720);
#73554=PRODUCT_DEFINITION_SHAPE('',$,#73721);
#73555=PRODUCT_DEFINITION_SHAPE('',$,#73722);
#73556=PRODUCT_DEFINITION_SHAPE('',$,#73723);
#73557=PRODUCT_DEFINITION_SHAPE('',$,#73724);
#73558=PRODUCT_DEFINITION_SHAPE('',$,#73725);
#73559=PRODUCT_DEFINITION_SHAPE('',$,#73726);
#73560=PRODUCT_DEFINITION_SHAPE('',$,#73727);
#73561=PRODUCT_DEFINITION_SHAPE('',$,#73728);
#73562=PRODUCT_DEFINITION_SHAPE('',$,#73729);
#73563=PRODUCT_DEFINITION_SHAPE('',$,#73730);
#73564=PRODUCT_DEFINITION_SHAPE('',$,#73731);
#73565=PRODUCT_DEFINITION_SHAPE($,$,#891);
#73566=PRODUCT_DEFINITION_SHAPE($,$,#892);
#73567=PRODUCT_DEFINITION_SHAPE($,$,#893);
#73568=PRODUCT_DEFINITION_SHAPE($,$,#894);
#73569=PRODUCT_DEFINITION_SHAPE($,$,#895);
#73570=PRODUCT_DEFINITION_SHAPE($,$,#896);
#73571=PRODUCT_DEFINITION_SHAPE($,$,#897);
#73572=PRODUCT_DEFINITION_SHAPE($,$,#898);
#73573=PRODUCT_DEFINITION_SHAPE($,$,#899);
#73574=PRODUCT_DEFINITION_SHAPE($,$,#900);
#73575=PRODUCT_DEFINITION_SHAPE($,$,#901);
#73576=PRODUCT_DEFINITION_SHAPE('',$,#73732);
#73577=PRODUCT_DEFINITION_SHAPE('',$,#73733);
#73578=PRODUCT_DEFINITION_SHAPE($,$,#902);
#73579=PRODUCT_DEFINITION_SHAPE($,$,#903);
#73580=PRODUCT_DEFINITION_SHAPE($,$,#904);
#73581=PRODUCT_DEFINITION_SHAPE($,$,#905);
#73582=PRODUCT_DEFINITION_SHAPE($,$,#906);
#73583=PRODUCT_DEFINITION_SHAPE($,$,#907);
#73584=PRODUCT_DEFINITION_SHAPE($,$,#908);
#73585=PRODUCT_DEFINITION_SHAPE($,$,#909);
#73586=PRODUCT_DEFINITION_SHAPE($,$,#910);
#73587=PRODUCT_DEFINITION_SHAPE($,$,#911);
#73588=PRODUCT_DEFINITION_SHAPE($,$,#912);
#73589=PRODUCT_DEFINITION_SHAPE($,$,#913);
#73590=PRODUCT_DEFINITION_SHAPE($,$,#914);
#73591=PRODUCT_DEFINITION_SHAPE($,$,#915);
#73592=PRODUCT_DEFINITION_SHAPE($,$,#916);
#73593=PRODUCT_DEFINITION_SHAPE($,$,#917);
#73594=PRODUCT_DEFINITION_SHAPE($,$,#918);
#73595=PRODUCT_DEFINITION_SHAPE($,$,#919);
#73596=PRODUCT_DEFINITION_SHAPE($,$,#920);
#73597=PRODUCT_DEFINITION_SHAPE($,$,#921);
#73598=PRODUCT_DEFINITION_SHAPE($,$,#922);
#73599=PRODUCT_DEFINITION_SHAPE($,$,#923);
#73600=PRODUCT_DEFINITION_SHAPE($,$,#924);
#73601=PRODUCT_DEFINITION_SHAPE($,$,#925);
#73602=PRODUCT_DEFINITION_SHAPE($,$,#926);
#73603=PRODUCT_DEFINITION_SHAPE($,$,#927);
#73604=PRODUCT_DEFINITION_SHAPE($,$,#928);
#73605=PRODUCT_DEFINITION_SHAPE($,$,#929);
#73606=PRODUCT_DEFINITION_SHAPE($,$,#930);
#73607=SHAPE_REPRESENTATION('',(#16812,#18454,#18455,#18456,#18457),#73303);
#73608=SHAPE_REPRESENTATION('',(#16813,#17704,#17705,#17706,#17707,#17708,
#17709,#17710,#17711,#17712,#17713,#17714,#17715,#17716,#17717,#17718,#17719,
#17720,#17721,#17722,#17723,#17724,#17725,#17726,#17727,#17728,#17729,#17730,
#17731,#17732,#17733,#17734,#17735,#17736,#17737,#17738,#17739,#17740,#17741,
#17742,#17743,#17744,#17745,#17746,#17747,#17748,#17749,#17750,#17751,#17752,
#17753,#17754,#17755,#17756,#17757,#17758,#17759,#17760,#17761,#17762,#17763),
#73304);
#73609=SHAPE_REPRESENTATION('',(#16814),#73305);
#73610=SHAPE_REPRESENTATION('',(#16833),#73306);
#73611=SHAPE_REPRESENTATION('',(#17006),#73307);
#73612=SHAPE_REPRESENTATION('',(#17167),#73308);
#73613=SHAPE_REPRESENTATION('',(#17173),#73309);
#73614=SHAPE_REPRESENTATION('',(#17179),#73310);
#73615=SHAPE_REPRESENTATION('',(#17185),#73311);
#73616=SHAPE_REPRESENTATION('',(#17191),#73312);
#73617=SHAPE_REPRESENTATION('',(#17225),#73313);
#73618=SHAPE_REPRESENTATION('',(#17259),#73314);
#73619=SHAPE_REPRESENTATION('',(#17284),#73315);
#73620=SHAPE_REPRESENTATION('',(#17309),#73316);
#73621=SHAPE_REPRESENTATION('',(#17334),#73317);
#73622=SHAPE_REPRESENTATION('',(#17359),#73318);
#73623=SHAPE_REPRESENTATION('',(#17378),#73319);
#73624=SHAPE_REPRESENTATION('',(#17385),#73320);
#73625=SHAPE_REPRESENTATION('',(#17392),#73321);
#73626=SHAPE_REPRESENTATION('',(#17416,#17539,#17540,#17541,#17542,#17543),
#73322);
#73627=SHAPE_REPRESENTATION('',(#17417),#73323);
#73628=SHAPE_REPRESENTATION('',(#17437),#73324);
#73629=SHAPE_REPRESENTATION('',(#17457),#73325);
#73630=SHAPE_REPRESENTATION('',(#17472),#73326);
#73631=SHAPE_REPRESENTATION('',(#17522),#73327);
#73632=SHAPE_REPRESENTATION('',(#17544,#17673,#17674,#17675,#17676,#17677),
#73328);
#73633=SHAPE_REPRESENTATION('',(#17545),#73329);
#73634=SHAPE_REPRESENTATION('',(#17565),#73330);
#73635=SHAPE_REPRESENTATION('',(#17585),#73331);
#73636=SHAPE_REPRESENTATION('',(#17602),#73332);
#73637=SHAPE_REPRESENTATION('',(#17656),#73333);
#73638=SHAPE_REPRESENTATION('',(#17678),#73334);
#73639=SHAPE_REPRESENTATION('',(#17764,#18234,#18235,#18236,#18237,#18238,
#18239,#18240,#18241,#18242,#18243,#18244),#73335);
#73640=SHAPE_REPRESENTATION('',(#17765),#73336);
#73641=SHAPE_REPRESENTATION('',(#17778),#73337);
#73642=SHAPE_REPRESENTATION('',(#17793),#73338);
#73643=SHAPE_REPRESENTATION('',(#17808),#73339);
#73644=SHAPE_REPRESENTATION('',(#17817),#73340);
#73645=SHAPE_REPRESENTATION('',(#17826),#73341);
#73646=SHAPE_REPRESENTATION('',(#17835),#73342);
#73647=SHAPE_REPRESENTATION('',(#17844),#73343);
#73648=SHAPE_REPRESENTATION('',(#17937),#73344);
#73649=SHAPE_REPRESENTATION('',(#17948,#18429,#18430,#18431,#18432,#18433,
#18434,#18435,#18436,#18437,#18438,#18439,#18440,#18441,#18442),#73345);
#73650=SHAPE_REPRESENTATION('',(#17949),#73346);
#73651=SHAPE_REPRESENTATION('',(#17969),#73347);
#73652=SHAPE_REPRESENTATION('',(#17984),#73348);
#73653=SHAPE_REPRESENTATION('',(#17999),#73349);
#73654=SHAPE_REPRESENTATION('',(#18008),#73350);
#73655=SHAPE_REPRESENTATION('',(#18017),#73351);
#73656=SHAPE_REPRESENTATION('',(#18026),#73352);
#73657=SHAPE_REPRESENTATION('',(#18035),#73353);
#73658=SHAPE_REPRESENTATION('',(#18044),#73354);
#73659=SHAPE_REPRESENTATION('',(#18137,#18443,#18444,#18445,#18446,#18447,
#18448,#18449,#18450,#18451,#18452,#18453),#73355);
#73660=SHAPE_REPRESENTATION('',(#18138),#73356);
#73661=SHAPE_REPRESENTATION('',(#18151),#73357);
#73662=SHAPE_REPRESENTATION('',(#18166),#73358);
#73663=SHAPE_REPRESENTATION('',(#18181),#73359);
#73664=SHAPE_REPRESENTATION('',(#18190),#73360);
#73665=SHAPE_REPRESENTATION('',(#18199),#73361);
#73666=SHAPE_REPRESENTATION('',(#18208),#73362);
#73667=SHAPE_REPRESENTATION('',(#18217),#73363);
#73668=SHAPE_REPRESENTATION('',(#18245),#73364);
#73669=SHAPE_REPRESENTATION('',(#18418),#73365);
#73670=PRODUCT_DEFINITION_CONTEXT('part definition',#73861,'design');
#73671=PRODUCT_DEFINITION('PAT-114',
'PAT-114',#73734,#73670);
#73672=PRODUCT_DEFINITION('Split housing','Split housing',#73735,#73670);
#73673=PRODUCT_DEFINITION('Base','Base',#73736,#73670);
#73674=PRODUCT_DEFINITION('Lower housing','Lower housing',#73737,#73670);
#73675=PRODUCT_DEFINITION('Upper housing','Upper housing',#73738,#73670);
#73676=PRODUCT_DEFINITION('Split dowel','Split dowel',#73739,#73670);
#73677=PRODUCT_DEFINITION('Split dowel (1)','Split dowel (1)',#73740,#73670);
#73678=PRODUCT_DEFINITION('Split dowel (2)','Split dowel (2)',#73741,#73670);
#73679=PRODUCT_DEFINITION('Split dowel (3)','Split dowel (3)',#73742,#73670);
#73680=PRODUCT_DEFINITION('mm end cap','mm end cap',#73743,#73670);
#73681=PRODUCT_DEFINITION('mm end cap (1)','mm end cap (1)',#73744,#73670);
#73682=PRODUCT_DEFINITION('mm end cap (2)','mm end cap (2)',#73745,#73670);
#73683=PRODUCT_DEFINITION('mm end cap (3)','mm end cap (3)',#73746,#73670);
#73684=PRODUCT_DEFINITION('mm end cap (4)','mm end cap (4)',#73747,#73670);
#73685=PRODUCT_DEFINITION('mm end cap (5)','mm end cap (5)',#73748,#73670);
#73686=PRODUCT_DEFINITION('Inspection cover','Inspection cover',#73749,
#73670);
#73687=PRODUCT_DEFINITION('Foot strip','Foot strip',#73750,#73670);
#73688=PRODUCT_DEFINITION('Foot strip (1)','Foot strip (1)',#73751,#73670);
#73689=PRODUCT_DEFINITION('M6x18 mounting screw','M6x18 mounting screw',
#73752,#73670);
#73690=PRODUCT_DEFINITION('Sealed Ball Bearing - 12 x 32 x 10 mm',
'Sealed Ball Bearing - 12 x 32 x 10 mm',#73753,#73670);
#73691=PRODUCT_DEFINITION('Inner ring','Inner ring',#73754,#73670);
#73692=PRODUCT_DEFINITION('Outer ring','Outer ring',#73755,#73670);
#73693=PRODUCT_DEFINITION('Balls','Balls',#73756,#73670);
#73694=PRODUCT_DEFINITION('Cage','Cage',#73757,#73670);
#73695=PRODUCT_DEFINITION('Seals 2RS','Seals 2RS',#73758,#73670);
#73696=PRODUCT_DEFINITION('Sealed Ball Bearing - 20 x 47 x 14 mm',
'Sealed Ball Bearing - 20 x 47 x 14 mm',#73759,#73670);
#73697=PRODUCT_DEFINITION('Inner ring (1)','Inner ring (1)',#73760,#73670);
#73698=PRODUCT_DEFINITION('Outer ring (1)','Outer ring (1)',#73761,#73670);
#73699=PRODUCT_DEFINITION('Balls (1)','Balls (1)',#73762,#73670);
#73700=PRODUCT_DEFINITION('Cage (1)','Cage (1)',#73763,#73670);
#73701=PRODUCT_DEFINITION('Seals 2RS (1)','Seals 2RS (1)',#73764,#73670);
#73702=PRODUCT_DEFINITION('Cap Screw - M4x16','Cap Screw - M4x16',#73765,
#73670);
#73703=PRODUCT_DEFINITION('Input rotor','Input rotor',#73766,#73670);
#73704=PRODUCT_DEFINITION('Shaft 1','Shaft 1',#73767,#73670);
#73705=PRODUCT_DEFINITION('mm shaft collar','mm shaft collar',#73768,#73670);
#73706=PRODUCT_DEFINITION('mm shaft collar (1)','mm shaft collar (1)',#73769,
#73670);
#73707=PRODUCT_DEFINITION('mm outer spacer','mm outer spacer',#73770,#73670);
#73708=PRODUCT_DEFINITION('mm outer spacer (1)','mm outer spacer (1)',#73771,
#73670);
#73709=PRODUCT_DEFINITION('Spacer d12 L25','Spacer d12 L25',#73772,#73670);
#73710=PRODUCT_DEFINITION('Spacer d12 L53','Spacer d12 L53',#73773,#73670);
#73711=PRODUCT_DEFINITION('Spur Gear - Module 2, 20 Teeth, 12 mm Bore',
'Spur Gear - Module 2, 20 Teeth, 12 mm Bore',#73774,#73670);
#73712=PRODUCT_DEFINITION('Key 4x4x14','Key 4x4x14',#73775,#73670);
#73713=PRODUCT_DEFINITION('Compound rotor','Compound rotor',#73776,#73670);
#73714=PRODUCT_DEFINITION('Shaft 2','Shaft 2',#73777,#73670);
#73715=PRODUCT_DEFINITION('mm shaft collar (2)','mm shaft collar (2)',#73778,
#73670);
#73716=PRODUCT_DEFINITION('mm shaft collar (3)','mm shaft collar (3)',#73779,
#73670);
#73717=PRODUCT_DEFINITION('mm outer spacer (2)','mm outer spacer (2)',#73780,
#73670);
#73718=PRODUCT_DEFINITION('mm outer spacer (3)','mm outer spacer (3)',#73781,
#73670);
#73719=PRODUCT_DEFINITION('Spacer d20 L23','Spacer d20 L23',#73782,#73670);
#73720=PRODUCT_DEFINITION('Spacer d20 L8','Spacer d20 L8',#73783,#73670);
#73721=PRODUCT_DEFINITION('Spacer d20 L11','Spacer d20 L11',#73784,#73670);
#73722=PRODUCT_DEFINITION('Compound pinion m2 z20 b20',
'Compound pinion m2 z20 b20',#73785,#73670);
#73723=PRODUCT_DEFINITION('Output rotor','Output rotor',#73786,#73670);
#73724=PRODUCT_DEFINITION('Shaft 3','Shaft 3',#73787,#73670);
#73725=PRODUCT_DEFINITION('mm shaft collar (4)','mm shaft collar (4)',#73788,
#73670);
#73726=PRODUCT_DEFINITION('mm shaft collar (5)','mm shaft collar (5)',#73789,
#73670);
#73727=PRODUCT_DEFINITION('mm outer spacer (4)','mm outer spacer (4)',#73790,
#73670);
#73728=PRODUCT_DEFINITION('mm outer spacer (5)','mm outer spacer (5)',#73791,
#73670);
#73729=PRODUCT_DEFINITION('Spacer d20 L63','Spacer d20 L63',#73792,#73670);
#73730=PRODUCT_DEFINITION('Spacer d20 L11 (1)','Spacer d20 L11 (1)',#73793,
#73670);
#73731=PRODUCT_DEFINITION('Socket Set Screw - M5x8',
'Socket Set Screw - M5x8',#73794,#73670);
#73732=PRODUCT_DEFINITION('Spur Gear - Module 2, 40 Teeth, 20 mm Bore',
'Spur Gear - Module 2, 40 Teeth, 20 mm Bore',#73795,#73670);
#73733=PRODUCT_DEFINITION('Key 6x6x20','Key 6x6x20',#73796,#73670);
#73734=PRODUCT_DEFINITION_FORMATION('',$,#73863);
#73735=PRODUCT_DEFINITION_FORMATION('',$,#73864);
#73736=PRODUCT_DEFINITION_FORMATION('',$,#73865);
#73737=PRODUCT_DEFINITION_FORMATION('',$,#73866);
#73738=PRODUCT_DEFINITION_FORMATION('',$,#73867);
#73739=PRODUCT_DEFINITION_FORMATION('',$,#73868);
#73740=PRODUCT_DEFINITION_FORMATION('',$,#73869);
#73741=PRODUCT_DEFINITION_FORMATION('',$,#73870);
#73742=PRODUCT_DEFINITION_FORMATION('',$,#73871);
#73743=PRODUCT_DEFINITION_FORMATION('',$,#73872);
#73744=PRODUCT_DEFINITION_FORMATION('',$,#73873);
#73745=PRODUCT_DEFINITION_FORMATION('',$,#73874);
#73746=PRODUCT_DEFINITION_FORMATION('',$,#73875);
#73747=PRODUCT_DEFINITION_FORMATION('',$,#73876);
#73748=PRODUCT_DEFINITION_FORMATION('',$,#73877);
#73749=PRODUCT_DEFINITION_FORMATION('',$,#73878);
#73750=PRODUCT_DEFINITION_FORMATION('',$,#73879);
#73751=PRODUCT_DEFINITION_FORMATION('',$,#73880);
#73752=PRODUCT_DEFINITION_FORMATION('',$,#73881);
#73753=PRODUCT_DEFINITION_FORMATION('',$,#73882);
#73754=PRODUCT_DEFINITION_FORMATION('',$,#73883);
#73755=PRODUCT_DEFINITION_FORMATION('',$,#73884);
#73756=PRODUCT_DEFINITION_FORMATION('',$,#73885);
#73757=PRODUCT_DEFINITION_FORMATION('',$,#73886);
#73758=PRODUCT_DEFINITION_FORMATION('',$,#73887);
#73759=PRODUCT_DEFINITION_FORMATION('',$,#73888);
#73760=PRODUCT_DEFINITION_FORMATION('',$,#73889);
#73761=PRODUCT_DEFINITION_FORMATION('',$,#73890);
#73762=PRODUCT_DEFINITION_FORMATION('',$,#73891);
#73763=PRODUCT_DEFINITION_FORMATION('',$,#73892);
#73764=PRODUCT_DEFINITION_FORMATION('',$,#73893);
#73765=PRODUCT_DEFINITION_FORMATION('',$,#73894);
#73766=PRODUCT_DEFINITION_FORMATION('',$,#73895);
#73767=PRODUCT_DEFINITION_FORMATION('',$,#73896);
#73768=PRODUCT_DEFINITION_FORMATION('',$,#73897);
#73769=PRODUCT_DEFINITION_FORMATION('',$,#73898);
#73770=PRODUCT_DEFINITION_FORMATION('',$,#73899);
#73771=PRODUCT_DEFINITION_FORMATION('',$,#73900);
#73772=PRODUCT_DEFINITION_FORMATION('',$,#73901);
#73773=PRODUCT_DEFINITION_FORMATION('',$,#73902);
#73774=PRODUCT_DEFINITION_FORMATION('',$,#73903);
#73775=PRODUCT_DEFINITION_FORMATION('',$,#73904);
#73776=PRODUCT_DEFINITION_FORMATION('',$,#73905);
#73777=PRODUCT_DEFINITION_FORMATION('',$,#73906);
#73778=PRODUCT_DEFINITION_FORMATION('',$,#73907);
#73779=PRODUCT_DEFINITION_FORMATION('',$,#73908);
#73780=PRODUCT_DEFINITION_FORMATION('',$,#73909);
#73781=PRODUCT_DEFINITION_FORMATION('',$,#73910);
#73782=PRODUCT_DEFINITION_FORMATION('',$,#73911);
#73783=PRODUCT_DEFINITION_FORMATION('',$,#73912);
#73784=PRODUCT_DEFINITION_FORMATION('',$,#73913);
#73785=PRODUCT_DEFINITION_FORMATION('',$,#73914);
#73786=PRODUCT_DEFINITION_FORMATION('',$,#73915);
#73787=PRODUCT_DEFINITION_FORMATION('',$,#73916);
#73788=PRODUCT_DEFINITION_FORMATION('',$,#73917);
#73789=PRODUCT_DEFINITION_FORMATION('',$,#73918);
#73790=PRODUCT_DEFINITION_FORMATION('',$,#73919);
#73791=PRODUCT_DEFINITION_FORMATION('',$,#73920);
#73792=PRODUCT_DEFINITION_FORMATION('',$,#73921);
#73793=PRODUCT_DEFINITION_FORMATION('',$,#73922);
#73794=PRODUCT_DEFINITION_FORMATION('',$,#73923);
#73795=PRODUCT_DEFINITION_FORMATION('',$,#73924);
#73796=PRODUCT_DEFINITION_FORMATION('',$,#73925);
#73797=PRODUCT_RELATED_PRODUCT_CATEGORY('PAT-114','PAT-114',(#73863));
#73798=PRODUCT_RELATED_PRODUCT_CATEGORY('Split housing','Split housing',
(#73864));
#73799=PRODUCT_RELATED_PRODUCT_CATEGORY('Base','Base',(#73865));
#73800=PRODUCT_RELATED_PRODUCT_CATEGORY('Lower housing','Lower housing',
(#73866));
#73801=PRODUCT_RELATED_PRODUCT_CATEGORY('Upper housing','Upper housing',
(#73867));
#73802=PRODUCT_RELATED_PRODUCT_CATEGORY('Split dowel','Split dowel',(#73868));
#73803=PRODUCT_RELATED_PRODUCT_CATEGORY('Split dowel (1)',
'Split dowel (1)',(#73869));
#73804=PRODUCT_RELATED_PRODUCT_CATEGORY('Split dowel (2)',
'Split dowel (2)',(#73870));
#73805=PRODUCT_RELATED_PRODUCT_CATEGORY('Split dowel (3)',
'Split dowel (3)',(#73871));
#73806=PRODUCT_RELATED_PRODUCT_CATEGORY('mm end cap','mm end cap',(#73872));
#73807=PRODUCT_RELATED_PRODUCT_CATEGORY('mm end cap (1)',
'mm end cap (1)',(#73873));
#73808=PRODUCT_RELATED_PRODUCT_CATEGORY('mm end cap (2)',
'mm end cap (2)',(#73874));
#73809=PRODUCT_RELATED_PRODUCT_CATEGORY('mm end cap (3)',
'mm end cap (3)',(#73875));
#73810=PRODUCT_RELATED_PRODUCT_CATEGORY('mm end cap (4)',
'mm end cap (4)',(#73876));
#73811=PRODUCT_RELATED_PRODUCT_CATEGORY('mm end cap (5)',
'mm end cap (5)',(#73877));
#73812=PRODUCT_RELATED_PRODUCT_CATEGORY('Inspection cover',
'Inspection cover',(#73878));
#73813=PRODUCT_RELATED_PRODUCT_CATEGORY('Foot strip','Foot strip',(#73879));
#73814=PRODUCT_RELATED_PRODUCT_CATEGORY('Foot strip (1)',
'Foot strip (1)',(#73880));
#73815=PRODUCT_RELATED_PRODUCT_CATEGORY('M6x18 mounting screw',
'M6x18 mounting screw',(#73881));
#73816=PRODUCT_RELATED_PRODUCT_CATEGORY(
'Sealed Ball Bearing - 12 x 32 x 10 mm',
'Sealed Ball Bearing - 12 x 32 x 10 mm',(#73882));
#73817=PRODUCT_RELATED_PRODUCT_CATEGORY('Inner ring','Inner ring',(#73883));
#73818=PRODUCT_RELATED_PRODUCT_CATEGORY('Outer ring','Outer ring',(#73884));
#73819=PRODUCT_RELATED_PRODUCT_CATEGORY('Balls','Balls',(#73885));
#73820=PRODUCT_RELATED_PRODUCT_CATEGORY('Cage','Cage',(#73886));
#73821=PRODUCT_RELATED_PRODUCT_CATEGORY('Seals 2RS','Seals 2RS',(#73887));
#73822=PRODUCT_RELATED_PRODUCT_CATEGORY(
'Sealed Ball Bearing - 20 x 47 x 14 mm',
'Sealed Ball Bearing - 20 x 47 x 14 mm',(#73888));
#73823=PRODUCT_RELATED_PRODUCT_CATEGORY('Inner ring (1)',
'Inner ring (1)',(#73889));
#73824=PRODUCT_RELATED_PRODUCT_CATEGORY('Outer ring (1)',
'Outer ring (1)',(#73890));
#73825=PRODUCT_RELATED_PRODUCT_CATEGORY('Balls (1)','Balls (1)',(#73891));
#73826=PRODUCT_RELATED_PRODUCT_CATEGORY('Cage (1)','Cage (1)',(#73892));
#73827=PRODUCT_RELATED_PRODUCT_CATEGORY('Seals 2RS (1)','Seals 2RS (1)',
(#73893));
#73828=PRODUCT_RELATED_PRODUCT_CATEGORY('Cap Screw - M4x16',
'Cap Screw - M4x16',(#73894));
#73829=PRODUCT_RELATED_PRODUCT_CATEGORY('Input rotor','Input rotor',(#73895));
#73830=PRODUCT_RELATED_PRODUCT_CATEGORY('Shaft 1','Shaft 1',(#73896));
#73831=PRODUCT_RELATED_PRODUCT_CATEGORY('mm shaft collar',
'mm shaft collar',(#73897));
#73832=PRODUCT_RELATED_PRODUCT_CATEGORY('mm shaft collar (1)',
'mm shaft collar (1)',(#73898));
#73833=PRODUCT_RELATED_PRODUCT_CATEGORY('mm outer spacer',
'mm outer spacer',(#73899));
#73834=PRODUCT_RELATED_PRODUCT_CATEGORY('mm outer spacer (1)',
'mm outer spacer (1)',(#73900));
#73835=PRODUCT_RELATED_PRODUCT_CATEGORY('Spacer d12 L25',
'Spacer d12 L25',(#73901));
#73836=PRODUCT_RELATED_PRODUCT_CATEGORY('Spacer d12 L53',
'Spacer d12 L53',(#73902));
#73837=PRODUCT_RELATED_PRODUCT_CATEGORY(
'Spur Gear - Module 2, 20 Teeth, 12 mm Bore',
'Spur Gear - Module 2, 20 Teeth, 12 mm Bore',(#73903));
#73838=PRODUCT_RELATED_PRODUCT_CATEGORY('Key 4x4x14','Key 4x4x14',(#73904));
#73839=PRODUCT_RELATED_PRODUCT_CATEGORY('Compound rotor',
'Compound rotor',(#73905));
#73840=PRODUCT_RELATED_PRODUCT_CATEGORY('Shaft 2','Shaft 2',(#73906));
#73841=PRODUCT_RELATED_PRODUCT_CATEGORY('mm shaft collar (2)',
'mm shaft collar (2)',(#73907));
#73842=PRODUCT_RELATED_PRODUCT_CATEGORY('mm shaft collar (3)',
'mm shaft collar (3)',(#73908));
#73843=PRODUCT_RELATED_PRODUCT_CATEGORY('mm outer spacer (2)',
'mm outer spacer (2)',(#73909));
#73844=PRODUCT_RELATED_PRODUCT_CATEGORY('mm outer spacer (3)',
'mm outer spacer (3)',(#73910));
#73845=PRODUCT_RELATED_PRODUCT_CATEGORY('Spacer d20 L23',
'Spacer d20 L23',(#73911));
#73846=PRODUCT_RELATED_PRODUCT_CATEGORY('Spacer d20 L8','Spacer d20 L8',
(#73912));
#73847=PRODUCT_RELATED_PRODUCT_CATEGORY('Spacer d20 L11',
'Spacer d20 L11',(#73913));
#73848=PRODUCT_RELATED_PRODUCT_CATEGORY('Compound pinion m2 z20 b20',
'Compound pinion m2 z20 b20',(#73914));
#73849=PRODUCT_RELATED_PRODUCT_CATEGORY('Output rotor','Output rotor',(#73915));
#73850=PRODUCT_RELATED_PRODUCT_CATEGORY('Shaft 3','Shaft 3',(#73916));
#73851=PRODUCT_RELATED_PRODUCT_CATEGORY('mm shaft collar (4)',
'mm shaft collar (4)',(#73917));
#73852=PRODUCT_RELATED_PRODUCT_CATEGORY('mm shaft collar (5)',
'mm shaft collar (5)',(#73918));
#73853=PRODUCT_RELATED_PRODUCT_CATEGORY('mm outer spacer (4)',
'mm outer spacer (4)',(#73919));
#73854=PRODUCT_RELATED_PRODUCT_CATEGORY('mm outer spacer (5)',
'mm outer spacer (5)',(#73920));
#73855=PRODUCT_RELATED_PRODUCT_CATEGORY('Spacer d20 L63',
'Spacer d20 L63',(#73921));
#73856=PRODUCT_RELATED_PRODUCT_CATEGORY('Spacer d20 L11 (1)',
'Spacer d20 L11 (1)',(#73922));
#73857=PRODUCT_RELATED_PRODUCT_CATEGORY('Socket Set Screw - M5x8',
'Socket Set Screw - M5x8',(#73923));
#73858=PRODUCT_RELATED_PRODUCT_CATEGORY(
'Spur Gear - Module 2, 40 Teeth, 20 mm Bore',
'Spur Gear - Module 2, 40 Teeth, 20 mm Bore',(#73924));
#73859=PRODUCT_RELATED_PRODUCT_CATEGORY('Key 6x6x20','Key 6x6x20',(#73925));
#73860=APPLICATION_PROTOCOL_DEFINITION('international standard',
'automotive_design',2009,#73861);
#73861=APPLICATION_CONTEXT(
'Core Data for Automotive Mechanical Design Process');
#73862=PRODUCT_CONTEXT('part definition',#73861,'mechanical');
#73863=PRODUCT('PAT-114','PAT-114',
'PAT-114',(#73862));
#73864=PRODUCT('Split housing','Split housing','Split housing',(#73862));
#73865=PRODUCT('Base','Base','Base',(#73862));
#73866=PRODUCT('Lower housing','Lower housing','Lower housing',(#73862));
#73867=PRODUCT('Upper housing','Upper housing','Upper housing',(#73862));
#73868=PRODUCT('Split dowel','Split dowel','Split dowel',(#73862));
#73869=PRODUCT('Split dowel (1)','Split dowel (1)','Split dowel (1)',(#73862));
#73870=PRODUCT('Split dowel (2)','Split dowel (2)','Split dowel (2)',(#73862));
#73871=PRODUCT('Split dowel (3)','Split dowel (3)','Split dowel (3)',(#73862));
#73872=PRODUCT('mm end cap','mm end cap','mm end cap',(#73862));
#73873=PRODUCT('mm end cap (1)','mm end cap (1)','mm end cap (1)',(#73862));
#73874=PRODUCT('mm end cap (2)','mm end cap (2)','mm end cap (2)',(#73862));
#73875=PRODUCT('mm end cap (3)','mm end cap (3)','mm end cap (3)',(#73862));
#73876=PRODUCT('mm end cap (4)','mm end cap (4)','mm end cap (4)',(#73862));
#73877=PRODUCT('mm end cap (5)','mm end cap (5)','mm end cap (5)',(#73862));
#73878=PRODUCT('Inspection cover','Inspection cover','Inspection cover',
(#73862));
#73879=PRODUCT('Foot strip','Foot strip','Foot strip',(#73862));
#73880=PRODUCT('Foot strip (1)','Foot strip (1)','Foot strip (1)',(#73862));
#73881=PRODUCT('M6x18 mounting screw','M6x18 mounting screw',
'M6x18 mounting screw',(#73862));
#73882=PRODUCT('Sealed Ball Bearing - 12 x 32 x 10 mm',
'Sealed Ball Bearing - 12 x 32 x 10 mm',
'Sealed Ball Bearing - 12 x 32 x 10 mm',(#73862));
#73883=PRODUCT('Inner ring','Inner ring','Inner ring',(#73862));
#73884=PRODUCT('Outer ring','Outer ring','Outer ring',(#73862));
#73885=PRODUCT('Balls','Balls','Balls',(#73862));
#73886=PRODUCT('Cage','Cage','Cage',(#73862));
#73887=PRODUCT('Seals 2RS','Seals 2RS','Seals 2RS',(#73862));
#73888=PRODUCT('Sealed Ball Bearing - 20 x 47 x 14 mm',
'Sealed Ball Bearing - 20 x 47 x 14 mm',
'Sealed Ball Bearing - 20 x 47 x 14 mm',(#73862));
#73889=PRODUCT('Inner ring (1)','Inner ring (1)','Inner ring (1)',(#73862));
#73890=PRODUCT('Outer ring (1)','Outer ring (1)','Outer ring (1)',(#73862));
#73891=PRODUCT('Balls (1)','Balls (1)','Balls (1)',(#73862));
#73892=PRODUCT('Cage (1)','Cage (1)','Cage (1)',(#73862));
#73893=PRODUCT('Seals 2RS (1)','Seals 2RS (1)','Seals 2RS (1)',(#73862));
#73894=PRODUCT('Cap Screw - M4x16','Cap Screw - M4x16',
'Cap Screw - M4x16',(#73862));
#73895=PRODUCT('Input rotor','Input rotor','Input rotor',(#73862));
#73896=PRODUCT('Shaft 1','Shaft 1','Shaft 1',(#73862));
#73897=PRODUCT('mm shaft collar','mm shaft collar','mm shaft collar',(#73862));
#73898=PRODUCT('mm shaft collar (1)','mm shaft collar (1)',
'mm shaft collar (1)',(#73862));
#73899=PRODUCT('mm outer spacer','mm outer spacer','mm outer spacer',(#73862));
#73900=PRODUCT('mm outer spacer (1)','mm outer spacer (1)',
'mm outer spacer (1)',(#73862));
#73901=PRODUCT('Spacer d12 L25','Spacer d12 L25','Spacer d12 L25',(#73862));
#73902=PRODUCT('Spacer d12 L53','Spacer d12 L53','Spacer d12 L53',(#73862));
#73903=PRODUCT('Spur Gear - Module 2, 20 Teeth, 12 mm Bore',
'Spur Gear - Module 2, 20 Teeth, 12 mm Bore',
'Spur Gear - Module 2, 20 Teeth, 12 mm Bore',(#73862));
#73904=PRODUCT('Key 4x4x14','Key 4x4x14','Key 4x4x14',(#73862));
#73905=PRODUCT('Compound rotor','Compound rotor','Compound rotor',(#73862));
#73906=PRODUCT('Shaft 2','Shaft 2','Shaft 2',(#73862));
#73907=PRODUCT('mm shaft collar (2)','mm shaft collar (2)',
'mm shaft collar (2)',(#73862));
#73908=PRODUCT('mm shaft collar (3)','mm shaft collar (3)',
'mm shaft collar (3)',(#73862));
#73909=PRODUCT('mm outer spacer (2)','mm outer spacer (2)',
'mm outer spacer (2)',(#73862));
#73910=PRODUCT('mm outer spacer (3)','mm outer spacer (3)',
'mm outer spacer (3)',(#73862));
#73911=PRODUCT('Spacer d20 L23','Spacer d20 L23','Spacer d20 L23',(#73862));
#73912=PRODUCT('Spacer d20 L8','Spacer d20 L8','Spacer d20 L8',(#73862));
#73913=PRODUCT('Spacer d20 L11','Spacer d20 L11','Spacer d20 L11',(#73862));
#73914=PRODUCT('Compound pinion m2 z20 b20',
'Compound pinion m2 z20 b20','Compound pinion m2 z20 b20',(#73862));
#73915=PRODUCT('Output rotor','Output rotor','Output rotor',(#73862));
#73916=PRODUCT('Shaft 3','Shaft 3','Shaft 3',(#73862));
#73917=PRODUCT('mm shaft collar (4)','mm shaft collar (4)',
'mm shaft collar (4)',(#73862));
#73918=PRODUCT('mm shaft collar (5)','mm shaft collar (5)',
'mm shaft collar (5)',(#73862));
#73919=PRODUCT('mm outer spacer (4)','mm outer spacer (4)',
'mm outer spacer (4)',(#73862));
#73920=PRODUCT('mm outer spacer (5)','mm outer spacer (5)',
'mm outer spacer (5)',(#73862));
#73921=PRODUCT('Spacer d20 L63','Spacer d20 L63','Spacer d20 L63',(#73862));
#73922=PRODUCT('Spacer d20 L11 (1)','Spacer d20 L11 (1)','Spacer d20 L11 (1)',
(#73862));
#73923=PRODUCT('Socket Set Screw - M5x8','Socket Set Screw - M5x8',
'Socket Set Screw - M5x8',(#73862));
#73924=PRODUCT('Spur Gear - Module 2, 40 Teeth, 20 mm Bore',
'Spur Gear - Module 2, 40 Teeth, 20 mm Bore',
'Spur Gear - Module 2, 40 Teeth, 20 mm Bore',(#73862));
#73925=PRODUCT('Key 6x6x20','Key 6x6x20','Key 6x6x20',(#73862));
#73926=PRESENTATION_STYLE_ASSIGNMENT((#73931));
#73927=PRESENTATION_STYLE_ASSIGNMENT((#73932));
#73928=PRESENTATION_STYLE_ASSIGNMENT((#73933));
#73929=PRESENTATION_STYLE_ASSIGNMENT((#73934));
#73930=PRESENTATION_STYLE_ASSIGNMENT((#73935));
#73931=SURFACE_STYLE_USAGE(.BOTH.,#73936);
#73932=SURFACE_STYLE_USAGE(.BOTH.,#73937);
#73933=SURFACE_STYLE_USAGE(.BOTH.,#73938);
#73934=SURFACE_STYLE_USAGE(.BOTH.,#73939);
#73935=SURFACE_STYLE_USAGE(.BOTH.,#73940);
#73936=SURFACE_SIDE_STYLE('',(#73941));
#73937=SURFACE_SIDE_STYLE('',(#73942));
#73938=SURFACE_SIDE_STYLE('',(#73943));
#73939=SURFACE_SIDE_STYLE('',(#73944));
#73940=SURFACE_SIDE_STYLE('',(#73945));
#73941=SURFACE_STYLE_FILL_AREA(#73946);
#73942=SURFACE_STYLE_FILL_AREA(#73947);
#73943=SURFACE_STYLE_FILL_AREA(#73948);
#73944=SURFACE_STYLE_FILL_AREA(#73949);
#73945=SURFACE_STYLE_FILL_AREA(#73950);
#73946=FILL_AREA_STYLE('Steel - Satin',(#73951));
#73947=FILL_AREA_STYLE('CAD Library Painted - Deep blue',(#73952));
#73948=FILL_AREA_STYLE('CAD Library Painted - Engineering blue',(#73953));
#73949=FILL_AREA_STYLE('CAD Library Painted - Graphite',(#73954));
#73950=FILL_AREA_STYLE('CAD Library Painted - Steel gray',(#73955));
#73951=FILL_AREA_STYLE_COLOUR('Steel - Satin',#73956);
#73952=FILL_AREA_STYLE_COLOUR('CAD Library Painted - Deep blue',#73957);
#73953=FILL_AREA_STYLE_COLOUR('CAD Library Painted - Engineering blue',
#73958);
#73954=FILL_AREA_STYLE_COLOUR('CAD Library Painted - Graphite',#73959);
#73955=FILL_AREA_STYLE_COLOUR('CAD Library Painted - Steel gray',#73960);
#73956=COLOUR_RGB('Steel - Satin',0.627450980392157,0.627450980392157,0.627450980392157);
#73957=COLOUR_RGB('CAD Library Painted - Deep blue',0.0784313725490196,
0.203921568627451,0.349019607843137);
#73958=COLOUR_RGB('CAD Library Painted - Engineering blue',0.12156862745098,
0.356862745098039,0.6);
#73959=COLOUR_RGB('CAD Library Painted - Graphite',0.168627450980392,0.192156862745098,
0.231372549019608);
#73960=COLOUR_RGB('CAD Library Painted - Steel gray',0.592156862745098,
0.631372549019608,0.67843137254902);
#73961=COLOUR_RGB('Dark Blue',0.08,0.2,0.34);
#73962=FILL_AREA_STYLE_COLOUR('',#73961);
#73963=FILL_AREA_STYLE('',(#73962));
#73964=SURFACE_STYLE_FILL_AREA(#73963);
#73965=SURFACE_SIDE_STYLE('',(#73964));
#73966=SURFACE_STYLE_USAGE(.BOTH.,#73965);
#73967=PRESENTATION_STYLE_ASSIGNMENT((#73966));
#73968=COLOUR_RGB('Light Blue',0.38,0.62,0.78);
#73969=FILL_AREA_STYLE_COLOUR('',#73968);
#73970=FILL_AREA_STYLE('',(#73969));
#73971=SURFACE_STYLE_FILL_AREA(#73970);
#73972=SURFACE_SIDE_STYLE('',(#73971));
#73973=SURFACE_STYLE_USAGE(.BOTH.,#73972);
#73974=PRESENTATION_STYLE_ASSIGNMENT((#73973));
#73975=COLOUR_RGB('Sky Blue',0.24,0.69,0.87);
#73976=FILL_AREA_STYLE_COLOUR('',#73975);
#73977=FILL_AREA_STYLE('',(#73976));
#73978=SURFACE_STYLE_FILL_AREA(#73977);
#73979=SURFACE_SIDE_STYLE('',(#73978));
#73980=SURFACE_STYLE_USAGE(.BOTH.,#73979);
#73981=PRESENTATION_STYLE_ASSIGNMENT((#73980));
#73982=COLOUR_RGB('Grey',0.48,0.52,0.57);
#73983=FILL_AREA_STYLE_COLOUR('',#73982);
#73984=FILL_AREA_STYLE('',(#73983));
#73985=SURFACE_STYLE_FILL_AREA(#73984);
#73986=SURFACE_SIDE_STYLE('',(#73985));
#73987=SURFACE_STYLE_USAGE(.BOTH.,#73986);
#73988=PRESENTATION_STYLE_ASSIGNMENT((#73987));
#73989=COLOUR_RGB('Black',0.12,0.14,0.17);
#73990=FILL_AREA_STYLE_COLOUR('',#73989);
#73991=FILL_AREA_STYLE('',(#73990));
#73992=SURFACE_STYLE_FILL_AREA(#73991);
#73993=SURFACE_SIDE_STYLE('',(#73992));
#73994=SURFACE_STYLE_USAGE(.BOTH.,#73993);
#73995=PRESENTATION_STYLE_ASSIGNMENT((#73994));
#73996=COLOUR_RGB('Off White',0.89,0.88,0.83);
#73997=FILL_AREA_STYLE_COLOUR('',#73996);
#73998=FILL_AREA_STYLE('',(#73997));
#73999=SURFACE_STYLE_FILL_AREA(#73998);
#74000=SURFACE_SIDE_STYLE('',(#73999));
#74001=SURFACE_STYLE_USAGE(.BOTH.,#74000);
#74002=PRESENTATION_STYLE_ASSIGNMENT((#74001));
ENDSEC;
END-ISO-10303-21;
